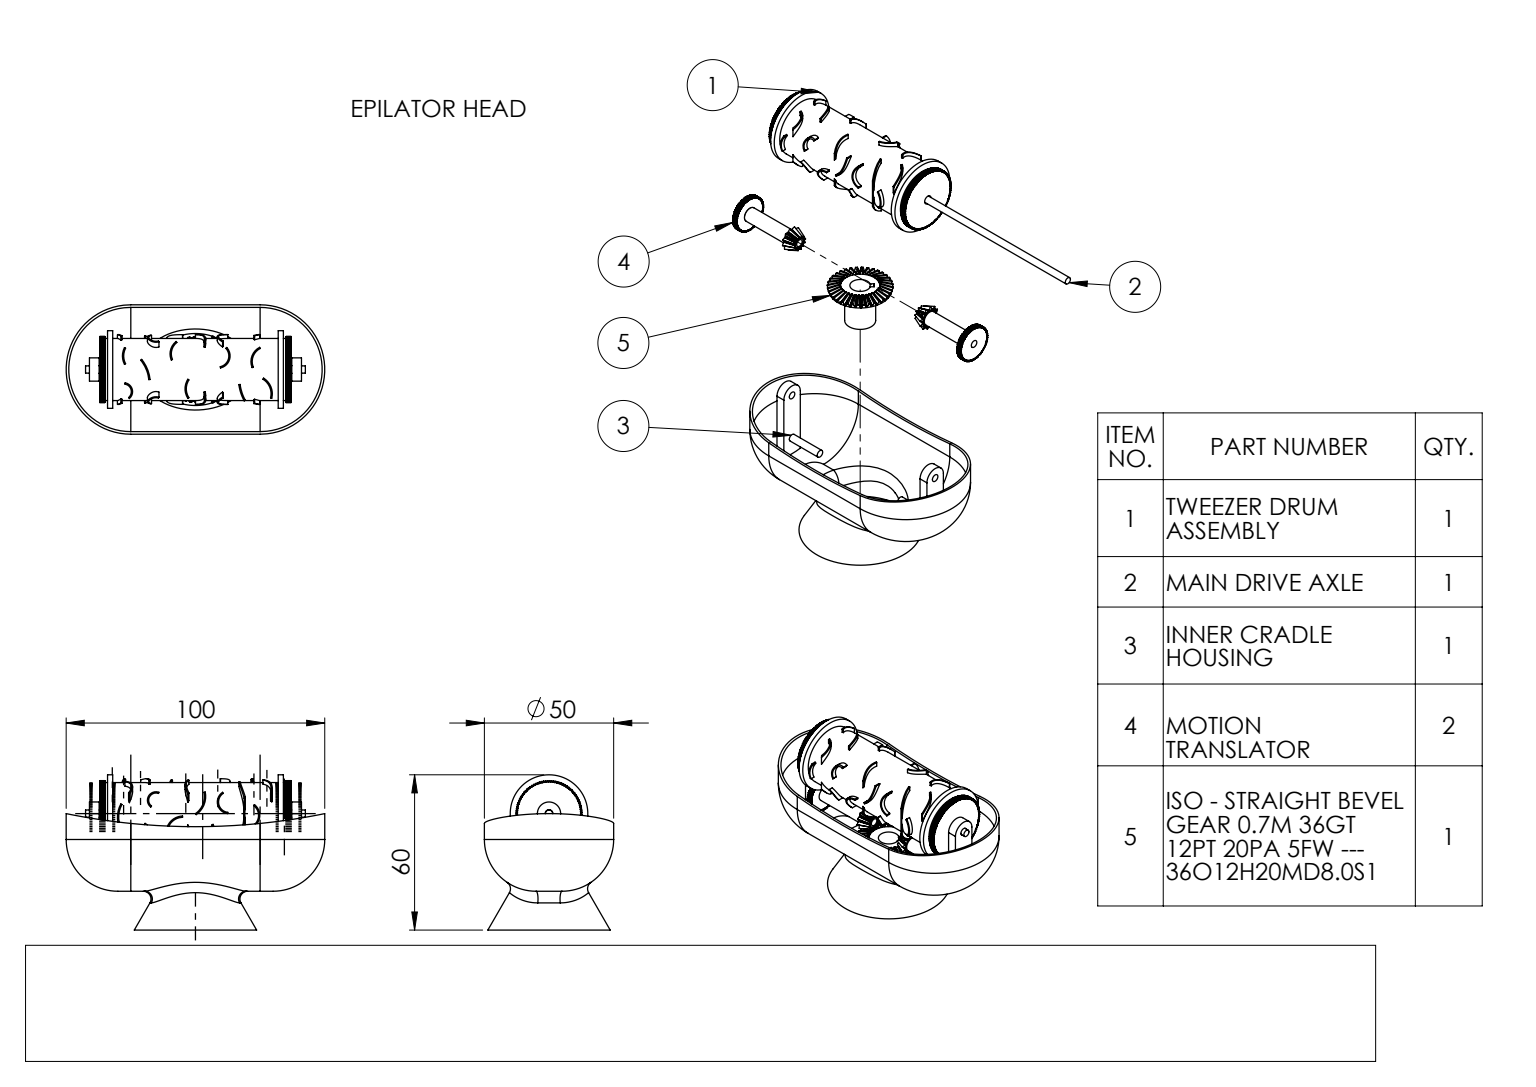
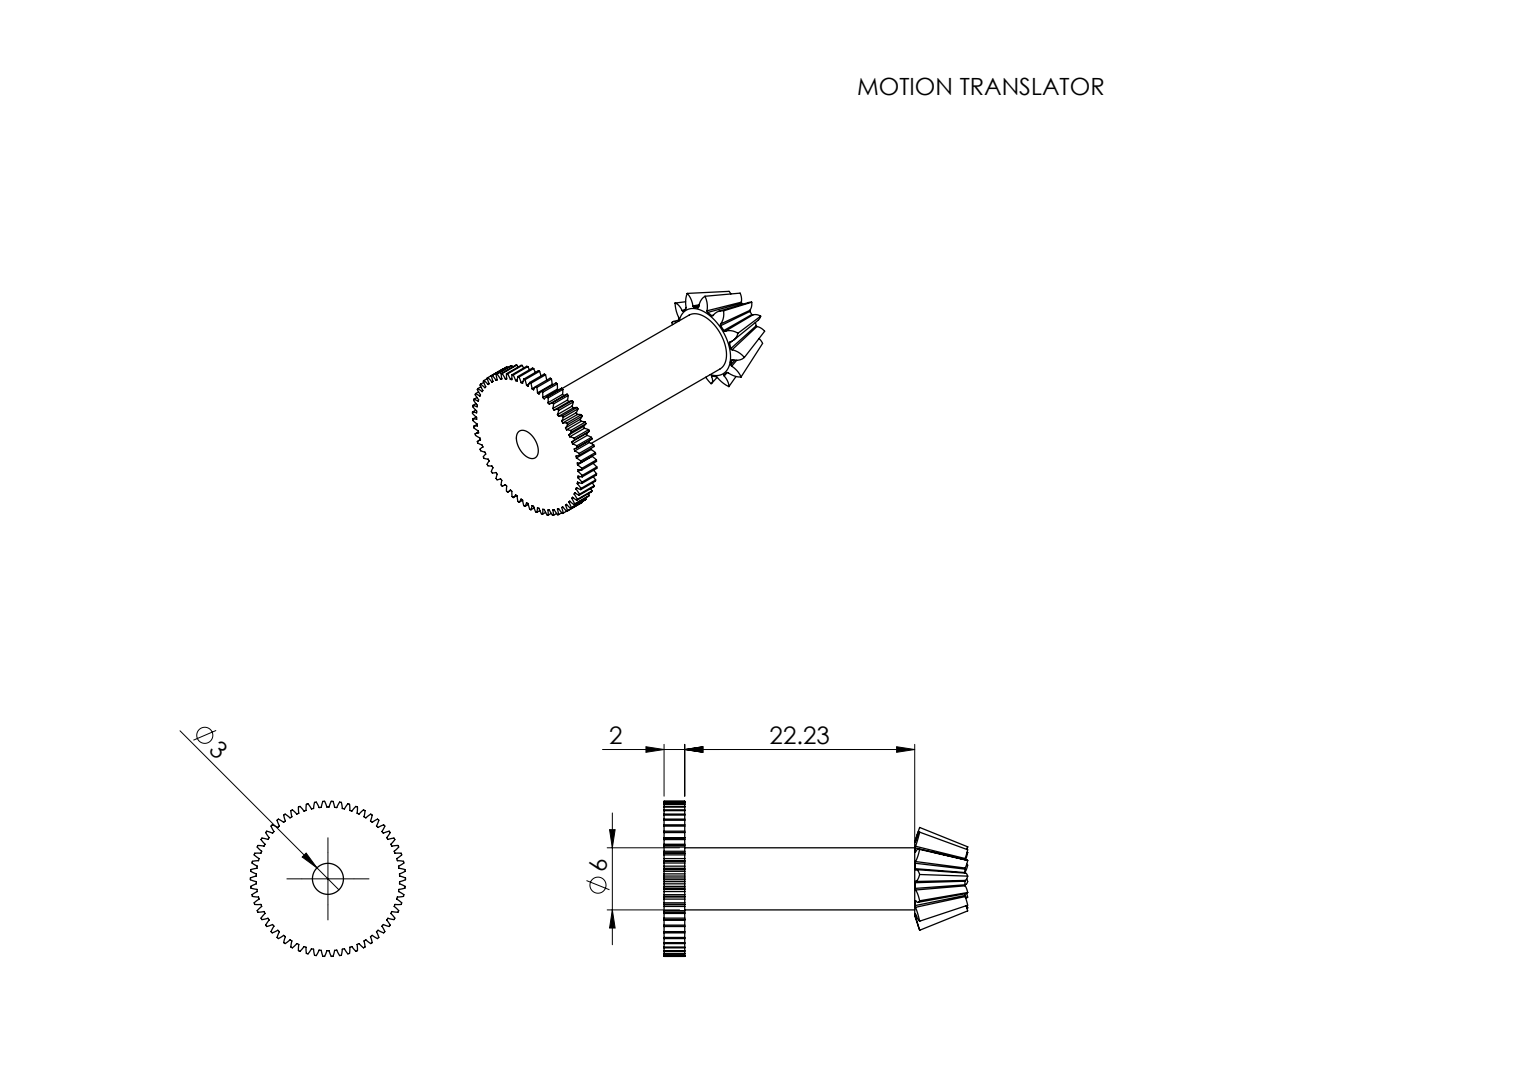
ISO-10303-21;
HEADER;
FILE_DESCRIPTION (('STEP AP214'),
    '1' );
FILE_NAME ('BR-837',
    '2026-10-09T15:17:24',
    ( '' ),
    ( '' ),
    'SwSTEP 2.0',
    'SolidWorks 2026',
    '' );
FILE_SCHEMA (( 'AUTOMOTIVE_DESIGN' ));
ENDSEC;

DATA;
#1 = ORIENTED_EDGE ( 'NONE', *, *, #54093, .F. ) ;
#2 =( BOUNDED_CURVE ( )  B_SPLINE_CURVE ( 3, ( #3306, #62815, #58857, #63152 ),
 .UNSPECIFIED., .F., .T. ) 
 B_SPLINE_CURVE_WITH_KNOTS ( ( 4, 4 ),
 ( 1.289274629942206873, 1.307832622343243267 ),
 .UNSPECIFIED. ) 
 CURVE ( )  GEOMETRIC_REPRESENTATION_ITEM ( )  RATIONAL_B_SPLINE_CURVE ( ( 1.000000000000000000, 0.9999713002824244246, 0.9999713002824244246, 1.000000000000000000 ) ) 
 REPRESENTATION_ITEM ( '' )  );
#3 = DIRECTION ( 'NONE',  ( 1.000000000000000000, 0.000000000000000000, -0.000000000000000000 ) ) ;
#4 = CARTESIAN_POINT ( 'NONE',  ( 34.00000000000000000, 1.267509437117510519E-14, 0.000000000000000000 ) ) ;
#5 = EDGE_CURVE ( 'NONE', #33980, #40116, #8200, .T. ) ;
#6 = ORIENTED_EDGE ( 'NONE', *, *, #26203, .T. ) ;
#7 = CARTESIAN_POINT ( 'NONE',  ( -27.64865282621882869, 11.88308961669896746, -6.412759754742364926 ) ) ;
#8 = CARTESIAN_POINT ( 'NONE',  ( 29.22757921152195948, 7.948027597311009274, 9.002217460645077551 ) ) ;
#9 = DIRECTION ( 'NONE',  ( -1.000000000000000000, 0.000000000000000000, 0.000000000000000000 ) ) ;
#10 = AXIS2_PLACEMENT_3D ( 'NONE', #51106, #21495, #16509 ) ;
#11 = EDGE_LOOP ( 'NONE', ( #13476, #2905, #46275, #26509, #7082, #64281 ) ) ;
#12 = CARTESIAN_POINT ( 'NONE',  ( 2.251152103363648127, -7.636644423939545234, 0.1252683866804877588 ) ) ;
#13 = EDGE_CURVE ( 'NONE', #20288, #62523, #39030, .T. ) ;
#14 = CIRCLE ( 'NONE', #45668, 4.999999999999999112 ) ;
#15 = ORIENTED_EDGE ( 'NONE', *, *, #45352, .F. ) ;
#16 = CARTESIAN_POINT ( 'NONE',  ( -2.532614230583026593, 25.00000000000000000, 10.89930238848911337 ) ) ;
#17 = CARTESIAN_POINT ( 'NONE',  ( -20.31445708845316389, -13.09484702705360704, -3.338600914039887346 ) ) ;
#18 = CARTESIAN_POINT ( 'NONE',  ( -9.857630741398541119, -27.64257788600498245, 14.42778837489968424 ) ) ;
#19 = DIRECTION ( 'NONE',  ( 1.000000000000000000, 0.000000000000000000, 0.000000000000000000 ) ) ;
#20 = CARTESIAN_POINT ( 'NONE',  ( 2.241509619876138171, 7.511759925807403704, 1.363398699156074922 ) ) ;
#21 = EDGE_LOOP ( 'NONE', ( #48561, #59529, #5133, #41435 ) ) ;
#22 = CARTESIAN_POINT ( 'NONE',  ( 37.00000000000000711, -6.303578524887017309, -10.42955799785317872 ) ) ;
#24 = AXIS2_PLACEMENT_3D ( 'NONE', #425, #35953, #14688 ) ;
#23 = CARTESIAN_POINT ( 'NONE',  ( 3.459614771489464946, -11.09853614738469396, 25.00000000000000000 ) ) ;
#25 = CARTESIAN_POINT ( 'NONE',  ( 2.241528039335009215, 3.830846649711605600, -6.603755931420445258 ) ) ;
#26 = CARTESIAN_POINT ( 'NONE',  ( 35.00000000000000000, 4.705694406421931860E-17, -3.469127814946512892E-15 ) ) ;
#27 = CIRCLE ( 'NONE', #62657, 12.18649999999999878 ) ;
#28 = CARTESIAN_POINT ( 'NONE',  ( 0.2671309869109511070, -12.08782215308010066, -1.966882337881812104 ) ) ;
#29 = CARTESIAN_POINT ( 'NONE',  ( 47.00000000000000711, 4.705694406421931860E-17, -3.469127814946512892E-15 ) ) ;
#30 = DIRECTION ( 'NONE',  ( 1.000000000000000000, -0.000000000000000000, 0.000000000000000000 ) ) ;
#31 = CARTESIAN_POINT ( 'NONE',  ( 0.2648978790185610999, -6.008231198269058382, 10.67083876753489946 ) ) ;
#32 = CARTESIAN_POINT ( 'NONE',  ( -36.00000000000000711, -2.527899948230555083, -12.49688848680887077 ) ) ;
#33 = B_SPLINE_CURVE_WITH_KNOTS ( 'NONE', 3,
 ( #58720, #44686, #34706, #18133, #9434, #8152, #55005, #39719, #13453, #43722, #8473, #64002, #3845, #49070, #3519, #23790 ),
 .UNSPECIFIED., .F., .F.,
 ( 4, 3, 3, 3, 3, 4 ),
 ( 0.000000000000000000, 0.0002999043160757348470, 0.0005998071753050991575, 0.0008997092107374514165, 0.001204458948195627314, 0.001510329163476480975 ),
 .UNSPECIFIED. ) ;
#34 = EDGE_CURVE ( 'NONE', #6901, #57938, #39765, .T. ) ;
#35 = CIRCLE ( 'NONE', #8525, 2.899999999999994582 ) ;
#36 = CIRCLE ( 'NONE', #39342, 5.000000000000000000 ) ;
#37 = ORIENTED_EDGE ( 'NONE', *, *, #2591, .T. ) ;
#38 = ORIENTED_EDGE ( 'NONE', *, *, #32481, .T. ) ;
#39 = DIRECTION ( 'NONE',  ( 0.2227494284590502138, 0.000000000000000000, 0.9748757316300199482 ) ) ;
#40 = CARTESIAN_POINT ( 'NONE',  ( -22.27721056931765631, -3.610969226755186057, 0.7178530073137494583 ) ) ;
#41 = DIRECTION ( 'NONE',  ( -1.000000000000000000, 0.000000000000000000, 0.000000000000000000 ) ) ;
#42 = DIRECTION ( 'NONE',  ( -0.000000000000000000, -0.000000000000000000, -1.000000000000000000 ) ) ;
#43 = ORIENTED_EDGE ( 'NONE', *, *, #16886, .F. ) ;
#44 = VERTEX_POINT ( 'NONE', #43427 ) ;
#45 = ORIENTED_EDGE ( 'NONE', *, *, #528, .T. ) ;
#46 = CARTESIAN_POINT ( 'NONE',  ( 2.931247277082686509, 3.034789039497289842, -7.255238984871596131 ) ) ;
#47 = AXIS2_PLACEMENT_3D ( 'NONE', #35700, #25750, #46038 ) ;
#48 = CARTESIAN_POINT ( 'NONE',  ( -20.92008205012189848, -11.37744109147143590, -3.816568647652266222 ) ) ;
#49 = EDGE_CURVE ( 'NONE', #39147, #50867, #8852, .T. ) ;
#50 = ORIENTED_EDGE ( 'NONE', *, *, #19511, .T. ) ;
#51 = CARTESIAN_POINT ( 'NONE',  ( 20.00005080000000035, 0.000000000000000000, 0.000000000000000000 ) ) ;
#52 = CARTESIAN_POINT ( 'NONE',  ( 35.00000000000000000, 3.511814412392283646, 11.66953048682395355 ) ) ;
#53 = CARTESIAN_POINT ( 'NONE',  ( 2.990245332647861964, -8.426135047918856813, 0.9653152459622899029 ) ) ;
#54 = ORIENTED_EDGE ( 'NONE', *, *, #43453, .T. ) ;
#55 = CARTESIAN_POINT ( 'NONE',  ( -22.30078715814471835, 0.2606204736987125514, 3.743307663037636956 ) ) ;
#56 = EDGE_CURVE ( 'NONE', #31963, #46746, #12133, .T. ) ;
#57 = CARTESIAN_POINT ( 'NONE',  ( 1.074417311476297821, -26.55384113566742599, -16.22365110280896161 ) ) ;
#58 = DIRECTION ( 'NONE',  ( -0.000000000000000000, -0.000000000000000000, -1.000000000000000000 ) ) ;
#59 = VERTEX_POINT ( 'NONE', #24459 ) ;
#60 = DIRECTION ( 'NONE',  ( -1.000000000000000000, 0.000000000000000000, 0.000000000000000000 ) ) ;
#61 = EDGE_CURVE ( 'NONE', #21447, #54893, #59089, .T. ) ;
#62 = EDGE_LOOP ( 'NONE', ( #29288, #23107, #41719, #50661 ) ) ;
#63 = CARTESIAN_POINT ( 'NONE',  ( 1.719304012339869514, -10.22720798541492471, 7.581471372739622794 ) ) ;
#64 = VECTOR ( 'NONE', #37546, 1000.000000000000000 ) ;
#65 = ORIENTED_EDGE ( 'NONE', *, *, #16176, .T. ) ;
#66 = CARTESIAN_POINT ( 'NONE',  ( -28.82521652700830117, 2.770713649382011923, -11.70126355471820467 ) ) ;
#67 = DIRECTION ( 'NONE',  ( -1.000000000000000000, 0.000000000000000000, 0.000000000000000000 ) ) ;
#68 = CARTESIAN_POINT ( 'NONE',  ( 37.00000000000000711, -11.24036214326524608, -6.018036132182126963 ) ) ;
#69 = DIRECTION ( 'NONE',  ( 1.000000000000000000, 0.000000000000000000, 0.000000000000000000 ) ) ;
#70 = CARTESIAN_POINT ( 'NONE',  ( -25.62834777364930616, 3.789932915281918113, 0.3208481691297681571 ) ) ;
#71 = LINE ( 'NONE', #60932, #20822 ) ;
#73 = ADVANCED_FACE ( 'NONE', ( #28468 ), #28161, .T. ) ;
#72 = FACE_OUTER_BOUND ( 'NONE', #21763, .T. ) ;
#74 = DIRECTION ( 'NONE',  ( 0.000000000000000000, 0.000000000000000000, -1.000000000000000000 ) ) ;
#75 = CARTESIAN_POINT ( 'NONE',  ( 0.2833330754217384673, -3.999965385632516579, -11.58086621621911583 ) ) ;
#77 = ORIENTED_EDGE ( 'NONE', *, *, #43041, .T. ) ;
#76 = CARTESIAN_POINT ( 'NONE',  ( -37.00000000000000711, 0.7536123767500182424, -11.72195762423409171 ) ) ;
#78 = CARTESIAN_POINT ( 'NONE',  ( -22.30625920655495165, -3.783486345733982237, 0.2529928606556808846 ) ) ;
#79 = AXIS2_PLACEMENT_3D ( 'NONE', #49490, #64734, #28522 ) ;
#80 = ORIENTED_EDGE ( 'NONE', *, *, #29710, .F. ) ;
#81 = CARTESIAN_POINT ( 'NONE',  ( 2.305787727787084407, -3.971363876083918498, -6.545285700970570275 ) ) ;
#82 = VERTEX_POINT ( 'NONE', #8514 ) ;
#83 = EDGE_CURVE ( 'NONE', #13628, #12164, #48775, .T. ) ;
#84 = CARTESIAN_POINT ( 'NONE',  ( 3.047904605210419504, -5.772373816836783078, -5.398304302092596707 ) ) ;
#85 = VECTOR ( 'NONE', #37422, 1000.000000000000000 ) ;
#86 = ORIENTED_EDGE ( 'NONE', *, *, #15250, .T. ) ;
#87 = DIRECTION ( 'NONE',  ( 1.000000000000000000, -0.000000000000000000, -0.000000000000000000 ) ) ;
#88 = LINE ( 'NONE', #34354, #47498 ) ;
#89 = CARTESIAN_POINT ( 'NONE',  ( -27.09229696323321335, -2.225368503508849294, 0.6397626223479151442 ) ) ;
#90 = DIRECTION ( 'NONE',  ( 0.000000000000000000, 0.000000000000000000, -1.000000000000000000 ) ) ;
#91 = DIRECTION ( 'NONE',  ( 1.000000000000000000, 0.000000000000000000, 0.000000000000000000 ) ) ;
#92 = CIRCLE ( 'NONE', #17079, 4.999999999999999112 ) ;
#93 = AXIS2_PLACEMENT_3D ( 'NONE', #46470, #925, #21193 ) ;
#94 = AXIS2_PLACEMENT_3D ( 'NONE', #16809, #31133, #22127 ) ;
#95 = VERTEX_POINT ( 'NONE', #49115 ) ;
#96 = CARTESIAN_POINT ( 'NONE',  ( -37.00000000000000711, 7.474872387601008583, 9.060822531526074641 ) ) ;
#97 = EDGE_CURVE ( 'NONE', #10033, #43796, #33778, .T. ) ;
#98 = AXIS2_PLACEMENT_3D ( 'NONE', #57341, #58008, #7118 ) ;
#99 = ORIENTED_EDGE ( 'NONE', *, *, #2192, .T. ) ;
#100 = CARTESIAN_POINT ( 'NONE',  ( -22.30625920655495165, 0.8854385781085528651, -3.687109008463846926 ) ) ;
#101 = EDGE_CURVE ( 'NONE', #9709, #46803, #31331, .T. ) ;
#102 = FACE_OUTER_BOUND ( 'NONE', #65679, .T. ) ;
#103 = CARTESIAN_POINT ( 'NONE',  ( 0.2652384529303130067, -7.922180393770610785, -9.338494547402472534 ) ) ;
#104 = ORIENTED_EDGE ( 'NONE', *, *, #19181, .T. ) ;
#105 = CARTESIAN_POINT ( 'NONE',  ( -35.00000000000000000, 0.000000000000000000, 0.000000000000000000 ) ) ;
#106 = AXIS2_PLACEMENT_3D ( 'NONE', #32837, #48187, #63433 ) ;
#107 = AXIS2_PLACEMENT_3D ( 'NONE', #48295, #12020, #32299 ) ;
#108 = CIRCLE ( 'NONE', #63839, 12.18649999999999700 ) ;
#109 = AXIS2_PLACEMENT_3D ( 'NONE', #42573, #46294, #734 ) ;
#110 = CARTESIAN_POINT ( 'NONE',  ( 49.33927601438018229, -0.1339636383559821564, -5.724480317196142032 ) ) ;
#111 = B_SPLINE_CURVE_WITH_KNOTS ( 'NONE', 3,
 ( #8141, #22114, #47410, #53377, #22445, #48713, #53707, #37074, #18119, #33412, #57373, #11799, #28412, #13126, #6844, #1847, #63323, #42709, #17792 ),
 .UNSPECIFIED., .F., .F.,
 ( 4, 3, 3, 3, 3, 3, 4 ),
 ( 0.000000000000000000, 2.831840207457774963E-05, 4.217266859783117455E-05, 5.602024318339443094E-05, 6.290810167912943239E-05, 9.120440630890260935E-05, 0.0001153103026480235913 ),
 .UNSPECIFIED. ) ;
#112 = AXIS2_PLACEMENT_3D ( 'NONE', #43314, #33991, #53653 ) ;
#113 = CARTESIAN_POINT ( 'NONE',  ( -10.71713000802667359, -9.043952695441483058, -10.03432938415238951 ) ) ;
#114 = CARTESIAN_POINT ( 'NONE',  ( -38.20713125073509531, -2.115151932665340961, -21.24219930640693832 ) ) ;
#115 = ORIENTED_EDGE ( 'NONE', *, *, #54584, .T. ) ;
#116 = CARTESIAN_POINT ( 'NONE',  ( 19.56743653832046803, -28.99999999999999645, -5.000000000000000888 ) ) ;
#117 = CARTESIAN_POINT ( 'NONE',  ( 2.000000000000001776, -6.441884263200823746, -2.217201541069834914 ) ) ;
#118 = CARTESIAN_POINT ( 'NONE',  ( 2.827825597296804272, -9.007857251166447199, -0.5449445831287991204 ) ) ;
#119 = AXIS2_PLACEMENT_3D ( 'NONE', #1581, #5588, #900 ) ;
#120 = ADVANCED_FACE ( 'NONE', ( #39097 ), #54424, .T. ) ;
#121 = ADVANCED_FACE ( 'NONE', ( #65020 ), #19493, .F. ) ;
#122 = CARTESIAN_POINT ( 'NONE',  ( -37.00000000000000711, 12.02534193257726969, -4.237174932027097718 ) ) ;
#123 = DIRECTION ( 'NONE',  ( 1.000000000000000000, -0.000000000000000000, 0.000000000000000000 ) ) ;
#124 = CIRCLE ( 'NONE', #37284, 5.000000000000000000 ) ;
#125 = VERTEX_POINT ( 'NONE', #10810 ) ;
#126 = CARTESIAN_POINT ( 'NONE',  ( -22.28506771379528573, 3.622079238249921840, 0.8783543640076683090 ) ) ;
#127 = CARTESIAN_POINT ( 'NONE',  ( 2.096166925314653984, 2.110369137379828786, -11.81794094722716260 ) ) ;
#128 = CARTESIAN_POINT ( 'NONE',  ( -22.29570301036918778, 3.588849529203733457, -1.042190670255880525 ) ) ;
#129 = EDGE_LOOP ( 'NONE', ( #26089, #45979, #28221, #53129 ) ) ;
#130 = CARTESIAN_POINT ( 'NONE',  ( -35.00000000000000000, 11.56998259273177787, 3.827046518385122553 ) ) ;
#131 = AXIS2_PLACEMENT_3D ( 'NONE', #9769, #50367, #4141 ) ;
#132 = CARTESIAN_POINT ( 'NONE',  ( 37.00000000000000711, 4.705694406421931860E-17, -3.469127814946512892E-15 ) ) ;
#133 = ORIENTED_EDGE ( 'NONE', *, *, #30675, .T. ) ;
#134 = EDGE_CURVE ( 'NONE', #53943, #37151, #49390, .T. ) ;
#135 = EDGE_LOOP ( 'NONE', ( #15997, #3702, #27078, #2033 ) ) ;
#136 = VERTEX_POINT ( 'NONE', #26116 ) ;
#137 = AXIS2_PLACEMENT_3D ( 'NONE', #15886, #35532, #47176 ) ;
#138 = AXIS2_PLACEMENT_3D ( 'NONE', #35736, #56035, #531 ) ;
#139 = VECTOR ( 'NONE', #13828, 1000.000000000000000 ) ;
#140 = EDGE_CURVE ( 'NONE', #38995, #49368, #10066, .T. ) ;
#141 = ORIENTED_EDGE ( 'NONE', *, *, #6255, .F. ) ;
#142 = FACE_OUTER_BOUND ( 'NONE', #36024, .T. ) ;
#143 = DIRECTION ( 'NONE',  ( 0.000000000000000000, -0.01356324068817999114, 0.9999080150203989437 ) ) ;
#144 = DIRECTION ( 'NONE',  ( 1.000000000000000000, 0.000000000000000000, 0.000000000000000000 ) ) ;
#145 = DIRECTION ( 'NONE',  ( 0.000000000000000000, -0.9796553971857763221, -0.2006870767258792099 ) ) ;
#146 = DIRECTION ( 'NONE',  ( 1.000000000000000000, 0.000000000000000000, 0.000000000000000000 ) ) ;
#147 = CARTESIAN_POINT ( 'NONE',  ( -8.315422948566315142, -32.37591480791618892, 12.77210737139424523 ) ) ;
#148 = CARTESIAN_POINT ( 'NONE',  ( -17.73782175230979874, 11.72754298194778677, 2.564785682591074867 ) ) ;
#150 = ORIENTED_EDGE ( 'NONE', *, *, #41675, .F. ) ;
#149 = CARTESIAN_POINT ( 'NONE',  ( 3.780834652287974773, 8.352030633203074927, 25.00000000000000000 ) ) ;
#151 = DIRECTION ( 'NONE',  ( 0.1024315404614497965, 0.9947400562552481951, 0.000000000000000000 ) ) ;
#152 = EDGE_CURVE ( 'NONE', #21897, #44042, #18588, .T. ) ;
#153 = VERTEX_POINT ( 'NONE', #21105 ) ;
#154 = CARTESIAN_POINT ( 'NONE',  ( 35.00000000000000000, 5.015831474386306610, -10.62137734850269943 ) ) ;
#155 = EDGE_LOOP ( 'NONE', ( #12731, #28986, #56785, #59281 ) ) ;
#156 = ORIENTED_EDGE ( 'NONE', *, *, #22157, .F. ) ;
#157 = CARTESIAN_POINT ( 'NONE',  ( -22.29018399051993882, -0.9010028109495024085, 3.609810019245832002 ) ) ;
#158 = AXIS2_PLACEMENT_3D ( 'NONE', #49089, #24435, #29743 ) ;
#159 = CARTESIAN_POINT ( 'NONE',  ( 14.19127861764911813, -30.11167671974727611, 5.095448428665359408 ) ) ;
#160 = DIRECTION ( 'NONE',  ( 0.9318405276259970060, 0.3628680629012471237, 0.000000000000000000 ) ) ;
#161 = AXIS2_PLACEMENT_3D ( 'NONE', #36598, #16644, #2007 ) ;
#162 = CARTESIAN_POINT ( 'NONE',  ( 3.152665057734087117, 7.886634106564184954, -0.9030954876737516956 ) ) ;
#163 = CARTESIAN_POINT ( 'NONE',  ( 37.00000000000000711, -4.426194442447322075, -11.35427606708804937 ) ) ;
#164 = FACE_OUTER_BOUND ( 'NONE', #34592, .T. ) ;
#166 = ORIENTED_EDGE ( 'NONE', *, *, #2823, .F. ) ;
#165 = AXIS2_PLACEMENT_3D ( 'NONE', #42783, #38794, #59092 ) ;
#167 = VERTEX_POINT ( 'NONE', #45398 ) ;
#168 = CARTESIAN_POINT ( 'NONE',  ( -36.00000000000000711, -10.59380114696474884, 7.094637218249319588 ) ) ;
#169 = EDGE_LOOP ( 'NONE', ( #2246, #11811, #65657, #252 ) ) ;
#170 = EDGE_CURVE ( 'NONE', #3983, #20113, #56362, .T. ) ;
#171 = AXIS2_PLACEMENT_3D ( 'NONE', #20760, #45365, #40362 ) ;
#172 = EDGE_CURVE ( 'NONE', #21730, #4780, #9821, .T. ) ;
#173 = VERTEX_POINT ( 'NONE', #29764 ) ;
#174 = FACE_OUTER_BOUND ( 'NONE', #28123, .T. ) ;
#175 = CARTESIAN_POINT ( 'NONE',  ( -27.08579483061202708, -2.287150433979698416, 0.2015567301747388795 ) ) ;
#176 = DIRECTION ( 'NONE',  ( 0.000000000000000000, -0.4380125133594036657, 0.8989688749565127868 ) ) ;
#177 = CARTESIAN_POINT ( 'NONE',  ( 0.6473888112830216146, -12.12394591856680570, 2.472751636945331732 ) ) ;
#178 = EDGE_CURVE ( 'NONE', #56217, #10069, #62087, .T. ) ;
#179 = FACE_OUTER_BOUND ( 'NONE', #65053, .T. ) ;
#180 = DIRECTION ( 'NONE',  ( -1.000000000000000000, 0.000000000000000000, 0.000000000000000000 ) ) ;
#181 = EDGE_CURVE ( 'NONE', #43273, #6060, #21747, .T. ) ;
#182 = AXIS2_PLACEMENT_3D ( 'NONE', #6884, #41786, #7187 ) ;
#183 = ORIENTED_EDGE ( 'NONE', *, *, #61876, .T. ) ;
#184 = ORIENTED_EDGE ( 'NONE', *, *, #58820, .T. ) ;
#185 = ADVANCED_FACE ( 'NONE', ( #61669 ), #5522, .T. ) ;
#186 = VECTOR ( 'NONE', #14671, 1000.000000000000000 ) ;
#187 = VECTOR ( 'NONE', #61611, 1000.000000000000000 ) ;
#188 = CARTESIAN_POINT ( 'NONE',  ( -19.47984447937493613, -3.750539801530005768, -12.96855624952674724 ) ) ;
#189 = CARTESIAN_POINT ( 'NONE',  ( 36.00000000000000711, 4.983891302653744582, 11.73555825188270596 ) ) ;
#190 = CARTESIAN_POINT ( 'NONE',  ( 6.361445718264521432, -4.355102044641763648, -12.77822703589027320 ) ) ;
#191 = B_SPLINE_CURVE_WITH_KNOTS ( 'NONE', 3,
 ( #18911, #33216, #7968, #28236, #58853, #48528 ),
 .UNSPECIFIED., .F., .F.,
 ( 4, 2, 4 ),
 ( 0.0002637379172017313396, 0.0009975831966478583904, 0.001731428476093985116 ),
 .UNSPECIFIED. ) ;
#192 = AXIS2_PLACEMENT_3D ( 'NONE', #53124, #17228, #57806 ) ;
#193 = VECTOR ( 'NONE', #7034, 1000.000000000000114 ) ;
#194 = CARTESIAN_POINT ( 'NONE',  ( -27.15511094194037867, -2.499833641087594760, 0.1446243978645337658 ) ) ;
#195 = CARTESIAN_POINT ( 'NONE',  ( -35.04709527796842394, 0.01012471662513447779, 0.007095259204982495849 ) ) ;
#196 =( BOUNDED_CURVE ( )  B_SPLINE_CURVE ( 3, ( #42557, #43227, #37603, #11661 ),
 .UNSPECIFIED., .F., .F. ) 
 B_SPLINE_CURVE_WITH_KNOTS ( ( 4, 4 ),
 ( 1.718692970945833176, 1.736025308729231442 ),
 .UNSPECIFIED. ) 
 CURVE ( )  GEOMETRIC_REPRESENTATION_ITEM ( )  RATIONAL_B_SPLINE_CURVE ( ( 1.000000000000000000, 0.9999749659955903258, 0.9999749659955903258, 1.000000000000000000 ) ) 
 REPRESENTATION_ITEM ( '' )  );
#197 = CYLINDRICAL_SURFACE ( 'NONE', #36249, 12.18650000000000055 ) ;
#198 = CARTESIAN_POINT ( 'NONE',  ( 0.4626703367448636306, 2.416235258140044362, -12.07256244737125961 ) ) ;
#199 = CARTESIAN_POINT ( 'NONE',  ( -27.08421860617808363, -2.116856729767840228, -0.8768262158915675064 ) ) ;
#200 = ORIENTED_EDGE ( 'NONE', *, *, #42042, .T. ) ;
#201 = CARTESIAN_POINT ( 'NONE',  ( -27.32343372485683730, 2.534722478175136740, 1.625341394141078144 ) ) ;
#202 = CARTESIAN_POINT ( 'NONE',  ( -35.00000000000000000, 10.14433819232434253, 6.753013023069750709 ) ) ;
#203 = FACE_OUTER_BOUND ( 'NONE', #44719, .T. ) ;
#204 = CIRCLE ( 'NONE', #54373, 12.74999999999999822 ) ;
#205 = AXIS2_PLACEMENT_3D ( 'NONE', #46819, #52490, #27194 ) ;
#206 = EDGE_CURVE ( 'NONE', #57207, #22857, #45089, .T. ) ;
#207 = AXIS2_PLACEMENT_3D ( 'NONE', #6492, #31105, #57702 ) ;
#208 = CARTESIAN_POINT ( 'NONE',  ( 0.2655924914740778187, -12.05257978623652448, -2.169924872618184786 ) ) ;
#209 = EDGE_CURVE ( 'NONE', #63155, #63467, #60591, .T. ) ;
#210 = CARTESIAN_POINT ( 'NONE',  ( 3.092491956585784241, -7.275786042219372085, 3.124176487320387441 ) ) ;
#211 = ORIENTED_EDGE ( 'NONE', *, *, #16595, .T. ) ;
#212 = CARTESIAN_POINT ( 'NONE',  ( -37.00000000000000711, -12.18632975068353019, -0.06441628369849204672 ) ) ;
#213 = CARTESIAN_POINT ( 'NONE',  ( 0.2638984909335720941, -12.02508546958698332, 2.322601104020627805 ) ) ;
#214 = CIRCLE ( 'NONE', #62853, 6.936499999999993449 ) ;
#215 = CARTESIAN_POINT ( 'NONE',  ( 16.21117406328132304, -34.99999999999999289, -4.142385751841744401 ) ) ;
#216 = B_SPLINE_CURVE_WITH_KNOTS ( 'NONE', 3,
 ( #1880, #63683, #38430, #58746, #6877, #27148, #47443, #64026, #15370, #54060, #44980, #50957, #45969, #34971, #50317, #55276, #15032, #5405, #30645 ),
 .UNSPECIFIED., .F., .F.,
 ( 4, 3, 3, 3, 3, 3, 4 ),
 ( 5.818439421673296370E-18, 2.825908398831187513E-05, 4.208813692483793747E-05, 5.591713746943596087E-05, 6.279584083231647704E-05, 9.105792820296370140E-05, 0.0001153131102488875055 ),
 .UNSPECIFIED. ) ;
#217 = VERTEX_POINT ( 'NONE', #15781 ) ;
#218 = CARTESIAN_POINT ( 'NONE',  ( -35.00000000000000000, 8.839356091080043498, 8.389074212634319849 ) ) ;
#219 = DIRECTION ( 'NONE',  ( -1.000000000000000000, 0.000000000000000000, 0.000000000000000000 ) ) ;
#220 = CARTESIAN_POINT ( 'NONE',  ( 0.2655924914740778742, -12.24627751708824341, 0.04405032194299108445 ) ) ;
#221 = AXIS2_PLACEMENT_3D ( 'NONE', #54414, #54070, #45388 ) ;
#222 = EDGE_CURVE ( 'NONE', #29075, #15867, #7943, .T. ) ;
#223 = B_SPLINE_CURVE_WITH_KNOTS ( 'NONE', 3,
 ( #13246, #39149, #18241, #53499, #54134, #28212, #28523, #8905, #39480, #12909, #43480, #33190, #48831, #38166, #17904, #19206 ),
 .UNSPECIFIED., .F., .F.,
 ( 4, 3, 3, 3, 3, 4 ),
 ( 4.848699518061080308E-19, 0.0002176109881720241597, 0.0004352086762394590945, 0.0006528017811446864237, 0.0007615147961451705421, 0.0009453342004947242697 ),
 .UNSPECIFIED. ) ;
#225 = ORIENTED_EDGE ( 'NONE', *, *, #59679, .F. ) ;
#224 = CARTESIAN_POINT ( 'NONE',  ( 2.305787727787083519, 1.164987321564732392, 7.566723232958076473 ) ) ;
#226 = DIRECTION ( 'NONE',  ( -1.000000000000000000, 0.000000000000000000, 0.000000000000000000 ) ) ;
#227 = EDGE_LOOP ( 'NONE', ( #64875, #62526, #21303, #60308, #50623, #6890 ) ) ;
#228 = FACE_OUTER_BOUND ( 'NONE', #46876, .T. ) ;
#229 = CIRCLE ( 'NONE', #27843, 5.000000000000000888 ) ;
#230 = CARTESIAN_POINT ( 'NONE',  ( -9.317410475120057711, 12.33400277018097313, -5.499978468384917996 ) ) ;
#231 = CARTESIAN_POINT ( 'NONE',  ( -18.58686583997218378, 5.413436517372335111, -12.37033473226556701 ) ) ;
#232 = DIRECTION ( 'NONE',  ( 0.000000000000000000, 0.9105187689795939399, -0.4134677391718545314 ) ) ;
#233 = CARTESIAN_POINT ( 'NONE',  ( 2.000000000000001776, -2.562706407243573459, -6.312399813420393357 ) ) ;
#234 = DIRECTION ( 'NONE',  ( 0.000000000000000000, -0.9718671068226485410, 0.2355298848897412756 ) ) ;
#235 = CARTESIAN_POINT ( 'NONE',  ( 0.3610902822527258804, 11.44530431865298681, -4.444884365376487345 ) ) ;
#236 = EDGE_CURVE ( 'NONE', #36605, #55598, #2693, .T. ) ;
#237 = ORIENTED_EDGE ( 'NONE', *, *, #59193, .T. ) ;
#238 = DIRECTION ( 'NONE',  ( 0.000000000000000000, -0.01356324068817999114, 0.9999080150203989437 ) ) ;
#239 = VERTEX_POINT ( 'NONE', #11151 ) ;
#240 = CIRCLE ( 'NONE', #37383, 5.000000000000000000 ) ;
#241 = EDGE_CURVE ( 'NONE', #20405, #8903, #32353, .T. ) ;
#242 = CARTESIAN_POINT ( 'NONE',  ( 35.00000000000000000, 1.771820996347156507, -11.61175578952786935 ) ) ;
#244 = LINE ( 'NONE', #9870, #20494 ) ;
#243 = VECTOR ( 'NONE', #9924, 1000.000000000000000 ) ;
#245 = AXIS2_PLACEMENT_3D ( 'NONE', #20192, #25505, #24868 ) ;
#246 = AXIS2_PLACEMENT_3D ( 'NONE', #24663, #44940, #65220 ) ;
#247 = CARTESIAN_POINT ( 'NONE',  ( 2.000000000000001776, -0.7281529553921466391, -7.464569195442808613 ) ) ;
#248 = ORIENTED_EDGE ( 'NONE', *, *, #64139, .T. ) ;
#249 = CARTESIAN_POINT ( 'NONE',  ( -41.00000000000000711, -1.694065894508600678E-18, 0.000000000000000000 ) ) ;
#250 = CARTESIAN_POINT ( 'NONE',  ( 11.97679899998448683, 9.005363106165312104, -7.938319193498352355 ) ) ;
#251 = CARTESIAN_POINT ( 'NONE',  ( -22.27721056931765631, -1.183805672860815283, 3.486117586310720995 ) ) ;
#252 = ORIENTED_EDGE ( 'NONE', *, *, #20641, .T. ) ;
#253 = ORIENTED_EDGE ( 'NONE', *, *, #48209, .T. ) ;
#254 = FACE_OUTER_BOUND ( 'NONE', #27919, .T. ) ;
#255 = ORIENTED_EDGE ( 'NONE', *, *, #44339, .F. ) ;
#256 = CARTESIAN_POINT ( 'NONE',  ( 25.05309951391468459, -8.823569016628452388, -8.132934882857099979 ) ) ;
#257 = CARTESIAN_POINT ( 'NONE',  ( 5.536195898058073439, 0.008496323383586253108, 0.0002547682446687139432 ) ) ;
#258 = CARTESIAN_POINT ( 'NONE',  ( -27.09483304420799143, 2.317106154747425872, -0.1669215111592681211 ) ) ;
#259 = ADVANCED_FACE ( 'NONE', ( #62326 ), #1174, .T. ) ;
#260 = CARTESIAN_POINT ( 'NONE',  ( -35.00000000000000000, 9.752226076388895493, 6.547236723514054724 ) ) ;
#261 = AXIS2_PLACEMENT_3D ( 'NONE', #65222, #29972, #35280 ) ;
#262 = CARTESIAN_POINT ( 'NONE',  ( -35.04834644901396956, -0.01383120537648091335, 0.0002835132723572086118 ) ) ;
#263 = FACE_OUTER_BOUND ( 'NONE', #15822, .T. ) ;
#264 = EDGE_CURVE ( 'NONE', #36108, #56656, #5132, .T. ) ;
#265 = DIRECTION ( 'NONE',  ( -1.000000000000000000, -0.000000000000000000, 0.000000000000000000 ) ) ;
#266 = VERTEX_POINT ( 'NONE', #11780 ) ;
#267 = AXIS2_PLACEMENT_3D ( 'NONE', #40883, #20912, #26243 ) ;
#268 = CARTESIAN_POINT ( 'NONE',  ( 2.259025283528087069, 7.639069972920474072, -0.1366755880739947138 ) ) ;
#269 = EDGE_CURVE ( 'NONE', #27971, #17610, #57880, .T. ) ;
#270 = DIRECTION ( 'NONE',  ( 1.000000000000000000, 0.000000000000000000, 0.000000000000000000 ) ) ;
#271 = DIRECTION ( 'NONE',  ( 0.000000000000000000, -0.01356324068817999114, 0.9999080150203989437 ) ) ;
#272 = LINE ( 'NONE', #49512, #53068 ) ;
#273 = LINE ( 'NONE', #15537, #61542 ) ;
#274 = FACE_OUTER_BOUND ( 'NONE', #61383, .T. ) ;
#275 = CARTESIAN_POINT ( 'NONE',  ( -37.00000000000000711, 1.591260454995410578, -12.08216339958899077 ) ) ;
#276 = DIRECTION ( 'NONE',  ( 1.000000000000000000, 0.000000000000000000, 0.000000000000000000 ) ) ;
#277 = ORIENTED_EDGE ( 'NONE', *, *, #65294, .F. ) ;
#278 = CARTESIAN_POINT ( 'NONE',  ( 35.00000000000000000, -4.545979934229326780, 11.30684963584393543 ) ) ;
#279 = EDGE_CURVE ( 'NONE', #31543, #49222, #7578, .T. ) ;
#280 = AXIS2_PLACEMENT_3D ( 'NONE', #4610, #53838, #9548 ) ;
#281 = VERTEX_POINT ( 'NONE', #27095 ) ;
#282 = CARTESIAN_POINT ( 'NONE',  ( -3.473816564737393087, -10.12352008167872164, 6.455743956261353667 ) ) ;
#283 = CARTESIAN_POINT ( 'NONE',  ( -37.00000000000000711, 5.246972444134173408, -10.99909370905151995 ) ) ;
#284 = FACE_OUTER_BOUND ( 'NONE', #48979, .T. ) ;
#285 = CYLINDRICAL_SURFACE ( 'NONE', #47961, 1.500000000000000222 ) ;
#286 = CARTESIAN_POINT ( 'NONE',  ( 10.75853767213705225, 7.830989516993144051, 25.00000000000000000 ) ) ;
#287 = ORIENTED_EDGE ( 'NONE', *, *, #23022, .F. ) ;
#288 = AXIS2_PLACEMENT_3D ( 'NONE', #38389, #39045, #58707 ) ;
#289 = FACE_OUTER_BOUND ( 'NONE', #43549, .T. ) ;
#290 = CARTESIAN_POINT ( 'NONE',  ( 2.000000000000001776, 3.155844197800189210, -6.177028383390422484 ) ) ;
#291 = AXIS2_PLACEMENT_3D ( 'NONE', #33597, #54208, #9283 ) ;
#292 = CARTESIAN_POINT ( 'NONE',  ( 1.375507693218757543, -12.51366828189661895, 1.606074886185397510 ) ) ;
#293 = CARTESIAN_POINT ( 'NONE',  ( -27.28573687977896611, -0.4470060700698409994, 2.862048090118440857 ) ) ;
#294 = VECTOR ( 'NONE', #14164, 1000.000000000000000 ) ;
#295 = CARTESIAN_POINT ( 'NONE',  ( 1.937114397841932290, 5.226660192101747704, -11.72279974487458354 ) ) ;
#296 = EDGE_CURVE ( 'NONE', #24592, #42057, #62639, .T. ) ;
#297 = CARTESIAN_POINT ( 'NONE',  ( 2.242418902651940105, 2.704708480794804082, 7.139616612143395713 ) ) ;
#298 = ORIENTED_EDGE ( 'NONE', *, *, #33062, .T. ) ;
#299 = CARTESIAN_POINT ( 'NONE',  ( -27.08702828306202193, -0.5765135930295117728, 2.226264228965860070 ) ) ;
#300 = ORIENTED_EDGE ( 'NONE', *, *, #9759, .F. ) ;
#301 = CYLINDRICAL_SURFACE ( 'NONE', #23785, 4.999999999999999112 ) ;
#302 = CARTESIAN_POINT ( 'NONE',  ( 36.00000000000000711, 1.457575200925544934, -12.66641127287626567 ) ) ;
#303 = B_SPLINE_CURVE_WITH_KNOTS ( 'NONE', 3,
 ( #44114, #19168, #39439, #59738, #4206, #61353, #15793, #39778, #54761, #14486, #10485, #24820, #45746, #4874, #9181, #29458 ),
 .UNSPECIFIED., .F., .F.,
 ( 4, 3, 3, 3, 3, 4 ),
 ( 0.000000000000000000, 0.0002176109881720250270, 0.0004352086762394614256, 0.0006528017811446909773, 0.0007615147961451746621, 0.0009453342004947338107 ),
 .UNSPECIFIED. ) ;
#304 = CIRCLE ( 'NONE', #21567, 6.936499999999989008 ) ;
#305 = CARTESIAN_POINT ( 'NONE',  ( -22.27218376572352554, -3.547715993389675582, 0.9890213205919727857 ) ) ;
#306 = CARTESIAN_POINT ( 'NONE',  ( 0.3675815128205912052, -11.62724744438068569, 3.951233083390429446 ) ) ;
#307 = VECTOR ( 'NONE', #56220, 1000.000000000000000 ) ;
#308 = ORIENTED_EDGE ( 'NONE', *, *, #52732, .F. ) ;
#309 = ORIENTED_EDGE ( 'NONE', *, *, #45374, .F. ) ;
#310 = CARTESIAN_POINT ( 'NONE',  ( -30.12760453383368286, -0.2822123306220293837, 11.99877405949625242 ) ) ;
#311 = VERTEX_POINT ( 'NONE', #11457 ) ;
#312 = CARTESIAN_POINT ( 'NONE',  ( -27.45775109278351067, -10.51123867646838050, -8.471355351200609007 ) ) ;
#313 = DIRECTION ( 'NONE',  ( 0.000000000000000000, 0.000000000000000000, 1.000000000000000000 ) ) ;
#314 = CARTESIAN_POINT ( 'NONE',  ( 2.903928887688428162, -8.044738195288756444, 3.491800274468522591 ) ) ;
#315 = CARTESIAN_POINT ( 'NONE',  ( 0.3675815128205894289, 9.235491948680119023, -8.093875121225982738 ) ) ;
#316 = CARTESIAN_POINT ( 'NONE',  ( -11.40165637463000259, -7.955952249420155553, 10.91980268859785141 ) ) ;
#317 = CARTESIAN_POINT ( 'NONE',  ( -11.37368538729251277, -6.793519583034608011, 9.901714675131643162 ) ) ;
#318 = ORIENTED_EDGE ( 'NONE', *, *, #52044, .T. ) ;
#319 = ADVANCED_FACE ( 'NONE', ( #1518 ), #2557, .F. ) ;
#320 = CARTESIAN_POINT ( 'NONE',  ( 2.000000000000001776, -4.962980376314093611, 4.846014654777763830 ) ) ;
#321 = EDGE_LOOP ( 'NONE', ( #20951, #13092, #29653, #40953 ) ) ;
#322 = CARTESIAN_POINT ( 'NONE',  ( -35.00000000000000000, 1.039216533673073206, -11.70009620280410445 ) ) ;
#323 = EDGE_CURVE ( 'NONE', #38878, #54941, #51144, .T. ) ;
#324 = FACE_OUTER_BOUND ( 'NONE', #21670, .T. ) ;
#325 = VERTEX_POINT ( 'NONE', #18102 ) ;
#326 = FACE_OUTER_BOUND ( 'NONE', #43910, .T. ) ;
#327 = ORIENTED_EDGE ( 'NONE', *, *, #30537, .F. ) ;
#328 = CARTESIAN_POINT ( 'NONE',  ( 0.2648978790185584908, 0.1321385342564118659, -12.24533305150758089 ) ) ;
#329 = CARTESIAN_POINT ( 'NONE',  ( -37.00000000000000711, -10.54834585426215732, -6.102719229070786788 ) ) ;
#330 = CARTESIAN_POINT ( 'NONE',  ( 35.00000000000000000, 1.285879139104720949E-14, 0.000000000000000000 ) ) ;
#331 = CARTESIAN_POINT ( 'NONE',  ( -27.09125059358652976, -2.243253600381622803, -0.5611156659262992452 ) ) ;
#332 = VERTEX_POINT ( 'NONE', #63974 ) ;
#333 = ORIENTED_EDGE ( 'NONE', *, *, #41127, .T. ) ;
#334 = CARTESIAN_POINT ( 'NONE',  ( 0.000000000000000000, 0.000000000000000000, 0.000000000000000000 ) ) ;
#335 = ORIENTED_EDGE ( 'NONE', *, *, #60895, .T. ) ;
#336 = CARTESIAN_POINT ( 'NONE',  ( 1.283627346226758892, -12.00363697230095994, -3.783098238613510578 ) ) ;
#337 = ORIENTED_EDGE ( 'NONE', *, *, #61367, .T. ) ;
#338 = VECTOR ( 'NONE', #37910, 1000.000000000000000 ) ;
#339 = AXIS2_PLACEMENT_3D ( 'NONE', #1310, #57489, #57162 ) ;
#340 = EDGE_LOOP ( 'NONE', ( #633, #26710, #31623, #29348 ) ) ;
#341 = EDGE_LOOP ( 'NONE', ( #2410, #23856, #26253, #58156 ) ) ;
#342 = FACE_OUTER_BOUND ( 'NONE', #65268, .T. ) ;
#343 = EDGE_CURVE ( 'NONE', #56731, #58632, #17524, .T. ) ;
#344 = CARTESIAN_POINT ( 'NONE',  ( 2.241352910868908754, -7.532448145350516988, 1.243507963608069700 ) ) ;
#345 = AXIS2_PLACEMENT_3D ( 'NONE', #43283, #37319, #57631 ) ;
#346 = CARTESIAN_POINT ( 'NONE',  ( 5.514624014163232779, 0.002216125254993209052, -0.003498325728817969996 ) ) ;
#347 = FACE_OUTER_BOUND ( 'NONE', #44647, .T. ) ;
#348 = LINE ( 'NONE', #20626, #43001 ) ;
#349 = EDGE_LOOP ( 'NONE', ( #5413, #53685, #34393, #20305 ) ) ;
#350 = DIRECTION ( 'NONE',  ( 1.000000000000000000, 0.000000000000000000, 0.000000000000000000 ) ) ;
#351 = ORIENTED_EDGE ( 'NONE', *, *, #15803, .T. ) ;
#352 = CARTESIAN_POINT ( 'NONE',  ( -17.29244623348158783, 2.525873743887551814, 13.26159725786978960 ) ) ;
#353 = CARTESIAN_POINT ( 'NONE',  ( -22.27706485742869091, 2.625261754997705310, -2.580541389029900934 ) ) ;
#354 = CARTESIAN_POINT ( 'NONE',  ( -27.59804998575971169, 11.74707290664110637, -6.658303971331236859 ) ) ;
#355 = VECTOR ( 'NONE', #27928, 1000.000000000000000 ) ;
#356 = CARTESIAN_POINT ( 'NONE',  ( 29.03457606387295087, 4.854210015632069997, 10.97436308512422265 ) ) ;
#357 = CARTESIAN_POINT ( 'NONE',  ( 1.375507693220682448, -10.61839108744987925, -6.813306181536405326 ) ) ;
#358 = EDGE_CURVE ( 'NONE', #57018, #62845, #48344, .T. ) ;
#359 = VECTOR ( 'NONE', #61792, 1000.000000000000000 ) ;
#360 = ORIENTED_EDGE ( 'NONE', *, *, #31909, .T. ) ;
#361 = LINE ( 'NONE', #6019, #33319 ) ;
#362 = AXIS2_PLACEMENT_3D ( 'NONE', #13702, #44294, #38671 ) ;
#363 = ORIENTED_EDGE ( 'NONE', *, *, #32286, .F. ) ;
#364 = CARTESIAN_POINT ( 'NONE',  ( 12.47628546223243617, 0.000000000000000000, 13.50000000000000178 ) ) ;
#365 = DIRECTION ( 'NONE',  ( -1.000000000000000000, 0.000000000000000000, 0.000000000000000000 ) ) ;
#366 = AXIS2_PLACEMENT_3D ( 'NONE', #23570, #33544, #18606 ) ;
#367 = CARTESIAN_POINT ( 'NONE',  ( 2.931247277082682068, 6.988361004535491361, -3.607110715259676859 ) ) ;
#368 = CARTESIAN_POINT ( 'NONE',  ( -10.90165637462999904, -7.508992741355383416, -9.360289953322597611 ) ) ;
#369 = CARTESIAN_POINT ( 'NONE',  ( -35.00000000000000000, 0.000000000000000000, 0.000000000000000000 ) ) ;
#370 = ORIENTED_EDGE ( 'NONE', *, *, #43413, .T. ) ;
#371 = DIRECTION ( 'NONE',  ( -1.000000000000000000, 0.000000000000000000, 0.000000000000000000 ) ) ;
#372 = CARTESIAN_POINT ( 'NONE',  ( 36.00000000000000711, 0.3137578094511053184, 12.74613886779084204 ) ) ;
#373 = CARTESIAN_POINT ( 'NONE',  ( 21.64884475953936160, 11.05386968847107454, -4.688304422177896669 ) ) ;
#374 = CARTESIAN_POINT ( 'NONE',  ( 35.00000000000000000, 8.854740511458958352, 7.717887834988148121 ) ) ;
#375 = CIRCLE ( 'NONE', #17362, 2.899999999999995026 ) ;
#376 = EDGE_CURVE ( 'NONE', #58777, #10202, #63172, .T. ) ;
#377 = CARTESIAN_POINT ( 'NONE',  ( -21.04919400413958286, 12.98042452237757516, -3.710884547572586900 ) ) ;
#378 = CARTESIAN_POINT ( 'NONE',  ( 3.152665057734130638, -4.725420687650661478, -6.378477742800524375 ) ) ;
#379 = EDGE_CURVE ( 'NONE', #7202, #39390, #41905, .T. ) ;
#380 = CARTESIAN_POINT ( 'NONE',  ( -37.00000000000000711, 10.80478261802190154, -5.636262487437199376 ) ) ;
#381 = CARTESIAN_POINT ( 'NONE',  ( -37.00000000000000711, -6.280308599560071592, -9.926225166347094842 ) ) ;
#382 = DIRECTION ( 'NONE',  ( 0.000000000000000000, 0.1740410799127543318, 0.9847383929261630531 ) ) ;
#383 = VECTOR ( 'NONE', #63975, 1000.000000000000000 ) ;
#384 = AXIS2_PLACEMENT_3D ( 'NONE', #29738, #61009, #5154 ) ;
#385 = VECTOR ( 'NONE', #46411, 1000.000000000000000 ) ;
#386 = CIRCLE ( 'NONE', #53354, 12.74999999999999822 ) ;
#387 = EDGE_CURVE ( 'NONE', #44901, #11376, #34493, .T. ) ;
#388 = ORIENTED_EDGE ( 'NONE', *, *, #52425, .T. ) ;
#389 = ORIENTED_EDGE ( 'NONE', *, *, #15138, .T. ) ;
#390 = LINE ( 'NONE', #40941, #307 ) ;
#391 = CARTESIAN_POINT ( 'NONE',  ( 36.99853283657033387, -2.301590494557431477, -20.84413141647362266 ) ) ;
#392 = DIRECTION ( 'NONE',  ( 0.000000000000000000, 0.000000000000000000, 1.000000000000000000 ) ) ;
#393 = AXIS2_PLACEMENT_3D ( 'NONE', #15543, #5604, #5260 ) ;
#394 = CARTESIAN_POINT ( 'NONE',  ( 2.241449424704146320, 3.870245369721822648, 6.580749518451812108 ) ) ;
#395 = VERTEX_POINT ( 'NONE', #38712 ) ;
#396 = EDGE_CURVE ( 'NONE', #8331, #58552, #45570, .T. ) ;
#397 = AXIS2_PLACEMENT_3D ( 'NONE', #55947, #25689, #45980 ) ;
#398 = ORIENTED_EDGE ( 'NONE', *, *, #32115, .T. ) ;
#399 = ORIENTED_EDGE ( 'NONE', *, *, #28460, .T. ) ;
#400 = DIRECTION ( 'NONE',  ( 1.000000000000000000, 0.000000000000000000, -0.000000000000000000 ) ) ;
#401 = VECTOR ( 'NONE', #10763, 1000.000000000000114 ) ;
#402 = CARTESIAN_POINT ( 'NONE',  ( 35.00000000000000000, 1.488153103996963100, -11.65150730582935523 ) ) ;
#403 = EDGE_LOOP ( 'NONE', ( #55251, #13058, #53258, #22516 ) ) ;
#404 = CARTESIAN_POINT ( 'NONE',  ( 2.903928887688316252, -0.5297564406061211484, -8.753847148606094919 ) ) ;
#405 = CARTESIAN_POINT ( 'NONE',  ( 35.00000000000000000, -9.076753354953932984, 8.954052073409695112 ) ) ;
#406 = DIRECTION ( 'NONE',  ( 0.000000000000000000, 0.01356324068817998940, -0.9999080150203989437 ) ) ;
#407 = ORIENTED_EDGE ( 'NONE', *, *, #56725, .T. ) ;
#408 = AXIS2_PLACEMENT_3D ( 'NONE', #57980, #3109, #2452 ) ;
#409 = CARTESIAN_POINT ( 'NONE',  ( 2.889800649504073782, 2.030191121417136646, 5.774917447013004690 ) ) ;
#410 =( BOUNDED_SURFACE ( )  B_SPLINE_SURFACE ( 3, 1, ( 
 ( #23398, #43669 ),
 ( #12102, #63958 ),
 ( #38699, #23746 ),
 ( #28707, #49020 ) ),
 .UNSPECIFIED., .F., .F., .F. ) 
 B_SPLINE_SURFACE_WITH_KNOTS ( ( 4, 4 ),
 ( 2, 2 ),
 ( 0.000000000000000000, 1.000000000000000000 ),
 ( 0.000000000000000000, 1.000000000000000000 ),
 .UNSPECIFIED. ) 
 GEOMETRIC_REPRESENTATION_ITEM ( )  RATIONAL_B_SPLINE_SURFACE ( (
 ( 1.000000000000000000, 1.000000000000000000),
 ( 0.9942764183789327692, 0.8450855930916585379),
 ( 0.9942764183789327692, 0.8450855930916585379),
 ( 1.000000000000000000, 1.000000000000000000) ) ) 
 REPRESENTATION_ITEM ( '' )  SURFACE ( )  );
#411 = VECTOR ( 'NONE', #62714, 1000.000000000000000 ) ;
#412 = CARTESIAN_POINT ( 'NONE',  ( -5.808548865028119401, -28.57390223679843544, -12.95295593664668310 ) ) ;
#413 = CARTESIAN_POINT ( 'NONE',  ( 5.515539859299206427, 0.005618668168217187849, 0.002251761459665550975 ) ) ;
#414 = ORIENTED_EDGE ( 'NONE', *, *, #15796, .T. ) ;
#415 = CARTESIAN_POINT ( 'NONE',  ( 35.00000000000000000, 10.80631716521673447, 4.603882218679430594 ) ) ;
#416 = VERTEX_POINT ( 'NONE', #33391 ) ;
#417 = CARTESIAN_POINT ( 'NONE',  ( -29.92777678363736626, -3.750539801530011985, -11.39883551934752681 ) ) ;
#418 = ORIENTED_EDGE ( 'NONE', *, *, #52411, .F. ) ;
#419 = CARTESIAN_POINT ( 'NONE',  ( -22.66110217412718697, 4.192227617777429138, 2.622110956932540038 ) ) ;
#420 = CARTESIAN_POINT ( 'NONE',  ( 2.000000000000001776, 0.000000000000000000, 0.000000000000000000 ) ) ;
#421 = FACE_OUTER_BOUND ( 'NONE', #30596, .T. ) ;
#422 = CARTESIAN_POINT ( 'NONE',  ( 26.08439714455133185, 25.00000000000000000, 3.743551691817327942 ) ) ;
#423 = AXIS2_PLACEMENT_3D ( 'NONE', #17587, #51850, #16598 ) ;
#424 = CARTESIAN_POINT ( 'NONE',  ( 0.2671309869109501633, -12.24572650704445032, 0.1620273132355259660 ) ) ;
#425 = CARTESIAN_POINT ( 'NONE',  ( 37.00000000000000711, 4.705694406421931860E-17, -3.469127814946512892E-15 ) ) ;
#426 = CARTESIAN_POINT ( 'NONE',  ( 25.00000000000000711, -30.00000000000000000, -24.00000000000000000 ) ) ;
#427 = CARTESIAN_POINT ( 'NONE',  ( 35.00000000000000000, -6.475373545682373333, -10.32377448871666026 ) ) ;
#429 = VERTEX_POINT ( 'NONE', #22 ) ;
#428 = CARTESIAN_POINT ( 'NONE',  ( 35.00000000000000000, 3.704519465651471499, 11.60979404548630178 ) ) ;
#430 = DIRECTION ( 'NONE',  ( 1.000000000000000000, 0.000000000000000000, -0.000000000000000000 ) ) ;
#431 = ORIENTED_EDGE ( 'NONE', *, *, #26732, .T. ) ;
#432 = CARTESIAN_POINT ( 'NONE',  ( 12.60173367434126490, -10.92909900068726792, -7.935196926251238736 ) ) ;
#433 = VERTEX_POINT ( 'NONE', #2833 ) ;
#434 = DIRECTION ( 'NONE',  ( 1.000000000000000000, 0.000000000000000000, 0.000000000000000000 ) ) ;
#435 = VECTOR ( 'NONE', #47244, 1000.000000000000000 ) ;
#436 = ORIENTED_EDGE ( 'NONE', *, *, #2172, .F. ) ;
#438 = CIRCLE ( 'NONE', #2582, 12.18650000000000055 ) ;
#437 = DIRECTION ( 'NONE',  ( 0.000000000000000000, 0.3554799084908900619, 0.9346839223284567622 ) ) ;
#439 = CARTESIAN_POINT ( 'NONE',  ( 0.8375941296816026282, 11.81283813871928068, -3.890418817177600186 ) ) ;
#440 = CARTESIAN_POINT ( 'NONE',  ( -27.20102706715913143, -0.8206313329275967128, -2.512061365242614919 ) ) ;
#441 = CIRCLE ( 'NONE', #54549, 6.936499999999987232 ) ;
#442 = EDGE_CURVE ( 'NONE', #3284, #31374, #16898, .T. ) ;
#443 = CARTESIAN_POINT ( 'NONE',  ( -37.00000000000000711, -11.71932350927023414, 3.511386971104904386 ) ) ;
#444 = EDGE_LOOP ( 'NONE', ( #60169, #14313, #42330, #32413 ) ) ;
#445 = CARTESIAN_POINT ( 'NONE',  ( 35.00000000000000000, 10.30098186818249673, -5.644643009979106729 ) ) ;
#446 = VECTOR ( 'NONE', #37071, 1000.000000000000000 ) ;
#447 = ORIENTED_EDGE ( 'NONE', *, *, #54741, .T. ) ;
#448 = FACE_BOUND ( 'NONE', #52190, .T. ) ;
#449 = CARTESIAN_POINT ( 'NONE',  ( 35.00000000000000000, 11.02904044024202967, -4.041347439436060007 ) ) ;
#450 = CARTESIAN_POINT ( 'NONE',  ( -35.00000000000000000, 4.426194442447240363, 11.35427606708807957 ) ) ;
#451 = VERTEX_POINT ( 'NONE', #48384 ) ;
#452 = DIRECTION ( 'NONE',  ( -1.000000000000000000, 0.000000000000000000, 0.000000000000000000 ) ) ;
#453 = AXIS2_PLACEMENT_3D ( 'NONE', #38158, #23546, #33523 ) ;
#454 = ADVANCED_FACE ( 'NONE', ( #53690 ), #60537, .T. ) ;
#455 = EDGE_CURVE ( 'NONE', #51352, #10755, #51524, .T. ) ;
#456 = CARTESIAN_POINT ( 'NONE',  ( -35.04709527796842394, 0.001003525937978352878, -0.01232256164996822778 ) ) ;
#457 = DIRECTION ( 'NONE',  ( 0.000000000000000000, 0.01356324068818000848, -0.9999080150203990547 ) ) ;
#458 = ADVANCED_FACE ( 'NONE', ( #18456 ), #8446, .T. ) ;
#459 = AXIS2_PLACEMENT_3D ( 'NONE', #21770, #46690, #52988 ) ;
#460 = CARTESIAN_POINT ( 'NONE',  ( 36.00000000000000711, -12.21925492305364713, -3.640372113593510761 ) ) ;
#461 = CARTESIAN_POINT ( 'NONE',  ( 0.2956976708475502202, -5.936640677855288040, -10.72256944221093811 ) ) ;
#462 = EDGE_CURVE ( 'NONE', #46347, #21361, #20738, .T. ) ;
#463 = ORIENTED_EDGE ( 'NONE', *, *, #54480, .T. ) ;
#464 = DIRECTION ( 'NONE',  ( 1.000000000000000000, 0.000000000000000000, 0.000000000000000000 ) ) ;
#465 = CARTESIAN_POINT ( 'NONE',  ( 15.59244419633153456, -34.16973227397373591, 7.752328951095602605 ) ) ;
#466 = CARTESIAN_POINT ( 'NONE',  ( 0.9296196016843265575, -3.871279966919617621, -11.85136013469065475 ) ) ;
#467 = CIRCLE ( 'NONE', #37622, 12.73084802173761787 ) ;
#468 = EDGE_CURVE ( 'NONE', #3878, #65629, #14971, .T. ) ;
#469 = CARTESIAN_POINT ( 'NONE',  ( 0.2646305136544072623, 9.465888453932963742, 7.770320294339208900 ) ) ;
#470 = CARTESIAN_POINT ( 'NONE',  ( -14.11589373245165469, 8.250315036047107142, -10.68561190601526256 ) ) ;
#471 = ORIENTED_EDGE ( 'NONE', *, *, #2353, .F. ) ;
#472 = CARTESIAN_POINT ( 'NONE',  ( 0.4626703367442831505, 10.51809671647419542, 6.399577980714641789 ) ) ;
#473 = EDGE_CURVE ( 'NONE', #55881, #65529, #14365, .T. ) ;
#474 = CYLINDRICAL_SURFACE ( 'NONE', #40618, 12.74999999999999822 ) ;
#475 = CARTESIAN_POINT ( 'NONE',  ( -22.28284753389937478, 3.563226652211057388, -0.9912969289936535144 ) ) ;
#476 = VERTEX_POINT ( 'NONE', #20306 ) ;
#477 = CARTESIAN_POINT ( 'NONE',  ( 35.00000000000000000, -11.80185301892977279, 4.824807283154242121 ) ) ;
#478 = CARTESIAN_POINT ( 'NONE',  ( 35.00000000000000000, 11.73808581813437080, -0.4353888892050498116 ) ) ;
#479 = ORIENTED_EDGE ( 'NONE', *, *, #27553, .F. ) ;
#480 = AXIS2_PLACEMENT_3D ( 'NONE', #59042, #13770, #54378 ) ;
#481 = AXIS2_PLACEMENT_3D ( 'NONE', #42373, #6510, #550 ) ;
#482 = ORIENTED_EDGE ( 'NONE', *, *, #61735, .F. ) ;
#483 = ORIENTED_EDGE ( 'NONE', *, *, #25990, .F. ) ;
#484 = EDGE_LOOP ( 'NONE', ( #30253, #3866, #979, #57703 ) ) ;
#485 = EDGE_CURVE ( 'NONE', #64690, #35052, #56203, .T. ) ;
#486 = CARTESIAN_POINT ( 'NONE',  ( 2.655192694324243430, 8.589732161578094605, 4.290256727311597906 ) ) ;
#487 = DIRECTION ( 'NONE',  ( 0.000000000000000000, -0.7381862504171878836, 0.6745969609292743474 ) ) ;
#488 = CARTESIAN_POINT ( 'NONE',  ( -35.00000000000000000, 0.000000000000000000, 0.000000000000000000 ) ) ;
#489 = CARTESIAN_POINT ( 'NONE',  ( 6.812204945636112896, -4.138731716409435712, 11.26369831714195335 ) ) ;
#490 = CARTESIAN_POINT ( 'NONE',  ( -4.989057617119008192, -0.9162120371760335003, 13.46887357958837406 ) ) ;
#491 = CARTESIAN_POINT ( 'NONE',  ( -12.26308380404417164, -33.73908083898199806, 10.29207979367737380 ) ) ;
#492 = CARTESIAN_POINT ( 'NONE',  ( 24.83805482081016791, -1.521295006216393908, -13.41549933947825224 ) ) ;
#494 = ORIENTED_EDGE ( 'NONE', *, *, #26778, .F. ) ;
#493 = CARTESIAN_POINT ( 'NONE',  ( 35.00000000000000000, 10.42955799785319648, -6.303578524886984447 ) ) ;
#495 = PLANE ( 'NONE',  #171 ) ;
#496 = ORIENTED_EDGE ( 'NONE', *, *, #1465, .F. ) ;
#497 = DIRECTION ( 'NONE',  ( -1.000000000000000000, 0.000000000000000000, 0.000000000000000000 ) ) ;
#498 = EDGE_LOOP ( 'NONE', ( #38392, #765, #24138, #47981 ) ) ;
#499 = ORIENTED_EDGE ( 'NONE', *, *, #57601, .F. ) ;
#500 = CARTESIAN_POINT ( 'NONE',  ( -22.29978294495153790, -0.8878583829805396510, 3.642708310327676280 ) ) ;
#501 = CARTESIAN_POINT ( 'NONE',  ( 10.20102756488484275, -27.72270395345634952, 14.27139701651698722 ) ) ;
#502 = AXIS2_PLACEMENT_3D ( 'NONE', #24845, #9864, #15502 ) ;
#503 = DIRECTION ( 'NONE',  ( -1.000000000000000000, -0.000000000000000000, 0.000000000000000000 ) ) ;
#504 = CYLINDRICAL_SURFACE ( 'NONE', #54627, 5.000000000000000888 ) ;
#505 = CYLINDRICAL_SURFACE ( 'NONE', #15469, 5.000000000000000888 ) ;
#506 = CARTESIAN_POINT ( 'NONE',  ( 0.3006302518452033112, -12.03044280705496050, 2.350739146140553792 ) ) ;
#507 = EDGE_LOOP ( 'NONE', ( #54481, #11346, #34608, #56245 ) ) ;
#508 = ORIENTED_EDGE ( 'NONE', *, *, #5192, .T. ) ;
#509 = DIRECTION ( 'NONE',  ( 1.000000000000000000, -0.000000000000000000, -0.000000000000000000 ) ) ;
#510 = ORIENTED_EDGE ( 'NONE', *, *, #14071, .T. ) ;
#511 = ORIENTED_EDGE ( 'NONE', *, *, #46854, .F. ) ;
#512 = CARTESIAN_POINT ( 'NONE',  ( 2.000000000000001776, 0.000000000000000000, 0.000000000000000000 ) ) ;
#513 = CARTESIAN_POINT ( 'NONE',  ( -35.00000000000000000, -10.99909370905153594, -5.246972444134134328 ) ) ;
#514 = CARTESIAN_POINT ( 'NONE',  ( -22.29978294495153790, 0.8878583829805657412, -3.642708310327676280 ) ) ;
#515 = CARTESIAN_POINT ( 'NONE',  ( 17.41455116976016981, 8.220693008476809283, 8.757759849264344254 ) ) ;
#516 = CARTESIAN_POINT ( 'NONE',  ( 2.259830038564999644, 7.639319632525575443, 0.1377140217659458543 ) ) ;
#517 = ADVANCED_FACE ( 'NONE', ( #51579 ), #45917, .T. ) ;
#518 = CARTESIAN_POINT ( 'NONE',  ( -5.884299113211928223, -0.9870258725403491251, -11.95978215124650923 ) ) ;
#519 = AXIS2_PLACEMENT_3D ( 'NONE', #15215, #29220, #49515 ) ;
#520 = CARTESIAN_POINT ( 'NONE',  ( -22.27721698446158172, -0.6951119527727915859, -3.615509722105072044 ) ) ;
#521 = ORIENTED_EDGE ( 'NONE', *, *, #24511, .T. ) ;
#522 = CARTESIAN_POINT ( 'NONE',  ( 2.000000000000001776, -3.979254915827311390, -5.681598592373819478 ) ) ;
#523 = VECTOR ( 'NONE', #9694, 1000.000000000000000 ) ;
#524 = LINE ( 'NONE', #25127, #20210 ) ;
#525 = EDGE_CURVE ( 'NONE', #52168, #55868, #30598, .T. ) ;
#526 = CARTESIAN_POINT ( 'NONE',  ( -3.378459980749651148, -10.08685364769616299, 9.001353960567275436 ) ) ;
#527 = DIRECTION ( 'NONE',  ( -1.000000000000000000, -0.000000000000000000, 0.000000000000000000 ) ) ;
#528 = EDGE_CURVE ( 'NONE', #9921, #51290, #11199, .T. ) ;
#529 = CARTESIAN_POINT ( 'NONE',  ( 35.00000000000000000, 11.42599468261429152, -4.237620530777845396 ) ) ;
#530 = VECTOR ( 'NONE', #52703, 1000.000000000000227 ) ;
#531 = DIRECTION ( 'NONE',  ( 0.000000000000000000, 0.9985334138511239299, -0.05413890858541457046 ) ) ;
#532 = EDGE_CURVE ( 'NONE', #49256, #59168, #43953, .T. ) ;
#533 = CARTESIAN_POINT ( 'NONE',  ( 37.00000000000000711, 2.696588552979229725, 12.46157735505186004 ) ) ;
#534 = CARTESIAN_POINT ( 'NONE',  ( 2.000000000000001776, 6.250523986464036064, -3.007653927006531447 ) ) ;
#535 = EDGE_CURVE ( 'NONE', #13015, #47412, #20651, .T. ) ;
#536 = ORIENTED_EDGE ( 'NONE', *, *, #57948, .T. ) ;
#537 = AXIS2_PLACEMENT_3D ( 'NONE', #40562, #25944, #41206 ) ;
#538 = CARTESIAN_POINT ( 'NONE',  ( 0.2653519890518156732, 10.60552241699067544, 6.123091032184181159 ) ) ;
#539 = DIRECTION ( 'NONE',  ( 0.000000000000000000, -0.6745969609292555846, -0.7381862504172049810 ) ) ;
#540 = LINE ( 'NONE', #61351, #50346 ) ;
#541 = AXIS2_PLACEMENT_3D ( 'NONE', #51689, #37348, #57984 ) ;
#542 = CARTESIAN_POINT ( 'NONE',  ( -15.05999060605171458, -34.74914171045087841, -6.965575872675125346 ) ) ;
#543 = CYLINDRICAL_SURFACE ( 'NONE', #45743, 12.75000000000000178 ) ;
#544 = ORIENTED_EDGE ( 'NONE', *, *, #30185, .F. ) ;
#545 = CARTESIAN_POINT ( 'NONE',  ( -19.17721427606680251, -3.894607805094318032, -12.92689141258588847 ) ) ;
#546 = CARTESIAN_POINT ( 'NONE',  ( 1.937114397841932290, -12.80345148322678561, -0.9020203649533019563 ) ) ;
#547 = ADVANCED_FACE ( 'NONE', ( #26942 ), #6028, .T. ) ;
#548 = CARTESIAN_POINT ( 'NONE',  ( 15.30590914263659386, -28.05839919878968303, -10.93630420992710128 ) ) ;
#549 = ORIENTED_EDGE ( 'NONE', *, *, #20317, .T. ) ;
#550 = DIRECTION ( 'NONE',  ( 0.000000000000000000, -0.01356324068817998940, 0.9999080150203990547 ) ) ;
#551 = DIRECTION ( 'NONE',  ( 0.000000000000000000, 0.000000000000000000, 1.000000000000000000 ) ) ;
#552 = CYLINDRICAL_SURFACE ( 'NONE', #25924, 4.999999999999999112 ) ;
#553 = EDGE_CURVE ( 'NONE', #5802, #65741, #4808, .T. ) ;
#555 = ORIENTED_EDGE ( 'NONE', *, *, #41297, .F. ) ;
#554 = LINE ( 'NONE', #31449, #3124 ) ;
#556 = B_SPLINE_CURVE_WITH_KNOTS ( 'NONE', 3,
 ( #63039, #7858, #51545, #7500, #658, #6873, #56507, #1875, #12169, #47438, #22145, #2879, #2553, #27143, #33103, #23135, #10952, #42744, #32440, #62695, #52750, #63355, #20917, #31239, #5658, #61474, #28134, #48097, #22822, #32755, #17162, #37439, #43078, #12481, #18153, #53412, #27793, #25927, #47754, #17821, #57750, #46216, #33445, #17503, #15916, #37773, #53064, #2203, #7174, #36200, #38426, #41191, #22481, #38086 ),
 .UNSPECIFIED., .F., .F.,
 ( 4, 2, 2, 2, 2, 2, 2, 2, 2, 2, 2, 2, 2, 2, 2, 2, 2, 2, 2, 2, 2, 2, 2, 2, 2, 2, 4 ),
 ( 0.000000000000000000, 0.004712545709777801912, 0.007068818564666702435, 0.009425091419555603825, 0.01413763712933342048, 0.01649390998422233315, 0.01885018283911124234, 0.02356272854888905727, 0.02591900140377796299, 0.02827527425866686525, 0.03063154711355577098, 0.03180968354100022211, 0.03298781996844467324, 0.03770036567822248469, 0.04005663853311138001, 0.04123477496055583114, 0.04241291138800028920, 0.04712545709777810760, 0.04948172995266700985, 0.05183800280755592599, 0.05655054851733373744, 0.06126309422711155583, 0.06361936708200047197, 0.06597563993688937423, 0.07068818564666717874, 0.07304445850155608100, 0.07540073135644498326 ),
 .UNSPECIFIED. ) ;
#557 = CARTESIAN_POINT ( 'NONE',  ( -27.09125059358652265, 2.243253600381615698, 0.5611156659262670487 ) ) ;
#558 = EDGE_CURVE ( 'NONE', #56170, #24551, #58977, .T. ) ;
#559 = CARTESIAN_POINT ( 'NONE',  ( 3.092491956585621260, -7.581757403488263769, -2.283527081234276057 ) ) ;
#560 = ORIENTED_EDGE ( 'NONE', *, *, #56639, .F. ) ;
#561 = EDGE_CURVE ( 'NONE', #2301, #2844, #15412, .T. ) ;
#562 = DIRECTION ( 'NONE',  ( -0.4327406564646559262, 0.9015184547431841500, 0.000000000000000000 ) ) ;
#563 = CARTESIAN_POINT ( 'NONE',  ( -27.08871896697694837, 1.309412067288143078, 1.896680818244922850 ) ) ;
#564 = CARTESIAN_POINT ( 'NONE',  ( 24.06146064158421538, -2.489685948191276310, -11.74338419841854098 ) ) ;
#565 = CARTESIAN_POINT ( 'NONE',  ( 8.449549814414584858, 4.860417429574915182, -12.59635262386618137 ) ) ;
#566 = DIRECTION ( 'NONE',  ( 0.000000000000000000, 0.4935949184179201366, -0.8696919319575217022 ) ) ;
#567 = ADVANCED_FACE ( 'NONE', ( #41231 ), #60880, .T. ) ;
#568 = CARTESIAN_POINT ( 'NONE',  ( 37.00000000000000711, 1.113475361586665491, 12.70128625845191195 ) ) ;
#569 = LINE ( 'NONE', #20831, #8503 ) ;
#570 = MECHANICAL_DESIGN_GEOMETRIC_PRESENTATION_REPRESENTATION (  '', ( #52641 ), #64299 ) ;
#571 = ORIENTED_EDGE ( 'NONE', *, *, #34753, .T. ) ;
#572 = CARTESIAN_POINT ( 'NONE',  ( 2.284126774967664364, -5.036818232552930041, 5.756079777200394432 ) ) ;
#573 = ORIENTED_EDGE ( 'NONE', *, *, #35161, .T. ) ;
#574 = DIRECTION ( 'NONE',  ( -1.149254302834639630E-17, 1.000000000000000000, -2.775557561562903061E-17 ) ) ;
#575 = DIRECTION ( 'NONE',  ( 1.000000000000000000, 0.000000000000000000, -0.000000000000000000 ) ) ;
#576 = CARTESIAN_POINT ( 'NONE',  ( 0.2648321136542706178, 11.45826514585342970, 4.321267941897541043 ) ) ;
#577 = LINE ( 'NONE', #31779, #44701 ) ;
#578 = ORIENTED_EDGE ( 'NONE', *, *, #49298, .F. ) ;
#579 = CARTESIAN_POINT ( 'NONE',  ( -35.00000000000000000, 4.309077947445652867, 10.92721691015457708 ) ) ;
#580 = AXIS2_PLACEMENT_3D ( 'NONE', #12761, #33050, #53357 ) ;
#581 = DIRECTION ( 'NONE',  ( 0.000000000000000000, 0.000000000000000000, 1.000000000000000000 ) ) ;
#582 = DIRECTION ( 'NONE',  ( 0.000000000000000000, 0.7381862504171926576, -0.6745969609292691294 ) ) ;
#583 = ORIENTED_EDGE ( 'NONE', *, *, #15533, .F. ) ;
#584 = ORIENTED_EDGE ( 'NONE', *, *, #3130, .T. ) ;
#585 = CARTESIAN_POINT ( 'NONE',  ( -35.00000000000000000, 0.000000000000000000, 0.000000000000000000 ) ) ;
#586 = EDGE_LOOP ( 'NONE', ( #58558, #49260, #9799, #51354 ) ) ;
#587 = DIRECTION ( 'NONE',  ( 0.000000000000000000, 0.01356324068817998940, -0.9999080150203990547 ) ) ;
#588 = CARTESIAN_POINT ( 'NONE',  ( -27.08485414902839494, 0.5917839443972588986, -2.215517476308472400 ) ) ;
#589 = CARTESIAN_POINT ( 'NONE',  ( -27.08871896697731785, 2.297279805116092977, -0.1856437051692902407 ) ) ;
#590 = AXIS2_PLACEMENT_3D ( 'NONE', #54056, #34078, #29119 ) ;
#591 = CARTESIAN_POINT ( 'NONE',  ( 2.941278708680199916, -2.226055275041829429, 5.721889327162144490 ) ) ;
#592 = EDGE_CURVE ( 'NONE', #6726, #39576, #27098, .T. ) ;
#593 = DIRECTION ( 'NONE',  ( 1.000000000000000000, 0.000000000000000000, -0.000000000000000000 ) ) ;
#594 = CARTESIAN_POINT ( 'NONE',  ( 2.705197763288548884, -7.714317563576063463, 1.076142490489843784 ) ) ;
#595 = DIRECTION ( 'NONE',  ( -0.000000000000000000, -0.000000000000000000, -1.000000000000000000 ) ) ;
#596 = ORIENTED_EDGE ( 'NONE', *, *, #56050, .F. ) ;
#597 =( BOUNDED_SURFACE ( )  B_SPLINE_SURFACE ( 3, 1, ( 
 ( #49658, #4097 ),
 ( #23740, #28066 ),
 ( #48364, #8109 ),
 ( #8428, #29046 ) ),
 .UNSPECIFIED., .F., .F., .F. ) 
 B_SPLINE_SURFACE_WITH_KNOTS ( ( 4, 4 ),
 ( 2, 2 ),
 ( 0.000000000000000000, 1.000000000000000000 ),
 ( 0.000000000000000000, 1.000000000000000000 ),
 .UNSPECIFIED. ) 
 GEOMETRIC_REPRESENTATION_ITEM ( )  RATIONAL_B_SPLINE_SURFACE ( (
 ( 1.000000000000000000, 1.000000000000000000),
 ( 0.6933888150995267674, 0.9895912004443193632),
 ( 0.6933888150995267674, 0.9895912004443193632),
 ( 1.000000000000000000, 1.000000000000000000) ) ) 
 REPRESENTATION_ITEM ( '' )  SURFACE ( )  );
#598 = CARTESIAN_POINT ( 'NONE',  ( 35.00000000000000000, 11.53507381115583108, 2.216820770815121744 ) ) ;
#599 = DIRECTION ( 'NONE',  ( 0.000000000000000000, -0.01356324068817998940, 0.9999080150203990547 ) ) ;
#600 = CARTESIAN_POINT ( 'NONE',  ( 37.00000000000000711, -4.732539170486179891, 11.23004253107769301 ) ) ;
#601 = CARTESIAN_POINT ( 'NONE',  ( 35.00000000000000000, 11.50504120060948487, 4.018060380616274685 ) ) ;
#602 = DIRECTION ( 'NONE',  ( -1.000000000000000000, 0.000000000000000000, -0.000000000000000000 ) ) ;
#603 = CARTESIAN_POINT ( 'NONE',  ( 0.3109076770649076837, -10.73466383006817360, -5.925244271826556108 ) ) ;
#604 = DIRECTION ( 'NONE',  ( -0.3865475372811021937, -0.6938894834606081918, 0.6075346789811139070 ) ) ;
#605 = ADVANCED_FACE ( 'NONE', ( #31279 ), #16314, .T. ) ;
#606 = CARTESIAN_POINT ( 'NONE',  ( 0.3040950598368152291, 4.428852722102732287, 11.43390362554254480 ) ) ;
#607 = AXIS2_PLACEMENT_3D ( 'NONE', #17941, #12282, #63161 ) ;
#608 = ORIENTED_EDGE ( 'NONE', *, *, #47164, .F. ) ;
#609 = CARTESIAN_POINT ( 'NONE',  ( 0.000000000000000000, -1.779948802829851129, 6.576141558201223702 ) ) ;
#610 = ORIENTED_EDGE ( 'NONE', *, *, #32209, .F. ) ;
#611 = CARTESIAN_POINT ( 'NONE',  ( -22.29677679919927868, -3.730758197825073008, 0.2674217835790752007 ) ) ;
#612 = CYLINDRICAL_SURFACE ( 'NONE', #1698, 12.75000000000000178 ) ;
#613 = CARTESIAN_POINT ( 'NONE',  ( 0.2652384770603640751, -12.07140968216695676, 2.061429379240443449 ) ) ;
#614 = CARTESIAN_POINT ( 'NONE',  ( 2.251152103363440293, 2.494172441821923325, -7.218942724308278436 ) ) ;
#615 = EDGE_CURVE ( 'NONE', #42846, #32620, #57927, .T. ) ;
#616 = ORIENTED_EDGE ( 'NONE', *, *, #59826, .T. ) ;
#617 = CARTESIAN_POINT ( 'NONE',  ( -11.08926364416224963, -9.550046432103219018, -9.555892453209455795 ) ) ;
#618 = DIRECTION ( 'NONE',  ( 0.000000000000000000, 0.01356324068817998593, -0.9999080150203990547 ) ) ;
#619 = CARTESIAN_POINT ( 'NONE',  ( 1.014383007554947813, -1.731118468093999496, 12.37541872618881023 ) ) ;
#620 = CARTESIAN_POINT ( 'NONE',  ( -22.71097035706202405, 4.089776368546564456, 2.846599994298306679 ) ) ;
#621 = CARTESIAN_POINT ( 'NONE',  ( 29.03457606387295087, -4.854210015632035358, 10.97436308512422265 ) ) ;
#622 = CARTESIAN_POINT ( 'NONE',  ( 0.000000000000000000, 0.000000000000000000, 0.000000000000000000 ) ) ;
#623 = AXIS2_PLACEMENT_3D ( 'NONE', #44497, #64774, #4635 ) ;
#624 = ORIENTED_EDGE ( 'NONE', *, *, #54431, .T. ) ;
#625 = CARTESIAN_POINT ( 'NONE',  ( -27.09229696323388836, -0.5586335684078734820, 2.247106967996828963 ) ) ;
#626 = ORIENTED_EDGE ( 'NONE', *, *, #10255, .T. ) ;
#627 = CARTESIAN_POINT ( 'NONE',  ( 0.2739690278137269508, -0.1830199730326568797, -12.24770428423990687 ) ) ;
#628 = CARTESIAN_POINT ( 'NONE',  ( 0.3675815128205894289, -2.391755495700522705, -12.04510820461661780 ) ) ;
#629 = CARTESIAN_POINT ( 'NONE',  ( 0.3665391374699472626, -9.237363111276819083, 8.095513416941198415 ) ) ;
#630 = CARTESIAN_POINT ( 'NONE',  ( -10.90165637462998660, -7.182798387602194801, 9.621968923399183637 ) ) ;
#631 = EDGE_CURVE ( 'NONE', #31040, #33343, #47243, .T. ) ;
#632 = CIRCLE ( 'NONE', #37787, 5.000000000000001776 ) ;
#633 = ORIENTED_EDGE ( 'NONE', *, *, #3467, .F. ) ;
#634 = VERTEX_POINT ( 'NONE', #46897 ) ;
#635 = CARTESIAN_POINT ( 'NONE',  ( 36.00000000000000711, 6.564808257521770329, -10.93004082984021252 ) ) ;
#636 = ADVANCED_FACE ( 'NONE', ( #57208 ), #11635, .T. ) ;
#637 = ORIENTED_EDGE ( 'NONE', *, *, #44495, .F. ) ;
#638 = DIRECTION ( 'NONE',  ( 0.000000000000000000, 0.1081190184239353008, 0.9941379571543603744 ) ) ;
#639 = CYLINDRICAL_SURFACE ( 'NONE', #40636, 4.999999999999999112 ) ;
#640 = CARTESIAN_POINT ( 'NONE',  ( -22.27721038036499479, -3.438655654856782373, -1.315315479297514134 ) ) ;
#641 = CARTESIAN_POINT ( 'NONE',  ( 1.549075743843502551, 9.261503792573927640, 8.652116335900316813 ) ) ;
#642 = CARTESIAN_POINT ( 'NONE',  ( 22.68150004936237707, 3.158880575389225065, 11.57756885178368833 ) ) ;
#643 = ADVANCED_FACE ( 'NONE', ( #37224 ), #17294, .T. ) ;
#644 = DIRECTION ( 'NONE',  ( 0.000000000000000000, 0.01356324068818000848, -0.9999080150203990547 ) ) ;
#645 = CARTESIAN_POINT ( 'NONE',  ( 1.198791140422372559, 12.44572864632920606, -1.670544840356793959 ) ) ;
#646 = VERTEX_POINT ( 'NONE', #11962 ) ;
#647 = CARTESIAN_POINT ( 'NONE',  ( 2.835339799623989965, -2.367573116406924694, -7.466040501142053643 ) ) ;
#648 = VERTEX_POINT ( 'NONE', #32243 ) ;
#649 = DIRECTION ( 'NONE',  ( 0.000000000000000000, 0.000000000000000000, 1.000000000000000000 ) ) ;
#650 = CARTESIAN_POINT ( 'NONE',  ( -37.00000000000000711, 7.238157050195776598, -10.49626516989263614 ) ) ;
#651 = CARTESIAN_POINT ( 'NONE',  ( -35.00000000000000000, 9.040300684349693583, 7.499679039484089316 ) ) ;
#652 = ORIENTED_EDGE ( 'NONE', *, *, #58820, .F. ) ;
#653 = CARTESIAN_POINT ( 'NONE',  ( -17.92531974009704498, -29.71422580122558088, 8.391737566679434934 ) ) ;
#654 = ORIENTED_EDGE ( 'NONE', *, *, #45190, .F. ) ;
#655 = CARTESIAN_POINT ( 'NONE',  ( 3.152665057735747567, 7.886634106564638813, 0.9030954876722160352 ) ) ;
#656 = CYLINDRICAL_SURFACE ( 'NONE', #61527, 10.20557198542813815 ) ;
#657 = CARTESIAN_POINT ( 'NONE',  ( 2.524535260912605938, 2.850096701925833642, 7.184101064217893295 ) ) ;
#658 = CARTESIAN_POINT ( 'NONE',  ( -31.19808003874556235, -3.097905286366202215, 23.19915556217947739 ) ) ;
#659 = VERTEX_POINT ( 'NONE', #32553 ) ;
#660 = ORIENTED_EDGE ( 'NONE', *, *, #35188, .F. ) ;
#661 = CARTESIAN_POINT ( 'NONE',  ( 0.000000000000000000, -1.734723475976807094E-15, 13.50000000000000178 ) ) ;
#662 = VERTEX_POINT ( 'NONE', #42878 ) ;
#663 = LINE ( 'NONE', #10958, #26308 ) ;
#664 = EDGE_LOOP ( 'NONE', ( #36440, #17580, #50368, #8037 ) ) ;
#665 = VERTEX_POINT ( 'NONE', #32884 ) ;
#666 = VERTEX_POINT ( 'NONE', #2338 ) ;
#667 = DIRECTION ( 'NONE',  ( 0.000000000000000000, 0.2960891610144510966, 0.9551603052523479631 ) ) ;
#668 = CARTESIAN_POINT ( 'NONE',  ( 0.9296196016816554719, 11.56707937094474126, 4.652334946094312862 ) ) ;
#669 = EDGE_CURVE ( 'NONE', #52645, #21040, #65347, .T. ) ;
#670 = CARTESIAN_POINT ( 'NONE',  ( 2.889800649504073782, 3.118861721612639748, -5.267262008933637496 ) ) ;
#671 = CARTESIAN_POINT ( 'NONE',  ( 0.3665391374699467075, 5.911453292029604789, 10.76665847464314929 ) ) ;
#672 = CARTESIAN_POINT ( 'NONE',  ( -22.31328051695926007, -2.608921479762108753, 2.748895659348124187 ) ) ;
#673 = ORIENTED_EDGE ( 'NONE', *, *, #65732, .F. ) ;
#674 = AXIS2_PLACEMENT_3D ( 'NONE', #36714, #57996, #52358 ) ;
#675 = DIRECTION ( 'NONE',  ( -1.000000000000000000, 0.000000000000000000, 0.000000000000000000 ) ) ;
#676 = ADVANCED_FACE ( 'NONE', ( #21954 ), #1688, .T. ) ;
#677 = CIRCLE ( 'NONE', #34620, 5.000000000000000000 ) ;
#678 = ORIENTED_EDGE ( 'NONE', *, *, #14140, .T. ) ;
#679 = CARTESIAN_POINT ( 'NONE',  ( -29.92777678363736626, -3.750539801530011985, -12.96855624952674724 ) ) ;
#680 = CARTESIAN_POINT ( 'NONE',  ( -27.08776759928964850, 0.6183458186125572187, 2.217308861843124035 ) ) ;
#681 = DIRECTION ( 'NONE',  ( 0.000000000000000000, -0.9246979985058763063, -0.3807014730195120711 ) ) ;
#682 = CARTESIAN_POINT ( 'NONE',  ( -37.00000000000000711, -10.91072401419407001, -5.428340790341820821 ) ) ;
#683 = FACE_OUTER_BOUND ( 'NONE', #43289, .T. ) ;
#684 = CARTESIAN_POINT ( 'NONE',  ( 1.634816307076842001, -10.62369813897163873, -6.964001572439102894 ) ) ;
#685 = EDGE_CURVE ( 'NONE', #60037, #21790, #40763, .T. ) ;
#686 = ORIENTED_EDGE ( 'NONE', *, *, #30624, .T. ) ;
#687 = CARTESIAN_POINT ( 'NONE',  ( 0.000000000000000000, -6.750946897830688798, -1.593658756657146292 ) ) ;
#688 = ORIENTED_EDGE ( 'NONE', *, *, #39482, .T. ) ;
#689 = FACE_OUTER_BOUND ( 'NONE', #23945, .T. ) ;
#690 = CARTESIAN_POINT ( 'NONE',  ( -4.968020780095184108, -25.99038707641916091, -15.26464785194325913 ) ) ;
#691 = CARTESIAN_POINT ( 'NONE',  ( 2.440552418640496768, 6.024135401262435963, -4.797131306497506742 ) ) ;
#692 = DIRECTION ( 'NONE',  ( 0.000000000000000000, -0.01356324068817998940, 0.9999080150203990547 ) ) ;
#693 = CARTESIAN_POINT ( 'NONE',  ( 1.000000000000000888, 7.414200355365252015, 1.131208685655162638 ) ) ;
#694 = EDGE_CURVE ( 'NONE', #57232, #43816, #50467, .T. ) ;
#695 = EDGE_CURVE ( 'NONE', #22968, #32750, #36676, .T. ) ;
#696 = ORIENTED_EDGE ( 'NONE', *, *, #59994, .F. ) ;
#697 = CARTESIAN_POINT ( 'NONE',  ( 36.00000000000000711, 4.400442035670942609, -11.96656215839370851 ) ) ;
#698 = CARTESIAN_POINT ( 'NONE',  ( 47.00000000000000711, 4.705694406421931860E-17, -3.469127814946512892E-15 ) ) ;
#699 = CARTESIAN_POINT ( 'NONE',  ( 23.32362518313050614, 9.357419094640528456, -7.519995448741596533 ) ) ;
#700 = CARTESIAN_POINT ( 'NONE',  ( 23.64431542999218294, -11.46495565953754792, -7.133712268643341403 ) ) ;
#701 = EDGE_CURVE ( 'NONE', #12145, #21025, #36642, .T. ) ;
#702 = CARTESIAN_POINT ( 'NONE',  ( 0.000000000000000000, 6.250523986463984549, 3.007653927006597172 ) ) ;
#703 = CARTESIAN_POINT ( 'NONE',  ( -35.04683013664716640, -0.009445816769442809055, -0.007968230201772305218 ) ) ;
#704 = CARTESIAN_POINT ( 'NONE',  ( -27.08429572838383947, 2.279961732801592422, -0.2296550094122856711 ) ) ;
#705 = CARTESIAN_POINT ( 'NONE',  ( 5.520433897694421610, -0.01120198501134828974, -0.01006947824912434765 ) ) ;
#706 = CARTESIAN_POINT ( 'NONE',  ( 5.520433897694421610, -0.01278034823631958410, -0.007971295965052542856 ) ) ;
#707 = VECTOR ( 'NONE', #33683, 1000.000000000000000 ) ;
#708 = EDGE_CURVE ( 'NONE', #10609, #56404, #22264, .T. ) ;
#709 = CIRCLE ( 'NONE', #32531, 7.499999999999988454 ) ;
#710 = ORIENTED_EDGE ( 'NONE', *, *, #27283, .T. ) ;
#711 = ADVANCED_FACE ( 'NONE', ( #43522 ), #63474, .T. ) ;
#712 = ORIENTED_EDGE ( 'NONE', *, *, #9742, .T. ) ;
#713 = LINE ( 'NONE', #60899, #29959 ) ;
#714 = CYLINDRICAL_SURFACE ( 'NONE', #28997, 4.999999999999997335 ) ;
#715 = CARTESIAN_POINT ( 'NONE',  ( -35.00000000000000000, 0.000000000000000000, 0.000000000000000000 ) ) ;
#716 = DIRECTION ( 'NONE',  ( 0.000000000000000000, -0.01356324068817991828, 0.9999080150203990547 ) ) ;
#717 = ORIENTED_EDGE ( 'NONE', *, *, #21995, .T. ) ;
#718 = ORIENTED_EDGE ( 'NONE', *, *, #61557, .T. ) ;
#719 = EDGE_LOOP ( 'NONE', ( #21137, #14630, #27756, #54283 ) ) ;
#720 = CARTESIAN_POINT ( 'NONE',  ( 37.00000000000000711, -12.74613886779084382, 0.3137578094510532489 ) ) ;
#721 = CARTESIAN_POINT ( 'NONE',  ( -22.27713295444592845, 0.8543895091636684036, 3.580881989303308810 ) ) ;
#722 = ORIENTED_EDGE ( 'NONE', *, *, #37336, .F. ) ;
#723 = CARTESIAN_POINT ( 'NONE',  ( 6.361445718264521432, -4.355102044641763648, 12.77822703589027320 ) ) ;
#724 = CYLINDRICAL_SURFACE ( 'NONE', #42705, 5.000000000000000888 ) ;
#725 = VERTEX_POINT ( 'NONE', #38552 ) ;
#726 = CARTESIAN_POINT ( 'NONE',  ( 2.256373768223944420, 4.807932997207285730, -5.936694589811832401 ) ) ;
#727 = CARTESIAN_POINT ( 'NONE',  ( 18.66975156949926529, -29.88417193384192316, -7.188590896528729068 ) ) ;
#728 = LINE ( 'NONE', #60250, #54703 ) ;
#729 = EDGE_LOOP ( 'NONE', ( #16935, #19715, #52598, #51184 ) ) ;
#730 = LINE ( 'NONE', #49960, #59686 ) ;
#731 = ORIENTED_EDGE ( 'NONE', *, *, #62834, .F. ) ;
#732 = LINE ( 'NONE', #6711, #42192 ) ;
#733 = ORIENTED_EDGE ( 'NONE', *, *, #40830, .F. ) ;
#734 = DIRECTION ( 'NONE',  ( 0.000000000000000000, 0.4134677391718449280, 0.9105187689795983808 ) ) ;
#735 = DIRECTION ( 'NONE',  ( -0.3939253465568944290, 0.1691689424289765653, 0.9034404741085558799 ) ) ;
#736 = CARTESIAN_POINT ( 'NONE',  ( 2.244591118396558560, 3.910457279126710262, 6.558116599718180062 ) ) ;
#737 = DIRECTION ( 'NONE',  ( 1.000000000000000000, 0.000000000000000000, 0.000000000000000000 ) ) ;
#738 = CARTESIAN_POINT ( 'NONE',  ( 3.152665057735260845, 4.377619405893435456, 6.622010822086191517 ) ) ;
#739 = CARTESIAN_POINT ( 'NONE',  ( 2.241352910868908310, -7.503490710578242684, 1.407733736974842165 ) ) ;
#740 = CARTESIAN_POINT ( 'NONE',  ( 1.719304012341582588, 7.017415949614099979, -10.62216384465570762 ) ) ;
#741 = DIRECTION ( 'NONE',  ( 0.9606638835031803270, 0.02862840969242944761, 0.2762341707520462042 ) ) ;
#743 = VERTEX_POINT ( 'NONE', #12287 ) ;
#742 = CARTESIAN_POINT ( 'NONE',  ( 5.187165255848094958, -10.33573060559526446, 8.685987315626189087 ) ) ;
#744 = CARTESIAN_POINT ( 'NONE',  ( 1.948354844647729012, 11.46941405766174604, 3.407825014328282442 ) ) ;
#745 = ADVANCED_FACE ( 'NONE', ( #17946 ), #38208, .T. ) ;
#746 = ORIENTED_EDGE ( 'NONE', *, *, #28329, .F. ) ;
#747 = CARTESIAN_POINT ( 'NONE',  ( 0.2706063244538032264, -4.353289770698299144, 11.44820198696414160 ) ) ;
#748 = CARTESIAN_POINT ( 'NONE',  ( 35.00000000000000000, 11.60979404548634619, -3.704519465651352483 ) ) ;
#749 = ORIENTED_EDGE ( 'NONE', *, *, #60715, .T. ) ;
#750 = CARTESIAN_POINT ( 'NONE',  ( 0.6473888112830223918, -12.36914475328378593, 0.3298838684458400006 ) ) ;
#751 = CARTESIAN_POINT ( 'NONE',  ( 1.375507693220482608, 12.04466556545283140, -3.754650692912763876 ) ) ;
#752 = CARTESIAN_POINT ( 'NONE',  ( -27.09569413923794912, -2.232620870184085060, 0.6513788562879397892 ) ) ;
#753 = AXIS2_PLACEMENT_3D ( 'NONE', #48750, #3202, #43746 ) ;
#754 = CYLINDRICAL_SURFACE ( 'NONE', #41257, 12.75000000000000178 ) ;
#755 = CARTESIAN_POINT ( 'NONE',  ( 2.251152103361941936, 7.218942724306940839, 2.494172441824263231 ) ) ;
#756 = EDGE_CURVE ( 'NONE', #28947, #52648, #34539, .T. ) ;
#757 = ORIENTED_EDGE ( 'NONE', *, *, #3796, .F. ) ;
#758 = VECTOR ( 'NONE', #8324, 1000.000000000000000 ) ;
#759 = CARTESIAN_POINT ( 'NONE',  ( -35.00000000000000000, 0.000000000000000000, 0.000000000000000000 ) ) ;
#760 = EDGE_LOOP ( 'NONE', ( #46114, #4042, #25768, #55762 ) ) ;
#761 = CARTESIAN_POINT ( 'NONE',  ( 2.589278595512600756, 0.2408616556818840848, 7.746633201026948967 ) ) ;
#762 = FACE_OUTER_BOUND ( 'NONE', #45586, .T. ) ;
#763 = CARTESIAN_POINT ( 'NONE',  ( 2.241352910868908310, -2.689314586382304917, -7.145045428366603169 ) ) ;
#764 = ADVANCED_FACE ( 'NONE', ( #2996 ), #41154, .F. ) ;
#765 = ORIENTED_EDGE ( 'NONE', *, *, #30183, .F. ) ;
#766 = CARTESIAN_POINT ( 'NONE',  ( 0.3654063281920738593, -4.446369912832434323, -11.44627072062583828 ) ) ;
#767 =( BOUNDED_CURVE ( )  B_SPLINE_CURVE ( 3, ( #59079, #17840, #43417, #33125 ),
 .UNSPECIFIED., .F., .F. ) 
 B_SPLINE_CURVE_WITH_KNOTS ( ( 4, 4 ),
 ( 0.6374084671583093442, 0.6849672343075862146 ),
 .UNSPECIFIED. ) 
 CURVE ( )  GEOMETRIC_REPRESENTATION_ITEM ( )  RATIONAL_B_SPLINE_CURVE ( ( 1.000000000000000000, 0.9998115225205463918, 0.9998115225205463918, 1.000000000000000000 ) ) 
 REPRESENTATION_ITEM ( '' )  );
#768 = CARTESIAN_POINT ( 'NONE',  ( 26.44191060433393048, 12.90701898410668846, 3.963759825896518763 ) ) ;
#769 = CARTESIAN_POINT ( 'NONE',  ( 49.19530910174992044, -0.1631003452855546987, 6.502801691937079021 ) ) ;
#770 = CARTESIAN_POINT ( 'NONE',  ( 11.99003848479309298, 10.55797189877291054, -8.414293459742244963 ) ) ;
#771 = CARTESIAN_POINT ( 'NONE',  ( 0.3002738374340877536, -5.932527270856326140, -10.72659044316170096 ) ) ;
#772 = CARTESIAN_POINT ( 'NONE',  ( -22.76187086591099984, -0.9059972289356940101, -5.055065309934924755 ) ) ;
#773 = CARTESIAN_POINT ( 'NONE',  ( 3.657075258475105617, -30.77912794045789724, 15.01778408663561493 ) ) ;
#774 = DIRECTION ( 'NONE',  ( -1.000000000000000000, 0.000000000000000000, 0.000000000000000000 ) ) ;
#775 = EDGE_CURVE ( 'NONE', #30093, #56170, #13911, .T. ) ;
#776 = EDGE_LOOP ( 'NONE', ( #11721, #57798, #2709, #5498 ) ) ;
#777 = CARTESIAN_POINT ( 'NONE',  ( -18.06053859689077257, 5.591681739832217168, 12.28972654602461922 ) ) ;
#778 = CARTESIAN_POINT ( 'NONE',  ( 5.514970785353741078, 0.002093325033904021564, 0.004233694591582523939 ) ) ;
#779 = ORIENTED_EDGE ( 'NONE', *, *, #18157, .F. ) ;
#780 = CARTESIAN_POINT ( 'NONE',  ( 2.903928887688147054, -5.221047506681327555, 7.046356840276350120 ) ) ;
#781 = CARTESIAN_POINT ( 'NONE',  ( 37.00000000000000711, 7.499679039484058229, -9.040300684349723781 ) ) ;
#782 = DIRECTION ( 'NONE',  ( 0.3939253465568944290, -0.3234796780324422083, 0.8603393047164927809 ) ) ;
#783 = EDGE_LOOP ( 'NONE', ( #27018, #40138, #64745, #62156 ) ) ;
#784 = CARTESIAN_POINT ( 'NONE',  ( 2.256373768223415510, -6.548448293197158598, 3.934258165100049442 ) ) ;
#785 = CARTESIAN_POINT ( 'NONE',  ( -37.00000000000000711, -11.37311665002361494, -2.936739658819992549 ) ) ;
#786 = VERTEX_POINT ( 'NONE', #60455 ) ;
#787 = ORIENTED_EDGE ( 'NONE', *, *, #22061, .F. ) ;
#788 = ORIENTED_EDGE ( 'NONE', *, *, #27671, .T. ) ;
#789 = EDGE_CURVE ( 'NONE', #16747, #25350, #24974, .T. ) ;
#790 = CARTESIAN_POINT ( 'NONE',  ( -27.20164183316782669, -1.409601201084045297, -2.237540722393188020 ) ) ;
#791 = CIRCLE ( 'NONE', #37956, 12.18650000000000233 ) ;
#792 = ORIENTED_EDGE ( 'NONE', *, *, #53491, .T. ) ;
#793 = CARTESIAN_POINT ( 'NONE',  ( 2.000000000000001776, -6.338823199656649088, -2.816798305433765748 ) ) ;
#794 = CARTESIAN_POINT ( 'NONE',  ( 0.2638984909335720941, -7.718810690099123129, 9.508791614589169328 ) ) ;
#795 = DIRECTION ( 'NONE',  ( -1.000000000000000000, 0.000000000000000000, 0.000000000000000000 ) ) ;
#796 = CARTESIAN_POINT ( 'NONE',  ( 10.75853767213705225, 7.830989516993144051, 9.092612561015865680 ) ) ;
#797 = VERTEX_POINT ( 'NONE', #24897 ) ;
#798 = CARTESIAN_POINT ( 'NONE',  ( 1.719304012341585475, 10.62216384465587993, -7.017415949613843296 ) ) ;
#799 = CARTESIAN_POINT ( 'NONE',  ( 3.702144525957873356, -25.87585389521097312, 15.43847573974272613 ) ) ;
#800 = CARTESIAN_POINT ( 'NONE',  ( 20.00005080000000035, 5.400000000000000355, -1.000000000000000000 ) ) ;
#802 = ORIENTED_EDGE ( 'NONE', *, *, #61825, .F. ) ;
#801 = CARTESIAN_POINT ( 'NONE',  ( 3.152665057734045373, -6.378477742800418682, 4.725420687650736085 ) ) ;
#803 = LINE ( 'NONE', #51023, #53281 ) ;
#804 = ORIENTED_EDGE ( 'NONE', *, *, #45884, .F. ) ;
#805 = CARTESIAN_POINT ( 'NONE',  ( -35.00000000000000000, 5.921969905510501064, -10.14408668126206869 ) ) ;
#806 = ORIENTED_EDGE ( 'NONE', *, *, #17340, .T. ) ;
#807 = VERTEX_POINT ( 'NONE', #45172 ) ;
#808 = LINE ( 'NONE', #11431, #63431 ) ;
#809 = CYLINDRICAL_SURFACE ( 'NONE', #10731, 4.999999999999998224 ) ;
#810 = CARTESIAN_POINT ( 'NONE',  ( 2.249013661412228249, -7.636012530783591323, -0.1200550008339948543 ) ) ;
#811 = ORIENTED_EDGE ( 'NONE', *, *, #53682, .F. ) ;
#812 = FACE_OUTER_BOUND ( 'NONE', #15918, .T. ) ;
#813 = CYLINDRICAL_SURFACE ( 'NONE', #28256, 4.725920239717170901 ) ;
#814 = LINE ( 'NONE', #56699, #25637 ) ;
#815 = VERTEX_POINT ( 'NONE', #59176 ) ;
#816 = EDGE_CURVE ( 'NONE', #36349, #13265, #3325, .T. ) ;
#817 = VERTEX_POINT ( 'NONE', #29533 ) ;
#818 = EDGE_CURVE ( 'NONE', #43621, #13249, #2936, .T. ) ;
#819 = CARTESIAN_POINT ( 'NONE',  ( 0.2911222467163545602, 12.02952766044175625, 2.338869407810904910 ) ) ;
#820 = EDGE_LOOP ( 'NONE', ( #51764, #48932, #27665, #36662 ) ) ;
#821 = EDGE_CURVE ( 'NONE', #21537, #33192, #25015, .T. ) ;
#822 = B_SPLINE_CURVE_WITH_KNOTS ( 'NONE', 3,
 ( #26185, #46458, #55458, #61745, #16205, #36483, #51792, #31492, #30184, #50487, #32778, #57107, #2578, #36811, #1899, #52456 ),
 .UNSPECIFIED., .F., .F.,
 ( 4, 3, 3, 3, 3, 4 ),
 ( 0.000000000000000000, 0.0002176109881720274394, 0.0004352086762394653287, 0.0006528017811446958562, 0.0007615147961451794326, 0.0009453342004942210915 ),
 .UNSPECIFIED. ) ;
#823 = ORIENTED_EDGE ( 'NONE', *, *, #31386, .T. ) ;
#824 = DIRECTION ( 'NONE',  ( -1.000000000000000000, 0.000000000000000000, 0.000000000000000000 ) ) ;
#825 = CARTESIAN_POINT ( 'NONE',  ( 0.000000000000000000, 6.539067737394526958, -2.314222412769764148 ) ) ;
#826 = DIRECTION ( 'NONE',  ( -1.000000000000000000, 0.000000000000000000, 0.000000000000000000 ) ) ;
#827 = B_SPLINE_CURVE_WITH_KNOTS ( 'NONE', 3,
 ( #32126, #1238, #21517, #12180, #16839, #26824, #2566, #37452 ),
 .UNSPECIFIED., .F., .F.,
 ( 4, 2, 2, 4 ),
 ( 0.000000000000000000, 0.0003639104015149979571, 0.0007278208030299959143, 0.001455641606059991829 ),
 .UNSPECIFIED. ) ;
#828 = LINE ( 'NONE', #62628, #34195 ) ;
#829 = LINE ( 'NONE', #56713, #27354 ) ;
#830 = CONICAL_SURFACE ( 'NONE', #22085, 7.938172270156617749, 1.280189991382167047 ) ;
#831 = CARTESIAN_POINT ( 'NONE',  ( -35.00000000000000000, -11.78745411414837818, -3.093009498344053032 ) ) ;
#832 = EDGE_CURVE ( 'NONE', #37322, #43331, #35952, .T. ) ;
#833 = DIRECTION ( 'NONE',  ( 1.000000000000000000, 0.000000000000000000, 0.000000000000000000 ) ) ;
#834 = CIRCLE ( 'NONE', #42232, 12.74999999999999822 ) ;
#835 = ORIENTED_EDGE ( 'NONE', *, *, #4136, .T. ) ;
#836 = FACE_OUTER_BOUND ( 'NONE', #5027, .T. ) ;
#837 = ADVANCED_FACE ( 'NONE', ( #54832 ), #8614, .T. ) ;
#838 = CARTESIAN_POINT ( 'NONE',  ( 2.266490820343223689, 7.500072841116514510, -1.470039317404083778 ) ) ;
#839 = CIRCLE ( 'NONE', #57095, 2.899999999999996358 ) ;
#840 = CARTESIAN_POINT ( 'NONE',  ( 4.036807064762983899, -10.39659893473963947, 5.993789462885469987 ) ) ;
#841 = LINE ( 'NONE', #529, #61898 ) ;
#842 = CIRCLE ( 'NONE', #43306, 5.000000000000000000 ) ;
#843 = ADVANCED_FACE ( 'NONE', ( #40163 ), #38885, .T. ) ;
#844 = CARTESIAN_POINT ( 'NONE',  ( 24.40033961665191953, -0.3581885377669972170, -13.50005958318994814 ) ) ;
#845 = CARTESIAN_POINT ( 'NONE',  ( 1.020182472824350040, 2.608319446515835249, -12.22263240120574146 ) ) ;
#846 = FACE_OUTER_BOUND ( 'NONE', #63936, .T. ) ;
#847 = ORIENTED_EDGE ( 'NONE', *, *, #52308, .T. ) ;
#848 = DIRECTION ( 'NONE',  ( -1.000000000000000000, 0.000000000000000000, -0.000000000000000000 ) ) ;
#849 = CARTESIAN_POINT ( 'NONE',  ( 35.00000000000000000, -10.62137734850271364, -5.015831474386272859 ) ) ;
#850 = CARTESIAN_POINT ( 'NONE',  ( 11.32672149592540833, -33.39346531321398714, 11.05302976539647197 ) ) ;
#851 = CARTESIAN_POINT ( 'NONE',  ( -24.94459482683992135, 9.240370367366107729, 7.658175360001901133 ) ) ;
#852 = CARTESIAN_POINT ( 'NONE',  ( 2.000000000000001776, 6.253963800348318003, -4.139799123620975685 ) ) ;
#853 = VERTEX_POINT ( 'NONE', #39190 ) ;
#854 = CARTESIAN_POINT ( 'NONE',  ( -17.83419946441818027, -9.720786832536937538, -9.367833439828872955 ) ) ;
#855 = DIRECTION ( 'NONE',  ( 0.000000000000000000, 0.01356324068817998940, -0.9999080150203990547 ) ) ;
#856 = CARTESIAN_POINT ( 'NONE',  ( 9.730232070128172595, -26.74067542416307219, -13.98809302346541372 ) ) ;
#857 = ORIENTED_EDGE ( 'NONE', *, *, #24910, .T. ) ;
#858 = DIRECTION ( 'NONE',  ( -1.000000000000000000, 0.000000000000000000, 0.000000000000000000 ) ) ;
#859 = CARTESIAN_POINT ( 'NONE',  ( 0.3040950598368144520, -12.25911170648142523, -0.2511348647276926971 ) ) ;
#860 = CARTESIAN_POINT ( 'NONE',  ( 37.00000000000000711, 4.705694406421931860E-17, -3.469127814946512892E-15 ) ) ;
#862 = ORIENTED_EDGE ( 'NONE', *, *, #20137, .F. ) ;
#861 = CARTESIAN_POINT ( 'NONE',  ( 35.00000000000000000, 4.705694406421931860E-17, -3.469127814946512892E-15 ) ) ;
#863 = CARTESIAN_POINT ( 'NONE',  ( -27.08850691366480490, 2.232573186527712306, 0.5697889027535342210 ) ) ;
#864 = CIRCLE ( 'NONE', #38023, 12.74999999999999822 ) ;
#865 = EDGE_CURVE ( 'NONE', #65236, #8648, #45234, .T. ) ;
#866 = CARTESIAN_POINT ( 'NONE',  ( 2.717984159219664964, -7.415470774237006069, -2.397195612260698994 ) ) ;
#867 = ORIENTED_EDGE ( 'NONE', *, *, #9217, .F. ) ;
#868 = CARTESIAN_POINT ( 'NONE',  ( -22.30625920655495165, 3.150098859949344909, -2.110841417170892242 ) ) ;
#869 = AXIS2_PLACEMENT_3D ( 'NONE', #36595, #26608, #21289 ) ;
#870 = CARTESIAN_POINT ( 'NONE',  ( 23.55206865562520946, -3.422725234784213200, -11.50504497094062550 ) ) ;
#871 = LINE ( 'NONE', #42385, #25569 ) ;
#872 = CARTESIAN_POINT ( 'NONE',  ( -9.790055383657291443, 10.81845249703099299, -5.209507621916693587 ) ) ;
#873 = CARTESIAN_POINT ( 'NONE',  ( -37.00000000000000711, 2.627174906296914525, 11.44858830469741129 ) ) ;
#875 = ORIENTED_EDGE ( 'NONE', *, *, #40087, .T. ) ;
#874 = CARTESIAN_POINT ( 'NONE',  ( 0.8320506296491582132, 0.3827056590416837434, 12.42924193558400958 ) ) ;
#876 = VECTOR ( 'NONE', #40647, 1000.000000000000000 ) ;
#877 = ORIENTED_EDGE ( 'NONE', *, *, #53294, .F. ) ;
#878 = DIRECTION ( 'NONE',  ( 1.000000000000000000, 0.000000000000000000, -0.000000000000000000 ) ) ;
#879 = ORIENTED_EDGE ( 'NONE', *, *, #58206, .T. ) ;
#880 = AXIS2_PLACEMENT_3D ( 'NONE', #6476, #57343, #1160 ) ;
#881 = DIRECTION ( 'NONE',  ( 0.000000000000000000, 0.000000000000000000, 1.000000000000000000 ) ) ;
#882 = CARTESIAN_POINT ( 'NONE',  ( -2.812344914800137818, -12.94091111974181452, 3.845999582511304471 ) ) ;
#883 = CARTESIAN_POINT ( 'NONE',  ( 2.969415267404913017, 1.748187016698500740, 7.680649281077271517 ) ) ;
#884 = EDGE_CURVE ( 'NONE', #59432, #13921, #39910, .T. ) ;
#885 = DIRECTION ( 'NONE',  ( 1.000000000000000000, -0.000000000000000000, -0.000000000000000000 ) ) ;
#886 = VERTEX_POINT ( 'NONE', #24230 ) ;
#887 = CARTESIAN_POINT ( 'NONE',  ( -37.00000000000000711, 12.15823808070322798, 0.8294751490779768144 ) ) ;
#888 = CARTESIAN_POINT ( 'NONE',  ( -37.00000000000000711, 7.608228585767727203, 10.23119532541075394 ) ) ;
#889 = EDGE_CURVE ( 'NONE', #27125, #49767, #43081, .T. ) ;
#890 = FACE_BOUND ( 'NONE', #11009, .T. ) ;
#891 = EDGE_LOOP ( 'NONE', ( #65575, #20229, #17505, #23044 ) ) ;
#892 = ORIENTED_EDGE ( 'NONE', *, *, #1040, .T. ) ;
#893 = CARTESIAN_POINT ( 'NONE',  ( 2.241317068080787234, -7.204761327832114759, -2.524952427345728445 ) ) ;
#894 = EDGE_CURVE ( 'NONE', #54998, #17169, #38397, .T. ) ;
#895 = ORIENTED_EDGE ( 'NONE', *, *, #62262, .F. ) ;
#896 = CARTESIAN_POINT ( 'NONE',  ( 37.00000000000000711, 12.46157735505189201, -2.696588552979104492 ) ) ;
#897 = CARTESIAN_POINT ( 'NONE',  ( 3.152665057733995191, 6.622010822086684456, 4.377619405892240856 ) ) ;
#898 = DIRECTION ( 'NONE',  ( -1.000000000000000000, 0.000000000000000000, 0.000000000000000000 ) ) ;
#899 = CARTESIAN_POINT ( 'NONE',  ( -37.00000000000000711, -9.733281772932221187, 8.235637554476612721 ) ) ;
#900 = DIRECTION ( 'NONE',  ( 0.000000000000000000, 0.9105187689795969375, -0.4134677391718481476 ) ) ;
#901 = CARTESIAN_POINT ( 'NONE',  ( 0.000000000000000000, 0.000000000000000000, 0.000000000000000000 ) ) ;
#902 = AXIS2_PLACEMENT_3D ( 'NONE', #63159, #17287, #26597 ) ;
#903 = ADVANCED_FACE ( 'NONE', ( #35516 ), #11835, .F. ) ;
#904 = CARTESIAN_POINT ( 'NONE',  ( 2.253265082352434501, 7.498995607278136966, 1.452519439326484640 ) ) ;
#905 = ORIENTED_EDGE ( 'NONE', *, *, #34232, .T. ) ;
#906 = CARTESIAN_POINT ( 'NONE',  ( -35.00000000000000000, -11.17622378668009020, 3.614449339633449387 ) ) ;
#907 = AXIS2_PLACEMENT_3D ( 'NONE', #20849, #15201, #35484 ) ;
#908 = EDGE_CURVE ( 'NONE', #45349, #45226, #9101, .T. ) ;
#909 = CYLINDRICAL_SURFACE ( 'NONE', #28937, 4.999999999999999112 ) ;
#910 = DIRECTION ( 'NONE',  ( 1.000000000000000000, 0.000000000000000000, 0.000000000000000000 ) ) ;
#911 = CARTESIAN_POINT ( 'NONE',  ( -8.866453229254560142, 8.638462841324983543, -8.362614154885761764 ) ) ;
#912 = DIRECTION ( 'NONE',  ( 0.000000000000000000, -0.3218879778916041157, 0.9467777615094549182 ) ) ;
#913 = CARTESIAN_POINT ( 'NONE',  ( -18.04458733766117362, 11.34280559204706584, 3.916728392552376370 ) ) ;
#914 = B_SPLINE_CURVE_WITH_KNOTS ( 'NONE', 3,
 ( #2656, #63447, #32211, #32526, #47213, #6961, #22916, #43171, #6312, #52534, #21927, #52836, #26574, #46867, #1970, #1329, #62158, #21605, #7610 ),
 .UNSPECIFIED., .F., .F.,
 ( 4, 3, 3, 3, 3, 3, 4 ),
 ( 1.226634733346699349E-18, 2.831840207458639276E-05, 4.217266859784439504E-05, 5.602024318340332140E-05, 6.290810167913971876E-05, 9.120440630891354624E-05, 0.0001153103026480218702 ),
 .UNSPECIFIED. ) ;
#915 = CARTESIAN_POINT ( 'NONE',  ( 2.000000000000001776, -4.962980376314023445, -4.846014654777856201 ) ) ;
#916 = EDGE_CURVE ( 'NONE', #29332, #12123, #10240, .T. ) ;
#917 = VECTOR ( 'NONE', #57645, 1000.000000000000000 ) ;
#918 = VERTEX_POINT ( 'NONE', #36152 ) ;
#919 = ORIENTED_EDGE ( 'NONE', *, *, #8955, .T. ) ;
#920 = DIRECTION ( 'NONE',  ( 0.000000000000000000, -0.01356324068818697166, 0.9999080150203988326 ) ) ;
#921 = EDGE_CURVE ( 'NONE', #1325, #239, #15234, .T. ) ;
#922 = AXIS2_PLACEMENT_3D ( 'NONE', #48961, #13037, #52946 ) ;
#923 = AXIS2_PLACEMENT_3D ( 'NONE', #20101, #14440, #41031 ) ;
#924 = VERTEX_POINT ( 'NONE', #56460 ) ;
#925 = DIRECTION ( 'NONE',  ( 1.000000000000000000, -0.000000000000000000, 0.000000000000000000 ) ) ;
#926 = CARTESIAN_POINT ( 'NONE',  ( -14.51396536449455610, 7.857708026690540137, -10.97759357154228432 ) ) ;
#927 = EDGE_CURVE ( 'NONE', #35439, #25961, #34586, .T. ) ;
#928 = VECTOR ( 'NONE', #37946, 1000.000000000000000 ) ;
#929 = CARTESIAN_POINT ( 'NONE',  ( 2.276198483117283455, 4.795748742147503130, 5.955030244776311932 ) ) ;
#930 = CARTESIAN_POINT ( 'NONE',  ( 1.937114397841932290, -5.620553190832896284, -11.53912442307261088 ) ) ;
#931 = EDGE_LOOP ( 'NONE', ( #4139, #42751, #11276, #57230 ) ) ;
#932 = CARTESIAN_POINT ( 'NONE',  ( 0.2638984909335720941, 9.508791614589194197, 7.718810690099093819 ) ) ;
#933 = CARTESIAN_POINT ( 'NONE',  ( 2.241526690369557873, -0.01730530154271369553, -7.634439869182785721 ) ) ;
#934 = CARTESIAN_POINT ( 'NONE',  ( 1.372161826076017777, -1.607409531431894134, 12.51237317864369558 ) ) ;
#935 = CIRCLE ( 'NONE', #32749, 5.000000000000000888 ) ;
#936 = CARTESIAN_POINT ( 'NONE',  ( 2.990245332647524901, 4.676740826319936595, -7.075286609974432039 ) ) ;
#937 = CARTESIAN_POINT ( 'NONE',  ( 0.2648321136542694521, 6.245325033825879224, -10.53380804838491791 ) ) ;
#938 = DIRECTION ( 'NONE',  ( -1.000000000000000000, -0.000000000000000000, 0.000000000000000000 ) ) ;
#939 = VERTEX_POINT ( 'NONE', #30517 ) ;
#940 = CARTESIAN_POINT ( 'NONE',  ( 5.516018279890452902, -0.002527316374434336339, 0.006286471671802434068 ) ) ;
#941 = ORIENTED_EDGE ( 'NONE', *, *, #51723, .F. ) ;
#942 = CARTESIAN_POINT ( 'NONE',  ( -22.27384469013076185, 3.564715702084495952, -0.9224151068931343289 ) ) ;
#943 = FACE_OUTER_BOUND ( 'NONE', #16437, .T. ) ;
#944 = CARTESIAN_POINT ( 'NONE',  ( 35.00000000000000000, -0.7214809346829402781, -11.72397916322012179 ) ) ;
#945 = CARTESIAN_POINT ( 'NONE',  ( 28.71051995168708970, -9.891108990099938936, 6.797948428913199947 ) ) ;
#946 = CARTESIAN_POINT ( 'NONE',  ( -5.393986094047766855, -1.427626268664394571, 11.91478156919506404 ) ) ;
#947 = EDGE_CURVE ( 'NONE', #60093, #51437, #11236, .T. ) ;
#948 = ADVANCED_FACE ( 'NONE', ( #65750 ), #31196, .T. ) ;
#949 = ORIENTED_EDGE ( 'NONE', *, *, #54584, .F. ) ;
#950 = EDGE_LOOP ( 'NONE', ( #25283, #63821, #8181, #28315 ) ) ;
#951 = CARTESIAN_POINT ( 'NONE',  ( 5.514624014163232779, -0.001921576324372115032, 0.003668383633201685416 ) ) ;
#952 = ORIENTED_EDGE ( 'NONE', *, *, #24463, .T. ) ;
#953 = CARTESIAN_POINT ( 'NONE',  ( 35.00000000000000000, -9.430788938293991563, 7.718225330433904574 ) ) ;
#954 = CARTESIAN_POINT ( 'NONE',  ( -36.00000000000000711, -12.02534193257724304, 4.237174932027182983 ) ) ;
#955 = CARTESIAN_POINT ( 'NONE',  ( 2.798553295784531159, 25.00000000000000000, 7.462808788758677814 ) ) ;
#956 = CARTESIAN_POINT ( 'NONE',  ( 1.719304012338201737, 9.242227816402087015, 8.755325027793320558 ) ) ;
#958 = CARTESIAN_POINT ( 'NONE',  ( 0.5572780756287532000, -7.697784780878664357, -9.649189244958765954 ) ) ;
#957 = AXIS2_PLACEMENT_3D ( 'NONE', #6472, #26751, #47375 ) ;
#959 = CARTESIAN_POINT ( 'NONE',  ( 1.462291587751621380, 11.25382118863405623, -5.766456054323407798 ) ) ;
#960 = CARTESIAN_POINT ( 'NONE',  ( -8.908813177951650175, -2.340099471291562150, 11.77039042327342067 ) ) ;
#961 = ORIENTED_EDGE ( 'NONE', *, *, #65675, .T. ) ;
#962 = EDGE_CURVE ( 'NONE', #2752, #28450, #1679, .T. ) ;
#963 = CARTESIAN_POINT ( 'NONE',  ( 37.00000000000000711, -9.913596905230170009, -8.017674001891752056 ) ) ;
#964 = ORIENTED_EDGE ( 'NONE', *, *, #16319, .F. ) ;
#965 = CIRCLE ( 'NONE', #16908, 6.936499999999989896 ) ;
#966 = CARTESIAN_POINT ( 'NONE',  ( -37.00000000000000711, 2.772148766916116891, 11.86701198550357361 ) ) ;
#967 = AXIS2_PLACEMENT_3D ( 'NONE', #4976, #11582, #20901 ) ;
#968 = FACE_BOUND ( 'NONE', #43387, .T. ) ;
#969 = ADVANCED_FACE ( 'NONE', ( #40500 ), #46804, .T. ) ;
#970 = ORIENTED_EDGE ( 'NONE', *, *, #59989, .T. ) ;
#971 = CARTESIAN_POINT ( 'NONE',  ( 41.00000000000000711, -25.03188948156373783, 4.499999999999997335 ) ) ;
#972 = CARTESIAN_POINT ( 'NONE',  ( -22.27715526084302056, 3.652257391294508881, -0.4651416883073660746 ) ) ;
#974 = ORIENTED_EDGE ( 'NONE', *, *, #28534, .T. ) ;
#973 = CIRCLE ( 'NONE', #5195, 2.899999999999995914 ) ;
#975 = CARTESIAN_POINT ( 'NONE',  ( 35.00000000000000000, -11.07407352312215387, -3.916263239775311433 ) ) ;
#976 =( BOUNDED_CURVE ( )  B_SPLINE_CURVE ( 3, ( #14907, #9952, #43298, #30235 ),
 .UNSPECIFIED., .F., .F. ) 
 B_SPLINE_CURVE_WITH_KNOTS ( ( 4, 4 ),
 ( 4.466372954730139178, 4.500313351398628647 ),
 .UNSPECIFIED. ) 
 CURVE ( )  GEOMETRIC_REPRESENTATION_ITEM ( )  RATIONAL_B_SPLINE_CURVE ( ( 1.000000000000000000, 0.9999040064266120353, 0.9999040064266120353, 1.000000000000000000 ) ) 
 REPRESENTATION_ITEM ( '' )  );
#977 = LINE ( 'NONE', #51851, #49870 ) ;
#978 = CARTESIAN_POINT ( 'NONE',  ( 47.00000000000000711, 4.705694406421931860E-17, -3.469127814946512892E-15 ) ) ;
#979 = ORIENTED_EDGE ( 'NONE', *, *, #2691, .F. ) ;
#980 = ORIENTED_EDGE ( 'NONE', *, *, #36684, .F. ) ;
#981 = CARTESIAN_POINT ( 'NONE',  ( 5.515188684475870851, -0.002983184900674883035, 0.004442604682416470725 ) ) ;
#982 = ADVANCED_FACE ( 'NONE', ( #30839 ), #5948, .T. ) ;
#983 = VERTEX_POINT ( 'NONE', #45830 ) ;
#984 = CARTESIAN_POINT ( 'NONE',  ( 1.014383007554946481, -11.88680274101309564, -3.853787798429523459 ) ) ;
#985 = ORIENTED_EDGE ( 'NONE', *, *, #43519, .T. ) ;
#986 = EDGE_LOOP ( 'NONE', ( #31605, #32517, #57643, #11627 ) ) ;
#987 = CIRCLE ( 'NONE', #55129, 12.18650000000000055 ) ;
#988 = EDGE_LOOP ( 'NONE', ( #38920, #20606, #12540, #50252 ) ) ;
#989 = CARTESIAN_POINT ( 'NONE',  ( 2.781367136451683653, -5.783466416658768594, 5.255136723410106292 ) ) ;
#990 = CARTESIAN_POINT ( 'NONE',  ( -17.07517663476617997, -28.52001404462332701, 9.261390606240922807 ) ) ;
#991 = CARTESIAN_POINT ( 'NONE',  ( 21.90174657591892071, -11.97747433400148864, -0.7349207973210698519 ) ) ;
#992 = DIRECTION ( 'NONE',  ( 0.000000000000000000, 0.000000000000000000, 1.000000000000000000 ) ) ;
#993 = DIRECTION ( 'NONE',  ( 0.000000000000000000, 0.01356324068817998940, -0.9999080150203989437 ) ) ;
#994 = ORIENTED_EDGE ( 'NONE', *, *, #57357, .F. ) ;
#995 = DIRECTION ( 'NONE',  ( 1.000000000000000000, 0.000000000000000000, -0.000000000000000000 ) ) ;
#996 = ORIENTED_EDGE ( 'NONE', *, *, #3434, .F. ) ;
#997 = CARTESIAN_POINT ( 'NONE',  ( -37.00000000000000711, 4.339012074900111315, -10.91536515067643620 ) ) ;
#998 = EDGE_CURVE ( 'NONE', #52904, #10633, #38823, .T. ) ;
#999 = CARTESIAN_POINT ( 'NONE',  ( -27.09030469827879628, 0.6314616953885330286, 2.221523195520524574 ) ) ;
#1000 = FACE_OUTER_BOUND ( 'NONE', #53126, .T. ) ;
#1001 = ADVANCED_FACE ( 'NONE', ( #289 ), #9308, .F. ) ;
#1002 = DIRECTION ( 'NONE',  ( 0.000000000000000000, 0.000000000000000000, 1.000000000000000000 ) ) ;
#1003 = CARTESIAN_POINT ( 'NONE',  ( 2.034671305878333225, -5.218565780491386086, -10.44529075079083213 ) ) ;
#1004 = FACE_OUTER_BOUND ( 'NONE', #17361, .T. ) ;
#1005 = EDGE_CURVE ( 'NONE', #21005, #53943, #44133, .T. ) ;
#1006 = AXIS2_PLACEMENT_3D ( 'NONE', #6026, #45915, #46251 ) ;
#1007 = ORIENTED_EDGE ( 'NONE', *, *, #42228, .T. ) ;
#1008 = CARTESIAN_POINT ( 'NONE',  ( 2.000000000000001776, 1.058508696394974358, 6.730038252034905355 ) ) ;
#1009 = ADVANCED_FACE ( 'NONE', ( #26854 ), #62740, .T. ) ;
#1010 = AXIS2_PLACEMENT_3D ( 'NONE', #24968, #10626, #19322 ) ;
#1011 = ORIENTED_EDGE ( 'NONE', *, *, #26962, .F. ) ;
#1012 = CARTESIAN_POINT ( 'NONE',  ( 20.00005080000000035, 0.000000000000000000, 4.000000000000000000 ) ) ;
#1013 = CARTESIAN_POINT ( 'NONE',  ( 7.856790134851108220, -26.39165916151114999, -14.61432118582568407 ) ) ;
#1014 = CARTESIAN_POINT ( 'NONE',  ( 37.00000000000000711, 4.705694406421931860E-17, -3.469127814946512892E-15 ) ) ;
#1015 = EDGE_CURVE ( 'NONE', #35544, #27543, #32852, .T. ) ;
#1016 = LINE ( 'NONE', #52861, #2253 ) ;
#1017 = CARTESIAN_POINT ( 'NONE',  ( -22.30625920655495165, -1.076742202099160606, -3.635849356906424745 ) ) ;
#1018 = ORIENTED_EDGE ( 'NONE', *, *, #29438, .F. ) ;
#1019 = DIRECTION ( 'NONE',  ( 0.000000000000000000, -0.01356324068818000848, 0.9999080150203990547 ) ) ;
#1020 = FACE_OUTER_BOUND ( 'NONE', #1382, .T. ) ;
#1021 = FACE_OUTER_BOUND ( 'NONE', #10782, .T. ) ;
#1022 = CARTESIAN_POINT ( 'NONE',  ( 22.12238245485356458, -12.73425672584572332, -4.485642937375443395 ) ) ;
#1023 = B_SPLINE_CURVE_WITH_KNOTS ( 'NONE', 3,
 ( #2979, #13270, #33551, #28551, #65099, #65414, #61104, #15536, #44480, #45156, #24542, #30187 ),
 .UNSPECIFIED., .F., .F.,
 ( 4, 2, 2, 2, 2, 4 ),
 ( 1.734723475976807094E-18, 0.002074334512336499341, 0.003111501768504749445, 0.004148669024672999549, 0.006223003537009496287, 0.008297338049345992159 ),
 .UNSPECIFIED. ) ;
#1024 = VECTOR ( 'NONE', #60903, 1000.000000000000000 ) ;
#1025 = VECTOR ( 'NONE', #16569, 1000.000000000000000 ) ;
#1026 = CARTESIAN_POINT ( 'NONE',  ( 0.2717059086739037066, 12.24704971877459592, -0.1760722388998280097 ) ) ;
#1027 = CARTESIAN_POINT ( 'NONE',  ( 5.516018279890452902, -0.004180585980734566158, 0.005331956019561453694 ) ) ;
#1028 = CARTESIAN_POINT ( 'NONE',  ( -35.00000000000000000, 11.98254675519231682, -2.220215194441768514 ) ) ;
#1029 = CARTESIAN_POINT ( 'NONE',  ( 35.00000000000000000, -8.573591947375261313, 8.029056188533775895 ) ) ;
#1030 = CARTESIAN_POINT ( 'NONE',  ( 2.259830038564998311, 0.1377140217660240973, -7.639319632525571002 ) ) ;
#1031 = ADVANCED_FACE ( 'NONE', ( #43113 ), #42126, .T. ) ;
#1032 = VERTEX_POINT ( 'NONE', #32477 ) ;
#1033 = EDGE_CURVE ( 'NONE', #57362, #60006, #14589, .T. ) ;
#1034 = ORIENTED_EDGE ( 'NONE', *, *, #30537, .T. ) ;
#1035 = CARTESIAN_POINT ( 'NONE',  ( 0.2652384770603646302, 2.061429379240482085, 12.07140968216694610 ) ) ;
#1036 = CARTESIAN_POINT ( 'NONE',  ( 46.86486279825821555, -0.6193039491651846085, 9.927184253397724589 ) ) ;
#1037 = DIRECTION ( 'NONE',  ( -1.000000000000000000, 0.000000000000000000, 0.000000000000000000 ) ) ;
#1038 = DIRECTION ( 'NONE',  ( 0.000000000000000000, 0.01356324068817998940, -0.9999080150203990547 ) ) ;
#1039 = ORIENTED_EDGE ( 'NONE', *, *, #46514, .F. ) ;
#1040 = EDGE_CURVE ( 'NONE', #59522, #20687, #26505, .T. ) ;
#1041 = ORIENTED_EDGE ( 'NONE', *, *, #25305, .F. ) ;
#1043 = ORIENTED_EDGE ( 'NONE', *, *, #24378, .F. ) ;
#1042 = B_SPLINE_CURVE_WITH_KNOTS ( 'NONE', 3,
 ( #23940, #43878, #8628, #58879, #19266, #64468, #18938, #3676, #64162, #13293, #33579, #18636, #38895, #54528, #39203, #59496 ),
 .UNSPECIFIED., .F., .F.,
 ( 4, 3, 3, 3, 3, 4 ),
 ( 1.453652989256292427E-15, 0.0002126834539180066941, 0.0004253519300366991030, 0.0006380165497225274117, 0.0007442707582429557286, 0.0009453531351408830897 ),
 .UNSPECIFIED. ) ;
#1044 = CARTESIAN_POINT ( 'NONE',  ( 2.756135405615951955E-15, -45.00000000000000000, 22.50555349946515804 ) ) ;
#1046 = LINE ( 'NONE', #40617, #52317 ) ;
#1045 = AXIS2_PLACEMENT_3D ( 'NONE', #33482, #4199, #54087 ) ;
#1047 = AXIS2_PLACEMENT_3D ( 'NONE', #27167, #17845, #32464 ) ;
#1048 = ORIENTED_EDGE ( 'NONE', *, *, #11029, .T. ) ;
#1049 = DIRECTION ( 'NONE',  ( -1.000000000000000000, 0.000000000000000000, 0.000000000000000000 ) ) ;
#1050 = DIRECTION ( 'NONE',  ( 1.000000000000000000, 0.000000000000000000, 0.000000000000000000 ) ) ;
#1051 = VERTEX_POINT ( 'NONE', #11553 ) ;
#1052 = CARTESIAN_POINT ( 'NONE',  ( -22.29479313954897890, 0.2707859422896981005, 3.724550806388638780 ) ) ;
#1053 = AXIS2_PLACEMENT_3D ( 'NONE', #55646, #61272, #35333 ) ;
#1054 = CARTESIAN_POINT ( 'NONE',  ( 9.591596427418878079, -32.12122108032075118, -13.09346764506430993 ) ) ;
#1055 = CARTESIAN_POINT ( 'NONE',  ( 37.00000000000000711, 4.705694406421931860E-17, -3.469127814946512892E-15 ) ) ;
#1056 = VERTEX_POINT ( 'NONE', #39108 ) ;
#1057 = CARTESIAN_POINT ( 'NONE',  ( 0.2657645697724713152, 12.08564806881063980, -1.977350809428408906 ) ) ;
#1058 = EDGE_CURVE ( 'NONE', #16108, #50142, #55821, .T. ) ;
#1059 = ORIENTED_EDGE ( 'NONE', *, *, #49853, .T. ) ;
#1060 = CARTESIAN_POINT ( 'NONE',  ( 1.104777566491141227, 7.679758239385275687, -9.895624035729994716 ) ) ;
#1061 = LINE ( 'NONE', #57586, #15991 ) ;
#1062 = EDGE_CURVE ( 'NONE', #33180, #57362, #50334, .T. ) ;
#1063 = AXIS2_PLACEMENT_3D ( 'NONE', #861, #10178, #41085 ) ;
#1064 = CARTESIAN_POINT ( 'NONE',  ( -4.348075857607831551, -31.41176936172747958, 14.02665938297152870 ) ) ;
#1065 = CARTESIAN_POINT ( 'NONE',  ( -24.22918518688384282, 4.353569350872102284, 0.3685645067157813370 ) ) ;
#1066 = DIRECTION ( 'NONE',  ( 1.000000000000000000, 0.000000000000000000, 0.000000000000000000 ) ) ;
#1067 = CARTESIAN_POINT ( 'NONE',  ( -35.00000000000000000, -11.26103545359858060, 3.340853584269496412 ) ) ;
#1068 = CARTESIAN_POINT ( 'NONE',  ( -27.28573687977896611, -2.255103317860393197, -1.818142657385574790 ) ) ;
#1069 = CARTESIAN_POINT ( 'NONE',  ( 0.2653519789438757992, 4.209148152332916837, 11.50012635727056853 ) ) ;
#1071 = ORIENTED_EDGE ( 'NONE', *, *, #40860, .F. ) ;
#1070 = CARTESIAN_POINT ( 'NONE',  ( 7.309108772466194281, -6.069286178474166071, 12.06637494226818497 ) ) ;
#1072 = AXIS2_PLACEMENT_3D ( 'NONE', #24249, #60472, #45192 ) ;
#1073 = CARTESIAN_POINT ( 'NONE',  ( -35.04709527796842394, 0.01117341439754726551, -0.005292201869334239861 ) ) ;
#1074 = VERTEX_POINT ( 'NONE', #18846 ) ;
#1075 = DIRECTION ( 'NONE',  ( -1.000000000000000000, 0.000000000000000000, 0.000000000000000000 ) ) ;
#1076 = DIRECTION ( 'NONE',  ( 1.000000000000000000, 0.000000000000000000, 0.000000000000000000 ) ) ;
#1077 = ORIENTED_EDGE ( 'NONE', *, *, #61845, .T. ) ;
#1078 = FACE_OUTER_BOUND ( 'NONE', #64648, .T. ) ;
#1079 = CARTESIAN_POINT ( 'NONE',  ( 37.00000000000000711, 4.705694406421931860E-17, -3.469127814946512892E-15 ) ) ;
#1080 = AXIS2_PLACEMENT_3D ( 'NONE', #63758, #8253, #58147 ) ;
#1081 = DIRECTION ( 'NONE',  ( 0.000000000000000000, 0.2006870767258889243, -0.9796553971857742127 ) ) ;
#1082 = CARTESIAN_POINT ( 'NONE',  ( -35.04643116707788408, 0.01204777744935082995, -0.001845126042314057524 ) ) ;
#1083 = EDGE_CURVE ( 'NONE', #21740, #52529, #32443, .T. ) ;
#1084 = CARTESIAN_POINT ( 'NONE',  ( 2.000000000000001776, 0.000000000000000000, 0.000000000000000000 ) ) ;
#1085 = ORIENTED_EDGE ( 'NONE', *, *, #1083, .F. ) ;
#1086 = CARTESIAN_POINT ( 'NONE',  ( 37.00000000000000711, 6.415447294506860132, 11.01837265713066039 ) ) ;
#1087 = EDGE_CURVE ( 'NONE', #56385, #30158, #48430, .T. ) ;
#1088 = ORIENTED_EDGE ( 'NONE', *, *, #19961, .F. ) ;
#1089 = CARTESIAN_POINT ( 'NONE',  ( -35.04683013664716640, -0.01065093278703673797, 0.006266879427257444207 ) ) ;
#1090 = DIRECTION ( 'NONE',  ( 0.000000000000000000, 0.5987040770935676548, -0.8009703041134167423 ) ) ;
#1091 = EDGE_CURVE ( 'NONE', #33895, #14308, #19679, .T. ) ;
#1092 = FACE_OUTER_BOUND ( 'NONE', #61960, .T. ) ;
#1093 = ORIENTED_EDGE ( 'NONE', *, *, #44532, .F. ) ;
#1094 = LINE ( 'NONE', #21366, #20226 ) ;
#1095 = CIRCLE ( 'NONE', #9555, 5.000000000000000000 ) ;
#1096 =( GEOMETRIC_REPRESENTATION_CONTEXT ( 3 ) GLOBAL_UNCERTAINTY_ASSIGNED_CONTEXT ( ( #2439 ) ) GLOBAL_UNIT_ASSIGNED_CONTEXT ( ( #30433, #21104, #11150 ) ) REPRESENTATION_CONTEXT ( 'NONE', 'WORKASPACE' ) );
#1097 = DIRECTION ( 'NONE',  ( -1.000000000000000000, 0.000000000000000000, 0.000000000000000000 ) ) ;
#1098 = DIRECTION ( 'NONE',  ( 0.000000000000000000, 0.5472293298355214164, -0.8369827122275381726 ) ) ;
#1099 = CARTESIAN_POINT ( 'NONE',  ( -28.66013792860432119, 1.673433383655442697, 0.7552004871165165500 ) ) ;
#1100 = CARTESIAN_POINT ( 'NONE',  ( -27.45775109278351067, 25.00000000000000000, -8.471355351200609007 ) ) ;
#1101 = CARTESIAN_POINT ( 'NONE',  ( 2.257661810676417691, -5.764872664104550459, 5.013319178751149963 ) ) ;
#1102 = DIRECTION ( 'NONE',  ( -1.000000000000000000, 0.000000000000000000, 0.000000000000000000 ) ) ;
#1103 = VECTOR ( 'NONE', #57071, 1000.000000000000000 ) ;
#1104 = B_SPLINE_CURVE_WITH_KNOTS ( 'NONE', 3,
 ( #36509, #936, #65439, #25213, #45834, #40167, #46481 ),
 .UNSPECIFIED., .F., .F.,
 ( 4, 3, 4 ),
 ( 0.000000000000000000, 0.001700533616330591547, 0.005002426799371403193 ),
 .UNSPECIFIED. ) ;
#1105 = ORIENTED_EDGE ( 'NONE', *, *, #29117, .F. ) ;
#1106 = CARTESIAN_POINT ( 'NONE',  ( -17.13707773434846970, 7.268845792200386846, 11.37713557020030208 ) ) ;
#1107 = CARTESIAN_POINT ( 'NONE',  ( -37.00000000000000711, 10.64792938439755510, 5.927257550915356887 ) ) ;
#1108 = CIRCLE ( 'NONE', #30794, 3.999999999999999112 ) ;
#1109 = EDGE_CURVE ( 'NONE', #46540, #6959, #56926, .T. ) ;
#1110 = ORIENTED_EDGE ( 'NONE', *, *, #38666, .T. ) ;
#1111 = CARTESIAN_POINT ( 'NONE',  ( -22.27720412283625961, 3.493592264983219398, 1.161733799004142309 ) ) ;
#1112 = CARTESIAN_POINT ( 'NONE',  ( -8.382709950485196515, 9.053270168017110819, -10.03930267771108475 ) ) ;
#1113 = VERTEX_POINT ( 'NONE', #19502 ) ;
#1114 = DIRECTION ( 'NONE',  ( -1.000000000000000000, -0.000000000000000000, -0.000000000000000000 ) ) ;
#1115 = DIRECTION ( 'NONE',  ( 0.000000000000000000, -0.3807014730195085739, 0.9246979985058777496 ) ) ;
#1116 = EDGE_LOOP ( 'NONE', ( #42630, #41333, #24812, #1836 ) ) ;
#1117 = AXIS2_PLACEMENT_3D ( 'NONE', #41618, #17000, #31633 ) ;
#1118 = CARTESIAN_POINT ( 'NONE',  ( 3.152665057735843490, -3.546019893114926713, 7.102135024646879735 ) ) ;
#1119 = ORIENTED_EDGE ( 'NONE', *, *, #35766, .T. ) ;
#1120 = ORIENTED_EDGE ( 'NONE', *, *, #9168, .T. ) ;
#1121 = CARTESIAN_POINT ( 'NONE',  ( -27.08417473062937120, -1.729223128152646671, 1.503027223283678548 ) ) ;
#1122 = EDGE_LOOP ( 'NONE', ( #11131, #28574, #253, #22854 ) ) ;
#1123 = DIRECTION ( 'NONE',  ( -1.000000000000000000, -0.000000000000000000, -0.000000000000000000 ) ) ;
#1124 = DIRECTION ( 'NONE',  ( -1.000000000000000000, -0.000000000000000000, -0.000000000000000000 ) ) ;
#1125 = DIRECTION ( 'NONE',  ( 1.000000000000000000, -0.000000000000000000, 0.000000000000000000 ) ) ;
#1126 = CIRCLE ( 'NONE', #7463, 7.499999999999988454 ) ;
#1127 = CARTESIAN_POINT ( 'NONE',  ( 0.6473888112830232799, -0.3298838684457962023, -12.36914475328378060 ) ) ;
#1128 = ORIENTED_EDGE ( 'NONE', *, *, #56050, .T. ) ;
#1129 = DIRECTION ( 'NONE',  ( -1.000000000000000000, 0.000000000000000000, -0.000000000000000000 ) ) ;
#1130 = CARTESIAN_POINT ( 'NONE',  ( 8.754896909465220034, -28.78086681028207749, 9.883947858767236028 ) ) ;
#1131 = CYLINDRICAL_SURFACE ( 'NONE', #46206, 7.499999999999988454 ) ;
#1133 = ORIENTED_EDGE ( 'NONE', *, *, #28308, .T. ) ;
#1132 = DIRECTION ( 'NONE',  ( 1.000000000000000000, -0.000000000000000000, 0.000000000000000000 ) ) ;
#1135 = CIRCLE ( 'NONE', #10652, 12.18649999999999878 ) ;
#1134 = CYLINDRICAL_SURFACE ( 'NONE', #47965, 20.00000000000000000 ) ;
#1136 = EDGE_CURVE ( 'NONE', #35622, #23170, #24469, .T. ) ;
#1137 = ORIENTED_EDGE ( 'NONE', *, *, #46137, .F. ) ;
#1138 = CARTESIAN_POINT ( 'NONE',  ( 35.00000000000000000, 4.041347439436019151, 11.02904044024204211 ) ) ;
#1139 = ORIENTED_EDGE ( 'NONE', *, *, #35866, .T. ) ;
#1140 = CARTESIAN_POINT ( 'NONE',  ( 24.48732188013169520, -8.567156455853016439, -8.406226182303409900 ) ) ;
#1141 = CARTESIAN_POINT ( 'NONE',  ( 35.00000000000000000, -12.31350058095520339, 3.307597835713371737 ) ) ;
#1142 = EDGE_CURVE ( 'NONE', #5306, #8685, #3822, .T. ) ;
#1143 = DIRECTION ( 'NONE',  ( 1.000000000000000000, 0.000000000000000000, -0.000000000000000000 ) ) ;
#1144 = CIRCLE ( 'NONE', #29776, 6.936499999999989008 ) ;
#1145 = ORIENTED_EDGE ( 'NONE', *, *, #50067, .F. ) ;
#1146 = VECTOR ( 'NONE', #37888, 1000.000000000000000 ) ;
#1148 = AXIS2_PLACEMENT_3D ( 'NONE', #55835, #61145, #51522 ) ;
#1147 = DIRECTION ( 'NONE',  ( 0.000000000000000000, 0.01356324068817998940, -0.9999080150203990547 ) ) ;
#1149 = CARTESIAN_POINT ( 'NONE',  ( -19.63078887151198515, 11.93475341793434730, -1.289600524599101572 ) ) ;
#1150 = CYLINDRICAL_SURFACE ( 'NONE', #57509, 7.499999999999988454 ) ;
#1151 = ORIENTED_EDGE ( 'NONE', *, *, #37057, .T. ) ;
#1152 = ORIENTED_EDGE ( 'NONE', *, *, #45461, .T. ) ;
#1153 = CARTESIAN_POINT ( 'NONE',  ( 35.00000000000000000, 2.772148766916280316, 11.86701198550353098 ) ) ;
#1154 = ORIENTED_EDGE ( 'NONE', *, *, #32074, .F. ) ;
#1155 = ORIENTED_EDGE ( 'NONE', *, *, #41410, .F. ) ;
#1156 = CARTESIAN_POINT ( 'NONE',  ( 35.00000000000000000, -11.68758509253247091, 1.171570255487570655 ) ) ;
#1157 = CARTESIAN_POINT ( 'NONE',  ( 0.7400311444011731243, -10.56075429936772103, 6.506979270898144208 ) ) ;
#1158 = CARTESIAN_POINT ( 'NONE',  ( 2.241537034860906275, -7.172440248506141813, -2.615577641485596239 ) ) ;
#1159 = CARTESIAN_POINT ( 'NONE',  ( 25.00000000000000355, -28.99999999999999645, -4.999999999999999112 ) ) ;
#1161 = AXIS2_PLACEMENT_3D ( 'NONE', #49958, #33676, #43990 ) ;
#1160 = DIRECTION ( 'NONE',  ( 0.000000000000000000, 0.7790879021242529401, -0.6269146997507959451 ) ) ;
#1162 = EDGE_CURVE ( 'NONE', #12842, #47761, #3890, .T. ) ;
#1163 = CIRCLE ( 'NONE', #38299, 4.999999999999999112 ) ;
#1164 = DIRECTION ( 'NONE',  ( 0.000000000000000000, -0.000000000000000000, 1.000000000000000000 ) ) ;
#1165 = CYLINDRICAL_SURFACE ( 'NONE', #49359, 12.74999999999999822 ) ;
#1166 = CIRCLE ( 'NONE', #20287, 4.999999999999999112 ) ;
#1167 =( BOUNDED_SURFACE ( )  B_SPLINE_SURFACE ( 3, 1, ( 
 ( #31988, #5779 ),
 ( #45999, #51654 ),
 ( #36332, #46982 ),
 ( #456, #57625 ) ),
 .UNSPECIFIED., .F., .F., .F. ) 
 B_SPLINE_SURFACE_WITH_KNOTS ( ( 4, 4 ),
 ( 2, 2 ),
 ( 0.000000000000000000, 1.000000000000000000 ),
 ( 0.000000000000000000, 1.000000000000000000 ),
 .UNSPECIFIED. ) 
 GEOMETRIC_REPRESENTATION_ITEM ( )  RATIONAL_B_SPLINE_SURFACE ( (
 ( 1.000000000000000000, 1.000000000000000000),
 ( 0.8716676215708681896, 0.8964445200148167814),
 ( 0.8716676215708681896, 0.8964445200148167814),
 ( 1.000000000000000000, 1.000000000000000000) ) ) 
 REPRESENTATION_ITEM ( '' )  SURFACE ( )  );
#1168 = ORIENTED_EDGE ( 'NONE', *, *, #27101, .T. ) ;
#1169 = AXIS2_PLACEMENT_3D ( 'NONE', #39836, #34520, #50801 ) ;
#1170 = B_SPLINE_CURVE_WITH_KNOTS ( 'NONE', 3,
 ( #43101, #1589, #42425, #52771, #17191, #57774, #63376, #17844, #47780, #2231, #42772, #63066, #37796, #58090, #12505, #32780 ),
 .UNSPECIFIED., .F., .F.,
 ( 4, 2, 2, 2, 2, 2, 2, 4 ),
 ( 0.000000000000000000, 0.001069476264344462095, 0.002138952528688924191, 0.003208428793033386069, 0.004277905057377848382, 0.005347381321722308525, 0.006416857586066768669, 0.008555810114755681151 ),
 .UNSPECIFIED. ) ;
#1171 = CARTESIAN_POINT ( 'NONE',  ( 5.515188684475870851, 0.001283816547384723609, -0.005194992164431485628 ) ) ;
#1172 = CIRCLE ( 'NONE', #59553, 1.500000000000000222 ) ;
#1173 = EDGE_CURVE ( 'NONE', #14200, #27538, #25441, .T. ) ;
#1174 = CYLINDRICAL_SURFACE ( 'NONE', #20700, 12.18650000000000055 ) ;
#1175 = DIRECTION ( 'NONE',  ( -0.5551681190699946367, -0.8317381556525372810, 0.000000000000000000 ) ) ;
#1176 = CIRCLE ( 'NONE', #2225, 2.899999999999994582 ) ;
#1177 = CARTESIAN_POINT ( 'NONE',  ( 23.98848397398876386, -2.635302845098066005, -13.24129003998613818 ) ) ;
#1178 = CARTESIAN_POINT ( 'NONE',  ( 1.719304012341412724, 2.961219984259706450, -12.38166659046466300 ) ) ;
#1179 = CARTESIAN_POINT ( 'NONE',  ( 0.000000000000000000, 2.315790869867065283, 7.133520354428103616 ) ) ;
#1180 = ORIENTED_EDGE ( 'NONE', *, *, #57328, .T. ) ;
#1181 = CYLINDRICAL_SURFACE ( 'NONE', #21717, 6.936499999999988120 ) ;
#1182 = CARTESIAN_POINT ( 'NONE',  ( 3.152665057736233845, -4.725420687649230622, 6.378477742801980988 ) ) ;
#1183 = CARTESIAN_POINT ( 'NONE',  ( 2.589278595513890391, 1.107986312493318248, -7.670769623692590855 ) ) ;
#1184 = DIRECTION ( 'NONE',  ( 0.000000000000000000, 0.01356324068817998940, -0.9999080150203990547 ) ) ;
#1185 = VECTOR ( 'NONE', #16056, 1000.000000000000000 ) ;
#1186 = AXIS2_PLACEMENT_3D ( 'NONE', #32629, #36666, #57626 ) ;
#1187 = AXIS2_PLACEMENT_3D ( 'NONE', #38821, #13847, #54458 ) ;
#1188 = CYLINDRICAL_SURFACE ( 'NONE', #10759, 12.18649999999999878 ) ;
#1189 = ADVANCED_FACE ( 'NONE', ( #24151 ), #60062, .T. ) ;
#1190 = ORIENTED_EDGE ( 'NONE', *, *, #47667, .T. ) ;
#1191 = VECTOR ( 'NONE', #8769, 1000.000000000000000 ) ;
#1192 = DIRECTION ( 'NONE',  ( 0.000000000000000000, -0.01356324068817991828, 0.9999080150203990547 ) ) ;
#1193 = CARTESIAN_POINT ( 'NONE',  ( 35.00000000000000000, 4.705694406421931860E-17, -3.469127814946512892E-15 ) ) ;
#1194 = CARTESIAN_POINT ( 'NONE',  ( -37.00000000000000711, 9.557269938331666381, -7.561043153947866635 ) ) ;
#1195 = ORIENTED_EDGE ( 'NONE', *, *, #16801, .F. ) ;
#1196 = ADVANCED_FACE ( 'NONE', ( #49754 ), #20478, .T. ) ;
#1197 = CARTESIAN_POINT ( 'NONE',  ( 1.719304012338199295, 12.64775761152512423, 1.452142814150486183 ) ) ;
#1198 = DIRECTION ( 'NONE',  ( 1.000000000000000000, -0.000000000000000000, 0.000000000000000000 ) ) ;
#1199 = DIRECTION ( 'NONE',  ( 0.000000000000000000, 0.01356324068817998940, -0.9999080150203990547 ) ) ;
#1201 = VERTEX_POINT ( 'NONE', #15147 ) ;
#1200 = DIRECTION ( 'NONE',  ( -0.3162277663656185012, 0.1673616205762862574, 0.9338040949457712125 ) ) ;
#1202 = CARTESIAN_POINT ( 'NONE',  ( -27.08935880048752409, 2.235999130317591010, 0.5666837974575442693 ) ) ;
#1203 = CIRCLE ( 'NONE', #58554, 2.899999999999995470 ) ;
#1204 = CIRCLE ( 'NONE', #54337, 12.74999999999999822 ) ;
#1205 = EDGE_CURVE ( 'NONE', #54991, #48474, #10944, .T. ) ;
#1206 = CARTESIAN_POINT ( 'NONE',  ( 5.514970785353741078, -0.001326349372336327673, 0.004532877335078707229 ) ) ;
#1207 = VERTEX_POINT ( 'NONE', #1182 ) ;
#1208 = AXIS2_PLACEMENT_3D ( 'NONE', #4040, #59247, #13668 ) ;
#1209 = CARTESIAN_POINT ( 'NONE',  ( 0.3675815128205894289, -9.574637318042015011, 7.689697408877242957 ) ) ;
#1210 = FACE_OUTER_BOUND ( 'NONE', #31559, .T. ) ;
#1211 = FACE_OUTER_BOUND ( 'NONE', #48333, .T. ) ;
#1212 = CARTESIAN_POINT ( 'NONE',  ( -3.937012649977812195, -11.99793950917781871, 6.201358434801304220 ) ) ;
#1213 = CARTESIAN_POINT ( 'NONE',  ( 0.2648978790185584908, -11.46165506714225479, -4.312320170909353045 ) ) ;
#1214 = AXIS2_PLACEMENT_3D ( 'NONE', #38750, #59356, #48734 ) ;
#1215 = DIRECTION ( 'NONE',  ( -1.000000000000000000, 0.000000000000000000, 0.000000000000000000 ) ) ;
#1217 = EDGE_LOOP ( 'NONE', ( #62554, #41264, #18470, #150 ) ) ;
#1216 = DIRECTION ( 'NONE',  ( 1.000000000000000000, 0.000000000000000000, -0.000000000000000000 ) ) ;
#1218 = EDGE_CURVE ( 'NONE', #50940, #29095, #58539, .T. ) ;
#1219 = ORIENTED_EDGE ( 'NONE', *, *, #23759, .T. ) ;
#1220 = CARTESIAN_POINT ( 'NONE',  ( 36.00000000000000711, -7.379373053628790480, 10.39746860227898395 ) ) ;
#1221 = AXIS2_PLACEMENT_3D ( 'NONE', #48517, #2969, #43494 ) ;
#1222 = ORIENTED_EDGE ( 'NONE', *, *, #6307, .F. ) ;
#1223 = CARTESIAN_POINT ( 'NONE',  ( 0.000000000000000000, 0.000000000000000000, 0.000000000000000000 ) ) ;
#1224 = DIRECTION ( 'NONE',  ( -0.000000000000000000, -0.000000000000000000, -1.000000000000000000 ) ) ;
#1225 = CARTESIAN_POINT ( 'NONE',  ( -18.08686583997241115, 5.151216734910855521, 10.83812558286605920 ) ) ;
#1226 = DIRECTION ( 'NONE',  ( -1.000000000000000000, -0.000000000000000000, 0.000000000000000000 ) ) ;
#1227 = ORIENTED_EDGE ( 'NONE', *, *, #18704, .T. ) ;
#1228 = DIRECTION ( 'NONE',  ( 0.000000000000000000, 0.8989688749565143411, 0.4380125133594006681 ) ) ;
#1229 = CARTESIAN_POINT ( 'NONE',  ( -32.00000000000000711, -12.00000000000000000, 0.000000000000000000 ) ) ;
#1230 = CARTESIAN_POINT ( 'NONE',  ( -22.27718150314433387, -1.117371044661075841, 3.507884203786634458 ) ) ;
#1231 = ORIENTED_EDGE ( 'NONE', *, *, #38538, .T. ) ;
#1232 = EDGE_LOOP ( 'NONE', ( #11511, #7631, #29856, #47653 ) ) ;
#1233 = CARTESIAN_POINT ( 'NONE',  ( 27.63711073776143223, -12.51469113205075168, 5.065401719838317440 ) ) ;
#1234 = VECTOR ( 'NONE', #2454, 1000.000000000000000 ) ;
#1235 = AXIS2_PLACEMENT_3D ( 'NONE', #2780, #48642, #58287 ) ;
#1236 = ORIENTED_EDGE ( 'NONE', *, *, #57082, .T. ) ;
#1237 = CARTESIAN_POINT ( 'NONE',  ( 21.94266139820581429, -11.68884937910924293, -2.741396137623683948 ) ) ;
#1238 = CARTESIAN_POINT ( 'NONE',  ( -22.35190811654612375, 3.252894036332518723, -2.161847148103698935 ) ) ;
#1239 = DIRECTION ( 'NONE',  ( 1.000000000000000000, 0.000000000000000000, 0.000000000000000000 ) ) ;
#1240 = CARTESIAN_POINT ( 'NONE',  ( -27.08579483061179261, 0.9690219683526832828, -2.081508743190604083 ) ) ;
#1241 = VECTOR ( 'NONE', #6426, 1000.000000000000000 ) ;
#1242 = AXIS2_PLACEMENT_3D ( 'NONE', #60511, #15295, #41533 ) ;
#1243 = LINE ( 'NONE', #20853, #12880 ) ;
#1244 = CARTESIAN_POINT ( 'NONE',  ( 35.00000000000000000, -4.986700593229777212, -10.63508530065520219 ) ) ;
#1245 = VECTOR ( 'NONE', #6917, 1000.000000000000000 ) ;
#1246 = CARTESIAN_POINT ( 'NONE',  ( 2.251139882113959878, 7.499076289418103336, 1.448366094935441550 ) ) ;
#1247 = EDGE_LOOP ( 'NONE', ( #2779, #5008, #62184, #20386 ) ) ;
#1248 = CARTESIAN_POINT ( 'NONE',  ( -35.00000000000000000, 0.000000000000000000, 0.000000000000000000 ) ) ;
#1249 = VERTEX_POINT ( 'NONE', #5189 ) ;
#1250 = DIRECTION ( 'NONE',  ( 0.000000000000000000, 0.07632122047556488820, -0.9970832820307038435 ) ) ;
#1251 = LINE ( 'NONE', #62721, #48697 ) ;
#1252 = CARTESIAN_POINT ( 'NONE',  ( 26.08439714455133185, -12.97057518889163674, 3.743551691817328386 ) ) ;
#1253 = CARTESIAN_POINT ( 'NONE',  ( 35.00000000000000000, -5.921969905510278132, 10.14408668126219304 ) ) ;
#1255 = B_SPLINE_CURVE_WITH_KNOTS ( 'NONE', 3,
 ( #54171, #8611, #43196, #19252, #7638, #53852, #59483, #34200, #27923, #33230, #43864, #64455, #39518 ),
 .UNSPECIFIED., .F., .F.,
 ( 4, 3, 3, 3, 4 ),
 ( 2.453269466693398698E-18, 6.607593386745386026E-05, 0.0001321518677373480157, 0.0001982171734706193690, 0.0002642860854759500723 ),
 .UNSPECIFIED. ) ;
#1254 = DIRECTION ( 'NONE',  ( 1.000000000000000000, 0.000000000000000000, 0.000000000000000000 ) ) ;
#1256 = FACE_BOUND ( 'NONE', #34167, .T. ) ;
#1257 = AXIS2_PLACEMENT_3D ( 'NONE', #41429, #62068, #5570 ) ;
#1258 = ORIENTED_EDGE ( 'NONE', *, *, #38065, .T. ) ;
#1259 = EDGE_CURVE ( 'NONE', #40664, #61618, #26125, .T. ) ;
#1260 = CIRCLE ( 'NONE', #23566, 6.936499999999989008 ) ;
#1261 = EDGE_LOOP ( 'NONE', ( #2127, #37907, #43374, #41136 ) ) ;
#1262 = CARTESIAN_POINT ( 'NONE',  ( 1.452237505248555660, -10.65201107290472393, 6.833827325205280800 ) ) ;
#1263 = AXIS2_PLACEMENT_3D ( 'NONE', #9918, #44836, #55139 ) ;
#1264 = ORIENTED_EDGE ( 'NONE', *, *, #30145, .F. ) ;
#1265 = CARTESIAN_POINT ( 'NONE',  ( -22.29479313954897890, -3.724550806388635227, 0.2707859422896675139 ) ) ;
#1266 = DIRECTION ( 'NONE',  ( 0.000000000000000000, 0.000000000000000000, 1.000000000000000000 ) ) ;
#1267 = AXIS2_PLACEMENT_3D ( 'NONE', #42009, #42317, #47666 ) ;
#1268 = CARTESIAN_POINT ( 'NONE',  ( 2.253265082352446935, 4.810902415501113971, 5.932955906470541052 ) ) ;
#1269 = CARTESIAN_POINT ( 'NONE',  ( 2.258463476536644698, 1.460294809171041708, -7.499249607179725885 ) ) ;
#1270 = ORIENTED_EDGE ( 'NONE', *, *, #14859, .T. ) ;
#1271 = DIRECTION ( 'NONE',  ( 0.000000000000000000, 0.000000000000000000, 1.000000000000000000 ) ) ;
#1273 = VECTOR ( 'NONE', #55372, 1000.000000000000000 ) ;
#1272 = DIRECTION ( 'NONE',  ( 0.000000000000000000, 0.01356324068817991828, -0.9999080150203990547 ) ) ;
#1274 = CARTESIAN_POINT ( 'NONE',  ( 1.104777566491146112, -1.703053712365408368, 12.40974092093471448 ) ) ;
#1275 = DIRECTION ( 'NONE',  ( 0.000000000000000000, 0.000000000000000000, 1.000000000000000000 ) ) ;
#1276 = EDGE_CURVE ( 'NONE', #40046, #47952, #60886, .T. ) ;
#1277 = CARTESIAN_POINT ( 'NONE',  ( 35.00000000000000000, 6.891188680298960811, 9.512294188640820991 ) ) ;
#1278 = CIRCLE ( 'NONE', #10844, 7.938172270156617749 ) ;
#1279 = CARTESIAN_POINT ( 'NONE',  ( -28.66013792860432119, 0.4872053345172169814, -1.770123732198267463 ) ) ;
#1280 = VERTEX_POINT ( 'NONE', #10480 ) ;
#1281 = EDGE_CURVE ( 'NONE', #41836, #46784, #10112, .T. ) ;
#1282 = DIRECTION ( 'NONE',  ( 0.000000000000000000, 0.000000000000000000, 1.000000000000000000 ) ) ;
#1283 = ORIENTED_EDGE ( 'NONE', *, *, #51389, .T. ) ;
#1284 = EDGE_CURVE ( 'NONE', #44262, #34193, #56371, .T. ) ;
#1285 = CARTESIAN_POINT ( 'NONE',  ( 0.000000000000000000, 0.000000000000000000, 0.000000000000000000 ) ) ;
#1286 = CARTESIAN_POINT ( 'NONE',  ( 37.00000000000000711, 12.18359334611896294, 0.2661492558803733588 ) ) ;
#1287 = CARTESIAN_POINT ( 'NONE',  ( 3.152665057734040488, 0.000000000000000000, 0.000000000000000000 ) ) ;
#1288 = CARTESIAN_POINT ( 'NONE',  ( 0.2646305136544065406, -9.296005949277276414, 7.972778379581520802 ) ) ;
#1289 = CYLINDRICAL_SURFACE ( 'NONE', #23548, 6.936499999999988120 ) ;
#1290 = CIRCLE ( 'NONE', #40516, 5.000000000000000888 ) ;
#1291 = CIRCLE ( 'NONE', #35191, 12.75000000000000178 ) ;
#1292 = ORIENTED_EDGE ( 'NONE', *, *, #30703, .T. ) ;
#1294 = VERTEX_POINT ( 'NONE', #16138 ) ;
#1293 = ADVANCED_FACE ( 'NONE', ( #5868 ), #46400, .T. ) ;
#1295 = LINE ( 'NONE', #635, #38213 ) ;
#1296 = ORIENTED_EDGE ( 'NONE', *, *, #64814, .F. ) ;
#1297 = CARTESIAN_POINT ( 'NONE',  ( -35.00000000000000000, -3.916263239775430005, 11.07407352312211302 ) ) ;
#1298 = CARTESIAN_POINT ( 'NONE',  ( 2.311395794103597190, 2.385532211604124431, -13.30448733390617200 ) ) ;
#1299 = DIRECTION ( 'NONE',  ( 0.000000000000000000, 0.9651210252299786685, 0.2618041379715667083 ) ) ;
#1300 = CARTESIAN_POINT ( 'NONE',  ( 1.020182472820979624, 9.280950437305079959, 8.370187102468841900 ) ) ;
#1301 = CARTESIAN_POINT ( 'NONE',  ( 2.907497136248777370, 7.848280798452265117, -0.3592423305246287835 ) ) ;
#1302 = EDGE_CURVE ( 'NONE', #3684, #16346, #11158, .T. ) ;
#1303 = CARTESIAN_POINT ( 'NONE',  ( -34.00000000000000000, 1.836970198721035357E-16, 0.000000000000000000 ) ) ;
#1304 = DIRECTION ( 'NONE',  ( 0.000000000000000000, 0.9985334138511240409, -0.05413890858541454271 ) ) ;
#1305 = ORIENTED_EDGE ( 'NONE', *, *, #43787, .F. ) ;
#1306 = CARTESIAN_POINT ( 'NONE',  ( 0.7400311444011726802, -5.892391870929093223, 10.91558650018040844 ) ) ;
#1307 = ORIENTED_EDGE ( 'NONE', *, *, #42679, .F. ) ;
#1308 = CARTESIAN_POINT ( 'NONE',  ( 35.00000000000000000, 11.30684963584395675, 4.545979934229284147 ) ) ;
#1309 = AXIS2_PLACEMENT_3D ( 'NONE', #24829, #20155, #14812 ) ;
#1310 = CARTESIAN_POINT ( 'NONE',  ( 37.00000000000000711, -11.68758509253247091, 1.171570255487570655 ) ) ;
#1312 = EDGE_CURVE ( 'NONE', #11089, #62148, #17781, .T. ) ;
#1311 = CIRCLE ( 'NONE', #12966, 7.938172270156617749 ) ;
#1313 = CARTESIAN_POINT ( 'NONE',  ( 37.00000000000000711, -11.23004253107767880, -4.732539170486222524 ) ) ;
#1314 = ORIENTED_EDGE ( 'NONE', *, *, #9225, .T. ) ;
#1315 = CARTESIAN_POINT ( 'NONE',  ( 37.00000000000000711, -12.18632975068352664, -0.06441628369832411161 ) ) ;
#1316 = CARTESIAN_POINT ( 'NONE',  ( -19.56743653832047158, -33.00000000000000000, 5.000000000000000888 ) ) ;
#1317 = DIRECTION ( 'NONE',  ( -1.000000000000000000, -0.000000000000000000, -0.000000000000000000 ) ) ;
#1318 = ORIENTED_EDGE ( 'NONE', *, *, #37285, .F. ) ;
#1319 = AXIS2_PLACEMENT_3D ( 'NONE', #334, #15284, #14603 ) ;
#1321 = ADVANCED_FACE ( 'NONE', ( #63314 ), #37395, .T. ) ;
#1320 = EDGE_LOOP ( 'NONE', ( #39520, #12299, #58562, #58515 ) ) ;
#1322 = CARTESIAN_POINT ( 'NONE',  ( 1.557635548354367794, 1.399767314629970505, 13.43135513698036299 ) ) ;
#1323 = EDGE_LOOP ( 'NONE', ( #39107, #2329, #36527, #17256 ) ) ;
#1324 = CARTESIAN_POINT ( 'NONE',  ( 0.5547464869798220954, -11.69908463509554331, -3.933612953276354851 ) ) ;
#1325 = VERTEX_POINT ( 'NONE', #7813 ) ;
#1326 = VERTEX_POINT ( 'NONE', #28096 ) ;
#1327 = ORIENTED_EDGE ( 'NONE', *, *, #32180, .F. ) ;
#1328 = CARTESIAN_POINT ( 'NONE',  ( 2.241537034860905386, -7.175668896091115023, 2.606707005150518341 ) ) ;
#1329 = CARTESIAN_POINT ( 'NONE',  ( 2.284126774967179863, 5.036818232552660923, -5.756079777200417524 ) ) ;
#1330 = CARTESIAN_POINT ( 'NONE',  ( -20.34666746044321073, -11.74305062490097029, -2.487411478320596725 ) ) ;
#1331 = CARTESIAN_POINT ( 'NONE',  ( -25.86628395826706850, 8.041618865309581921, 10.84354029019568522 ) ) ;
#1332 = FACE_OUTER_BOUND ( 'NONE', #7494, .T. ) ;
#1333 = ORIENTED_EDGE ( 'NONE', *, *, #46244, .T. ) ;
#1334 = CARTESIAN_POINT ( 'NONE',  ( -22.59983133926798615, -3.996991822164155383, -2.378226455340851420 ) ) ;
#1335 = AXIS2_PLACEMENT_3D ( 'NONE', #32137, #48122, #7196 ) ;
#1336 = VERTEX_POINT ( 'NONE', #43038 ) ;
#1337 = DIRECTION ( 'NONE',  ( -1.000000000000000000, 0.000000000000000000, 0.000000000000000000 ) ) ;
#1338 = CARTESIAN_POINT ( 'NONE',  ( -22.27711351828769892, 2.657880562424700610, -2.547249869018249235 ) ) ;
#1339 = DIRECTION ( 'NONE',  ( 0.000000000000000000, -0.01356324068817999114, 0.9999080150203989437 ) ) ;
#1340 = CARTESIAN_POINT ( 'NONE',  ( 0.3675815128205912052, 9.574637318042068301, -7.689697408877177232 ) ) ;
#1341 = CARTESIAN_POINT ( 'NONE',  ( 0.5572780756290729443, -10.53376864352709674, -6.434474476008335664 ) ) ;
#1342 = CIRCLE ( 'NONE', #7733, 5.000000000000000000 ) ;
#1343 = CIRCLE ( 'NONE', #26811, 4.999999999999999112 ) ;
#1344 = ADVANCED_FACE ( 'NONE', ( #48392 ), #32400, .T. ) ;
#1345 = AXIS2_PLACEMENT_3D ( 'NONE', #49197, #64138, #59165 ) ;
#1346 = ORIENTED_EDGE ( 'NONE', *, *, #6034, .T. ) ;
#1347 = DIRECTION ( 'NONE',  ( 1.000000000000000000, 0.000000000000000000, 0.000000000000000000 ) ) ;
#1348 = VERTEX_POINT ( 'NONE', #6497 ) ;
#1349 = FACE_OUTER_BOUND ( 'NONE', #63831, .T. ) ;
#1350 = CARTESIAN_POINT ( 'NONE',  ( 9.722110222095126986, -26.73349363795548328, -14.00621188957225272 ) ) ;
#1351 = CARTESIAN_POINT ( 'NONE',  ( 2.931247277082681180, 6.255823895767027132, -4.765826751677371576 ) ) ;
#1352 = CARTESIAN_POINT ( 'NONE',  ( 2.177405672431261152, 6.668684901899884387, -8.997150696569983452 ) ) ;
#1353 = CARTESIAN_POINT ( 'NONE',  ( -37.00000000000000711, 12.31350058095527977, -3.307597835713114609 ) ) ;
#1354 = ORIENTED_EDGE ( 'NONE', *, *, #49116, .T. ) ;
#1355 = EDGE_CURVE ( 'NONE', #63364, #34567, #51610, .T. ) ;
#1356 = CARTESIAN_POINT ( 'NONE',  ( 36.00000000000000711, -12.02534193257717732, 4.237174932027350849 ) ) ;
#1357 = CARTESIAN_POINT ( 'NONE',  ( -19.56743653832047514, -30.00000000000000000, 5.000000000000000888 ) ) ;
#1358 = CARTESIAN_POINT ( 'NONE',  ( -37.00000000000000711, 0.000000000000000000, 0.000000000000000000 ) ) ;
#1359 = CARTESIAN_POINT ( 'NONE',  ( 3.152665057734095555, 3.546019893116337141, 7.102135024645864547 ) ) ;
#1360 = AXIS2_PLACEMENT_3D ( 'NONE', #14903, #24921, #60155 ) ;
#1361 = EDGE_CURVE ( 'NONE', #21752, #26538, #18835, .T. ) ;
#1362 = CARTESIAN_POINT ( 'NONE',  ( -37.00000000000000711, 9.063649021439076137, -8.146229107149299153 ) ) ;
#1363 = CIRCLE ( 'NONE', #62902, 4.999999999999999112 ) ;
#1364 = CARTESIAN_POINT ( 'NONE',  ( -35.00000000000000000, 3.645068577060182946, -11.16627499335651130 ) ) ;
#1365 = EDGE_CURVE ( 'NONE', #54583, #6133, #31419, .T. ) ;
#1366 = CARTESIAN_POINT ( 'NONE',  ( 0.7446945582524626683, -5.891988114924091136, -10.91757157182818538 ) ) ;
#1367 = DIRECTION ( 'NONE',  ( 1.000000000000000000, -0.000000000000000000, 0.000000000000000000 ) ) ;
#1368 = DIRECTION ( 'NONE',  ( 0.000000000000000000, 0.2149704402110177992, 0.9766205557100881007 ) ) ;
#1369 = VERTEX_POINT ( 'NONE', #17121 ) ;
#1370 = AXIS2_PLACEMENT_3D ( 'NONE', #58301, #28044, #48656 ) ;
#1371 = ORIENTED_EDGE ( 'NONE', *, *, #30278, .F. ) ;
#1373 = CARTESIAN_POINT ( 'NONE',  ( 2.000000000000001776, 1.836970198721030181E-16, -1.500000000000000222 ) ) ;
#1372 =( BOUNDED_CURVE ( )  B_SPLINE_CURVE ( 3, ( #42728, #17809, #52740, #7164 ),
 .UNSPECIFIED., .F., .F. ) 
 B_SPLINE_CURVE_WITH_KNOTS ( ( 4, 4 ),
 ( 4.409534938676864968, 4.430491180286858288 ),
 .UNSPECIFIED. ) 
 CURVE ( )  GEOMETRIC_REPRESENTATION_ITEM ( )  RATIONAL_B_SPLINE_CURVE ( ( 1.000000000000000000, 0.9999634033296326274, 0.9999634033296326274, 1.000000000000000000 ) ) 
 REPRESENTATION_ITEM ( '' )  );
#1374 = CARTESIAN_POINT ( 'NONE',  ( 2.000000000000001776, 6.586971819220387658, -3.586335490831350725 ) ) ;
#1375 = CARTESIAN_POINT ( 'NONE',  ( 0.7400311444011752338, -7.698344902199155904, 9.726551103566787759 ) ) ;
#1376 = ADVANCED_FACE ( 'NONE', ( #27415 ), #62998, .T. ) ;
#1377 = CARTESIAN_POINT ( 'NONE',  ( 0.2671309869109468327, -1.966882337881771248, 12.08782215308011843 ) ) ;
#1378 = ORIENTED_EDGE ( 'NONE', *, *, #20910, .F. ) ;
#1379 = EDGE_CURVE ( 'NONE', #26248, #26251, #21803, .T. ) ;
#1380 = CIRCLE ( 'NONE', #59751, 2.899999999999994582 ) ;
#1381 = ORIENTED_EDGE ( 'NONE', *, *, #64814, .T. ) ;
#1382 = EDGE_LOOP ( 'NONE', ( #26703, #19641, #8896, #19929 ) ) ;
#1383 = DIRECTION ( 'NONE',  ( -1.000000000000000000, -0.000000000000000000, 0.000000000000000000 ) ) ;
#1384 = EDGE_CURVE ( 'NONE', #9803, #36432, #16619, .T. ) ;
#1385 = AXIS2_PLACEMENT_3D ( 'NONE', #65031, #20479, #15478 ) ;
#1387 = AXIS2_PLACEMENT_3D ( 'NONE', #21736, #33335, #27348 ) ;
#1386 = CARTESIAN_POINT ( 'NONE',  ( -35.00000000000000000, 11.68758509253248334, -1.171570255487489609 ) ) ;
#1388 = EDGE_LOOP ( 'NONE', ( #16752, #1462, #26249, #1120 ) ) ;
#1389 = EDGE_CURVE ( 'NONE', #56717, #10498, #42052, .T. ) ;
#1390 = LINE ( 'NONE', #6701, #43213 ) ;
#1391 = ADVANCED_FACE ( 'NONE', ( #57364 ), #22783, .T. ) ;
#1392 = DIRECTION ( 'NONE',  ( -1.000000000000000000, 0.000000000000000000, 0.000000000000000000 ) ) ;
#1393 = VERTEX_POINT ( 'NONE', #52389 ) ;
#1394 = DIRECTION ( 'NONE',  ( -1.000000000000000000, 0.000000000000000000, 0.000000000000000000 ) ) ;
#1395 = CARTESIAN_POINT ( 'NONE',  ( 19.43600551875691451, -29.99999999999999645, -5.447264023289523749 ) ) ;
#1396 = CARTESIAN_POINT ( 'NONE',  ( 22.88594695219327235, -4.822122601967141264, 10.98850006195556261 ) ) ;
#1397 = ORIENTED_EDGE ( 'NONE', *, *, #11958, .F. ) ;
#1398 = EDGE_CURVE ( 'NONE', #41624, #60517, #38382, .T. ) ;
#1399 = CARTESIAN_POINT ( 'NONE',  ( 0.2648978790185593790, 12.08224454301451445, -1.996248716311504801 ) ) ;
#1400 = ORIENTED_EDGE ( 'NONE', *, *, #54116, .T. ) ;
#1401 = CARTESIAN_POINT ( 'NONE',  ( 1.633930747253263371, 7.601388527387222815, -10.17701904908809141 ) ) ;
#1402 = CIRCLE ( 'NONE', #65067, 12.18650000000000055 ) ;
#1403 = CARTESIAN_POINT ( 'NONE',  ( -17.99580626142726913, -9.062273765671413628, 10.02044534816332444 ) ) ;
#1404 = FACE_OUTER_BOUND ( 'NONE', #7670, .T. ) ;
#1405 = AXIS2_PLACEMENT_3D ( 'NONE', #57150, #41841, #26543 ) ;
#1406 = CARTESIAN_POINT ( 'NONE',  ( 2.000000000000001776, -6.767909380267593811, 0.7805499053120233954 ) ) ;
#1407 = DIRECTION ( 'NONE',  ( 1.000000000000000000, 0.000000000000000000, 0.000000000000000000 ) ) ;
#1408 = CARTESIAN_POINT ( 'NONE',  ( 9.378405691591813920, 1.708243947577828603, 11.87965240138111334 ) ) ;
#1409 = CARTESIAN_POINT ( 'NONE',  ( 1.109979610372474168, 6.674783385105688360, -10.60154531817214085 ) ) ;
#1410 = CARTESIAN_POINT ( 'NONE',  ( -37.00000000000000711, 4.074242145636005397, 12.08151691381191917 ) ) ;
#1411 = EDGE_LOOP ( 'NONE', ( #9726, #61869, #50151, #56073 ) ) ;
#1412 = LINE ( 'NONE', #16368, #43875 ) ;
#1413 = ORIENTED_EDGE ( 'NONE', *, *, #32374, .T. ) ;
#1414 = DIRECTION ( 'NONE',  ( -1.000000000000000000, 0.000000000000000000, 0.000000000000000000 ) ) ;
#1415 = AXIS2_PLACEMENT_3D ( 'NONE', #34083, #430, #18818 ) ;
#1416 = CARTESIAN_POINT ( 'NONE',  ( 3.152665057733930798, -5.761241965769118067, -5.461013642405381674 ) ) ;
#1417 = ORIENTED_EDGE ( 'NONE', *, *, #45658, .F. ) ;
#1418 = CARTESIAN_POINT ( 'NONE',  ( 2.368238019615325651, 7.273245349264801263, 2.455958560214660746 ) ) ;
#1419 = CARTESIAN_POINT ( 'NONE',  ( 1.452237505248555660, 10.06489946308202299, 7.672309600508729233 ) ) ;
#1420 = DIRECTION ( 'NONE',  ( -0.000000000000000000, -0.000000000000000000, -1.000000000000000000 ) ) ;
#1421 = DIRECTION ( 'NONE',  ( 0.000000000000000000, -0.2355298848897586506, -0.9718671068226442111 ) ) ;
#1422 = VERTEX_POINT ( 'NONE', #54684 ) ;
#1423 = CARTESIAN_POINT ( 'NONE',  ( 2.653899356900081941, -4.109946795501341121, -6.596318473603846044 ) ) ;
#1424 = EDGE_CURVE ( 'NONE', #59191, #52452, #53699, .T. ) ;
#1425 = VECTOR ( 'NONE', #15661, 1000.000000000000000 ) ;
#1426 = ORIENTED_EDGE ( 'NONE', *, *, #42084, .F. ) ;
#1427 = CARTESIAN_POINT ( 'NONE',  ( -17.22487315615078529, -6.630673841149409498, -10.00324445667050632 ) ) ;
#1428 = ORIENTED_EDGE ( 'NONE', *, *, #17508, .T. ) ;
#1429 = CARTESIAN_POINT ( 'NONE',  ( 1.000000000000000888, -7.414200355365233364, -1.131208685655244350 ) ) ;
#1430 = DIRECTION ( 'NONE',  ( 0.000000000000000000, 0.01356324068817991828, -0.9999080150203990547 ) ) ;
#1431 = DIRECTION ( 'NONE',  ( -1.000000000000000000, 0.000000000000000000, 0.000000000000000000 ) ) ;
#1432 = ORIENTED_EDGE ( 'NONE', *, *, #31378, .F. ) ;
#1433 = AXIS2_PLACEMENT_3D ( 'NONE', #57152, #60822, #5639 ) ;
#1434 = EDGE_CURVE ( 'NONE', #33641, #15285, #25060, .T. ) ;
#1435 = AXIS2_PLACEMENT_3D ( 'NONE', #4838, #49720, #160 ) ;
#1436 = CARTESIAN_POINT ( 'NONE',  ( 0.3109076770649051857, -4.414555973477746420, -11.43910935267336804 ) ) ;
#1437 = AXIS2_PLACEMENT_3D ( 'NONE', #13118, #38721, #7136 ) ;
#1438 = AXIS2_PLACEMENT_3D ( 'NONE', #54853, #24588, #58891 ) ;
#1439 = CARTESIAN_POINT ( 'NONE',  ( 25.05309951391468459, -8.823569016628452388, -8.132934882857099979 ) ) ;
#1440 = FACE_OUTER_BOUND ( 'NONE', #7234, .T. ) ;
#1441 = CIRCLE ( 'NONE', #47057, 12.74999999999999822 ) ;
#1442 = CARTESIAN_POINT ( 'NONE',  ( -47.00000000000000711, 0.000000000000000000, 0.000000000000000000 ) ) ;
#1443 = DIRECTION ( 'NONE',  ( 0.000000000000000000, 0.01356324068817998593, -0.9999080150203990547 ) ) ;
#1444 = ADVANCED_FACE ( 'NONE', ( #44036 ), #64307, .T. ) ;
#1445 = CARTESIAN_POINT ( 'NONE',  ( -35.00000000000000000, 8.029056188533687077, 8.573591947375351907 ) ) ;
#1446 = CARTESIAN_POINT ( 'NONE',  ( 3.459614771489464946, -11.09853614738469396, -4.563167253695070258 ) ) ;
#1447 = CARTESIAN_POINT ( 'NONE',  ( 0.000000000000000000, 0.000000000000000000, 0.000000000000000000 ) ) ;
#1448 = AXIS2_PLACEMENT_3D ( 'NONE', #48467, #3236, #53776 ) ;
#1449 = EDGE_CURVE ( 'NONE', #61567, #28743, #13368, .T. ) ;
#1450 = AXIS2_PLACEMENT_3D ( 'NONE', #48727, #3181, #23447 ) ;
#1451 = ORIENTED_EDGE ( 'NONE', *, *, #30996, .F. ) ;
#1452 = CARTESIAN_POINT ( 'NONE',  ( -17.69390680376402258, 6.600471761193754894, 11.77845348364601996 ) ) ;
#1453 = DIRECTION ( 'NONE',  ( -1.000000000000000000, 0.000000000000000000, -0.000000000000000000 ) ) ;
#1454 = ORIENTED_EDGE ( 'NONE', *, *, #58874, .T. ) ;
#1455 = CARTESIAN_POINT ( 'NONE',  ( 1.549075743843518982, 10.62322497417013878, 6.912427991522386961 ) ) ;
#1456 = CARTESIAN_POINT ( 'NONE',  ( 0.5572780756290133253, -9.256402261579143698, -8.165890079445691896 ) ) ;
#1457 = CIRCLE ( 'NONE', #52440, 12.73084802173761787 ) ;
#1458 = ORIENTED_EDGE ( 'NONE', *, *, #55303, .T. ) ;
#1459 = CARTESIAN_POINT ( 'NONE',  ( -35.00000000000000000, 12.00000000000000000, 1.469576158976823947E-15 ) ) ;
#1460 = VERTEX_POINT ( 'NONE', #19429 ) ;
#1461 = CARTESIAN_POINT ( 'NONE',  ( -35.00000000000000000, -12.63095688309030251, 1.738225594539951180 ) ) ;
#1462 = ORIENTED_EDGE ( 'NONE', *, *, #37652, .F. ) ;
#1463 = ORIENTED_EDGE ( 'NONE', *, *, #41590, .T. ) ;
#1464 = ADVANCED_FACE ( 'NONE', ( #54013 ), #21162, .F. ) ;
#1465 = EDGE_CURVE ( 'NONE', #23780, #54185, #42038, .T. ) ;
#1466 = CARTESIAN_POINT ( 'NONE',  ( 2.297017764050093724, -7.133399178907334104, 2.771707546665567623 ) ) ;
#1467 = AXIS2_PLACEMENT_3D ( 'NONE', #21914, #47200, #23554 ) ;
#1468 = ORIENTED_EDGE ( 'NONE', *, *, #58715, .T. ) ;
#1469 = EDGE_CURVE ( 'NONE', #55989, #47412, #52698, .T. ) ;
#1470 = CARTESIAN_POINT ( 'NONE',  ( -24.82451523953541894, -8.749778939910779485, 8.214417963206811280 ) ) ;
#1471 = CARTESIAN_POINT ( 'NONE',  ( -22.28169757117798966, -3.561623073126547911, 0.9841724999439861454 ) ) ;
#1472 = CYLINDRICAL_SURFACE ( 'NONE', #36511, 12.18650000000000055 ) ;
#1473 = DIRECTION ( 'NONE',  ( -0.000000000000000000, -1.000000000000000000, -0.000000000000000000 ) ) ;
#1474 = VERTEX_POINT ( 'NONE', #29386 ) ;
#1475 = CARTESIAN_POINT ( 'NONE',  ( 0.2650492433740077591, -6.027445608088923379, 10.66007796911767080 ) ) ;
#1476 = CARTESIAN_POINT ( 'NONE',  ( 3.024435290549866817, -27.93754772256033192, 12.30283293119135202 ) ) ;
#1477 = CARTESIAN_POINT ( 'NONE',  ( 2.000000000000001776, 7.203928197742132333, -2.086484728383096510 ) ) ;
#1479 = VERTEX_POINT ( 'NONE', #9411 ) ;
#1478 = CARTESIAN_POINT ( 'NONE',  ( -24.30326519513172912, 8.383402268046477701, 8.588829520052238209 ) ) ;
#1480 = EDGE_CURVE ( 'NONE', #50535, #50607, #4897, .T. ) ;
#1481 = FACE_OUTER_BOUND ( 'NONE', #57483, .T. ) ;
#1482 = VERTEX_POINT ( 'NONE', #63983 ) ;
#1483 = AXIS2_PLACEMENT_3D ( 'NONE', #18572, #34782, #53801 ) ;
#1484 = DIRECTION ( 'NONE',  ( 1.000000000000000000, 0.000000000000000000, 0.000000000000000000 ) ) ;
#1485 = AXIS2_PLACEMENT_3D ( 'NONE', #4253, #44462, #34500 ) ;
#1486 = B_SPLINE_CURVE_WITH_KNOTS ( 'NONE', 3,
 ( #50746, #210, #56740, #61051, #4875, #35747, #46729, #20148, #11164, #10486, #61686, #6183, #65677, #51738, #56043, #40418 ),
 .UNSPECIFIED., .F., .F.,
 ( 4, 3, 3, 3, 3, 4 ),
 ( 2.556437191840625382E-15, 0.0002126834539179719454, 0.0004253519300366298225, 0.0006380165497224222441, 0.0007442707582428313706, 0.0009453531351417650882 ),
 .UNSPECIFIED. ) ;
#1487 = EDGE_LOOP ( 'NONE', ( #40463, #44615, #58905, #31420 ) ) ;
#1488 = CARTESIAN_POINT ( 'NONE',  ( 23.33049619018955312, -9.351986643931601506, -7.526857238819390616 ) ) ;
#1489 = DIRECTION ( 'NONE',  ( 0.000000000000000000, 0.000000000000000000, 1.000000000000000000 ) ) ;
#1490 = CARTESIAN_POINT ( 'NONE',  ( 2.298277635560269871, -7.651596582281746883, -0.1650558796844905085 ) ) ;
#1491 = ORIENTED_EDGE ( 'NONE', *, *, #26515, .F. ) ;
#1492 = DIRECTION ( 'NONE',  ( 0.000000000000000000, 0.01356324068817998940, -0.9999080150203990547 ) ) ;
#1493 = EDGE_CURVE ( 'NONE', #46522, #8559, #53740, .T. ) ;
#1494 = DIRECTION ( 'NONE',  ( 0.000000000000000000, -0.01356324068817998940, 0.9999080150203990547 ) ) ;
#1495 = CARTESIAN_POINT ( 'NONE',  ( 0.3654063281920717499, -12.04448018134537612, 2.391195511198612067 ) ) ;
#1496 = ORIENTED_EDGE ( 'NONE', *, *, #9929, .F. ) ;
#1497 = AXIS2_PLACEMENT_3D ( 'NONE', #59919, #25635, #9334 ) ;
#1498 = EDGE_LOOP ( 'NONE', ( #10895, #64421, #21344, #12911 ) ) ;
#1499 = CARTESIAN_POINT ( 'NONE',  ( 2.507146904658096531, 7.565123178000315640, 1.553587269793084369 ) ) ;
#1500 = ORIENTED_EDGE ( 'NONE', *, *, #63507, .F. ) ;
#1501 = AXIS2_PLACEMENT_3D ( 'NONE', #3959, #28890, #49202 ) ;
#1502 = VERTEX_POINT ( 'NONE', #59660 ) ;
#1503 = AXIS2_PLACEMENT_3D ( 'NONE', #7546, #12863, #16874 ) ;
#1504 = DIRECTION ( 'NONE',  ( 1.000000000000000000, 0.000000000000000000, 0.000000000000000000 ) ) ;
#1505 = DIRECTION ( 'NONE',  ( -1.000000000000000000, 0.000000000000000000, 0.000000000000000000 ) ) ;
#1506 = CARTESIAN_POINT ( 'NONE',  ( 2.665405856346786173, -7.981834391067681445, -5.274989403260977205 ) ) ;
#1507 = DIRECTION ( 'NONE',  ( 1.000000000000000000, 0.000000000000000000, 0.000000000000000000 ) ) ;
#1508 = LINE ( 'NONE', #21785, #38033 ) ;
#1509 = CIRCLE ( 'NONE', #9928, 5.000000000000000888 ) ;
#1510 = CARTESIAN_POINT ( 'NONE',  ( -9.424604252909290381, -2.780242171103320725, -11.67835095153480651 ) ) ;
#1511 = CARTESIAN_POINT ( 'NONE',  ( 2.000000000000001776, 6.201547234537079234, -2.820401998297854096 ) ) ;
#1512 = EDGE_CURVE ( 'NONE', #38977, #43321, #21885, .T. ) ;
#1513 = ORIENTED_EDGE ( 'NONE', *, *, #62573, .T. ) ;
#1514 = VECTOR ( 'NONE', #11526, 1000.000000000000000 ) ;
#1515 = DIRECTION ( 'NONE',  ( 0.000000000000000000, 0.01356324068817992175, -0.9999080150203990547 ) ) ;
#1516 = CARTESIAN_POINT ( 'NONE',  ( -3.700366998126892071, -10.78403306819907037, 5.280571526603965005 ) ) ;
#1517 = EDGE_CURVE ( 'NONE', #63755, #61730, #59022, .T. ) ;
#1518 = FACE_OUTER_BOUND ( 'NONE', #51247, .T. ) ;
#1519 = AXIS2_PLACEMENT_3D ( 'NONE', #11060, #47303, #56621 ) ;
#1520 = CARTESIAN_POINT ( 'NONE',  ( 35.00000000000000000, -11.60979404548631777, 3.704519465651427534 ) ) ;
#1521 = DIRECTION ( 'NONE',  ( -1.000000000000000000, -0.000000000000000000, 0.000000000000000000 ) ) ;
#1522 = CARTESIAN_POINT ( 'NONE',  ( 8.459345231580508440, 3.955827861842277748, -11.33263784498325322 ) ) ;
#1523 = EDGE_CURVE ( 'NONE', #39184, #59129, #3827, .T. ) ;
#1525 = EDGE_CURVE ( 'NONE', #15504, #38810, #44342, .T. ) ;
#1524 = VERTEX_POINT ( 'NONE', #24080 ) ;
#1526 = DIRECTION ( 'NONE',  ( -1.000000000000000000, 0.000000000000000000, 0.000000000000000000 ) ) ;
#1527 = AXIS2_PLACEMENT_3D ( 'NONE', #57874, #11963, #21638 ) ;
#1528 = DIRECTION ( 'NONE',  ( -1.000000000000000000, 0.000000000000000000, 0.000000000000000000 ) ) ;
#1529 = CARTESIAN_POINT ( 'NONE',  ( 2.524535260913002954, 1.123794384998896723, -7.646662375930566746 ) ) ;
#1530 = CARTESIAN_POINT ( 'NONE',  ( 2.653899356900512707, -1.606012885791721301, -7.604196386057654244 ) ) ;
#1531 = EDGE_CURVE ( 'NONE', #662, #48402, #34379, .T. ) ;
#1532 = CARTESIAN_POINT ( 'NONE',  ( 12.03570575446059365, 0.5714357744993003863, -13.48808386659669090 ) ) ;
#1533 = DIRECTION ( 'NONE',  ( 0.000000000000000000, 0.9987865678893278476, -0.04924826701374234589 ) ) ;
#1534 = CLOSED_SHELL ( 'NONE', ( #61097, #60293, #55039, #63809, #65692, #36548, #31545, #4048, #46722, #5916, #49794, #18381, #24153, #54881, #39764, #57160, #48204, #14423, #31819, #52918, #23674, #36072, #52484, #33996, #2388, #27711, #30410, #65420, #34631, #9670, #41058, #5324, #39090, #32330, #20790, #31553, #49718, #12763, #5443, #3476, #17652, #11291, #42458, #3290, #53534, #8291, #18824, #18027, #37065, #13983, #7474, #5343, #2011, #60008, #5837, #32345, #41997, #50663, #16888, #6344, #11148, #16828, #63038, #3194, #5981, #42443, #26756, #6094, #41656, #1001, #51727, #37752, #57889, #51260, #27088, #26537, #33506, #14084, #49706, #47692, #9016, #29626, #8784, #27764, #35173, #14851, #19005, #63559, #30435, #55708, #8623, #63017, #48062, #63044, #22083, #26074, #14451, #31023, #42961, #33246, #20326, #40141, #56157, #53157, #9000, #57877, #8318, #24540, #22751, #43204, #24087, #33581, #15983, #12791, #43599, #13639, #2157, #17263, #40787, #25448, #43334, #33495, #16627, #59249, #23082, #63319, #28888, #19325, #51959, #1464, #28257, #4273, #18577, #30908, #63121, #52092, #58110, #34611, #63148, #62236, #20008, #2469, #36392, #23464, #6164, #62123, #37365, #45048, #39120, #29510, #9505, #13049, #46742, #47214, #60429, #12676, #2515, #26231, #6264, #63857, #7817, #10864, #62386, #22559, #14257, #25422, #46622, #60118, #58678, #46459, #56758, #13518, #33462, #18825, #58588, #36167, #49217, #9341, #63347, #52697, #34562, #24565, #12292, #40397, #20582, #5259, #11251, #11162, #27328, #45183, #57079, #48542, #50182, #36994, #52097, #42520, #27918, #34127, #56808, #52127, #33866, #56491, #62991, #12737, #764, #54809, #34581, #1963, #19146, #55464, #21738, #34803, #48240, #25556, #62162, #42914, #50897, #19201, #2666, #51451, #11461, #45211, #36616, #33709, #23761, #29010, #16423, #46858, #60665, #26591, #6379 ) ) ;
#1535 = ORIENTED_EDGE ( 'NONE', *, *, #11385, .T. ) ;
#1536 = CARTESIAN_POINT ( 'NONE',  ( 1.719304012341585253, 9.242227816401774376, -8.755325027795295867 ) ) ;
#1537 = DIRECTION ( 'NONE',  ( -1.000000000000000000, 0.000000000000000000, 0.000000000000000000 ) ) ;
#1538 = CARTESIAN_POINT ( 'NONE',  ( -22.30625920655495165, 3.783486345733975131, -0.2529928606556600679 ) ) ;
#1539 = VERTEX_POINT ( 'NONE', #34687 ) ;
#1540 = CARTESIAN_POINT ( 'NONE',  ( -8.891032880924175430, -12.93614229090407974, -3.860857758255645589 ) ) ;
#1541 = CYLINDRICAL_SURFACE ( 'NONE', #57609, 7.499999999999988454 ) ;
#1542 = B_SPLINE_CURVE_WITH_KNOTS ( 'NONE', 3,
 ( #51876, #51564, #50572, #60863, #26268, #61497, #680, #20290, #6013, #999, #20936, #40568, #50886, #25607, #46542, #21267, #41542, #36573, #45900 ),
 .UNSPECIFIED., .F., .F.,
 ( 4, 3, 3, 3, 3, 3, 4 ),
 ( 0.000000000000000000, 2.832085443540684365E-05, 4.217789847394754410E-05, 5.603488375046140088E-05, 6.989180858579403647E-05, 9.821094829919064780E-05, 0.0001178165571465091021 ),
 .UNSPECIFIED. ) ;
#1543 = CIRCLE ( 'NONE', #56749, 4.999999999999999112 ) ;
#1545 = ORIENTED_EDGE ( 'NONE', *, *, #49357, .T. ) ;
#1544 = CARTESIAN_POINT ( 'NONE',  ( 0.2651627682582918810, -12.24583720278847210, 0.08809604936501859440 ) ) ;
#1546 = CARTESIAN_POINT ( 'NONE',  ( -37.00000000000000711, 0.000000000000000000, 0.000000000000000000 ) ) ;
#1547 = EDGE_CURVE ( 'NONE', #54224, #31440, #12444, .T. ) ;
#1548 = DIRECTION ( 'NONE',  ( 0.000000000000000000, 0.1740410799127544150, 0.9847383929261631641 ) ) ;
#1549 = EDGE_LOOP ( 'NONE', ( #57812, #3118, #14716, #20448, #33194, #50371 ) ) ;
#1550 = EDGE_CURVE ( 'NONE', #14567, #26639, #62212, .T. ) ;
#1551 = LINE ( 'NONE', #37087, #27003 ) ;
#1552 = DIRECTION ( 'NONE',  ( 0.000000000000000000, -0.8515178078024812081, 0.5243256840888652626 ) ) ;
#1553 = CARTESIAN_POINT ( 'NONE',  ( 0.2653141334712548205, -7.837911425448844227, 9.409392642815717522 ) ) ;
#1554 = FACE_OUTER_BOUND ( 'NONE', #54024, .T. ) ;
#1555 = CARTESIAN_POINT ( 'NONE',  ( -22.27722019117890540, 0.6494988092404053726, 3.623917154020592335 ) ) ;
#1556 = AXIS2_PLACEMENT_3D ( 'NONE', #41594, #52585, #31301 ) ;
#1557 = CARTESIAN_POINT ( 'NONE',  ( 0.2676618633000453218, 5.983781707237607606, 10.68562420805844582 ) ) ;
#1559 = ORIENTED_EDGE ( 'NONE', *, *, #44651, .T. ) ;
#1558 = CARTESIAN_POINT ( 'NONE',  ( 0.2648978790185619880, 11.46165506714233828, -4.312320170909121231 ) ) ;
#1560 = VERTEX_POINT ( 'NONE', #36338 ) ;
#1561 = CARTESIAN_POINT ( 'NONE',  ( -37.00000000000000711, 11.26103545359856106, -3.340853584269573684 ) ) ;
#1562 = ORIENTED_EDGE ( 'NONE', *, *, #47404, .F. ) ;
#1563 = APPLICATION_PROTOCOL_DEFINITION ( 'draft international standard', 'automotive_design', 1998, #13670 ) ;
#1564 = CARTESIAN_POINT ( 'NONE',  ( 0.000000000000000000, 6.470132594555819239, 2.133363481234098469 ) ) ;
#1565 = CARTESIAN_POINT ( 'NONE',  ( 2.665405856346785285, 1.089747929268691351, 9.505137710817288976 ) ) ;
#1566 = AXIS2_PLACEMENT_3D ( 'NONE', #49824, #8597, #40146 ) ;
#1567 = CARTESIAN_POINT ( 'NONE',  ( 35.00000000000000000, -10.70999494708488520, 5.814360711498399503 ) ) ;
#1568 = ORIENTED_EDGE ( 'NONE', *, *, #10098, .T. ) ;
#1569 =( BOUNDED_SURFACE ( )  B_SPLINE_SURFACE ( 3, 1, ( 
 ( #43414, #12496 ),
 ( #32770, #33121 ),
 ( #28148, #53752 ),
 ( #47453, #27812 ) ),
 .UNSPECIFIED., .F., .F., .F. ) 
 B_SPLINE_SURFACE_WITH_KNOTS ( ( 4, 4 ),
 ( 2, 2 ),
 ( 0.000000000000000000, 1.000000000000000000 ),
 ( 0.000000000000000000, 1.000000000000000000 ),
 .UNSPECIFIED. ) 
 GEOMETRIC_REPRESENTATION_ITEM ( )  RATIONAL_B_SPLINE_SURFACE ( (
 ( 1.000000000000000000, 1.000000000000000000),
 ( 0.6933888150995267674, 0.9895912004443193632),
 ( 0.6933888150995267674, 0.9895912004443193632),
 ( 1.000000000000000000, 1.000000000000000000) ) ) 
 REPRESENTATION_ITEM ( '' )  SURFACE ( )  );
#1570 = CARTESIAN_POINT ( 'NONE',  ( 2.000000000000001776, 0.000000000000000000, 0.000000000000000000 ) ) ;
#1571 = CARTESIAN_POINT ( 'NONE',  ( -37.00000000000000711, 0.000000000000000000, 0.000000000000000000 ) ) ;
#1572 = ORIENTED_EDGE ( 'NONE', *, *, #64314, .T. ) ;
#1573 = ORIENTED_EDGE ( 'NONE', *, *, #28751, .T. ) ;
#1574 = CARTESIAN_POINT ( 'NONE',  ( 2.430348790457260488, 7.544199152379035489, -1.528169972228324625 ) ) ;
#1575 = AXIS2_PLACEMENT_3D ( 'NONE', #57977, #37341, #41999 ) ;
#1576 = ORIENTED_EDGE ( 'NONE', *, *, #65162, .F. ) ;
#1577 = CARTESIAN_POINT ( 'NONE',  ( 2.241528039335008327, 1.341200777944249634, -7.515727438419993689 ) ) ;
#1578 = CARTESIAN_POINT ( 'NONE',  ( 5.515188684475870851, -0.005140903460551598213, -0.001485678338381495175 ) ) ;
#1579 = DIRECTION ( 'NONE',  ( 0.000000000000000000, 0.5243256840888563808, 0.8515178078024868702 ) ) ;
#1580 = CARTESIAN_POINT ( 'NONE',  ( 1.283627346226319244, 12.47820286973601966, 1.641214790178025629 ) ) ;
#1581 = CARTESIAN_POINT ( 'NONE',  ( -35.00000000000000000, 8.854740511458851770, 7.717887834988275131 ) ) ;
#1582 = CARTESIAN_POINT ( 'NONE',  ( 37.00000000000000711, -0.3025107581130382917, 11.74226168163341022 ) ) ;
#1583 = CARTESIAN_POINT ( 'NONE',  ( 2.245754705088396808, 7.499730934370272273, 1.435454129948234625 ) ) ;
#1584 = ADVANCED_FACE ( 'NONE', ( #50355 ), #16049, .T. ) ;
#1585 = VERTEX_POINT ( 'NONE', #30683 ) ;
#1586 = CARTESIAN_POINT ( 'NONE',  ( 0.8320506296491603226, 12.42924193558400070, -0.3827056590417270421 ) ) ;
#1587 = VERTEX_POINT ( 'NONE', #41315 ) ;
#1588 = CARTESIAN_POINT ( 'NONE',  ( 145.1370849898475797, 3.309064568108273190E-14, 0.000000000000000000 ) ) ;
#1589 = CARTESIAN_POINT ( 'NONE',  ( -9.027317351555117497, -12.84017734719011727, -4.182396712693398300 ) ) ;
#1590 = AXIS2_PLACEMENT_3D ( 'NONE', #52840, #62468, #52200 ) ;
#1591 = CARTESIAN_POINT ( 'NONE',  ( -7.181456785175555524, 5.890186129966279438, -10.45493698471458188 ) ) ;
#1592 = CARTESIAN_POINT ( 'NONE',  ( 2.255723233588951437, -3.933511348457480405, 6.548644987607549872 ) ) ;
#1593 = CARTESIAN_POINT ( 'NONE',  ( 0.2739690278137277835, -10.69833303470760377, -5.965352196073705926 ) ) ;
#1594 = CARTESIAN_POINT ( 'NONE',  ( 0.2648978790185584908, -11.46165506714225479, -4.312320170909353045 ) ) ;
#1595 = VECTOR ( 'NONE', #34066, 1000.000000000000000 ) ;
#1596 = ORIENTED_EDGE ( 'NONE', *, *, #24861, .F. ) ;
#1597 = VERTEX_POINT ( 'NONE', #55314 ) ;
#1598 = ADVANCED_FACE ( 'NONE', ( #60629 ), #60302, .T. ) ;
#1599 = CARTESIAN_POINT ( 'NONE',  ( 5.514624014163232779, -0.003498325728817977369, -0.002216125254993196909 ) ) ;
#1600 = ORIENTED_EDGE ( 'NONE', *, *, #54426, .F. ) ;
#1601 = CYLINDRICAL_SURFACE ( 'NONE', #4382, 4.999999999999999112 ) ;
#1602 = CARTESIAN_POINT ( 'NONE',  ( -15.22041587299536580, 7.970357817492780939, -10.89607067939092921 ) ) ;
#1603 = CARTESIAN_POINT ( 'NONE',  ( 35.00000000000000000, -8.295159312811920316, -8.927548052240867449 ) ) ;
#1604 = CARTESIAN_POINT ( 'NONE',  ( 0.2651627682582914924, -0.08809604936497586469, -12.24583720278847565 ) ) ;
#1605 = EDGE_CURVE ( 'NONE', #5918, #64188, #25380, .T. ) ;
#1606 = ORIENTED_EDGE ( 'NONE', *, *, #38771, .T. ) ;
#1607 = CARTESIAN_POINT ( 'NONE',  ( 3.100650473569745547, 2.280184661131199775, 7.585586315875747943 ) ) ;
#1608 = CYLINDRICAL_SURFACE ( 'NONE', #8785, 4.999999999999999112 ) ;
#1609 = CARTESIAN_POINT ( 'NONE',  ( 1.194176325881340039, -1.672143286119645245, 12.44396189284383958 ) ) ;
#1610 = CARTESIAN_POINT ( 'NONE',  ( -49.33927601438018939, -0.1339636383559742183, 5.724480317196145585 ) ) ;
#1611 = CIRCLE ( 'NONE', #16463, 12.74999999999999822 ) ;
#1612 = CARTESIAN_POINT ( 'NONE',  ( -19.69476066079020171, -4.201994156881551312, 12.82938989607585789 ) ) ;
#1613 = DIRECTION ( 'NONE',  ( 0.000000000000000000, 0.4935949184179201366, -0.8696919319575218132 ) ) ;
#1614 = VERTEX_POINT ( 'NONE', #41003 ) ;
#1615 = DIRECTION ( 'NONE',  ( 0.000000000000000000, 0.01356324068817998940, -0.9999080150203990547 ) ) ;
#1616 = EDGE_LOOP ( 'NONE', ( #3027, #44782, #54567, #22064 ) ) ;
#1617 = LINE ( 'NONE', #46492, #47192 ) ;
#1618 = DIRECTION ( 'NONE',  ( -1.000000000000000000, -0.000000000000000000, 0.000000000000000000 ) ) ;
#1619 = CARTESIAN_POINT ( 'NONE',  ( 2.903928887688454363, -8.528865300112075332, 2.041797854847293703 ) ) ;
#1620 = CARTESIAN_POINT ( 'NONE',  ( -35.04643116707788408, 0.01156612771643569793, 0.003844232202706091006 ) ) ;
#1621 = CARTESIAN_POINT ( 'NONE',  ( -10.41597200609069596, -5.095536857955488941, 10.87159232434287048 ) ) ;
#1622 = ORIENTED_EDGE ( 'NONE', *, *, #18904, .T. ) ;
#1623 = VERTEX_POINT ( 'NONE', #20397 ) ;
#1624 = CARTESIAN_POINT ( 'NONE',  ( 1.937114397841935398, -12.80345148322679982, 0.9020203649531247647 ) ) ;
#1625 = VERTEX_POINT ( 'NONE', #11083 ) ;
#1626 = FACE_OUTER_BOUND ( 'NONE', #59385, .T. ) ;
#1628 = AXIS2_PLACEMENT_3D ( 'NONE', #62830, #62492, #53855 ) ;
#1627 = CARTESIAN_POINT ( 'NONE',  ( 3.221585903514446514, 4.631497350863631901, -12.68724791558186737 ) ) ;
#1629 = CARTESIAN_POINT ( 'NONE',  ( 35.00000000000000000, 0.4871980014161481631, -12.74068829017554272 ) ) ;
#1630 = DIRECTION ( 'NONE',  ( 0.000000000000000000, 0.000000000000000000, -1.000000000000000000 ) ) ;
#1631 = CARTESIAN_POINT ( 'NONE',  ( 0.7446945582524635565, -7.698291984229281404, -9.728576129010285456 ) ) ;
#1632 = FACE_OUTER_BOUND ( 'NONE', #13235, .T. ) ;
#1633 = CARTESIAN_POINT ( 'NONE',  ( 0.4626703367451678317, 12.17089897506954799, -1.858541096400990078 ) ) ;
#1634 = ORIENTED_EDGE ( 'NONE', *, *, #57808, .T. ) ;
#1635 = EDGE_CURVE ( 'NONE', #18994, #21897, #55971, .T. ) ;
#1636 = CARTESIAN_POINT ( 'NONE',  ( -27.35552965826137140, 1.320216934008397569, 2.810569013793730697 ) ) ;
#1637 = EDGE_LOOP ( 'NONE', ( #29744, #46586, #63482, #8654 ) ) ;
#1638 = B_SPLINE_CURVE_WITH_KNOTS ( 'NONE', 3,
 ( #48811, #3262, #32499, #43138, #63417, #43461, #17887, #7925, #63741, #23535, #43809, #64089, #13532, #33812, #54111, #49149, #24840, #19532, #4896, #8888, #39459, #35111 ),
 .UNSPECIFIED., .F., .F.,
 ( 4, 3, 3, 3, 3, 3, 3, 4 ),
 ( 5.421010862427522170E-20, 4.449119708437005534E-05, 6.626296329540603137E-05, 8.803456484962761982E-05, 0.0001098060367612829541, 0.0001315774408628521560, 0.0001760698110411172115, 0.0001829697163287832666 ),
 .UNSPECIFIED. ) ;
#1639 = CARTESIAN_POINT ( 'NONE',  ( 35.00000000000000000, 4.705694406421931860E-17, -3.469127814946512892E-15 ) ) ;
#1641 = CYLINDRICAL_SURFACE ( 'NONE', #30194, 12.18649999999999878 ) ;
#1640 = AXIS2_PLACEMENT_3D ( 'NONE', #55925, #40284, #5392 ) ;
#1642 = EDGE_CURVE ( 'NONE', #14018, #19254, #4803, .T. ) ;
#1643 = CARTESIAN_POINT ( 'NONE',  ( 5.516018279890452902, 0.005752102158674347356, 0.003580555109620895717 ) ) ;
#1644 = DIRECTION ( 'NONE',  ( 0.000000000000000000, 0.3193015301359806712, -0.9476531711828022342 ) ) ;
#1645 = ORIENTED_EDGE ( 'NONE', *, *, #22512, .F. ) ;
#1646 = CARTESIAN_POINT ( 'NONE',  ( 35.00000000000000000, -12.16632754454236043, 0.7008968033240018380 ) ) ;
#1647 = CARTESIAN_POINT ( 'NONE',  ( -35.00000000000000000, -3.473736367725171359, -12.26766708251995475 ) ) ;
#1648 = CARTESIAN_POINT ( 'NONE',  ( 35.00000000000000000, 6.946017217730082294, 10.01317267707878500 ) ) ;
#1649 = ORIENTED_EDGE ( 'NONE', *, *, #26145, .F. ) ;
#1650 = VERTEX_POINT ( 'NONE', #65597 ) ;
#1651 = CARTESIAN_POINT ( 'NONE',  ( 2.676981048097610394, 3.126245636041473652, 13.13819726198281401 ) ) ;
#1652 = ORIENTED_EDGE ( 'NONE', *, *, #36627, .F. ) ;
#1653 = ORIENTED_EDGE ( 'NONE', *, *, #51338, .T. ) ;
#1654 = ORIENTED_EDGE ( 'NONE', *, *, #24018, .F. ) ;
#1655 = B_SPLINE_CURVE_WITH_KNOTS ( 'NONE', 3,
 ( #51192, #41178, #5645, #4979, #20251, #35546, #10270, #41505, #647, #10592, #60484, #61460, #20904, #36186, #65464, #40532 ),
 .UNSPECIFIED., .F., .F.,
 ( 4, 3, 3, 3, 3, 4 ),
 ( 0.000000000000000000, 0.0002176109881720252981, 0.0004352086762394648950, 0.0006528017811446961815, 0.0007615147961451798663, 0.0009453342004946652891 ),
 .UNSPECIFIED. ) ;
#1656 = ORIENTED_EDGE ( 'NONE', *, *, #24245, .F. ) ;
#1657 = FACE_OUTER_BOUND ( 'NONE', #27220, .T. ) ;
#1658 = DIRECTION ( 'NONE',  ( 0.000000000000000000, -0.2149704402110115264, -0.9766205557100894330 ) ) ;
#1659 = CIRCLE ( 'NONE', #59005, 12.74999999999999822 ) ;
#1660 = ADVANCED_FACE ( 'NONE', ( #46334 ), #20072, .T. ) ;
#1661 = DIRECTION ( 'NONE',  ( 0.000000000000000000, -0.01356324068817991828, 0.9999080150203990547 ) ) ;
#1662 = CARTESIAN_POINT ( 'NONE',  ( -27.28563798457900091, 1.483130241384917891, -2.487904455214884347 ) ) ;
#1663 = DIRECTION ( 'NONE',  ( 1.000000000000000000, 0.000000000000000000, 0.000000000000000000 ) ) ;
#1664 = EDGE_LOOP ( 'NONE', ( #38738, #24437, #29499, #200 ) ) ;
#1665 = CARTESIAN_POINT ( 'NONE',  ( -22.71097035706202405, -4.089776368546547580, -2.846599994298351977 ) ) ;
#1666 = EDGE_CURVE ( 'NONE', #31754, #32570, #1716, .T. ) ;
#1667 = ORIENTED_EDGE ( 'NONE', *, *, #21231, .F. ) ;
#1668 = LINE ( 'NONE', #56531, #27445 ) ;
#1669 = B_SPLINE_CURVE_WITH_KNOTS ( 'NONE', 3,
 ( #31136, #6861, #61708, #872, #27441, #2186, #26800, #51446, #5894, #37091, #10848, #26155, #51760, #12155, #22465, #46752, #21144, #16814 ),
 .UNSPECIFIED., .F., .F.,
 ( 4, 2, 2, 2, 2, 2, 2, 2, 4 ),
 ( 3.127317220692751144E-18, 0.001286103680247937435, 0.002572207360495871835, 0.003858311040743806018, 0.004501362880867774627, 0.005144414720991742802, 0.006430518401239680021, 0.007716622081487616372, 0.01028882944198348734 ),
 .UNSPECIFIED. ) ;
#1670 = DIRECTION ( 'NONE',  ( 0.000000000000000000, 0.01356324068817998940, -0.9999080150203990547 ) ) ;
#1671 = EDGE_CURVE ( 'NONE', #3168, #52651, #38877, .T. ) ;
#1672 = DIRECTION ( 'NONE',  ( 1.000000000000000000, -0.000000000000000000, -0.000000000000000000 ) ) ;
#1673 = CARTESIAN_POINT ( 'NONE',  ( 0.2915757698887273541, -8.040595355212891704, -9.248369946372616113 ) ) ;
#1674 = DIRECTION ( 'NONE',  ( 1.000000000000000000, -0.000000000000000000, 0.000000000000000000 ) ) ;
#1675 = DIRECTION ( 'NONE',  ( -1.000000000000000000, -1.836970198721029688E-16, -0.000000000000000000 ) ) ;
#1676 = ORIENTED_EDGE ( 'NONE', *, *, #56782, .T. ) ;
#1677 = ADVANCED_FACE ( 'NONE', ( #17384 ), #47633, .T. ) ;
#1678 = DIRECTION ( 'NONE',  ( -1.000000000000000000, 0.000000000000000000, 0.000000000000000000 ) ) ;
#1679 = CIRCLE ( 'NONE', #36735, 2.899999999999994582 ) ;
#1680 = ORIENTED_EDGE ( 'NONE', *, *, #29933, .T. ) ;
#1681 = EDGE_CURVE ( 'NONE', #29318, #36377, #56899, .T. ) ;
#1682 = DIRECTION ( 'NONE',  ( -1.000000000000000000, 0.000000000000000000, 0.000000000000000000 ) ) ;
#1683 = CARTESIAN_POINT ( 'NONE',  ( -0.4967434119545894866, -25.72578597719286364, -15.66300405139958407 ) ) ;
#1684 = CARTESIAN_POINT ( 'NONE',  ( 2.990245332647883725, 8.130497889782956733, -2.413832934171042055 ) ) ;
#1685 = CARTESIAN_POINT ( 'NONE',  ( -27.08702828306175903, -0.6138566972905382668, -2.216258174335471232 ) ) ;
#1686 = CARTESIAN_POINT ( 'NONE',  ( 2.251139882113957658, -6.675617500148627315, 3.710800524304805226 ) ) ;
#1687 = EDGE_LOOP ( 'NONE', ( #43716, #4623, #55256, #11570 ) ) ;
#1688 = CYLINDRICAL_SURFACE ( 'NONE', #32395, 12.18650000000000055 ) ;
#1689 = CARTESIAN_POINT ( 'NONE',  ( -22.71097035706202760, 2.846599994298365743, -4.089776368546553798 ) ) ;
#1690 = DIRECTION ( 'NONE',  ( -1.000000000000000000, 0.000000000000000000, -0.000000000000000000 ) ) ;
#1691 = CARTESIAN_POINT ( 'NONE',  ( 0.2648978790185610999, -2.256510822326061483, -12.03635331166814382 ) ) ;
#1692 = AXIS2_PLACEMENT_3D ( 'NONE', #2032, #7331, #31944 ) ;
#1693 = ADVANCED_FACE ( 'NONE', ( #32327 ), #21378, .T. ) ;
#1694 = CARTESIAN_POINT ( 'NONE',  ( 0.2647959493198550618, 12.24513905663510549, -0.1469673141001992533 ) ) ;
#1695 = ORIENTED_EDGE ( 'NONE', *, *, #38371, .T. ) ;
#1696 = CARTESIAN_POINT ( 'NONE',  ( 2.368238019615076961, -0.1797502808084734671, -7.674602282635998307 ) ) ;
#1697 = DIRECTION ( 'NONE',  ( 0.000000000000000000, 0.01356324068817992522, -0.9999080150203990547 ) ) ;
#1698 = AXIS2_PLACEMENT_3D ( 'NONE', #20873, #11872, #61116 ) ;
#1699 = ORIENTED_EDGE ( 'NONE', *, *, #52657, .F. ) ;
#1700 = ORIENTED_EDGE ( 'NONE', *, *, #12834, .F. ) ;
#1701 = CARTESIAN_POINT ( 'NONE',  ( 0.2638984909335716500, -2.322601104020747265, 12.02508546958696201 ) ) ;
#1702 = CARTESIAN_POINT ( 'NONE',  ( 48.61333473403966821, -0.2789806315675412152, 4.308813575818149388 ) ) ;
#1703 = DIRECTION ( 'NONE',  ( 0.000000000000000000, 0.01356324068817998940, -0.9999080150203990547 ) ) ;
#1704 = CARTESIAN_POINT ( 'NONE',  ( 0.3654063281920745809, -1.872466061177166408, 12.13594617907221540 ) ) ;
#1705 = ORIENTED_EDGE ( 'NONE', *, *, #15911, .F. ) ;
#1706 = ORIENTED_EDGE ( 'NONE', *, *, #28656, .F. ) ;
#1707 = ORIENTED_EDGE ( 'NONE', *, *, #343, .F. ) ;
#1708 = FACE_OUTER_BOUND ( 'NONE', #2461, .T. ) ;
#1709 = ADVANCED_FACE ( 'NONE', ( #31357 ), #52315, .T. ) ;
#1710 = FACE_OUTER_BOUND ( 'NONE', #53273, .T. ) ;
#1711 = ORIENTED_EDGE ( 'NONE', *, *, #56369, .F. ) ;
#1712 = AXIS2_PLACEMENT_3D ( 'NONE', #44240, #23311, #59541 ) ;
#1713 = DIRECTION ( 'NONE',  ( -0.000000000000000000, -1.000000000000000000, -0.000000000000000000 ) ) ;
#1714 = FACE_OUTER_BOUND ( 'NONE', #2932, .T. ) ;
#1715 = ORIENTED_EDGE ( 'NONE', *, *, #65265, .F. ) ;
#1716 = CIRCLE ( 'NONE', #7019, 12.73084802173761787 ) ;
#1717 = CARTESIAN_POINT ( 'NONE',  ( 0.2648978790185619880, 11.46165506714233828, -4.312320170909121231 ) ) ;
#1718 = CARTESIAN_POINT ( 'NONE',  ( 9.992127424267872371, -32.24574823824523406, -12.88148438038769150 ) ) ;
#1719 = CARTESIAN_POINT ( 'NONE',  ( 2.276198483118644145, 7.130755363255238066, 2.759333101208258476 ) ) ;
#1720 = ORIENTED_EDGE ( 'NONE', *, *, #27553, .T. ) ;
#1721 = CARTESIAN_POINT ( 'NONE',  ( 0.2676618633000472092, 12.08777609394272368, -1.968216791520369657 ) ) ;
#1722 = ORIENTED_EDGE ( 'NONE', *, *, #16385, .T. ) ;
#1723 = CARTESIAN_POINT ( 'NONE',  ( 12.19644689801851811, 0.02881586504203031279, -13.50000000000000000 ) ) ;
#1724 = CARTESIAN_POINT ( 'NONE',  ( -18.06844711592810526, -5.734463224907465850, 12.22455983143679781 ) ) ;
#1725 = CARTESIAN_POINT ( 'NONE',  ( 16.21117406328131594, -35.00000000000000000, -4.142385751841773711 ) ) ;
#1726 = CARTESIAN_POINT ( 'NONE',  ( 36.00000000000000711, 11.01837265713073144, -6.415447294506746445 ) ) ;
#1727 = DIRECTION ( 'NONE',  ( -1.000000000000000000, -1.836970198721029688E-16, 0.000000000000000000 ) ) ;
#1728 = EDGE_CURVE ( 'NONE', #28136, #25112, #677, .T. ) ;
#1729 = DIRECTION ( 'NONE',  ( -1.000000000000000000, -0.000000000000000000, -0.000000000000000000 ) ) ;
#1730 = FACE_OUTER_BOUND ( 'NONE', #16630, .T. ) ;
#1731 = CARTESIAN_POINT ( 'NONE',  ( 0.2650492433740070375, 4.291726136518546397, 11.46945725111968706 ) ) ;
#1732 = ORIENTED_EDGE ( 'NONE', *, *, #54686, .T. ) ;
#1733 = CARTESIAN_POINT ( 'NONE',  ( 0.000000000000000000, -5.217815162096861137, 5.387430271863535403 ) ) ;
#1734 = ORIENTED_EDGE ( 'NONE', *, *, #29161, .F. ) ;
#1735 = CARTESIAN_POINT ( 'NONE',  ( -47.00000000000000711, 0.000000000000000000, 0.000000000000000000 ) ) ;
#1736 = EDGE_CURVE ( 'NONE', #3747, #26969, #6009, .T. ) ;
#1737 = DIRECTION ( 'NONE',  ( 0.000000000000000000, -0.01356324068817998940, 0.9999080150203990547 ) ) ;
#1738 = EDGE_CURVE ( 'NONE', #35815, #16693, #51652, .T. ) ;
#1739 = ORIENTED_EDGE ( 'NONE', *, *, #46333, .F. ) ;
#1740 = DIRECTION ( 'NONE',  ( 0.000000000000000000, -0.01356324068818000848, 0.9999080150203990547 ) ) ;
#1741 = CARTESIAN_POINT ( 'NONE',  ( 0.2647959493198567271, 6.249846955854266639, 10.53111783886892994 ) ) ;
#1742 = DIRECTION ( 'NONE',  ( -1.000000000000000000, 0.000000000000000000, 0.000000000000000000 ) ) ;
#1743 = EDGE_LOOP ( 'NONE', ( #40308, #678, #33809, #1774 ) ) ;
#1744 = ORIENTED_EDGE ( 'NONE', *, *, #5, .T. ) ;
#1745 = EDGE_CURVE ( 'NONE', #21179, #58982, #25187, .T. ) ;
#1746 = FACE_OUTER_BOUND ( 'NONE', #56468, .T. ) ;
#1747 = ORIENTED_EDGE ( 'NONE', *, *, #45104, .F. ) ;
#1748 = EDGE_CURVE ( 'NONE', #34943, #52755, #41980, .T. ) ;
#1749 = DIRECTION ( 'NONE',  ( -1.000000000000000000, -1.836970198721029688E-16, 0.000000000000000000 ) ) ;
#1750 = DIRECTION ( 'NONE',  ( 0.000000000000000000, 0.000000000000000000, -1.000000000000000000 ) ) ;
#1751 = B_SPLINE_CURVE_WITH_KNOTS ( 'NONE', 3,
 ( #23981, #53906, #2734, #8675, #52911, #43248, #23312, #44241, #3382, #58579, #3721, #23652, #33288, #43575, #58921, #33618 ),
 .UNSPECIFIED., .F., .F.,
 ( 4, 3, 3, 3, 3, 4 ),
 ( 9.757819552369539906E-19, 0.0003017745587525238376, 0.0006035491769808721142, 0.0009053241094668146218, 0.001207275924541910319, 0.001510325902536801233 ),
 .UNSPECIFIED. ) ;
#1752 = CARTESIAN_POINT ( 'NONE',  ( -3.167879205347148286, -12.42824319244124531, 5.282660448253479579 ) ) ;
#1753 = CYLINDRICAL_SURFACE ( 'NONE', #48787, 5.000000000000000888 ) ;
#1754 = CARTESIAN_POINT ( 'NONE',  ( 0.000000000000000000, 0.000000000000000000, 0.000000000000000000 ) ) ;
#1755 = EDGE_CURVE ( 'NONE', #35942, #13458, #26717, .T. ) ;
#1756 = EDGE_LOOP ( 'NONE', ( #52914, #46976, #29109, #49555 ) ) ;
#1757 = B_SPLINE_CURVE_WITH_KNOTS ( 'NONE', 3,
 ( #44467, #64747, #17915, #23229, #28868, #48842, #59148, #63769, #64429, #13259, #13560, #53512, #14220, #7956, #33843, #28223, #3289, #38177, #58489 ),
 .UNSPECIFIED., .F., .F.,
 ( 4, 3, 3, 3, 3, 3, 4 ),
 ( 0.000000000000000000, 2.832085443685227149E-05, 4.217789847592207954E-05, 5.603488375296408508E-05, 6.989180858882511338E-05, 9.821094830335176152E-05, 0.0001178165571463577204 ),
 .UNSPECIFIED. ) ;
#1758 = CARTESIAN_POINT ( 'NONE',  ( 0.2706063244538056134, -12.03021891034989466, -2.299194104693211393 ) ) ;
#1759 = EDGE_CURVE ( 'NONE', #13124, #60470, #2769, .T. ) ;
#1760 = B_SPLINE_CURVE_WITH_KNOTS ( 'NONE', 3,
 ( #23699, #59589, #48325, #23035, #48636, #3091, #19025, #19359, #43968, #58959, #63909, #49314, #43290, #24326, #39624, #53633, #32983, #13370, #18042, #49617, #53947, #8388 ),
 .UNSPECIFIED., .F., .F.,
 ( 4, 3, 3, 3, 3, 3, 3, 4 ),
 ( 2.201357640472097428E-18, 4.449119708436821897E-05, 6.626296329540375455E-05, 8.803456484962473314E-05, 0.0001098060367612801081, 0.0001315774408628522915, 0.0001760698110411177265, 0.0001829697163287813150 ),
 .UNSPECIFIED. ) ;
#1761 = EDGE_CURVE ( 'NONE', #38782, #40551, #43282, .T. ) ;
#1762 = CARTESIAN_POINT ( 'NONE',  ( -22.70624764888619751, -1.907540768355087124, -4.891815784104558418 ) ) ;
#1763 =( BOUNDED_CURVE ( )  B_SPLINE_CURVE ( 3, ( #62574, #31355, #37317, #22346 ),
 .UNSPECIFIED., .F., .F. ) 
 B_SPLINE_CURVE_WITH_KNOTS ( ( 4, 4 ),
 ( 1.881236687097070925, 1.898360998982701053 ),
 .UNSPECIFIED. ) 
 CURVE ( )  GEOMETRIC_REPRESENTATION_ITEM ( )  RATIONAL_B_SPLINE_CURVE ( ( 1.000000000000000000, 0.9999755633111596653, 0.9999755633111596653, 1.000000000000000000 ) ) 
 REPRESENTATION_ITEM ( '' )  );
#1764 = DIRECTION ( 'NONE',  ( 0.000000000000000000, -0.8989688749565204473, -0.4380125133593880671 ) ) ;
#1765 = ADVANCED_FACE ( 'NONE', ( #32972 ), #59258, .T. ) ;
#1766 = CARTESIAN_POINT ( 'NONE',  ( 2.000000000000001776, 5.457833520448658327, 4.281014542496528463 ) ) ;
#1767 = CARTESIAN_POINT ( 'NONE',  ( 0.3160775863651090756, -5.922381034681523104, -10.73821170199162545 ) ) ;
#1768 = CARTESIAN_POINT ( 'NONE',  ( 5.514624014163232779, -0.0005510299962886537617, -0.004104370840204212174 ) ) ;
#1769 = DIRECTION ( 'NONE',  ( 0.000000000000000000, -0.01356324068817998940, 0.9999080150203990547 ) ) ;
#1770 = DIRECTION ( 'NONE',  ( 1.000000000000000000, -0.000000000000000000, -0.000000000000000000 ) ) ;
#1771 = ORIENTED_EDGE ( 'NONE', *, *, #21808, .T. ) ;
#1772 = CARTESIAN_POINT ( 'NONE',  ( 2.889800649504073782, -2.030191121417098898, -5.774917447013018901 ) ) ;
#1773 = DIRECTION ( 'NONE',  ( 0.000000000000000000, 0.5155538571770230671, -0.8568571761675883858 ) ) ;
#1774 = ORIENTED_EDGE ( 'NONE', *, *, #61825, .T. ) ;
#1775 = DIRECTION ( 'NONE',  ( 1.000000000000000000, 0.000000000000000000, 0.000000000000000000 ) ) ;
#1776 = CARTESIAN_POINT ( 'NONE',  ( 3.152665057736204535, -4.377619405894248139, -6.622010822085805160 ) ) ;
#1777 = ORIENTED_EDGE ( 'NONE', *, *, #54236, .F. ) ;
#1778 = CARTESIAN_POINT ( 'NONE',  ( -35.04834644901396956, -0.01046409687784406219, -0.009049049589502401736 ) ) ;
#1779 = ORIENTED_EDGE ( 'NONE', *, *, #28548, .F. ) ;
#1780 = CARTESIAN_POINT ( 'NONE',  ( 0.3474126878361822324, -5.911350916722116544, 10.75620725594714422 ) ) ;
#1781 = ORIENTED_EDGE ( 'NONE', *, *, #64674, .F. ) ;
#1782 = ORIENTED_EDGE ( 'NONE', *, *, #35275, .F. ) ;
#1784 = ADVANCED_FACE ( 'NONE', ( #7730 ), #18376, .T. ) ;
#1783 = DIRECTION ( 'NONE',  ( 0.000000000000000000, -0.6269146997508042718, -0.7790879021242460567 ) ) ;
#1785 = ORIENTED_EDGE ( 'NONE', *, *, #13728, .F. ) ;
#1786 = DIRECTION ( 'NONE',  ( 0.000000000000000000, 0.01356324068817992522, -0.9999080150203990547 ) ) ;
#1787 = CARTESIAN_POINT ( 'NONE',  ( 1.634816307077031849, -11.67158647524064108, -5.013416918609148176 ) ) ;
#1788 = DIRECTION ( 'NONE',  ( -0.9688695217174486674, 0.000000000000000000, -0.2475719085175094036 ) ) ;
#1789 = DIRECTION ( 'NONE',  ( -1.000000000000000000, 0.000000000000000000, 0.000000000000000000 ) ) ;
#1790 = EDGE_LOOP ( 'NONE', ( #47577, #39844, #6297, #333 ) ) ;
#1791 = CARTESIAN_POINT ( 'NONE',  ( 0.3610902822527190525, -7.689482111308914014, 9.572034936626860002 ) ) ;
#1792 = CARTESIAN_POINT ( 'NONE',  ( 5.926183177043330197, -31.73296902231061978, 13.63811545878544607 ) ) ;
#1793 = CARTESIAN_POINT ( 'NONE',  ( 5.530133899448235191, -0.01437126147332077469, -0.006998616117864021532 ) ) ;
#1795 = VERTEX_POINT ( 'NONE', #64870 ) ;
#1794 = CARTESIAN_POINT ( 'NONE',  ( -25.77840011361687189, 10.55150440484683294, 5.716830058840185025 ) ) ;
#1796 = CARTESIAN_POINT ( 'NONE',  ( -27.86543437857248762, 9.320859823866943117, -7.583027560034842018 ) ) ;
#1797 = ORIENTED_EDGE ( 'NONE', *, *, #8646, .F. ) ;
#1798 = DIRECTION ( 'NONE',  ( 0.000000000000000000, -0.8009703041134103030, -0.5987040770935764256 ) ) ;
#1799 = EDGE_CURVE ( 'NONE', #65150, #23145, #39949, .T. ) ;
#1800 = VERTEX_POINT ( 'NONE', #38642 ) ;
#1801 = CIRCLE ( 'NONE', #44264, 12.75000000000000178 ) ;
#1802 = DIRECTION ( 'NONE',  ( 0.000000000000000000, 0.000000000000000000, 1.000000000000000000 ) ) ;
#1803 = CARTESIAN_POINT ( 'NONE',  ( 0.000000000000000000, 5.107597897712347290, 4.693343793638412365 ) ) ;
#1804 = CARTESIAN_POINT ( 'NONE',  ( 1.719304012338831678, -5.066286238785654206, 11.67935079956403044 ) ) ;
#1805 = ORIENTED_EDGE ( 'NONE', *, *, #54412, .T. ) ;
#1806 = FACE_BOUND ( 'NONE', #38250, .T. ) ;
#1807 = EDGE_CURVE ( 'NONE', #32874, #52513, #58953, .T. ) ;
#1808 = VECTOR ( 'NONE', #48269, 1000.000000000000000 ) ;
#1809 = DIRECTION ( 'NONE',  ( 0.000000000000000000, 0.01356324068817992175, -0.9999080150203990547 ) ) ;
#1810 = DIRECTION ( 'NONE',  ( 0.000000000000000000, 1.000000000000000000, 0.000000000000000000 ) ) ;
#1811 = ORIENTED_EDGE ( 'NONE', *, *, #58271, .F. ) ;
#1812 = ORIENTED_EDGE ( 'NONE', *, *, #41245, .T. ) ;
#1813 = DIRECTION ( 'NONE',  ( 0.000000000000000000, 0.000000000000000000, -1.000000000000000000 ) ) ;
#1814 = VERTEX_POINT ( 'NONE', #13683 ) ;
#1815 = EDGE_CURVE ( 'NONE', #7231, #19321, #55904, .T. ) ;
#1816 = VERTEX_POINT ( 'NONE', #54275 ) ;
#1817 = LINE ( 'NONE', #12101, #62500 ) ;
#1818 = DIRECTION ( 'NONE',  ( 0.000000000000000000, -0.9551603052523447435, 0.2960891610144610886 ) ) ;
#1819 = FACE_OUTER_BOUND ( 'NONE', #27952, .T. ) ;
#1820 = DIRECTION ( 'NONE',  ( -1.000000000000000000, 0.000000000000000000, 0.000000000000000000 ) ) ;
#1821 = DIRECTION ( 'NONE',  ( -1.000000000000000000, 0.000000000000000000, 0.000000000000000000 ) ) ;
#1822 = LINE ( 'NONE', #48030, #35229 ) ;
#1823 = CARTESIAN_POINT ( 'NONE',  ( -22.27706485742869091, -0.9221835209182183135, -3.563814065926679042 ) ) ;
#1824 = ORIENTED_EDGE ( 'NONE', *, *, #38666, .F. ) ;
#1825 = DIRECTION ( 'NONE',  ( -1.000000000000000000, 0.000000000000000000, 0.000000000000000000 ) ) ;
#1826 = CARTESIAN_POINT ( 'NONE',  ( -37.00000000000000711, -11.39945968423475264, 5.710938531231672499 ) ) ;
#1827 = EDGE_CURVE ( 'NONE', #7333, #31040, #33603, .T. ) ;
#1828 = DIRECTION ( 'NONE',  ( 0.000000000000000000, 0.01356324068817998940, -0.9999080150203990547 ) ) ;
#1829 = CARTESIAN_POINT ( 'NONE',  ( -36.00000000000000711, 12.26766708251996363, -3.473736367725129615 ) ) ;
#1830 = CARTESIAN_POINT ( 'NONE',  ( 2.000000000000001776, 4.376687952327412034, -5.220963330856592144 ) ) ;
#1831 = EDGE_CURVE ( 'NONE', #15972, #44370, #64383, .T. ) ;
#1832 = VECTOR ( 'NONE', #59971, 1000.000000000000000 ) ;
#1833 = CYLINDRICAL_SURFACE ( 'NONE', #33063, 5.000000000000002665 ) ;
#1834 = ADVANCED_FACE ( 'NONE', ( #44583 ), #4050, .T. ) ;
#1835 = CARTESIAN_POINT ( 'NONE',  ( 11.92129028673735647, 0.08362343793122377356, -11.99997311782909115 ) ) ;
#1836 = ORIENTED_EDGE ( 'NONE', *, *, #35408, .T. ) ;
#1837 = CARTESIAN_POINT ( 'NONE',  ( -27.08419642509983305, 0.4837273216075048676, 2.239682169453929284 ) ) ;
#1838 = CARTESIAN_POINT ( 'NONE',  ( -35.00000000000000000, 0.000000000000000000, 0.000000000000000000 ) ) ;
#1839 = CARTESIAN_POINT ( 'NONE',  ( 2.368238019615420242, 1.155661230551846330, -7.589221137922761429 ) ) ;
#1840 = CARTESIAN_POINT ( 'NONE',  ( 2.000000000000001776, 1.145812388885126820, 6.715725538143592743 ) ) ;
#1841 = AXIS2_PLACEMENT_3D ( 'NONE', #48515, #54145, #34174 ) ;
#1842 = CARTESIAN_POINT ( 'NONE',  ( -24.81237754203414170, 8.088796810898713829, 8.871815844506174997 ) ) ;
#1843 = DIRECTION ( 'NONE',  ( 0.000000000000000000, -0.01356324068817991828, 0.9999080150203990547 ) ) ;
#1844 = ORIENTED_EDGE ( 'NONE', *, *, #16176, .F. ) ;
#1845 = CARTESIAN_POINT ( 'NONE',  ( 18.54132159498832166, -6.065857072570194575, 10.36437726158596639 ) ) ;
#1846 = CARTESIAN_POINT ( 'NONE',  ( 37.00000000000000711, 10.68873102412842258, -6.950793414699834472 ) ) ;
#1847 = CARTESIAN_POINT ( 'NONE',  ( 2.284126774967170093, -4.793997684221434241, -5.959830409747408630 ) ) ;
#1848 = CARTESIAN_POINT ( 'NONE',  ( 42.50000000000000000, -2.710505431213761085E-17, 1.201363017033314212E-18 ) ) ;
#1849 = ORIENTED_EDGE ( 'NONE', *, *, #57670, .T. ) ;
#1850 = CARTESIAN_POINT ( 'NONE',  ( 0.2739690278137246748, 2.307031017960451624, 12.02985305092651735 ) ) ;
#1851 = CARTESIAN_POINT ( 'NONE',  ( -25.54417658651491863, 7.498517398407837931, 11.22596262356930197 ) ) ;
#1853 = VERTEX_POINT ( 'NONE', #19017 ) ;
#1852 = DIRECTION ( 'NONE',  ( 0.000000000000000000, 0.01356324068817998940, -0.9999080150203989437 ) ) ;
#1854 = DIRECTION ( 'NONE',  ( 1.000000000000000000, -0.000000000000000000, -0.000000000000000000 ) ) ;
#1855 = EDGE_CURVE ( 'NONE', #51673, #20923, #59103, .T. ) ;
#1856 = DIRECTION ( 'NONE',  ( 0.000000000000000000, 0.000000000000000000, 1.000000000000000000 ) ) ;
#1857 = ORIENTED_EDGE ( 'NONE', *, *, #50684, .F. ) ;
#1858 = DIRECTION ( 'NONE',  ( 0.000000000000000000, 0.000000000000000000, -1.000000000000000000 ) ) ;
#1859 = EDGE_CURVE ( 'NONE', #22430, #41989, #61215, .T. ) ;
#1860 = CARTESIAN_POINT ( 'NONE',  ( 16.78263030916553689, 12.17295508002146320, 5.836879698929895888 ) ) ;
#1861 = CARTESIAN_POINT ( 'NONE',  ( 23.76574300270097595, 1.690451441203562055, -11.88488507406290218 ) ) ;
#1862 = CARTESIAN_POINT ( 'NONE',  ( 37.00000000000000711, -11.81949347079744506, 2.968224442958526943 ) ) ;
#1863 = CARTESIAN_POINT ( 'NONE',  ( 1.000000000000000888, 7.414200355365271555, -1.131208685655096691 ) ) ;
#1864 = CARTESIAN_POINT ( 'NONE',  ( 0.2956976708475462234, 5.936640677855365311, 10.72256944221088837 ) ) ;
#1866 = ORIENTED_EDGE ( 'NONE', *, *, #24512, .T. ) ;
#1865 = DIRECTION ( 'NONE',  ( 0.000000000000000000, 0.000000000000000000, 1.000000000000000000 ) ) ;
#1867 = CARTESIAN_POINT ( 'NONE',  ( -22.27722019094931483, 2.374181302999014420, 2.813874087059979878 ) ) ;
#1868 = ORIENTED_EDGE ( 'NONE', *, *, #60167, .F. ) ;
#1869 = CARTESIAN_POINT ( 'NONE',  ( 24.83517902727939841, -1.538878142198703225, -11.90257845377566248 ) ) ;
#1870 = ORIENTED_EDGE ( 'NONE', *, *, #60748, .F. ) ;
#1871 = EDGE_CURVE ( 'NONE', #25468, #16649, #27987, .T. ) ;
#1872 = DIRECTION ( 'NONE',  ( -1.000000000000000000, 0.000000000000000000, 0.000000000000000000 ) ) ;
#1873 = AXIS2_PLACEMENT_3D ( 'NONE', #18740, #13079, #53659 ) ;
#1874 = CARTESIAN_POINT ( 'NONE',  ( 0.3665391374699467075, -9.576575648339071378, 7.691255657244262522 ) ) ;
#1875 = CARTESIAN_POINT ( 'NONE',  ( -35.62380706382417372, -2.504225566391070856, 21.57767586339570443 ) ) ;
#1876 = CARTESIAN_POINT ( 'NONE',  ( 22.68139259647346861, 3.158742727684422213, 13.12595410559641529 ) ) ;
#1877 = ORIENTED_EDGE ( 'NONE', *, *, #58799, .T. ) ;
#1878 = AXIS2_PLACEMENT_3D ( 'NONE', #1248, #41449, #20858 ) ;
#1879 = CARTESIAN_POINT ( 'NONE',  ( 5.514624014163232779, -0.004104370840204217379, 0.0005510299962886126704 ) ) ;
#1880 = CARTESIAN_POINT ( 'NONE',  ( 2.305787727787083519, 5.756228004061526349, -5.047606869482997638 ) ) ;
#1881 = ORIENTED_EDGE ( 'NONE', *, *, #7064, .T. ) ;
#1882 = ORIENTED_EDGE ( 'NONE', *, *, #60352, .F. ) ;
#1883 = CARTESIAN_POINT ( 'NONE',  ( 2.247112776671467138, -7.214825360831402357, -2.501955819907554890 ) ) ;
#1884 = EDGE_CURVE ( 'NONE', #16592, #38075, #50271, .T. ) ;
#1885 = EDGE_LOOP ( 'NONE', ( #14299, #23165, #55326, #62263 ) ) ;
#1886 = CIRCLE ( 'NONE', #64523, 7.499999999999988454 ) ;
#1887 = CARTESIAN_POINT ( 'NONE',  ( 12.93723047338301058, 4.476360154859203355, 25.00000000000000000 ) ) ;
#1888 = DIRECTION ( 'NONE',  ( -1.000000000000000000, -0.000000000000000000, -0.000000000000000000 ) ) ;
#1889 = ADVANCED_FACE ( 'NONE', ( #10654 ), #14645, .T. ) ;
#1890 = CARTESIAN_POINT ( 'NONE',  ( 1.633930747250412319, 12.61425129500095643, 1.494486044210056708 ) ) ;
#1891 = LINE ( 'NONE', #13483, #39409 ) ;
#1892 = DIRECTION ( 'NONE',  ( 0.000000000000000000, 0.000000000000000000, 1.000000000000000000 ) ) ;
#1893 = AXIS2_PLACEMENT_3D ( 'NONE', #48503, #64107, #53151 ) ;
#1894 = B_SPLINE_CURVE_WITH_KNOTS ( 'NONE', 3,
 ( #256, #56088, #21170, #25179, #10527, #41440, #9884, #61399, #61731, #20531, #45453, #51124, #11206, #31483, #51780, #1237, #25851, #46142, #21516, #65719 ),
 .UNSPECIFIED., .F., .F.,
 ( 4, 2, 2, 2, 2, 2, 2, 2, 2, 4 ),
 ( 8.498374721940737388E-18, 0.001129263999270209906, 0.002258527998540411572, 0.003387791997810613454, 0.004517055997080814470, 0.005646319996351015919, 0.006210951995986116643, 0.006775583995621218235, 0.007904847994891418816, 0.009034111994161618531 ),
 .UNSPECIFIED. ) ;
#1895 = DIRECTION ( 'NONE',  ( -1.000000000000000000, 0.000000000000000000, 0.000000000000000000 ) ) ;
#1896 = VERTEX_POINT ( 'NONE', #31 ) ;
#1897 = FACE_OUTER_BOUND ( 'NONE', #12593, .T. ) ;
#1898 = ORIENTED_EDGE ( 'NONE', *, *, #59724, .T. ) ;
#1899 = CARTESIAN_POINT ( 'NONE',  ( 3.100650473569758869, 4.345221797103608452, -6.622643684997338909 ) ) ;
#1900 = DIRECTION ( 'NONE',  ( -0.000000000000000000, -0.000000000000000000, -1.000000000000000000 ) ) ;
#1901 = B_SPLINE_CURVE_WITH_KNOTS ( 'NONE', 3,
 ( #15994, #36282, #35629, #11028, #35937, #45955, #4754, #50619, #16350, #31309, #51611, #40624, #26315, #15010, #1052, #36621, #55, #56927, #11347, #60574, #30326, #35296 ),
 .UNSPECIFIED., .F., .F.,
 ( 4, 3, 3, 3, 3, 3, 3, 4 ),
 ( 0.000000000000000000, 4.447697177976342209E-05, 6.624143997791237092E-05, 8.800576886944197236E-05, 0.0001097699864780881258, 0.0001315341395364363788, 0.0001760120188223247427, 0.0001867971373174718945 ),
 .UNSPECIFIED. ) ;
#1902 = CARTESIAN_POINT ( 'NONE',  ( 2.969415267404317493, -3.055358878717488569, -7.260393470501798951 ) ) ;
#1903 = CARTESIAN_POINT ( 'NONE',  ( 0.2652384770603659625, -11.48486213386623511, -4.250454630553679891 ) ) ;
#1904 = EDGE_CURVE ( 'NONE', #63443, #65388, #61219, .T. ) ;
#1905 = ORIENTED_EDGE ( 'NONE', *, *, #19527, .F. ) ;
#1906 = ORIENTED_EDGE ( 'NONE', *, *, #49929, .T. ) ;
#1907 = CARTESIAN_POINT ( 'NONE',  ( -27.09048036756592026, 0.1785511875143080684, 2.303144499688032809 ) ) ;
#1908 = ADVANCED_FACE ( 'NONE', ( #30945 ), #45928, .T. ) ;
#1909 = ORIENTED_EDGE ( 'NONE', *, *, #42296, .F. ) ;
#1910 = CARTESIAN_POINT ( 'NONE',  ( 35.00000000000000000, 4.705694406421931860E-17, -3.469127814946512892E-15 ) ) ;
#1911 = CARTESIAN_POINT ( 'NONE',  ( 37.00000000000000711, 4.705694406421931860E-17, -3.469127814946512892E-15 ) ) ;
#1912 = ORIENTED_EDGE ( 'NONE', *, *, #9583, .T. ) ;
#1913 = CARTESIAN_POINT ( 'NONE',  ( 2.507146904658095199, 2.437115546363220808, 7.328382489803280997 ) ) ;
#1914 = DIRECTION ( 'NONE',  ( -1.000000000000000000, 0.000000000000000000, 0.000000000000000000 ) ) ;
#1915 = CARTESIAN_POINT ( 'NONE',  ( -29.25399988568289444, 1.550971944432816718, -13.41706731610524450 ) ) ;
#1916 = CYLINDRICAL_SURFACE ( 'NONE', #55027, 5.000000000000000888 ) ;
#1917 = AXIS2_PLACEMENT_3D ( 'NONE', #3547, #23819, #64352 ) ;
#1918 = B_SPLINE_CURVE_WITH_KNOTS ( 'NONE', 3,
 ( #19464, #51029, #9791, #25101, #30408, #46047, #45370, #60670, #15107, #35386, #55693, #10130, #50705, #5151, #5491, #12086, #2117, #26400, #26090 ),
 .UNSPECIFIED., .F., .F.,
 ( 4, 3, 3, 3, 3, 3, 4 ),
 ( 8.883182750045175563E-18, 4.457896483013979952E-05, 6.639290541541090999E-05, 8.820687556477923707E-05, 0.0001100173248778835882, 0.0001545671401658055700, 0.0001830328308068600405 ),
 .UNSPECIFIED. ) ;
#1919 = CARTESIAN_POINT ( 'NONE',  ( 37.00000000000000711, 12.60630747491662973, -1.908798535168425792 ) ) ;
#1920 = CARTESIAN_POINT ( 'NONE',  ( -47.00000000000000711, 0.000000000000000000, 0.000000000000000000 ) ) ;
#1921 = VECTOR ( 'NONE', #32346, 1000.000000000000000 ) ;
#1922 = ORIENTED_EDGE ( 'NONE', *, *, #61949, .F. ) ;
#1923 = CARTESIAN_POINT ( 'NONE',  ( -12.81094353615575088, -29.07674955874293943, -3.635823793966369788 ) ) ;
#1924 = ORIENTED_EDGE ( 'NONE', *, *, #23729, .F. ) ;
#1925 = CIRCLE ( 'NONE', #13586, 4.999999999999999112 ) ;
#1926 = CARTESIAN_POINT ( 'NONE',  ( -35.04683013664716640, -0.01075274317999010479, -0.006090538653967201080 ) ) ;
#1927 = FACE_OUTER_BOUND ( 'NONE', #51480, .T. ) ;
#1928 = CARTESIAN_POINT ( 'NONE',  ( -35.00000000000000000, 9.896810808925495806, -7.110831038798170134 ) ) ;
#1929 = VECTOR ( 'NONE', #21014, 1000.000000000000000 ) ;
#1930 = CARTESIAN_POINT ( 'NONE',  ( 37.00000000000000711, 4.705694406421931860E-17, -3.469127814946512892E-15 ) ) ;
#1931 = DIRECTION ( 'NONE',  ( 0.000000000000000000, 0.000000000000000000, -1.000000000000000000 ) ) ;
#1932 = ORIENTED_EDGE ( 'NONE', *, *, #16739, .T. ) ;
#1933 = ORIENTED_EDGE ( 'NONE', *, *, #24025, .T. ) ;
#1934 = CARTESIAN_POINT ( 'NONE',  ( 0.2833330754217391889, 1.928200609300473101, 12.09951353627561588 ) ) ;
#1935 = ORIENTED_EDGE ( 'NONE', *, *, #12328, .T. ) ;
#1936 = EDGE_CURVE ( 'NONE', #29286, #11296, #27408, .T. ) ;
#1937 = LINE ( 'NONE', #63105, #47894 ) ;
#1939 = CARTESIAN_POINT ( 'NONE',  ( -35.04643116707788408, -0.01204777744936991191, 0.001845126042312322800 ) ) ;
#1938 =( BOUNDED_SURFACE ( )  B_SPLINE_SURFACE ( 3, 1, ( 
 ( #40206, #60495 ),
 ( #14927, #20915 ),
 ( #41189, #31237 ),
 ( #51543, #44882 ) ),
 .UNSPECIFIED., .F., .F., .F. ) 
 B_SPLINE_SURFACE_WITH_KNOTS ( ( 4, 4 ),
 ( 2, 2 ),
 ( 0.000000000000000000, 1.000000000000000000 ),
 ( 0.000000000000000000, 1.000000000000000000 ),
 .UNSPECIFIED. ) 
 GEOMETRIC_REPRESENTATION_ITEM ( )  RATIONAL_B_SPLINE_SURFACE ( (
 ( 1.000000000000000000, 1.000000000000000000),
 ( 0.6933888150995267674, 0.9895912004443193632),
 ( 0.6933888150995267674, 0.9895912004443193632),
 ( 1.000000000000000000, 1.000000000000000000) ) ) 
 REPRESENTATION_ITEM ( '' )  SURFACE ( )  );
#1940 = CARTESIAN_POINT ( 'NONE',  ( 0.000000000000000000, 5.769711778877324448, 4.791703871138532023 ) ) ;
#1941 = CARTESIAN_POINT ( 'NONE',  ( 1.633930747253263149, 3.662223193115260234, -12.16309769563678067 ) ) ;
#1942 = CARTESIAN_POINT ( 'NONE',  ( 1.549075743846073827, -7.618376504786843029, -10.12891450359553147 ) ) ;
#1943 = CARTESIAN_POINT ( 'NONE',  ( 2.305787727787084407, 7.566723232958072032, 1.164987321564758371 ) ) ;
#1944 = LINE ( 'NONE', #33818, #55213 ) ;
#1945 = EDGE_LOOP ( 'NONE', ( #24408, #51110, #63276, #20739 ) ) ;
#1946 = VERTEX_POINT ( 'NONE', #15642 ) ;
#1947 = B_SPLINE_CURVE_WITH_KNOTS ( 'NONE', 3,
 ( #30120, #4868, #25454, #199, #45403, #20141, #40407, #60711, #40755, #61043, #56037, #35738, #14158, #34450, #11155, #57361 ),
 .UNSPECIFIED., .F., .F.,
 ( 4, 3, 3, 3, 3, 4 ),
 ( 1.371419323662639293E-18, 6.991367980366453884E-05, 0.0001398269368981367756, 0.0002097400188389093086, 0.0002811534801551364318, 0.0003526297678872523478 ),
 .UNSPECIFIED. ) ;
#1948 = CARTESIAN_POINT ( 'NONE',  ( 1.372161826076364610, -5.789954543171384138, 11.20801830616777472 ) ) ;
#1949 = ORIENTED_EDGE ( 'NONE', *, *, #12500, .T. ) ;
#1950 = CARTESIAN_POINT ( 'NONE',  ( -9.351388602708162523, 11.42638970207765681, -3.665735721005252135 ) ) ;
#1951 = DIRECTION ( 'NONE',  ( 1.000000000000000000, 0.000000000000000000, -0.000000000000000000 ) ) ;
#1952 = EDGE_CURVE ( 'NONE', #1056, #33980, #27239, .T. ) ;
#1953 = CARTESIAN_POINT ( 'NONE',  ( -27.09569413923886572, 1.680421072128821303, 1.607816962455205889 ) ) ;
#1954 = ORIENTED_EDGE ( 'NONE', *, *, #62247, .F. ) ;
#1955 = CARTESIAN_POINT ( 'NONE',  ( 0.9232058338315058954, -0.3773051331667114372, -12.46548196349786508 ) ) ;
#1956 = CARTESIAN_POINT ( 'NONE',  ( -22.38932658256920405, 1.810630688302315550, -3.587092141214307528 ) ) ;
#1957 = AXIS2_PLACEMENT_3D ( 'NONE', #7343, #42932, #58578 ) ;
#1958 = CARTESIAN_POINT ( 'NONE',  ( 3.152665057734126197, -1.848755561852092333, 7.719888720907804647 ) ) ;
#1959 = VERTEX_POINT ( 'NONE', #4388 ) ;
#1960 = ORIENTED_EDGE ( 'NONE', *, *, #22683, .F. ) ;
#1961 = FACE_OUTER_BOUND ( 'NONE', #62063, .T. ) ;
#1962 = ORIENTED_EDGE ( 'NONE', *, *, #44115, .T. ) ;
#1963 = ADVANCED_FACE ( 'NONE', ( #30300 ), #64464, .F. ) ;
#1964 = ORIENTED_EDGE ( 'NONE', *, *, #3810, .F. ) ;
#1965 = DIRECTION ( 'NONE',  ( -1.000000000000000000, 0.000000000000000000, 0.000000000000000000 ) ) ;
#1966 = ORIENTED_EDGE ( 'NONE', *, *, #19244, .F. ) ;
#1967 = ORIENTED_EDGE ( 'NONE', *, *, #3399, .F. ) ;
#1968 = CARTESIAN_POINT ( 'NONE',  ( 2.241506898688420346, -7.160521809579514674, 2.648071636522706829 ) ) ;
#1969 = EDGE_CURVE ( 'NONE', #23644, #35611, #24068, .T. ) ;
#1971 = CIRCLE ( 'NONE', #5193, 4.999999999999999112 ) ;
#1970 = CARTESIAN_POINT ( 'NONE',  ( 2.276198483116805615, 5.031786924855208731, -5.756970692722325644 ) ) ;
#1972 = FACE_OUTER_BOUND ( 'NONE', #43844, .T. ) ;
#1973 = CARTESIAN_POINT ( 'NONE',  ( 5.516018279890452902, -0.006771744149385743039, -0.0002248006052446425063 ) ) ;
#1974 = CARTESIAN_POINT ( 'NONE',  ( -37.00000000000000711, -9.821084925794515641, -7.215058775251366185 ) ) ;
#1975 = CARTESIAN_POINT ( 'NONE',  ( -35.00000000000000000, -8.389074212634351824, 8.839356091080015076 ) ) ;
#1976 = VECTOR ( 'NONE', #45259, 1000.000000000000000 ) ;
#1977 = VECTOR ( 'NONE', #16746, 1000.000000000000000 ) ;
#1978 = ORIENTED_EDGE ( 'NONE', *, *, #49712, .T. ) ;
#1979 = FACE_OUTER_BOUND ( 'NONE', #46224, .T. ) ;
#1980 = DIRECTION ( 'NONE',  ( 0.000000000000000000, 0.8369827122275325104, 0.5472293298355301872 ) ) ;
#1981 = CIRCLE ( 'NONE', #20001, 12.74999999999999822 ) ;
#1982 = DIRECTION ( 'NONE',  ( 0.000000000000000000, -0.5243256840888623760, -0.8515178078024829844 ) ) ;
#1983 = CARTESIAN_POINT ( 'NONE',  ( 0.000000000000000000, 1.145812388885215194, -6.715725538143608730 ) ) ;
#1984 = CARTESIAN_POINT ( 'NONE',  ( -35.00000000000000000, 0.000000000000000000, 0.000000000000000000 ) ) ;
#1985 = DIRECTION ( 'NONE',  ( -1.000000000000000000, 0.000000000000000000, 0.000000000000000000 ) ) ;
#1986 = AXIS2_PLACEMENT_3D ( 'NONE', #50488, #910, #46153 ) ;
#1987 = EDGE_CURVE ( 'NONE', #13432, #21858, #51426, .T. ) ;
#1988 = ORIENTED_EDGE ( 'NONE', *, *, #28623, .F. ) ;
#1989 = CARTESIAN_POINT ( 'NONE',  ( -37.00000000000000711, -1.488153103997047033, 11.65150730582934102 ) ) ;
#1990 = ORIENTED_EDGE ( 'NONE', *, *, #27825, .F. ) ;
#1991 = CARTESIAN_POINT ( 'NONE',  ( 2.000000000000001776, 5.107597897712416568, -4.693343793638371508 ) ) ;
#1992 = CARTESIAN_POINT ( 'NONE',  ( 2.249013661412227805, 5.926694833810679519, -4.816366775941289369 ) ) ;
#1993 = CARTESIAN_POINT ( 'NONE',  ( 2.034671305879536263, 11.19279775165900226, -3.325478336154866099 ) ) ;
#1994 = DIRECTION ( 'NONE',  ( 0.000000000000000000, 0.000000000000000000, 1.000000000000000000 ) ) ;
#1995 = CARTESIAN_POINT ( 'NONE',  ( 2.835339799623984636, -4.778327228934542426, -6.206025468804415191 ) ) ;
#1996 = ORIENTED_EDGE ( 'NONE', *, *, #57073, .F. ) ;
#1997 = DIRECTION ( 'NONE',  ( 0.000000000000000000, -0.01356324068818000848, 0.9999080150203990547 ) ) ;
#1998 = DIRECTION ( 'NONE',  ( 1.000000000000000000, 0.000000000000000000, 0.000000000000000000 ) ) ;
#1999 = LINE ( 'NONE', #38210, #3599 ) ;
#2000 = CYLINDRICAL_SURFACE ( 'NONE', #44416, 12.18650000000000055 ) ;
#2001 = EDGE_CURVE ( 'NONE', #40032, #38215, #40767, .T. ) ;
#2002 = CARTESIAN_POINT ( 'NONE',  ( -37.00000000000000711, -4.018060380616481631, 11.50504120060941915 ) ) ;
#2003 = ORIENTED_EDGE ( 'NONE', *, *, #41792, .T. ) ;
#2004 = AXIS2_PLACEMENT_3D ( 'NONE', #64591, #39333, #49661 ) ;
#2005 = PRODUCT_DEFINITION_CONTEXT ( 'detailed design', #20477, 'design' ) ;
#2006 = CARTESIAN_POINT ( 'NONE',  ( 0.2655924914740778187, -9.409507842006076928, 7.838010948425017332 ) ) ;
#2007 = DIRECTION ( 'NONE',  ( 0.000000000000000000, -0.01356324068817992001, 0.9999080150203990547 ) ) ;
#2008 = CIRCLE ( 'NONE', #26402, 4.999999999999999112 ) ;
#2009 = EDGE_LOOP ( 'NONE', ( #41662, #43468, #25227, #43967 ) ) ;
#2010 = VECTOR ( 'NONE', #19988, 1000.000000000000000 ) ;
#2012 = ORIENTED_EDGE ( 'NONE', *, *, #5105, .T. ) ;
#2011 = ADVANCED_FACE ( 'NONE', ( #40934 ), #48387, .F. ) ;
#2013 = CARTESIAN_POINT ( 'NONE',  ( 0.3040950598368144520, -2.376091969481297195, 12.02925914197704493 ) ) ;
#2014 = CARTESIAN_POINT ( 'NONE',  ( 31.24126863879125438, -3.096129103239020797, 23.22707964006411530 ) ) ;
#2015 = CARTESIAN_POINT ( 'NONE',  ( -34.00000000000000000, 1.836970198721036590E-16, 0.000000000000000000 ) ) ;
#2016 = VECTOR ( 'NONE', #25948, 1000.000000000000000 ) ;
#2017 = CARTESIAN_POINT ( 'NONE',  ( 0.3341166715381319596, -1.881279064087924224, 12.12403120948088642 ) ) ;
#2018 = EDGE_CURVE ( 'NONE', #8029, #9770, #16324, .T. ) ;
#2019 = VERTEX_POINT ( 'NONE', #56903 ) ;
#2020 = ORIENTED_EDGE ( 'NONE', *, *, #24564, .T. ) ;
#2021 = CIRCLE ( 'NONE', #27500, 12.18649999999999878 ) ;
#2022 = VERTEX_POINT ( 'NONE', #36601 ) ;
#2023 = CARTESIAN_POINT ( 'NONE',  ( 3.100650473568240084, 7.907988569971625026, 0.4517506188700623482 ) ) ;
#2024 = DIRECTION ( 'NONE',  ( 0.000000000000000000, 0.01356324068817998940, -0.9999080150203989437 ) ) ;
#2025 = EDGE_CURVE ( 'NONE', #49629, #4304, #26614, .T. ) ;
#2026 = VERTEX_POINT ( 'NONE', #21647 ) ;
#2027 = CARTESIAN_POINT ( 'NONE',  ( 35.00000000000000000, 6.018036132182163378, -11.24036214326522654 ) ) ;
#2028 = CARTESIAN_POINT ( 'NONE',  ( 2.245754705088394587, -7.538396044169879850, 1.216173395688216807 ) ) ;
#2029 = VERTEX_POINT ( 'NONE', #48150 ) ;
#2030 = DIRECTION ( 'NONE',  ( 1.000000000000000000, -0.000000000000000000, 0.000000000000000000 ) ) ;
#2031 = CARTESIAN_POINT ( 'NONE',  ( 8.782331025771476618, -31.88110954670732866, -13.48440172003491178 ) ) ;
#2032 = CARTESIAN_POINT ( 'NONE',  ( 35.00000000000000000, 11.72397916322012179, -0.7214809346829029746 ) ) ;
#2033 = ORIENTED_EDGE ( 'NONE', *, *, #20320, .F. ) ;
#2034 = ORIENTED_EDGE ( 'NONE', *, *, #18654, .F. ) ;
#2035 = DIRECTION ( 'NONE',  ( -1.000000000000000000, -0.000000000000000000, -0.000000000000000000 ) ) ;
#2036 = ORIENTED_EDGE ( 'NONE', *, *, #6051, .T. ) ;
#2037 = DIRECTION ( 'NONE',  ( 0.000000000000000000, 0.000000000000000000, 1.000000000000000000 ) ) ;
#2038 = DIRECTION ( 'NONE',  ( 1.000000000000000000, 0.000000000000000000, -0.000000000000000000 ) ) ;
#2039 = CARTESIAN_POINT ( 'NONE',  ( -19.47984447937493613, -3.750539801530005768, 11.39883551934753925 ) ) ;
#2040 = CARTESIAN_POINT ( 'NONE',  ( 35.00000000000000000, 5.143145423404279271, -11.66664283989681827 ) ) ;
#2042 = CARTESIAN_POINT ( 'NONE',  ( 0.2646305136544065406, 9.296005949277333258, -7.972778379581457742 ) ) ;
#2041 = AXIS2_PLACEMENT_3D ( 'NONE', #13469, #8488, #3540 ) ;
#2043 = DIRECTION ( 'NONE',  ( -1.000000000000000000, -0.000000000000000000, -0.000000000000000000 ) ) ;
#2044 = CARTESIAN_POINT ( 'NONE',  ( 0.6511581176972717211, 6.471755598256907049, -10.54760823437315764 ) ) ;
#2045 = DIRECTION ( 'NONE',  ( 0.000000000000000000, 0.01356324068817991828, -0.9999080150203990547 ) ) ;
#2046 = EDGE_LOOP ( 'NONE', ( #35707, #36113, #6467, #52889 ) ) ;
#2047 = ADVANCED_FACE ( 'NONE', ( #61865 ), #13980, .F. ) ;
#2048 = CARTESIAN_POINT ( 'NONE',  ( 2.000000000000001776, -5.997115278587647147, 3.485633455389469226 ) ) ;
#2049 = ORIENTED_EDGE ( 'NONE', *, *, #24914, .F. ) ;
#2050 = AXIS2_PLACEMENT_3D ( 'NONE', #58930, #64215, #44560 ) ;
#2051 = DIRECTION ( 'NONE',  ( 1.000000000000000000, 0.000000000000000000, 0.000000000000000000 ) ) ;
#2052 = CARTESIAN_POINT ( 'NONE',  ( 2.269879328255101303, 6.692746930934405647, 3.692763753157670692 ) ) ;
#2053 = ORIENTED_EDGE ( 'NONE', *, *, #21061, .T. ) ;
#2054 = CARTESIAN_POINT ( 'NONE',  ( 1.547277799338579118, -12.65564732076265209, 0.6737945300323602282 ) ) ;
#2055 = CARTESIAN_POINT ( 'NONE',  ( 0.2834382757448004053, 12.02923522794685240, -2.326926314863185130 ) ) ;
#2056 = DIRECTION ( 'NONE',  ( 0.000000000000000000, -0.5472293298355331848, 0.8369827122275305120 ) ) ;
#2057 = AXIS2_PLACEMENT_3D ( 'NONE', #13838, #8880, #29172 ) ;
#2058 = VERTEX_POINT ( 'NONE', #31287 ) ;
#2059 = ORIENTED_EDGE ( 'NONE', *, *, #5404, .T. ) ;
#2060 = DIRECTION ( 'NONE',  ( -1.000000000000000000, -0.000000000000000000, -0.000000000000000000 ) ) ;
#2061 = CIRCLE ( 'NONE', #26445, 7.499999999999988454 ) ;
#2062 = ORIENTED_EDGE ( 'NONE', *, *, #6020, .T. ) ;
#2063 = CARTESIAN_POINT ( 'NONE',  ( -35.00000000000000000, -6.657191900728257394, -9.677500615117970995 ) ) ;
#2064 = CARTESIAN_POINT ( 'NONE',  ( -27.08429572838383947, 2.089332284968718145, 0.9410937941433747955 ) ) ;
#2065 = FACE_OUTER_BOUND ( 'NONE', #44955, .T. ) ;
#2066 = DIRECTION ( 'NONE',  ( -1.000000000000000000, -0.000000000000000000, 0.000000000000000000 ) ) ;
#2067 = EDGE_LOOP ( 'NONE', ( #8310, #48829, #48406, #37613 ) ) ;
#2068 = B_SPLINE_CURVE_WITH_KNOTS ( 'NONE', 3,
 ( #49290, #3745, #24000, #39269, #34286, #24644, #10318, #51245, #15950, #56550, #14967, #30288, #19977, #56199, #25622, #50901 ),
 .UNSPECIFIED., .F., .F.,
 ( 4, 3, 3, 3, 3, 4 ),
 ( 3.074549376240319640E-15, 0.0002126834539179954726, 0.0004253519300366764974, 0.0006380165497224911993, 0.0007442707582429119268, 0.0009453531351411830885 ),
 .UNSPECIFIED. ) ;
#2069 = AXIS2_PLACEMENT_3D ( 'NONE', #61587, #41642, #16388 ) ;
#2070 = DIRECTION ( 'NONE',  ( 0.000000000000000000, 0.000000000000000000, 1.000000000000000000 ) ) ;
#2071 = EDGE_CURVE ( 'NONE', #47315, #28963, #61561, .T. ) ;
#2072 = CARTESIAN_POINT ( 'NONE',  ( 19.24109636373441390, -29.98159021036885363, -5.977446804020350335 ) ) ;
#2073 = DIRECTION ( 'NONE',  ( -1.000000000000000000, 0.000000000000000000, 0.000000000000000000 ) ) ;
#2074 = CARTESIAN_POINT ( 'NONE',  ( 6.361445718264521432, -4.355102044641763648, 25.00000000000000000 ) ) ;
#2075 = CARTESIAN_POINT ( 'NONE',  ( 2.000000000000001776, 1.058508696395052517, -6.730038252034905355 ) ) ;
#2076 = FACE_OUTER_BOUND ( 'NONE', #5382, .T. ) ;
#2077 = CARTESIAN_POINT ( 'NONE',  ( 2.247112776671465806, -5.774169979601956548, 4.997244136394455083 ) ) ;
#2078 = CARTESIAN_POINT ( 'NONE',  ( 2.373367633546872302, 5.072743978105314966, -5.764146204907413917 ) ) ;
#2079 = AXIS2_PLACEMENT_3D ( 'NONE', #1911, #22182, #57787 ) ;
#2080 = EDGE_CURVE ( 'NONE', #32174, #47999, #22752, .T. ) ;
#2081 = ORIENTED_EDGE ( 'NONE', *, *, #2651, .F. ) ;
#2082 = DIRECTION ( 'NONE',  ( 1.000000000000000000, 0.000000000000000000, 0.000000000000000000 ) ) ;
#2083 = CARTESIAN_POINT ( 'NONE',  ( 37.00000000000000711, 10.43555801961475282, -5.391785509271000087 ) ) ;
#2084 = ORIENTED_EDGE ( 'NONE', *, *, #42682, .T. ) ;
#2085 = VECTOR ( 'NONE', #49994, 1000.000000000000000 ) ;
#2086 = EDGE_CURVE ( 'NONE', #28230, #52659, #42461, .T. ) ;
#2087 = CARTESIAN_POINT ( 'NONE',  ( 36.00000000000000711, -2.250029553613672295, 12.54989509947652770 ) ) ;
#2088 = CARTESIAN_POINT ( 'NONE',  ( -35.00000000000000000, -11.56998259273174945, -3.827046518385204266 ) ) ;
#2089 = ORIENTED_EDGE ( 'NONE', *, *, #34398, .T. ) ;
#2090 = DIRECTION ( 'NONE',  ( -1.000000000000000000, 0.000000000000000000, 0.000000000000000000 ) ) ;
#2091 = EDGE_CURVE ( 'NONE', #2794, #25335, #38473, .T. ) ;
#2092 = ORIENTED_EDGE ( 'NONE', *, *, #36645, .T. ) ;
#2093 = DIRECTION ( 'NONE',  ( -1.000000000000000000, 0.000000000000000000, 0.000000000000000000 ) ) ;
#2094 = EDGE_LOOP ( 'NONE', ( #25010, #16187, #63956, #48859 ) ) ;
#2095 = VERTEX_POINT ( 'NONE', #63401 ) ;
#2096 = AXIS2_PLACEMENT_3D ( 'NONE', #30955, #20971, #1038 ) ;
#2097 = CARTESIAN_POINT ( 'NONE',  ( -27.08426571771018487, -1.845988025802333787, 1.357728109767515345 ) ) ;
#2098 = EDGE_CURVE ( 'NONE', #21166, #60814, #11002, .T. ) ;
#2099 = ORIENTED_EDGE ( 'NONE', *, *, #13165, .T. ) ;
#2100 = DIRECTION ( 'NONE',  ( 0.000000000000000000, 0.000000000000000000, 1.000000000000000000 ) ) ;
#2101 = CARTESIAN_POINT ( 'NONE',  ( 3.709656308118471912, 4.519821899412372446, 12.72824511710198792 ) ) ;
#2102 = AXIS2_PLACEMENT_3D ( 'NONE', #59192, #59504, #34226 ) ;
#2103 = CARTESIAN_POINT ( 'NONE',  ( -36.00000000000000711, -4.824807283154036064, -11.80185301892985983 ) ) ;
#2104 = CARTESIAN_POINT ( 'NONE',  ( 1.719304012341317467, -0.7661785589597189805, -12.70777170743969009 ) ) ;
#2105 = ORIENTED_EDGE ( 'NONE', *, *, #26511, .T. ) ;
#2106 = CYLINDRICAL_SURFACE ( 'NONE', #45841, 12.18649999999999878 ) ;
#2107 = ADVANCED_FACE ( 'NONE', ( #28182 ), #48472, .T. ) ;
#2108 = CARTESIAN_POINT ( 'NONE',  ( 13.74768401152558894, -27.65692779101644305, 12.04119239038937117 ) ) ;
#2109 = CARTESIAN_POINT ( 'NONE',  ( 2.589278595513877512, -7.746633201027364635, 0.2408616556822583132 ) ) ;
#2111 = VERTEX_POINT ( 'NONE', #2920 ) ;
#2110 = CARTESIAN_POINT ( 'NONE',  ( 0.2651627682582904932, -12.07509313786331973, -2.039709641845705690 ) ) ;
#2112 = CARTESIAN_POINT ( 'NONE',  ( 35.00000000000000000, -5.927257550915237871, 10.64792938439761549 ) ) ;
#2113 = VERTEX_POINT ( 'NONE', #45105 ) ;
#2114 = CARTESIAN_POINT ( 'NONE',  ( -37.00000000000000711, 0.000000000000000000, 0.000000000000000000 ) ) ;
#2115 = AXIS2_PLACEMENT_3D ( 'NONE', #55523, #34569, #4003 ) ;
#2116 = ORIENTED_EDGE ( 'NONE', *, *, #16294, .T. ) ;
#2117 = CARTESIAN_POINT ( 'NONE',  ( 0.2657645697724712597, 9.477802844074149746, -7.755260067564052839 ) ) ;
#2118 = DIRECTION ( 'NONE',  ( 0.000000000000000000, -0.01356324068817998940, 0.9999080150203990547 ) ) ;
#2119 = CARTESIAN_POINT ( 'NONE',  ( 35.00000000000000000, 6.917234959366825642, -9.493370459201726064 ) ) ;
#2120 = ORIENTED_EDGE ( 'NONE', *, *, #57931, .F. ) ;
#2121 = CARTESIAN_POINT ( 'NONE',  ( 0.7400311444011720141, 8.241979373543657061, 9.270387619166349680 ) ) ;
#2122 = DIRECTION ( 'NONE',  ( -1.000000000000000000, -0.000000000000000000, -0.000000000000000000 ) ) ;
#2123 = CARTESIAN_POINT ( 'NONE',  ( -22.29018399051993526, -3.609810019245839108, -0.9010028109495191728 ) ) ;
#2125 = ORIENTED_EDGE ( 'NONE', *, *, #13653, .F. ) ;
#2124 = EDGE_CURVE ( 'NONE', #33360, #15413, #64127, .T. ) ;
#2126 =( BOUNDED_SURFACE ( )  B_SPLINE_SURFACE ( 3, 1, ( 
 ( #44053, #14106 ),
 ( #55002, #3517 ),
 ( #18790, #14429 ),
 ( #39053, #59343 ) ),
 .UNSPECIFIED., .F., .F., .F. ) 
 B_SPLINE_SURFACE_WITH_KNOTS ( ( 4, 4 ),
 ( 2, 2 ),
 ( 0.000000000000000000, 1.000000000000000000 ),
 ( 0.000000000000000000, 1.000000000000000000 ),
 .UNSPECIFIED. ) 
 GEOMETRIC_REPRESENTATION_ITEM ( )  RATIONAL_B_SPLINE_SURFACE ( (
 ( 1.000000000000000000, 1.000000000000000000),
 ( 0.8716676215708681896, 0.8964445200148167814),
 ( 0.8716676215708681896, 0.8964445200148167814),
 ( 1.000000000000000000, 1.000000000000000000) ) ) 
 REPRESENTATION_ITEM ( '' )  SURFACE ( )  );
#2127 = ORIENTED_EDGE ( 'NONE', *, *, #26732, .F. ) ;
#2128 = CARTESIAN_POINT ( 'NONE',  ( 3.100650473569637189, 7.709402782713580038, 1.818095316078564005 ) ) ;
#2129 = ORIENTED_EDGE ( 'NONE', *, *, #32713, .F. ) ;
#2130 = EDGE_CURVE ( 'NONE', #20972, #23800, #14807, .T. ) ;
#2131 = ORIENTED_EDGE ( 'NONE', *, *, #7041, .F. ) ;
#2132 = LINE ( 'NONE', #16763, #49799 ) ;
#2133 = CARTESIAN_POINT ( 'NONE',  ( 145.1370849898475797, 3.309064568108273190E-14, 0.000000000000000000 ) ) ;
#2134 = DIRECTION ( 'NONE',  ( 0.000000000000000000, -0.2006870767258747135, 0.9796553971857772103 ) ) ;
#2135 = DIRECTION ( 'NONE',  ( 0.000000000000000000, 0.000000000000000000, 1.000000000000000000 ) ) ;
#2136 = CARTESIAN_POINT ( 'NONE',  ( 5.516018279890452902, -0.003191189039764480428, 0.005976902763918706153 ) ) ;
#2137 = DIRECTION ( 'NONE',  ( 0.000000000000000000, 0.000000000000000000, -1.000000000000000000 ) ) ;
#2138 = AXIS2_PLACEMENT_3D ( 'NONE', #59492, #54521, #3333 ) ;
#2139 = AXIS2_PLACEMENT_3D ( 'NONE', #1984, #38191, #22252 ) ;
#2140 = DIRECTION ( 'NONE',  ( 0.000000000000000000, -1.000000000000000000, 0.000000000000000000 ) ) ;
#2141 =( BOUNDED_SURFACE ( )  B_SPLINE_SURFACE ( 3, 1, ( 
 ( #10981, #61837 ),
 ( #15307, #35583 ),
 ( #55877, #20636 ),
 ( #45902, #10309 ) ),
 .UNSPECIFIED., .F., .F., .F. ) 
 B_SPLINE_SURFACE_WITH_KNOTS ( ( 4, 4 ),
 ( 2, 2 ),
 ( 0.000000000000000000, 1.000000000000000000 ),
 ( 0.000000000000000000, 1.000000000000000000 ),
 .UNSPECIFIED. ) 
 GEOMETRIC_REPRESENTATION_ITEM ( )  RATIONAL_B_SPLINE_SURFACE ( (
 ( 1.000000000000000000, 1.000000000000000000),
 ( 0.6933888150995267674, 0.9895912004443193632),
 ( 0.6933888150995267674, 0.9895912004443193632),
 ( 1.000000000000000000, 1.000000000000000000) ) ) 
 REPRESENTATION_ITEM ( '' )  SURFACE ( )  );
#2142 = VERTEX_POINT ( 'NONE', #4209 ) ;
#2143 = CARTESIAN_POINT ( 'NONE',  ( -35.00000000000000000, -12.01765980939843281, 2.021542716731355771 ) ) ;
#2144 = DIRECTION ( 'NONE',  ( 0.000000000000000000, -0.9551603052523509607, 0.2960891610144411601 ) ) ;
#2145 = AXIS2_PLACEMENT_3D ( 'NONE', #15184, #25163, #54118 ) ;
#2146 = EDGE_CURVE ( 'NONE', #58714, #32257, #64385, .T. ) ;
#2147 = CARTESIAN_POINT ( 'NONE',  ( 0.3278977287071224711, 4.427879319183047890, -11.44003061923226916 ) ) ;
#2148 = CARTESIAN_POINT ( 'NONE',  ( 35.00000000000000000, 4.705694406421931860E-17, -3.469127814946512892E-15 ) ) ;
#2149 = CARTESIAN_POINT ( 'NONE',  ( -35.00000000000000000, 0.000000000000000000, 0.000000000000000000 ) ) ;
#2150 = CONICAL_SURFACE ( 'NONE', #3216, 7.938172270156617749, 1.280189991382167047 ) ;
#2151 = CARTESIAN_POINT ( 'NONE',  ( 35.00000000000000000, 11.05394794832829497, -5.130401251914769922 ) ) ;
#2152 = CARTESIAN_POINT ( 'NONE',  ( 9.625472734749340731, 2.219514715007567141, -11.79494074077256904 ) ) ;
#2153 = ORIENTED_EDGE ( 'NONE', *, *, #52516, .T. ) ;
#2154 = DIRECTION ( 'NONE',  ( 0.000000000000000000, -0.6943713148249691658, 0.7196168960969744344 ) ) ;
#2155 = DIRECTION ( 'NONE',  ( 0.000000000000000000, -0.01356324068817999114, 0.9999080150203989437 ) ) ;
#2156 = CARTESIAN_POINT ( 'NONE',  ( 5.536195898058073439, -0.008071068258923201275, 0.002666509901869582554 ) ) ;
#2157 = ADVANCED_FACE ( 'NONE', ( #19171 ), #20787, .F. ) ;
#2158 = LINE ( 'NONE', #52714, #51393 ) ;
#2159 = ADVANCED_FACE ( 'NONE', ( #59408 ), #9498, .T. ) ;
#2160 = CARTESIAN_POINT ( 'NONE',  ( 12.93723047338301058, 4.476360154859203355, 25.00000000000000000 ) ) ;
#2161 = DIRECTION ( 'NONE',  ( -1.000000000000000000, 0.000000000000000000, -0.000000000000000000 ) ) ;
#2162 = VECTOR ( 'NONE', #8756, 1000.000000000000000 ) ;
#2163 = ORIENTED_EDGE ( 'NONE', *, *, #21823, .T. ) ;
#2164 = DIRECTION ( 'NONE',  ( -0.000000000000000000, -1.000000000000000000, -0.000000000000000000 ) ) ;
#2165 = CARTESIAN_POINT ( 'NONE',  ( 1.452237505248552996, -1.611965288198645929, -12.55261342181977113 ) ) ;
#2166 = CARTESIAN_POINT ( 'NONE',  ( 0.2648978790185593790, 9.295532325666449935, 7.972372351883061370 ) ) ;
#2167 = CARTESIAN_POINT ( 'NONE',  ( -22.70624764888619751, -0.08990180771016251238, 5.249808673991983810 ) ) ;
#2168 = ORIENTED_EDGE ( 'NONE', *, *, #39019, .F. ) ;
#2169 = DIRECTION ( 'NONE',  ( 0.000000000000000000, -0.01356324068817998940, 0.9999080150203990547 ) ) ;
#2170 = AXIS2_PLACEMENT_3D ( 'NONE', #48812, #60085, #56399 ) ;
#2171 = LINE ( 'NONE', #61362, #7840 ) ;
#2172 = EDGE_CURVE ( 'NONE', #43940, #7543, #5285, .T. ) ;
#2173 = ORIENTED_EDGE ( 'NONE', *, *, #50269, .F. ) ;
#2174 = ORIENTED_EDGE ( 'NONE', *, *, #31651, .F. ) ;
#2175 = FACE_OUTER_BOUND ( 'NONE', #40364, .T. ) ;
#2176 = VECTOR ( 'NONE', #45492, 999.9999999999998863 ) ;
#2177 = AXIS2_PLACEMENT_3D ( 'NONE', #50583, #33950, #34604 ) ;
#2178 = VECTOR ( 'NONE', #11059, 1000.000000000000000 ) ;
#2179 = CIRCLE ( 'NONE', #46744, 7.499999999999988454 ) ;
#2180 = CARTESIAN_POINT ( 'NONE',  ( -37.00000000000000711, 0.000000000000000000, 0.000000000000000000 ) ) ;
#2181 = VERTEX_POINT ( 'NONE', #24823 ) ;
#2182 = CARTESIAN_POINT ( 'NONE',  ( 0.2676618633000428238, -9.484212776852388060, 7.748413788583189188 ) ) ;
#2183 = DIRECTION ( 'NONE',  ( 0.000000000000000000, 0.1118654143051617117, 0.9937233664769761221 ) ) ;
#2184 = CARTESIAN_POINT ( 'NONE',  ( 2.241526690369555652, 7.515450538999852270, -1.342748965918806769 ) ) ;
#2185 = CARTESIAN_POINT ( 'NONE',  ( -35.00000000000000000, 11.29812557209476864, 3.213188559034282132 ) ) ;
#2186 = CARTESIAN_POINT ( 'NONE',  ( -9.838546225284394708, 10.19292628221959518, -6.347466807329325000 ) ) ;
#2187 = ADVANCED_FACE ( 'NONE', ( #54097 ), #54782, .F. ) ;
#2188 = CARTESIAN_POINT ( 'NONE',  ( -10.79842706929647278, -9.842369975612381694, 9.240427863961670596 ) ) ;
#2190 = VERTEX_POINT ( 'NONE', #49764 ) ;
#2189 = CARTESIAN_POINT ( 'NONE',  ( -35.00000000000000000, 10.62137734850268345, 5.015831474386344802 ) ) ;
#2191 = DIRECTION ( 'NONE',  ( -1.000000000000000000, 0.000000000000000000, 0.000000000000000000 ) ) ;
#2192 = EDGE_CURVE ( 'NONE', #46377, #63634, #59915, .T. ) ;
#2193 = ORIENTED_EDGE ( 'NONE', *, *, #20768, .T. ) ;
#2194 = DIRECTION ( 'NONE',  ( -1.000000000000000000, 0.000000000000000000, 0.000000000000000000 ) ) ;
#2195 = ORIENTED_EDGE ( 'NONE', *, *, #39656, .F. ) ;
#2196 = ORIENTED_EDGE ( 'NONE', *, *, #14629, .T. ) ;
#2197 = APPLICATION_PROTOCOL_DEFINITION ( 'draft international standard', 'automotive_design', 1998, #57885 ) ;
#2198 = CARTESIAN_POINT ( 'NONE',  ( 0.4613984246114896104, -11.46927345719239710, 4.475519447653946159 ) ) ;
#2199 = EDGE_CURVE ( 'NONE', #16200, #36996, #52042, .T. ) ;
#2200 = CIRCLE ( 'NONE', #15984, 12.74999999999999822 ) ;
#2201 = CARTESIAN_POINT ( 'NONE',  ( -15.83540182711247191, -34.24586518154816872, 7.348477566591424370 ) ) ;
#2202 = LINE ( 'NONE', #32439, #39618 ) ;
#2203 = CARTESIAN_POINT ( 'NONE',  ( -32.73308617475133531, -2.903166307960748593, -22.77405829473930865 ) ) ;
#2204 = EDGE_CURVE ( 'NONE', #16590, #54151, #60955, .T. ) ;
#2205 = DIRECTION ( 'NONE',  ( 1.000000000000000000, 0.000000000000000000, 0.000000000000000000 ) ) ;
#2207 = ORIENTED_EDGE ( 'NONE', *, *, #64392, .F. ) ;
#2206 = VECTOR ( 'NONE', #46791, 1000.000000000000000 ) ;
#2208 = AXIS2_PLACEMENT_3D ( 'NONE', #47807, #57803, #36840 ) ;
#2209 = CARTESIAN_POINT ( 'NONE',  ( 0.2646305136544072623, 11.55263159009964191, -4.064188116014436858 ) ) ;
#2210 = CARTESIAN_POINT ( 'NONE',  ( 0.8320506296491601006, -3.891425424503382580, 11.81055997318802397 ) ) ;
#2211 = ORIENTED_EDGE ( 'NONE', *, *, #33043, .F. ) ;
#2212 = ORIENTED_EDGE ( 'NONE', *, *, #49357, .F. ) ;
#2213 = VECTOR ( 'NONE', #3653, 1000.000000000000000 ) ;
#2214 = EDGE_CURVE ( 'NONE', #62530, #44220, #34597, .T. ) ;
#2215 = FACE_OUTER_BOUND ( 'NONE', #44117, .T. ) ;
#2216 = ORIENTED_EDGE ( 'NONE', *, *, #20034, .F. ) ;
#2217 = AXIS2_PLACEMENT_3D ( 'NONE', #18678, #9303, #9630 ) ;
#2218 = CYLINDRICAL_SURFACE ( 'NONE', #31691, 12.75000000000000178 ) ;
#2219 = DIRECTION ( 'NONE',  ( 1.000000000000000000, 0.000000000000000000, -0.000000000000000000 ) ) ;
#2220 = CARTESIAN_POINT ( 'NONE',  ( -37.00000000000000711, -11.74614673114904129, -0.01609748574457297438 ) ) ;
#2221 = CARTESIAN_POINT ( 'NONE',  ( -22.27706485742869091, 0.9221835209182547288, 3.563814065926663499 ) ) ;
#2222 = DIRECTION ( 'NONE',  ( 1.000000000000000000, 0.000000000000000000, 0.000000000000000000 ) ) ;
#2223 = CARTESIAN_POINT ( 'NONE',  ( -27.08429572838383947, -1.859677275556421927, 1.338867938658193424 ) ) ;
#2224 = CARTESIAN_POINT ( 'NONE',  ( 2.253265082352434057, 3.929729351083079969, -6.549959928643395379 ) ) ;
#2225 = AXIS2_PLACEMENT_3D ( 'NONE', #29351, #65559, #9712 ) ;
#2226 = ORIENTED_EDGE ( 'NONE', *, *, #55583, .F. ) ;
#2227 = DIRECTION ( 'NONE',  ( 1.000000000000000000, -0.000000000000000000, -0.000000000000000000 ) ) ;
#2228 = ORIENTED_EDGE ( 'NONE', *, *, #7230, .F. ) ;
#2229 = AXIS2_PLACEMENT_3D ( 'NONE', #23782, #33074, #27763 ) ;
#2230 = CARTESIAN_POINT ( 'NONE',  ( 0.2652384770603659070, -6.180206054297680218, 10.57229757085620570 ) ) ;
#2231 = CARTESIAN_POINT ( 'NONE',  ( -9.010009660721790326, -10.91952191215454526, -7.945783354247663688 ) ) ;
#2232 = DIRECTION ( 'NONE',  ( 0.000000000000000000, 0.000000000000000000, 1.000000000000000000 ) ) ;
#2233 = DIRECTION ( 'NONE',  ( -1.000000000000000000, -0.000000000000000000, 0.000000000000000000 ) ) ;
#2234 = VERTEX_POINT ( 'NONE', #25144 ) ;
#2235 = CIRCLE ( 'NONE', #41508, 4.999999999999999112 ) ;
#2236 = EDGE_CURVE ( 'NONE', #28622, #44459, #25071, .T. ) ;
#2237 = CIRCLE ( 'NONE', #35086, 2.899999999999995026 ) ;
#2238 = ORIENTED_EDGE ( 'NONE', *, *, #18675, .T. ) ;
#2239 = VECTOR ( 'NONE', #46424, 1000.000000000000000 ) ;
#2240 = CYLINDRICAL_SURFACE ( 'NONE', #64129, 4.999999999999997335 ) ;
#2241 = VERTEX_POINT ( 'NONE', #212 ) ;
#2242 = DIRECTION ( 'NONE',  ( 1.000000000000000000, 0.000000000000000000, 0.000000000000000000 ) ) ;
#2243 = CARTESIAN_POINT ( 'NONE',  ( 8.437200413559441614, 4.868584981346780971, 10.97613720874745269 ) ) ;
#2244 = CARTESIAN_POINT ( 'NONE',  ( 1.194176325881340039, -9.940715479868391213, -7.670099510969166978 ) ) ;
#2245 = DIRECTION ( 'NONE',  ( 0.000000000000000000, -0.9903235168508566222, -0.1387779952735712363 ) ) ;
#2246 = ORIENTED_EDGE ( 'NONE', *, *, #64741, .T. ) ;
#2247 = CARTESIAN_POINT ( 'NONE',  ( 0.3610902822527219946, 12.13436647668549639, 1.873269382026034657 ) ) ;
#2248 = CARTESIAN_POINT ( 'NONE',  ( -23.41523303002442091, -0.3963225057404748397, 4.681453266967022131 ) ) ;
#2249 = EDGE_CURVE ( 'NONE', #23975, #51925, #11474, .T. ) ;
#2250 = CARTESIAN_POINT ( 'NONE',  ( -22.71097035706202405, 0.4203397252017515573, -4.965150228107761521 ) ) ;
#2251 = CARTESIAN_POINT ( 'NONE',  ( -35.00000000000000000, 9.321877890560440250, 7.146664589317944127 ) ) ;
#2252 = CIRCLE ( 'NONE', #10729, 1.500000000000000222 ) ;
#2253 = VECTOR ( 'NONE', #26938, 1000.000000000000000 ) ;
#2254 = CARTESIAN_POINT ( 'NONE',  ( -37.00000000000000711, 12.71517666308949579, -0.9416912585473031783 ) ) ;
#2255 = VECTOR ( 'NONE', #41696, 1000.000000000000000 ) ;
#2256 = CARTESIAN_POINT ( 'NONE',  ( 2.000000000000001776, -1.865193240757054394, -6.552473556515217012 ) ) ;
#2257 = EDGE_LOOP ( 'NONE', ( #19542, #2542, #30218, #9068 ) ) ;
#2258 = CIRCLE ( 'NONE', #62750, 4.999999999999999112 ) ;
#2259 = CARTESIAN_POINT ( 'NONE',  ( -12.58725039716645000, -33.86007533429943095, -10.00564543523592320 ) ) ;
#2260 = ORIENTED_EDGE ( 'NONE', *, *, #47857, .T. ) ;
#2261 = CARTESIAN_POINT ( 'NONE',  ( 35.00000000000000000, 4.705694406421931860E-17, -3.469127814946512892E-15 ) ) ;
#2262 = DIRECTION ( 'NONE',  ( -1.000000000000000000, -0.000000000000000000, -0.000000000000000000 ) ) ;
#2263 = DIRECTION ( 'NONE',  ( 0.000000000000000000, 0.01356324068817991481, -0.9999080150203990547 ) ) ;
#2264 = EDGE_CURVE ( 'NONE', #48793, #61407, #52467, .T. ) ;
#2265 = AXIS2_PLACEMENT_3D ( 'NONE', #52763, #53431, #48444 ) ;
#2266 = DIRECTION ( 'NONE',  ( 0.9364047569793457759, -0.3509218304786018705, 0.000000000000000000 ) ) ;
#2267 = EDGE_CURVE ( 'NONE', #47648, #28210, #63924, .T. ) ;
#2268 = CARTESIAN_POINT ( 'NONE',  ( 0.2739690278137258961, -11.44648082006009560, 4.360944092821414486 ) ) ;
#2269 = VERTEX_POINT ( 'NONE', #41398 ) ;
#2270 = ORIENTED_EDGE ( 'NONE', *, *, #57217, .F. ) ;
#2271 = CARTESIAN_POINT ( 'NONE',  ( 5.516018279890452902, 0.003580555109620797271, 0.005752102158673854694 ) ) ;
#2272 = ORIENTED_EDGE ( 'NONE', *, *, #56146, .T. ) ;
#2273 = AXIS2_PLACEMENT_3D ( 'NONE', #3939, #24202, #8262 ) ;
#2274 = CARTESIAN_POINT ( 'NONE',  ( 2.872766899732817958, 3.568102790788560963, 11.46450991852135637 ) ) ;
#2275 = CARTESIAN_POINT ( 'NONE',  ( 2.507146904658100084, 7.328382489803307642, -2.437115546363147534 ) ) ;
#2276 = CARTESIAN_POINT ( 'NONE',  ( 3.152665057736161902, 7.719888720907650992, -1.848755561854025231 ) ) ;
#2277 = CARTESIAN_POINT ( 'NONE',  ( 1.283627346226916766, 3.783098238613507913, -12.00363697230100968 ) ) ;
#2278 = CARTESIAN_POINT ( 'NONE',  ( 0.000000000000000000, -5.457833520448623688, -4.281014542496604847 ) ) ;
#2279 = CARTESIAN_POINT ( 'NONE',  ( 2.305787727787084407, -1.164987321564783684, 7.566723232958066703 ) ) ;
#2280 = DIRECTION ( 'NONE',  ( 0.000000000000000000, 0.01356324068817998940, -0.9999080150203990547 ) ) ;
#2281 = ORIENTED_EDGE ( 'NONE', *, *, #44975, .F. ) ;
#2282 = AXIS2_PLACEMENT_3D ( 'NONE', #17570, #57151, #6936 ) ;
#2283 = ORIENTED_EDGE ( 'NONE', *, *, #18854, .F. ) ;
#2284 = DIRECTION ( 'NONE',  ( 0.000000000000000000, -0.01356324068817999114, 0.9999080150203989437 ) ) ;
#2285 = ORIENTED_EDGE ( 'NONE', *, *, #6769, .F. ) ;
#2286 =( NAMED_UNIT ( * ) SI_UNIT ( $, .STERADIAN. ) SOLID_ANGLE_UNIT ( ) );
#2287 = EDGE_CURVE ( 'NONE', #58825, #45959, #61688, .T. ) ;
#2288 = DIRECTION ( 'NONE',  ( 1.000000000000000000, 0.000000000000000000, 0.000000000000000000 ) ) ;
#2290 = DIRECTION ( 'NONE',  ( -1.000000000000000000, -0.000000000000000000, 0.000000000000000000 ) ) ;
#2289 = VECTOR ( 'NONE', #8965, 1000.000000000000114 ) ;
#2291 = ADVANCED_FACE ( 'NONE', ( #11166 ), #31441, .T. ) ;
#2292 = CARTESIAN_POINT ( 'NONE',  ( -22.31213670151049300, -1.669817926839913147, 3.398324501467281156 ) ) ;
#2293 = VERTEX_POINT ( 'NONE', #33068 ) ;
#2294 = DIRECTION ( 'NONE',  ( 1.000000000000000000, 0.000000000000000000, -0.000000000000000000 ) ) ;
#2295 = CARTESIAN_POINT ( 'NONE',  ( -14.80332308495361815, -33.90539544391017301, -8.876538241604327695 ) ) ;
#2296 = CARTESIAN_POINT ( 'NONE',  ( -37.00000000000000711, 0.000000000000000000, 0.000000000000000000 ) ) ;
#2297 = VERTEX_POINT ( 'NONE', #53375 ) ;
#2298 = VERTEX_POINT ( 'NONE', #62659 ) ;
#2299 = EDGE_CURVE ( 'NONE', #49715, #11584, #43045, .T. ) ;
#2300 = CARTESIAN_POINT ( 'NONE',  ( 1.719304012338199517, 0.000000000000000000, 0.000000000000000000 ) ) ;
#2301 = VERTEX_POINT ( 'NONE', #32079 ) ;
#2302 = ORIENTED_EDGE ( 'NONE', *, *, #37993, .T. ) ;
#2303 = DIRECTION ( 'NONE',  ( 0.000000000000000000, 0.6478160128811893959, -0.7617968321374923857 ) ) ;
#2304 = VERTEX_POINT ( 'NONE', #62341 ) ;
#2305 = ORIENTED_EDGE ( 'NONE', *, *, #52599, .T. ) ;
#2306 = CIRCLE ( 'NONE', #40486, 4.999999999999999112 ) ;
#2307 = CARTESIAN_POINT ( 'NONE',  ( -22.27720412283625961, -2.752887114864230877, 2.444672752438195928 ) ) ;
#2308 = CARTESIAN_POINT ( 'NONE',  ( 37.00000000000000711, 4.705694406421931860E-17, -3.469127814946512892E-15 ) ) ;
#2309 = CIRCLE ( 'NONE', #50049, 12.74999999999999822 ) ;
#2310 = FACE_BOUND ( 'NONE', #52616, .T. ) ;
#2311 = DIRECTION ( 'NONE',  ( 0.000000000000000000, 0.9937233664769765662, -0.1118654143051580896 ) ) ;
#2312 = DIRECTION ( 'NONE',  ( -1.000000000000000000, 0.000000000000000000, 0.000000000000000000 ) ) ;
#2313 = ADVANCED_FACE ( 'NONE', ( #7821 ), #12135, .T. ) ;
#2314 = CIRCLE ( 'NONE', #22459, 6.000000000000000888 ) ;
#2315 = DIRECTION ( 'NONE',  ( -1.000000000000000000, -0.000000000000000000, 0.000000000000000000 ) ) ;
#2316 = EDGE_LOOP ( 'NONE', ( #32470, #31681, #2371, #436 ) ) ;
#2317 = CARTESIAN_POINT ( 'NONE',  ( 2.941278708680199916, 1.198640839021388960, -6.021511413163950444 ) ) ;
#2318 = CARTESIAN_POINT ( 'NONE',  ( -35.00000000000000000, 0.000000000000000000, 0.000000000000000000 ) ) ;
#2319 = CIRCLE ( 'NONE', #62810, 4.999999999999998224 ) ;
#2320 = CARTESIAN_POINT ( 'NONE',  ( 5.514970785353741078, 0.002619824551223220045, -0.003929719953530077733 ) ) ;
#2321 = CARTESIAN_POINT ( 'NONE',  ( 29.56688794281942023, 5.030830317295369447, 10.90585321954392128 ) ) ;
#2322 = DIRECTION ( 'NONE',  ( -1.000000000000000000, 0.000000000000000000, -0.000000000000000000 ) ) ;
#2323 = CARTESIAN_POINT ( 'NONE',  ( 0.3474126878361875614, -11.61929161290143675, -3.953748424960759067 ) ) ;
#2324 = DIRECTION ( 'NONE',  ( 0.000000000000000000, 0.07632122047556495759, -0.9970832820307038435 ) ) ;
#2325 = ORIENTED_EDGE ( 'NONE', *, *, #25207, .T. ) ;
#2326 = CARTESIAN_POINT ( 'NONE',  ( 2.963017218115622242, -7.259628195185911181, -3.051711603120605520 ) ) ;
#2327 = CIRCLE ( 'NONE', #63862, 12.18650000000000055 ) ;
#2328 = EDGE_CURVE ( 'NONE', #51491, #51616, #5770, .T. ) ;
#2329 = ORIENTED_EDGE ( 'NONE', *, *, #24038, .F. ) ;
#2330 = CARTESIAN_POINT ( 'NONE',  ( 0.3654063281920728601, 10.76363796011285068, 5.910280591919091719 ) ) ;
#2331 = CARTESIAN_POINT ( 'NONE',  ( 2.268878695253351729, 5.949442550447466616, -4.798796461777989464 ) ) ;
#2332 = CARTESIAN_POINT ( 'NONE',  ( 12.25434804473628247, -13.17050011957374878, -2.969510513515200678 ) ) ;
#2333 = AXIS2_PLACEMENT_3D ( 'NONE', #2318, #52845, #48524 ) ;
#2335 = AXIS2_PLACEMENT_3D ( 'NONE', #7078, #53299, #42629 ) ;
#2334 = CARTESIAN_POINT ( 'NONE',  ( 0.000000000000000000, 0.000000000000000000, 0.000000000000000000 ) ) ;
#2336 = DIRECTION ( 'NONE',  ( 0.000000000000000000, -0.6051742151937558045, -0.7960930657056509707 ) ) ;
#2337 = ORIENTED_EDGE ( 'NONE', *, *, #54609, .F. ) ;
#2338 = CARTESIAN_POINT ( 'NONE',  ( -22.27722019117889474, -0.6494988092404023750, -3.623917154020615428 ) ) ;
#2339 = DIRECTION ( 'NONE',  ( 0.000000000000000000, 0.000000000000000000, 1.000000000000000000 ) ) ;
#2340 = B_SPLINE_CURVE_WITH_KNOTS ( 'NONE', 3,
 ( #23938, #38893, #9258, #64784, #33887, #8624 ),
 .UNSPECIFIED., .F., .F.,
 ( 4, 2, 4 ),
 ( 0.004238702544367933985, 0.006292126001073344854, 0.008345549457778756591 ),
 .UNSPECIFIED. ) ;
#2341 = CYLINDRICAL_SURFACE ( 'NONE', #29013, 12.75000000000000178 ) ;
#2342 = CARTESIAN_POINT ( 'NONE',  ( -4.007992427301752869, 10.70267137441327776, 8.237965989174103498 ) ) ;
#2343 = AXIS2_PLACEMENT_3D ( 'NONE', #42066, #43375, #6515 ) ;
#2344 = AXIS2_PLACEMENT_3D ( 'NONE', #27897, #6645, #37868 ) ;
#2345 = CYLINDRICAL_SURFACE ( 'NONE', #59473, 2.899999999999994582 ) ;
#2346 =( BOUNDED_SURFACE ( )  B_SPLINE_SURFACE ( 3, 1, ( 
 ( #940, #40508 ),
 ( #10571, #10248 ),
 ( #35180, #41828 ),
 ( #60805, #15243 ) ),
 .UNSPECIFIED., .F., .F., .F. ) 
 B_SPLINE_SURFACE_WITH_KNOTS ( ( 4, 4 ),
 ( 2, 2 ),
 ( 0.000000000000000000, 1.000000000000000000 ),
 ( 0.000000000000000000, 1.000000000000000000 ),
 .UNSPECIFIED. ) 
 GEOMETRIC_REPRESENTATION_ITEM ( )  RATIONAL_B_SPLINE_SURFACE ( (
 ( 1.000000000000000000, 1.000000000000000000),
 ( 0.6933888150995267674, 0.9895912004443193632),
 ( 0.6933888150995267674, 0.9895912004443193632),
 ( 1.000000000000000000, 1.000000000000000000) ) ) 
 REPRESENTATION_ITEM ( '' )  SURFACE ( )  );
#2347 = ORIENTED_EDGE ( 'NONE', *, *, #1361, .T. ) ;
#2348 = FACE_OUTER_BOUND ( 'NONE', #36031, .T. ) ;
#2350 = EDGE_CURVE ( 'NONE', #55613, #65690, #32260, .T. ) ;
#2349 = CARTESIAN_POINT ( 'NONE',  ( -8.868684597663976987, -31.89901926473304883, 13.46243262195112678 ) ) ;
#2351 = B_SPLINE_CURVE_WITH_KNOTS ( 'NONE', 3,
 ( #16438, #52674, #32031, #11745, #52351, #6790, #27065, #47357, #22063, #42319, #17073, #37352, #23382 ),
 .UNSPECIFIED., .F., .F.,
 ( 4, 3, 3, 3, 4 ),
 ( 2.453269466693398313E-18, 6.607593386745693668E-05, 0.0001321518677373556864, 0.0001982171734706220795, 0.0002642860854759481208 ),
 .UNSPECIFIED. ) ;
#2352 = AXIS2_PLACEMENT_3D ( 'NONE', #46510, #35850, #16256 ) ;
#2353 = EDGE_CURVE ( 'NONE', #8559, #36681, #30130, .T. ) ;
#2354 = AXIS2_PLACEMENT_3D ( 'NONE', #53205, #2698, #23941 ) ;
#2355 = EDGE_LOOP ( 'NONE', ( #59616, #36920, #42552, #1572 ) ) ;
#2357 = CARTESIAN_POINT ( 'NONE',  ( -7.181456785175555524, 5.890186129966279438, -10.45493698471458188 ) ) ;
#2356 = VECTOR ( 'NONE', #36667, 1000.000000000000000 ) ;
#2358 = ORIENTED_EDGE ( 'NONE', *, *, #39553, .T. ) ;
#2359 = FACE_OUTER_BOUND ( 'NONE', #61775, .T. ) ;
#2360 = CARTESIAN_POINT ( 'NONE',  ( 2.000000000000001776, -1.956810415765224187, 6.654767106875530303 ) ) ;
#2361 = CARTESIAN_POINT ( 'NONE',  ( 25.79281180259795292, -3.718204414137759262, 24.00000000000000355 ) ) ;
#2362 = CARTESIAN_POINT ( 'NONE',  ( -29.52025388906147541, -3.281486406648443044, 13.10044398286176559 ) ) ;
#2363 = CIRCLE ( 'NONE', #39501, 5.000000000000000000 ) ;
#2364 = CARTESIAN_POINT ( 'NONE',  ( -22.31213670151048944, -2.108126385153791471, -3.145266995071696936 ) ) ;
#2365 = ORIENTED_EDGE ( 'NONE', *, *, #45022, .T. ) ;
#2366 = AXIS2_PLACEMENT_3D ( 'NONE', #52693, #43023, #28390 ) ;
#2367 = ORIENTED_EDGE ( 'NONE', *, *, #58785, .F. ) ;
#2368 = ORIENTED_EDGE ( 'NONE', *, *, #20567, .F. ) ;
#2369 = CARTESIAN_POINT ( 'NONE',  ( 2.249013661412228693, 7.216565855998295476, -2.498855301843012633 ) ) ;
#2370 = EDGE_CURVE ( 'NONE', #48435, #47727, #23795, .T. ) ;
#2371 = ORIENTED_EDGE ( 'NONE', *, *, #33515, .F. ) ;
#2372 = CARTESIAN_POINT ( 'NONE',  ( 36.00000000000000711, -11.66664283989683604, -5.143145423404237526 ) ) ;
#2373 = AXIS2_PLACEMENT_3D ( 'NONE', #61023, #56020, #35404 ) ;
#2374 = CARTESIAN_POINT ( 'NONE',  ( 35.00000000000000000, 0.4993900848169179896, 12.17626345777662600 ) ) ;
#2375 = ORIENTED_EDGE ( 'NONE', *, *, #23711, .F. ) ;
#2376 = CARTESIAN_POINT ( 'NONE',  ( -22.27706485742869091, 0.9832726768967819941, -3.547445275915930285 ) ) ;
#2377 = CARTESIAN_POINT ( 'NONE',  ( 2.260457164927187623, -2.742969430850472179, -7.131443009846826442 ) ) ;
#2378 = CARTESIAN_POINT ( 'NONE',  ( 2.298277635560813881, 7.133696409974520591, 2.772101951899156536 ) ) ;
#2379 = EDGE_LOOP ( 'NONE', ( #45485, #48910, #61777, #48884 ) ) ;
#2380 = ORIENTED_EDGE ( 'NONE', *, *, #59871, .T. ) ;
#2381 = LINE ( 'NONE', #57244, #29962 ) ;
#2382 = ORIENTED_EDGE ( 'NONE', *, *, #28629, .F. ) ;
#2383 = CARTESIAN_POINT ( 'NONE',  ( 8.437200413559445167, 4.214301595845684645, -12.82835998935028776 ) ) ;
#2384 = ORIENTED_EDGE ( 'NONE', *, *, #27450, .F. ) ;
#2385 = AXIS2_PLACEMENT_3D ( 'NONE', #34946, #59937, #23119 ) ;
#2386 = CARTESIAN_POINT ( 'NONE',  ( 2.298277635560277421, 3.682855706290137032, 6.709004959608384944 ) ) ;
#2387 = DIRECTION ( 'NONE',  ( -1.000000000000000000, 0.000000000000000000, 0.000000000000000000 ) ) ;
#2388 = ADVANCED_FACE ( 'NONE', ( #16794 ), #54608, .T. ) ;
#2389 = DIRECTION ( 'NONE',  ( 0.000000000000000000, -0.7196168960969868689, -0.6943713148249562872 ) ) ;
#2390 = DIRECTION ( 'NONE',  ( 0.000000000000000000, -0.01356324068817998940, 0.9999080150203990547 ) ) ;
#2391 = DIRECTION ( 'NONE',  ( -0.3939253465568943735, -0.6978179301705798032, 0.5982248387291173586 ) ) ;
#2392 = CARTESIAN_POINT ( 'NONE',  ( 0.2638984909335716500, -6.295352574289060144, 10.50550771760518209 ) ) ;
#2393 = CARTESIAN_POINT ( 'NONE',  ( 3.347841273039249721, -10.61118957148187825, -5.603807266321158664 ) ) ;
#2394 = ORIENTED_EDGE ( 'NONE', *, *, #41950, .T. ) ;
#2395 = CARTESIAN_POINT ( 'NONE',  ( 3.152665057734040488, 0.000000000000000000, 0.000000000000000000 ) ) ;
#2396 = EDGE_LOOP ( 'NONE', ( #28433, #35547, #30639, #32533 ) ) ;
#2397 = CARTESIAN_POINT ( 'NONE',  ( -28.67667724226168602, 1.695959153103731465, 0.8389685652161870122 ) ) ;
#2398 = CYLINDRICAL_SURFACE ( 'NONE', #45760, 12.18650000000000055 ) ;
#2399 = EDGE_LOOP ( 'NONE', ( #12021, #54011, #25735, #54477 ) ) ;
#2400 = CARTESIAN_POINT ( 'NONE',  ( 2.524535260912720958, 7.335347545455701557, 2.434550409953099681 ) ) ;
#2401 = CARTESIAN_POINT ( 'NONE',  ( 0.2801149460245138112, 12.02936836014266220, -2.320387321174041784 ) ) ;
#2402 = CARTESIAN_POINT ( 'NONE',  ( -35.04683013664716640, -0.0001018103929411406472, -0.01235741808123163275 ) ) ;
#2403 = CIRCLE ( 'NONE', #33181, 6.936499999999989008 ) ;
#2404 = VERTEX_POINT ( 'NONE', #52719 ) ;
#2405 = VECTOR ( 'NONE', #14019, 1000.000000000000000 ) ;
#2406 = EDGE_LOOP ( 'NONE', ( #28324, #28630, #43642, #24421 ) ) ;
#2407 = CARTESIAN_POINT ( 'NONE',  ( -37.00000000000000711, -5.921969905510425569, 10.14408668126211488 ) ) ;
#2408 = EDGE_CURVE ( 'NONE', #63443, #41839, #57713, .T. ) ;
#2409 = VECTOR ( 'NONE', #52013, 1000.000000000000000 ) ;
#2410 = ORIENTED_EDGE ( 'NONE', *, *, #19134, .F. ) ;
#2411 = DIRECTION ( 'NONE',  ( 0.000000000000000000, -0.01356324068817998940, 0.9999080150203990547 ) ) ;
#2412 = CIRCLE ( 'NONE', #56560, 12.18649999999999878 ) ;
#2413 = CARTESIAN_POINT ( 'NONE',  ( -27.08418322526030408, 2.134267017050455184, 0.8335872080609374457 ) ) ;
#2414 = EDGE_CURVE ( 'NONE', #8430, #7261, #43305, .T. ) ;
#2415 = CARTESIAN_POINT ( 'NONE',  ( 2.350038591457886294, 10.55267716396152444, -1.210550722321003692 ) ) ;
#2416 = CARTESIAN_POINT ( 'NONE',  ( 2.000000000000001776, 3.786546189469266466, -5.663561025469129540 ) ) ;
#2417 = VERTEX_POINT ( 'NONE', #11797 ) ;
#2418 = CARTESIAN_POINT ( 'NONE',  ( -35.00000000000000000, 9.926225166347114381, -6.280308599560036065 ) ) ;
#2419 = EDGE_CURVE ( 'NONE', #45412, #12619, #55215, .T. ) ;
#2420 = CIRCLE ( 'NONE', #19356, 4.999999999999999112 ) ;
#2421 = CARTESIAN_POINT ( 'NONE',  ( 9.836964722002395689, -27.64452029744604644, -14.41904541651817873 ) ) ;
#2422 = CARTESIAN_POINT ( 'NONE',  ( 22.21243700998469350, 12.61357499758618772, -4.824052666793012811 ) ) ;
#2423 = CARTESIAN_POINT ( 'NONE',  ( 37.00000000000000711, -9.060822531525994705, 7.474872387601095625 ) ) ;
#2424 = CARTESIAN_POINT ( 'NONE',  ( 22.88594695219327235, -4.822122601967141264, 12.60940655271284427 ) ) ;
#2425 = ADVANCED_FACE ( 'NONE', ( #35755 ), #19838, .T. ) ;
#2426 = DIRECTION ( 'NONE',  ( -1.000000000000000000, 0.000000000000000000, -0.000000000000000000 ) ) ;
#2427 = CARTESIAN_POINT ( 'NONE',  ( -22.29382655386184453, -2.689927793811001333, -2.586160974799840417 ) ) ;
#2428 = CIRCLE ( 'NONE', #53399, 12.75000000000000178 ) ;
#2429 = CIRCLE ( 'NONE', #26809, 4.999999999999999112 ) ;
#2430 = AXIS2_PLACEMENT_3D ( 'NONE', #53108, #39109, #3235 ) ;
#2431 = CIRCLE ( 'NONE', #34264, 7.499999999999988454 ) ;
#2432 = ORIENTED_EDGE ( 'NONE', *, *, #10252, .T. ) ;
#2433 = CARTESIAN_POINT ( 'NONE',  ( -2.952869152607106251, 25.00000000000000000, 3.755417052241485365 ) ) ;
#2434 = CARTESIAN_POINT ( 'NONE',  ( 0.3002738374340838678, -12.25576345519757915, -0.2255758963752761692 ) ) ;
#2435 = ORIENTED_EDGE ( 'NONE', *, *, #47857, .F. ) ;
#2436 = LINE ( 'NONE', #28027, #11062 ) ;
#2437 = CARTESIAN_POINT ( 'NONE',  ( -22.46509356695200310, 3.157489876851330646, 2.840174833751751393 ) ) ;
#2438 = ORIENTED_EDGE ( 'NONE', *, *, #28088, .F. ) ;
#2439 = UNCERTAINTY_MEASURE_WITH_UNIT (LENGTH_MEASURE( 1.000000000000000082E-05 ), #30433, 'distance_accuracy_value', 'NONE');
#2440 = CARTESIAN_POINT ( 'NONE',  ( -35.00000000000000000, 4.603882218679707705, -10.80631716521661900 ) ) ;
#2441 = ORIENTED_EDGE ( 'NONE', *, *, #38364, .T. ) ;
#2442 = AXIS2_PLACEMENT_3D ( 'NONE', #13497, #39763, #55052 ) ;
#2443 = CARTESIAN_POINT ( 'NONE',  ( 37.00000000000000711, 4.074242145636174151, 12.08151691381185167 ) ) ;
#2444 = VERTEX_POINT ( 'NONE', #45112 ) ;
#2445 = VERTEX_POINT ( 'NONE', #25811 ) ;
#2446 = AXIS2_PLACEMENT_3D ( 'NONE', #8640, #54538, #58545 ) ;
#2447 = CARTESIAN_POINT ( 'NONE',  ( -22.49803948133827802, 0.1132714802761836531, 4.343047530463623573 ) ) ;
#2448 = VERTEX_POINT ( 'NONE', #55747 ) ;
#2449 = CARTESIAN_POINT ( 'NONE',  ( -35.00000000000000000, -9.926225166347071749, 6.280308599560108007 ) ) ;
#2450 = CARTESIAN_POINT ( 'NONE',  ( 3.598314112554458877, 4.116749633316167944, 12.86379551159408230 ) ) ;
#2451 = CARTESIAN_POINT ( 'NONE',  ( 22.57855258442564761, -4.427776684447072952, 25.00000000000000000 ) ) ;
#2452 = DIRECTION ( 'NONE',  ( 0.000000000000000000, 0.000000000000000000, 1.000000000000000000 ) ) ;
#2453 = ORIENTED_EDGE ( 'NONE', *, *, #32816, .F. ) ;
#2454 = DIRECTION ( 'NONE',  ( 6.123233995736778362E-17, -0.8660254037844380415, 0.5000000000000009992 ) ) ;
#2455 = AXIS2_PLACEMENT_3D ( 'NONE', #53253, #11362, #7700 ) ;
#2456 = CARTESIAN_POINT ( 'NONE',  ( 2.000000000000001776, 0.000000000000000000, 0.000000000000000000 ) ) ;
#2457 = CARTESIAN_POINT ( 'NONE',  ( 2.491965175174684521, -7.715025372671061810, 0.2120508241299217667 ) ) ;
#2459 = ORIENTED_EDGE ( 'NONE', *, *, #57575, .F. ) ;
#2458 = CARTESIAN_POINT ( 'NONE',  ( 12.51043607184429796, 0.3316456940255356201, -13.49694458083817672 ) ) ;
#2460 = DIRECTION ( 'NONE',  ( -1.000000000000000000, 0.000000000000000000, 0.000000000000000000 ) ) ;
#2461 = EDGE_LOOP ( 'NONE', ( #41703, #13045, #49058, #56258 ) ) ;
#2463 = EDGE_CURVE ( 'NONE', #11727, #14210, #30140, .T. ) ;
#2462 = CARTESIAN_POINT ( 'NONE',  ( 37.00000000000000711, 11.39945968423471534, -5.710938531231753323 ) ) ;
#2464 = ORIENTED_EDGE ( 'NONE', *, *, #55323, .T. ) ;
#2465 = CARTESIAN_POINT ( 'NONE',  ( 2.034671305879986125, 3.325478336154549019, 11.19279775165752788 ) ) ;
#2466 = FACE_OUTER_BOUND ( 'NONE', #17509, .T. ) ;
#2467 = DIRECTION ( 'NONE',  ( 0.000000000000000000, 0.000000000000000000, 1.000000000000000000 ) ) ;
#2468 = CARTESIAN_POINT ( 'NONE',  ( 0.2767916011545403787, -4.010899340181499184, 11.57477803659171478 ) ) ;
#2469 = ADVANCED_FACE ( 'NONE', ( #65045 ), #16121, .F. ) ;
#2470 = AXIS2_PLACEMENT_3D ( 'NONE', #20680, #41265, #25661 ) ;
#2471 = DIRECTION ( 'NONE',  ( 0.000000000000000000, 0.01356324068817998940, -0.9999080150203990547 ) ) ;
#2472 = DIRECTION ( 'NONE',  ( -1.000000000000000000, 0.000000000000000000, -0.000000000000000000 ) ) ;
#2473 = CARTESIAN_POINT ( 'NONE',  ( 13.41517466982755558, 12.56449639282538833, -4.957758779083538236 ) ) ;
#2474 = ORIENTED_EDGE ( 'NONE', *, *, #20938, .T. ) ;
#2475 = ORIENTED_EDGE ( 'NONE', *, *, #36230, .F. ) ;
#2476 = CARTESIAN_POINT ( 'NONE',  ( 0.2759803524722195811, 12.02930579076649664, 2.313459762622579685 ) ) ;
#2477 = ORIENTED_EDGE ( 'NONE', *, *, #26149, .F. ) ;
#2478 = AXIS2_PLACEMENT_3D ( 'NONE', #14581, #34555, #38906 ) ;
#2479 = VERTEX_POINT ( 'NONE', #50440 ) ;
#2481 = CIRCLE ( 'NONE', #60848, 12.18650000000000233 ) ;
#2480 = CARTESIAN_POINT ( 'NONE',  ( 19.13486214123186357, -6.258902428715801491, 11.96274114462062421 ) ) ;
#2482 = CARTESIAN_POINT ( 'NONE',  ( -22.28350523959501217, 3.346230442873243227, 1.580062893038950200 ) ) ;
#2483 = DIRECTION ( 'NONE',  ( 1.000000000000000000, 0.000000000000000000, -0.000000000000000000 ) ) ;
#2484 = B_SPLINE_CURVE_WITH_KNOTS ( 'NONE', 3,
 ( #64919, #60270, #53981, #8425, #24054, #19058 ),
 .UNSPECIFIED., .F., .F.,
 ( 4, 2, 4 ),
 ( 0.0001654224980408428632, 0.0006219428995476552254, 0.001078463301054467588 ),
 .UNSPECIFIED. ) ;
#2485 = CARTESIAN_POINT ( 'NONE',  ( -22.27878402819508352, 0.9624056734348347408, 3.558531829368139388 ) ) ;
#2486 = DIRECTION ( 'NONE',  ( -1.000000000000000000, 0.000000000000000000, 0.000000000000000000 ) ) ;
#2487 = CARTESIAN_POINT ( 'NONE',  ( -37.00000000000000711, -0.4353888892047496628, -11.73808581813438501 ) ) ;
#2488 = AXIS2_PLACEMENT_3D ( 'NONE', #35844, #4974, #31221 ) ;
#2489 = EDGE_CURVE ( 'NONE', #52527, #15712, #57782, .T. ) ;
#2490 = LINE ( 'NONE', #54339, #47208 ) ;
#2491 = ADVANCED_FACE ( 'NONE', ( #35448 ), #552, .T. ) ;
#2492 = EDGE_CURVE ( 'NONE', #7978, #11644, #55076, .T. ) ;
#2493 = EDGE_LOOP ( 'NONE', ( #46842, #4376, #48635, #47775 ) ) ;
#2494 = CIRCLE ( 'NONE', #9917, 5.000000000000000000 ) ;
#2495 = DIRECTION ( 'NONE',  ( -1.000000000000000000, 0.000000000000000000, 0.000000000000000000 ) ) ;
#2496 = ADVANCED_FACE ( 'NONE', ( #41084 ), #4216, .T. ) ;
#2497 = CARTESIAN_POINT ( 'NONE',  ( -35.00000000000000000, 0.000000000000000000, 0.000000000000000000 ) ) ;
#2498 = VECTOR ( 'NONE', #5951, 1000.000000000000000 ) ;
#2499 = CIRCLE ( 'NONE', #34317, 6.936499999999989896 ) ;
#2500 = CARTESIAN_POINT ( 'NONE',  ( 2.273267844204871047, -4.797225296800578853, 5.952585402747290644 ) ) ;
#2501 = FACE_OUTER_BOUND ( 'NONE', #39729, .T. ) ;
#2502 = DIRECTION ( 'NONE',  ( 0.000000000000000000, -0.4198891015602527754, -0.9075754196709624466 ) ) ;
#2503 = EDGE_CURVE ( 'NONE', #4743, #56025, #48873, .T. ) ;
#2504 = CIRCLE ( 'NONE', #57753, 5.000000000000000000 ) ;
#2505 = DIRECTION ( 'NONE',  ( -1.000000000000000000, 0.000000000000000000, 0.000000000000000000 ) ) ;
#2506 = EDGE_CURVE ( 'NONE', #21166, #40181, #46097, .T. ) ;
#2507 = VECTOR ( 'NONE', #995, 1000.000000000000000 ) ;
#2508 = CARTESIAN_POINT ( 'NONE',  ( 0.2648978790185593790, -0.1321385342563263510, 12.24533305150758089 ) ) ;
#2509 = VERTEX_POINT ( 'NONE', #36762 ) ;
#2510 = DIRECTION ( 'NONE',  ( 1.000000000000000000, 0.000000000000000000, 0.000000000000000000 ) ) ;
#2511 = DIRECTION ( 'NONE',  ( 0.000000000000000000, 0.01356324068817998940, -0.9999080150203990547 ) ) ;
#2512 = CARTESIAN_POINT ( 'NONE',  ( 32.00000000000000000, 1.230770033143089974E-14, 0.000000000000000000 ) ) ;
#2513 = CARTESIAN_POINT ( 'NONE',  ( 2.907497136251165237, -1.716624290781506135, -7.666666002096779842 ) ) ;
#2514 = CIRCLE ( 'NONE', #39659, 5.000000000000000000 ) ;
#2515 = ADVANCED_FACE ( 'NONE', ( #41405 ), #23720, .F. ) ;
#2516 = DIRECTION ( 'NONE',  ( -1.000000000000000000, 0.000000000000000000, -0.000000000000000000 ) ) ;
#2517 = CARTESIAN_POINT ( 'NONE',  ( 2.000000000000001776, 6.201547234537035713, 2.820401998297911383 ) ) ;
#2518 = EDGE_LOOP ( 'NONE', ( #38015, #52775, #11245, #28931 ) ) ;
#2519 = CARTESIAN_POINT ( 'NONE',  ( 17.54630545878690739, -9.526853237520755968, 7.355185947339629493 ) ) ;
#2520 = CARTESIAN_POINT ( 'NONE',  ( -35.00000000000000000, 0.000000000000000000, 0.000000000000000000 ) ) ;
#2521 = DIRECTION ( 'NONE',  ( -1.000000000000000000, 0.000000000000000000, 0.000000000000000000 ) ) ;
#2522 = CARTESIAN_POINT ( 'NONE',  ( 2.305787727787083519, 1.164987321564732392, 7.566723232958076473 ) ) ;
#2523 = ORIENTED_EDGE ( 'NONE', *, *, #45730, .F. ) ;
#2524 = DIRECTION ( 'NONE',  ( 0.000000000000000000, -1.000000000000000000, 0.000000000000000000 ) ) ;
#2525 = DIRECTION ( 'NONE',  ( 0.000000000000000000, 0.1387779952735747058, -0.9903235168508560671 ) ) ;
#2526 = ORIENTED_EDGE ( 'NONE', *, *, #49622, .T. ) ;
#2527 = AXIS2_PLACEMENT_3D ( 'NONE', #64911, #15366, #45966 ) ;
#2528 = VERTEX_POINT ( 'NONE', #51433 ) ;
#2529 = DIRECTION ( 'NONE',  ( -1.000000000000000000, 0.000000000000000000, 0.000000000000000000 ) ) ;
#2530 = CIRCLE ( 'NONE', #56693, 5.000000000000000000 ) ;
#2531 = CARTESIAN_POINT ( 'NONE',  ( -35.00000000000000000, 3.093009498344089447, -11.78745411414836930 ) ) ;
#2532 = VERTEX_POINT ( 'NONE', #15806 ) ;
#2533 = DIRECTION ( 'NONE',  ( 0.000000000000000000, -0.01356324068817999114, 0.9999080150203989437 ) ) ;
#2534 = DIRECTION ( 'NONE',  ( 0.000000000000000000, -0.01356324068817991828, 0.9999080150203990547 ) ) ;
#2536 = CARTESIAN_POINT ( 'NONE',  ( 0.000000000000000000, 6.997684042076905087, 2.698595569414227402 ) ) ;
#2535 =( BOUNDED_CURVE ( )  B_SPLINE_CURVE ( 3, ( #49702, #64636, #34062, #34402 ),
 .UNSPECIFIED., .F., .F. ) 
 B_SPLINE_CURVE_WITH_KNOTS ( ( 4, 4 ),
 ( 0.4559373747858286308, 0.4950834085599552514 ),
 .UNSPECIFIED. ) 
 CURVE ( )  GEOMETRIC_REPRESENTATION_ITEM ( )  RATIONAL_B_SPLINE_CURVE ( ( 1.000000000000000000, 0.9998723030801468514, 0.9998723030801468514, 1.000000000000000000 ) ) 
 REPRESENTATION_ITEM ( '' )  );
#2537 = CARTESIAN_POINT ( 'NONE',  ( 2.244591118396556340, -7.537402265771627086, -1.219892024449326762 ) ) ;
#2538 = CARTESIAN_POINT ( 'NONE',  ( -27.65886887683002726, 11.28192300254632663, -4.098983338605609816 ) ) ;
#2539 = VECTOR ( 'NONE', #28558, 1000.000000000000000 ) ;
#2540 = CARTESIAN_POINT ( 'NONE',  ( -37.00000000000000711, 0.000000000000000000, 0.000000000000000000 ) ) ;
#2542 = ORIENTED_EDGE ( 'NONE', *, *, #25059, .F. ) ;
#2541 = DIRECTION ( 'NONE',  ( 0.000000000000000000, 0.01356324068817992522, -0.9999080150203990547 ) ) ;
#2543 = CARTESIAN_POINT ( 'NONE',  ( 9.269227953188480029, 6.105058365070425097, 12.04509100434534652 ) ) ;
#2544 = ORIENTED_EDGE ( 'NONE', *, *, #14124, .F. ) ;
#2545 = CARTESIAN_POINT ( 'NONE',  ( 37.00000000000000711, 7.817492529713852889, -9.348667969174437431 ) ) ;
#2546 = VECTOR ( 'NONE', #7137, 1000.000000000000000 ) ;
#2547 = VERTEX_POINT ( 'NONE', #17137 ) ;
#2548 = EDGE_LOOP ( 'NONE', ( #555, #42906, #60473, #53029 ) ) ;
#2549 = CARTESIAN_POINT ( 'NONE',  ( -16.05148112979938091, 8.371939882860468529, 10.59070107784759962 ) ) ;
#2550 = CARTESIAN_POINT ( 'NONE',  ( -22.27722019094931483, 3.623977093944217298, -0.6491642780571648119 ) ) ;
#2551 = CARTESIAN_POINT ( 'NONE',  ( -27.19357181888462094, 12.48377454417557253, 5.138615876886901468 ) ) ;
#2552 = EDGE_CURVE ( 'NONE', #42135, #11634, #2171, .T. ) ;
#2553 = CARTESIAN_POINT ( 'NONE',  ( -41.38732981120779186, -1.602042930228848583, 17.55180477253565030 ) ) ;
#2554 = DIRECTION ( 'NONE',  ( 1.000000000000000000, -0.000000000000000000, 0.000000000000000000 ) ) ;
#2555 = ORIENTED_EDGE ( 'NONE', *, *, #39920, .F. ) ;
#2556 = CARTESIAN_POINT ( 'NONE',  ( 37.00000000000000711, 6.711949091238143872, -10.84030624090609152 ) ) ;
#2557 =( BOUNDED_SURFACE ( )  B_SPLINE_SURFACE ( 3, 1, ( 
 ( #37386, #12116 ),
 ( #32391, #27737 ),
 ( #27406, #47702 ),
 ( #22420, #42686 ) ),
 .UNSPECIFIED., .F., .F., .F. ) 
 B_SPLINE_SURFACE_WITH_KNOTS ( ( 4, 4 ),
 ( 2, 2 ),
 ( 0.000000000000000000, 1.000000000000000000 ),
 ( 0.000000000000000000, 1.000000000000000000 ),
 .UNSPECIFIED. ) 
 GEOMETRIC_REPRESENTATION_ITEM ( )  RATIONAL_B_SPLINE_SURFACE ( (
 ( 1.000000000000000000, 1.000000000000000000),
 ( 0.9257577194822556033, 0.9980522942447415113),
 ( 0.9257577194822556033, 0.9980522942447415113),
 ( 1.000000000000000000, 1.000000000000000000) ) ) 
 REPRESENTATION_ITEM ( '' )  SURFACE ( )  );
#2558 = DIRECTION ( 'NONE',  ( 1.000000000000000000, 0.000000000000000000, -0.000000000000000000 ) ) ;
#2560 = ORIENTED_EDGE ( 'NONE', *, *, #60361, .F. ) ;
#2559 = CARTESIAN_POINT ( 'NONE',  ( 2.000000000000001776, 3.805198749487436416, 5.799611601383225512 ) ) ;
#2561 = AXIS2_PLACEMENT_3D ( 'NONE', #19143, #40066, #50410 ) ;
#2562 = ORIENTED_EDGE ( 'NONE', *, *, #48987, .T. ) ;
#2563 = DIRECTION ( 'NONE',  ( -1.000000000000000000, 0.000000000000000000, 0.000000000000000000 ) ) ;
#2564 = VERTEX_POINT ( 'NONE', #26788 ) ;
#2565 = DIRECTION ( 'NONE',  ( -1.000000000000000000, 0.000000000000000000, 0.000000000000000000 ) ) ;
#2566 = CARTESIAN_POINT ( 'NONE',  ( -22.65996813707687707, 4.292955455498910666, -2.220979297960689713 ) ) ;
#2567 = CARTESIAN_POINT ( 'NONE',  ( 2.000000000000001776, 5.107597897712347290, 4.693343793638412365 ) ) ;
#2568 = CARTESIAN_POINT ( 'NONE',  ( -27.28573687977897677, -2.702109387930236473, 1.043905432732878946 ) ) ;
#2569 = CARTESIAN_POINT ( 'NONE',  ( 37.00000000000000711, -6.280308599560208371, -9.926225166347007800 ) ) ;
#2570 = CARTESIAN_POINT ( 'NONE',  ( -28.41827485489077532, 3.509237424706436403, 13.03592162821792222 ) ) ;
#2571 = AXIS2_PLACEMENT_3D ( 'NONE', #975, #61164, #56161 ) ;
#2572 = ADVANCED_FACE ( 'NONE', ( #62043 ), #10836, .T. ) ;
#2573 = LINE ( 'NONE', #50725, #18514 ) ;
#2574 = ORIENTED_EDGE ( 'NONE', *, *, #14124, .T. ) ;
#2575 = DIRECTION ( 'NONE',  ( -1.000000000000000000, -0.000000000000000000, -0.000000000000000000 ) ) ;
#2576 = ADVANCED_FACE ( 'NONE', ( #42063 ), #52725, .T. ) ;
#2577 = EDGE_LOOP ( 'NONE', ( #65321, #31343, #61697, #48279 ) ) ;
#2578 = CARTESIAN_POINT ( 'NONE',  ( 2.994568964204218808, 4.283796412555572530, -6.620406464816346315 ) ) ;
#2579 = EDGE_CURVE ( 'NONE', #14758, #35654, #35134, .T. ) ;
#2580 = DIRECTION ( 'NONE',  ( 0.000000000000000000, 0.01356324068818000848, -0.9999080150203990547 ) ) ;
#2581 = CARTESIAN_POINT ( 'NONE',  ( 2.524535260912187162, -2.850096701925626252, -7.184101064217829347 ) ) ;
#2582 = AXIS2_PLACEMENT_3D ( 'NONE', #22580, #42842, #37862 ) ;
#2583 = DIRECTION ( 'NONE',  ( -1.000000000000000000, 0.000000000000000000, 0.000000000000000000 ) ) ;
#2584 = VERTEX_POINT ( 'NONE', #1851 ) ;
#2585 = AXIS2_PLACEMENT_3D ( 'NONE', #57639, #36678, #56977 ) ;
#2586 = ORIENTED_EDGE ( 'NONE', *, *, #36253, .F. ) ;
#2587 = DIRECTION ( 'NONE',  ( -1.000000000000000000, 0.000000000000000000, -0.000000000000000000 ) ) ;
#2588 = AXIS2_PLACEMENT_3D ( 'NONE', #1029, #15966, #21296 ) ;
#2589 = EDGE_LOOP ( 'NONE', ( #35933, #7040, #52957, #50640 ) ) ;
#2590 = CARTESIAN_POINT ( 'NONE',  ( -35.00000000000000000, -9.621072037177055947, 8.366449238204328509 ) ) ;
#2591 = EDGE_CURVE ( 'NONE', #8602, #8461, #30871, .T. ) ;
#2592 = DIRECTION ( 'NONE',  ( -1.000000000000000000, -0.000000000000000000, 0.000000000000000000 ) ) ;
#2593 = CARTESIAN_POINT ( 'NONE',  ( 2.305787727787084407, 5.047606869483056258, 5.756228004061473946 ) ) ;
#2594 = CARTESIAN_POINT ( 'NONE',  ( 35.00000000000000000, 4.705694406421931860E-17, -3.469127814946512892E-15 ) ) ;
#2595 = EDGE_CURVE ( 'NONE', #35057, #40781, #8626, .T. ) ;
#2596 = ORIENTED_EDGE ( 'NONE', *, *, #4064, .F. ) ;
#2597 = CIRCLE ( 'NONE', #19571, 12.74999999999999822 ) ;
#2598 = CARTESIAN_POINT ( 'NONE',  ( 0.2653519789438758547, -6.142177718873863768, -10.59450269107740183 ) ) ;
#2599 = CARTESIAN_POINT ( 'NONE',  ( -22.27706089016750113, -2.622757446538683368, 2.583072118615359347 ) ) ;
#2600 = CARTESIAN_POINT ( 'NONE',  ( 0.2648978790185593790, -10.53870023327859151, -6.237101853238657512 ) ) ;
#2601 = CARTESIAN_POINT ( 'NONE',  ( -35.00000000000000000, 11.26103545359856106, -3.340853584269573684 ) ) ;
#2602 = EDGE_CURVE ( 'NONE', #51996, #19892, #7527, .T. ) ;
#2603 = CIRCLE ( 'NONE', #52479, 12.74999999999999822 ) ;
#2604 = EDGE_CURVE ( 'NONE', #3374, #31862, #32415, .T. ) ;
#2605 = CARTESIAN_POINT ( 'NONE',  ( 2.781367136452101541, -3.637318098960572677, 6.916275212954527518 ) ) ;
#2606 = DIRECTION ( 'NONE',  ( -0.3939253465568944290, 0.5982248387291196901, 0.6978179301705778048 ) ) ;
#2607 = ORIENTED_EDGE ( 'NONE', *, *, #908, .T. ) ;
#2608 = CARTESIAN_POINT ( 'NONE',  ( -27.08417568107324058, 1.774279301226123984, -1.449568724721373325 ) ) ;
#2610 = VECTOR ( 'NONE', #61883, 1000.000000000000000 ) ;
#2609 = CARTESIAN_POINT ( 'NONE',  ( 29.29356854117942177, 11.61667008512750598, 6.891473480132332519 ) ) ;
#2612 = EDGE_CURVE ( 'NONE', #39541, #30999, #6493, .T. ) ;
#2611 = CARTESIAN_POINT ( 'NONE',  ( -13.20530710592869283, -34.09051099065911217, -9.405657446765959051 ) ) ;
#2613 = ORIENTED_EDGE ( 'NONE', *, *, #45161, .T. ) ;
#2614 = CARTESIAN_POINT ( 'NONE',  ( -11.40165637462999548, -7.140361382672671731, -11.46568811481329320 ) ) ;
#2615 = CARTESIAN_POINT ( 'NONE',  ( 1.634816307076110586, -8.702988562439410103, 9.253014110594328656 ) ) ;
#2616 = DIRECTION ( 'NONE',  ( 1.000000000000000000, 0.000000000000000000, 0.000000000000000000 ) ) ;
#2617 = CARTESIAN_POINT ( 'NONE',  ( 0.2833330754217406322, -11.58086621621910517, 3.999965385632548553 ) ) ;
#2618 = CIRCLE ( 'NONE', #1519, 7.938172270156617749 ) ;
#2619 = ORIENTED_EDGE ( 'NONE', *, *, #60397, .T. ) ;
#2620 = ORIENTED_EDGE ( 'NONE', *, *, #53045, .F. ) ;
#2621 = CARTESIAN_POINT ( 'NONE',  ( 0.3053067050349203004, 1.901204202464671589, 12.11120005789971188 ) ) ;
#2622 = ORIENTED_EDGE ( 'NONE', *, *, #56044, .F. ) ;
#2623 = CARTESIAN_POINT ( 'NONE',  ( 34.00000000000000000, 1.267509437117510519E-14, 0.000000000000000000 ) ) ;
#2624 = CARTESIAN_POINT ( 'NONE',  ( 2.573738926104376379, 7.355212866432331076, -2.426778239006382343 ) ) ;
#2625 = CARTESIAN_POINT ( 'NONE',  ( 2.406456491624914484, 10.14681500356570432, -2.427896847127299029 ) ) ;
#2626 = CARTESIAN_POINT ( 'NONE',  ( -19.47984447937493613, -1.416020129149132334, 25.00000000000000000 ) ) ;
#2627 = CARTESIAN_POINT ( 'NONE',  ( 2.241537034860907163, -3.821322318518419969, 6.609284473755325351 ) ) ;
#2628 = CARTESIAN_POINT ( 'NONE',  ( 2.280717697723836590, 7.556934756535390818, 1.173604464351628573 ) ) ;
#2629 = DIRECTION ( 'NONE',  ( 1.000000000000000000, 0.000000000000000000, -0.000000000000000000 ) ) ;
#2630 = EDGE_LOOP ( 'NONE', ( #53656, #57220, #39139, #9933 ) ) ;
#2631 = CIRCLE ( 'NONE', #4763, 12.75000000000000178 ) ;
#2632 = VERTEX_POINT ( 'NONE', #52403 ) ;
#2633 = CIRCLE ( 'NONE', #48298, 6.936499999999989896 ) ;
#2634 = CARTESIAN_POINT ( 'NONE',  ( 5.514624014163232779, 0.003060352188290547774, -0.002789935220458479061 ) ) ;
#2635 = ORIENTED_EDGE ( 'NONE', *, *, #54269, .T. ) ;
#2636 = B_SPLINE_CURVE_WITH_KNOTS ( 'NONE', 3,
 ( #47547, #58180, #32879, #58864, #7636, #1992, #22608, #27575, #17288, #52859, #63469, #57867, #2679, #2331, #58517, #42523, #37218, #12281, #12946 ),
 .UNSPECIFIED., .F., .F.,
 ( 4, 3, 3, 3, 3, 3, 4 ),
 ( 0.000000000000000000, 2.831840207499475751E-05, 4.217266859840493434E-05, 5.602024318395896146E-05, 6.290810167969121175E-05, 9.120440630944927764E-05, 0.0001153103026479774721 ),
 .UNSPECIFIED. ) ;
#2637 = SURFACE_STYLE_FILL_AREA ( #47829 ) ;
#2638 = CARTESIAN_POINT ( 'NONE',  ( -22.28546858134833641, 2.587024666338670897, -2.654201075783116259 ) ) ;
#2639 = DIRECTION ( 'NONE',  ( 0.000000000000000000, 0.000000000000000000, -1.000000000000000000 ) ) ;
#2640 = EDGE_CURVE ( 'NONE', #57837, #60506, #33011, .T. ) ;
#2641 = DIRECTION ( 'NONE',  ( 0.000000000000000000, 0.7621620551276377942, -0.6473862847818260269 ) ) ;
#2642 = ORIENTED_EDGE ( 'NONE', *, *, #31297, .F. ) ;
#2643 = DIRECTION ( 'NONE',  ( 1.000000000000000000, 0.000000000000000000, -0.000000000000000000 ) ) ;
#2644 = CARTESIAN_POINT ( 'NONE',  ( -29.43980975494970309, -3.641506875706030488, 12.99959336572439561 ) ) ;
#2645 = CARTESIAN_POINT ( 'NONE',  ( 2.835339799623987300, -1.682641786445494336, 7.649567297875986327 ) ) ;
#2646 = ORIENTED_EDGE ( 'NONE', *, *, #13071, .F. ) ;
#2647 = ORIENTED_EDGE ( 'NONE', *, *, #17683, .T. ) ;
#2648 = CARTESIAN_POINT ( 'NONE',  ( 0.000000000000000000, 1.018311147294167274, 6.861346417234447159 ) ) ;
#2649 = ORIENTED_EDGE ( 'NONE', *, *, #13071, .T. ) ;
#2650 = DIRECTION ( 'NONE',  ( 0.000000000000000000, -1.000000000000000000, 0.000000000000000000 ) ) ;
#2651 = EDGE_CURVE ( 'NONE', #28214, #62051, #55328, .T. ) ;
#2652 = ORIENTED_EDGE ( 'NONE', *, *, #2214, .F. ) ;
#2653 = ORIENTED_EDGE ( 'NONE', *, *, #12034, .T. ) ;
#2654 = CARTESIAN_POINT ( 'NONE',  ( -22.27721038036499834, -2.858424446490929416, 2.320305412324230154 ) ) ;
#2655 = AXIS2_PLACEMENT_3D ( 'NONE', #36098, #10849, #41096 ) ;
#2656 = CARTESIAN_POINT ( 'NONE',  ( 2.241352910868908310, 4.970878533273838329, -5.794346703933798359 ) ) ;
#2657 = DIRECTION ( 'NONE',  ( -1.000000000000000000, 0.000000000000000000, 0.000000000000000000 ) ) ;
#2658 = CARTESIAN_POINT ( 'NONE',  ( 0.3106921474978480702, 8.060345844326409548, -9.239619355094065511 ) ) ;
#2659 = CARTESIAN_POINT ( 'NONE',  ( 35.00000000000000000, 9.060822531526046220, -7.474872387601039669 ) ) ;
#2660 = EDGE_CURVE ( 'NONE', #41862, #6306, #7153, .T. ) ;
#2661 = CARTESIAN_POINT ( 'NONE',  ( 0.3006302518452008132, 11.59403866275566131, 3.979421585299158348 ) ) ;
#2662 = ORIENTED_EDGE ( 'NONE', *, *, #40756, .F. ) ;
#2663 = DIRECTION ( 'NONE',  ( -1.000000000000000000, -0.000000000000000000, -0.000000000000000000 ) ) ;
#2664 = CARTESIAN_POINT ( 'NONE',  ( -22.27718112499583469, 2.901898111564464422, -2.265557025479496556 ) ) ;
#2665 = DIRECTION ( 'NONE',  ( -1.000000000000000000, 0.000000000000000000, 0.000000000000000000 ) ) ;
#2666 = ADVANCED_FACE ( 'NONE', ( #61694 ), #37287, .F. ) ;
#2667 = CARTESIAN_POINT ( 'NONE',  ( -22.27384469013076185, -3.358914544760244869, -1.508555848190776150 ) ) ;
#2668 = DIRECTION ( 'NONE',  ( -0.3939253465568943735, 0.8008152550167566552, 0.4511294145502791619 ) ) ;
#2669 = CARTESIAN_POINT ( 'NONE',  ( 35.00000000000000000, -0.7008968033239626472, -12.16632754454236576 ) ) ;
#2670 = FACE_OUTER_BOUND ( 'NONE', #15590, .T. ) ;
#2671 = DIRECTION ( 'NONE',  ( 1.000000000000000000, 0.000000000000000000, -0.000000000000000000 ) ) ;
#2672 = CARTESIAN_POINT ( 'NONE',  ( -27.31123137524929589, -10.57279367158372452, -8.394978051634900851 ) ) ;
#2673 = VECTOR ( 'NONE', #38869, 1000.000000000000000 ) ;
#2674 = EDGE_LOOP ( 'NONE', ( #5927, #12896, #37205, #6932 ) ) ;
#2675 = B_SPLINE_CURVE_WITH_KNOTS ( 'NONE', 3,
 ( #45573, #51251, #6031, #46900, #56896, #10013, #15326, #15637, #30294, #11320, #35264, #35907, #50591, #25628, #60541, #1359 ),
 .UNSPECIFIED., .F., .F.,
 ( 4, 3, 3, 3, 3, 4 ),
 ( 0.000000000000000000, 0.0002176109881720219913, 0.0004352086762394580103, 0.0006528017811446826290, 0.0007615147961451645790, 0.0009453342004946926110 ),
 .UNSPECIFIED. ) ;
#2676 = DIRECTION ( 'NONE',  ( 0.000000000000000000, 0.9847383929261624980, -0.1740410799127578012 ) ) ;
#2677 = ORIENTED_EDGE ( 'NONE', *, *, #40477, .F. ) ;
#2678 = CARTESIAN_POINT ( 'NONE',  ( -11.40165637463000436, -7.977372332587114201, 8.984547431638254977 ) ) ;
#2679 = CARTESIAN_POINT ( 'NONE',  ( 2.262775599886255762, 5.943524836196993455, -4.802882839669003978 ) ) ;
#2680 = DIRECTION ( 'NONE',  ( -1.000000000000000000, 0.000000000000000000, 0.000000000000000000 ) ) ;
#2681 = CARTESIAN_POINT ( 'NONE',  ( -22.27706485742869091, -2.985151051101489372, 2.154081322712201096 ) ) ;
#2682 = CARTESIAN_POINT ( 'NONE',  ( 3.152665057734130638, -4.725420687650661478, -6.378477742800524375 ) ) ;
#2683 = ORIENTED_EDGE ( 'NONE', *, *, #3424, .T. ) ;
#2684 =( GEOMETRIC_REPRESENTATION_CONTEXT ( 3 ) GLOBAL_UNCERTAINTY_ASSIGNED_CONTEXT ( ( #8334 ) ) GLOBAL_UNIT_ASSIGNED_CONTEXT ( ( #22219, #27215, #7937 ) ) REPRESENTATION_CONTEXT ( 'NONE', 'WORKASPACE' ) );
#2685 = CARTESIAN_POINT ( 'NONE',  ( 1.459561108994217093, 10.62073135189165285, -6.861308540878105156 ) ) ;
#2686 = CARTESIAN_POINT ( 'NONE',  ( -35.00000000000000000, 0.000000000000000000, 0.000000000000000000 ) ) ;
#2687 = LINE ( 'NONE', #43870, #355 ) ;
#2688 = CARTESIAN_POINT ( 'NONE',  ( 0.2653519789438763543, -2.148225749114911487, -12.05632450344285012 ) ) ;
#2689 = EDGE_CURVE ( 'NONE', #20437, #55446, #54310, .T. ) ;
#2690 = B_SPLINE_CURVE_WITH_KNOTS ( 'NONE', 3,
 ( #28970, #54248, #8687, #43938, #50247, #49278, #29599, #45240, #49589, #3393, #19966, #39916, #9643, #60200, #44561, #23663, #4706, #39594, #65497 ),
 .UNSPECIFIED., .F., .F.,
 ( 4, 3, 3, 3, 3, 3, 4 ),
 ( 1.164142361166801473E-17, 4.457896483014695525E-05, 6.639290541541897374E-05, 8.820687556478713819E-05, 0.0001100173248778907168, 0.0001545671401658091479, 0.0001830328308068564897 ),
 .UNSPECIFIED. ) ;
#2691 = EDGE_CURVE ( 'NONE', #29107, #17242, #13445, .T. ) ;
#2692 = DIRECTION ( 'NONE',  ( 0.000000000000000000, -0.01356324068817998940, 0.9999080150203990547 ) ) ;
#2693 = CIRCLE ( 'NONE', #21753, 6.936499999999989008 ) ;
#2694 = ORIENTED_EDGE ( 'NONE', *, *, #462, .T. ) ;
#2696 = ADVANCED_FACE ( 'NONE', ( #43051 ), #18125, .T. ) ;
#2695 = CARTESIAN_POINT ( 'NONE',  ( 3.092491956585210477, -0.4473002062004609036, -7.905533744258606887 ) ) ;
#2697 = DIRECTION ( 'NONE',  ( -1.000000000000000000, 0.000000000000000000, 0.000000000000000000 ) ) ;
#2698 = DIRECTION ( 'NONE',  ( 1.000000000000000000, 0.000000000000000000, 0.000000000000000000 ) ) ;
#2699 = AXIS2_PLACEMENT_3D ( 'NONE', #64569, #33007, #39647 ) ;
#2700 = ORIENTED_EDGE ( 'NONE', *, *, #12386, .F. ) ;
#2701 = DIRECTION ( 'NONE',  ( 0.000000000000000000, -0.9467777615094604693, -0.3218879778915876289 ) ) ;
#2702 = ORIENTED_EDGE ( 'NONE', *, *, #47798, .T. ) ;
#2703 = CARTESIAN_POINT ( 'NONE',  ( -18.01337138201670030, 3.271325267346269161, 11.54736685641333160 ) ) ;
#2704 = DIRECTION ( 'NONE',  ( -1.000000000000000000, 0.000000000000000000, 0.000000000000000000 ) ) ;
#2705 = CARTESIAN_POINT ( 'NONE',  ( 36.00000000000000711, 7.882940143791775434, -10.02106554660711701 ) ) ;
#2706 = DIRECTION ( 'NONE',  ( 0.000000000000000000, 0.000000000000000000, 1.000000000000000000 ) ) ;
#2707 = CARTESIAN_POINT ( 'NONE',  ( -22.28482751661422512, -2.105139449411421282, -3.048214341614495559 ) ) ;
#2708 = ORIENTED_EDGE ( 'NONE', *, *, #49696, .T. ) ;
#2709 = ORIENTED_EDGE ( 'NONE', *, *, #4391, .T. ) ;
#2710 = ORIENTED_EDGE ( 'NONE', *, *, #39070, .T. ) ;
#2711 = CARTESIAN_POINT ( 'NONE',  ( -42.50000000000000000, 1.443454975684918283E-16, -1.399999999999999911 ) ) ;
#2712 = AXIS2_PLACEMENT_3D ( 'NONE', #43683, #48380, #14076 ) ;
#2713 = CYLINDRICAL_SURFACE ( 'NONE', #41655, 12.74999999999999822 ) ;
#2714 = EDGE_CURVE ( 'NONE', #45191, #35989, #40850, .T. ) ;
#2715 = ORIENTED_EDGE ( 'NONE', *, *, #55077, .F. ) ;
#2716 = CARTESIAN_POINT ( 'NONE',  ( 35.00000000000000000, 4.705694406421931860E-17, -3.469127814946512892E-15 ) ) ;
#2717 = CARTESIAN_POINT ( 'NONE',  ( -22.31099767395441091, -0.2534174342804020874, -3.774495463598473766 ) ) ;
#2718 = EDGE_CURVE ( 'NONE', #29384, #11130, #33416, .T. ) ;
#2719 = EDGE_LOOP ( 'NONE', ( #32378, #45023, #65484, #60596 ) ) ;
#2720 = FACE_OUTER_BOUND ( 'NONE', #7014, .T. ) ;
#2721 = CARTESIAN_POINT ( 'NONE',  ( 0.000000000000000000, 0.000000000000000000, 0.000000000000000000 ) ) ;
#2722 = DIRECTION ( 'NONE',  ( 1.000000000000000000, 0.000000000000000000, -0.000000000000000000 ) ) ;
#2723 = ORIENTED_EDGE ( 'NONE', *, *, #63965, .F. ) ;
#2724 = ORIENTED_EDGE ( 'NONE', *, *, #48916, .T. ) ;
#2725 = CARTESIAN_POINT ( 'NONE',  ( 35.00000000000000000, 11.07407352312218052, 3.916263239775223504 ) ) ;
#2726 = ORIENTED_EDGE ( 'NONE', *, *, #3503, .T. ) ;
#2727 = EDGE_LOOP ( 'NONE', ( #27679, #35001, #15455, #28749 ) ) ;
#2728 = CARTESIAN_POINT ( 'NONE',  ( 9.222597103870787905, 1.921402420396019828, -13.36471210326569725 ) ) ;
#2729 = EDGE_LOOP ( 'NONE', ( #58236, #27164, #39804, #57675 ) ) ;
#2730 = EDGE_CURVE ( 'NONE', #9320, #16904, #18178, .T. ) ;
#2731 = CARTESIAN_POINT ( 'NONE',  ( 2.305787727787083519, 3.682701754025512919, 6.711944854845837583 ) ) ;
#2732 = CARTESIAN_POINT ( 'NONE',  ( 35.00000000000000000, 4.705694406421931860E-17, -3.469127814946512892E-15 ) ) ;
#2733 = FACE_OUTER_BOUND ( 'NONE', #18156, .T. ) ;
#2734 = CARTESIAN_POINT ( 'NONE',  ( 0.5547464869798248710, 11.49049644196208853, -4.506704303875337381 ) ) ;
#2735 = CARTESIAN_POINT ( 'NONE',  ( 0.7446945582518830209, -0.3561743995936043627, 12.40088838629986157 ) ) ;
#2736 = CARTESIAN_POINT ( 'NONE',  ( -27.28559572956275758, -11.69480911083762642, -2.740757448209772740 ) ) ;
#2737 = ORIENTED_EDGE ( 'NONE', *, *, #63333, .T. ) ;
#2738 = CARTESIAN_POINT ( 'NONE',  ( 0.5547464869798232057, 10.83828453080465160, 5.905377260991259369 ) ) ;
#2739 = VECTOR ( 'NONE', #36907, 1000.000000000000000 ) ;
#2740 = ORIENTED_EDGE ( 'NONE', *, *, #51926, .T. ) ;
#2741 = CARTESIAN_POINT ( 'NONE',  ( 2.249013661412229137, -2.724484898587339110, 7.134443398813868242 ) ) ;
#2742 = CARTESIAN_POINT ( 'NONE',  ( 2.266490820341523715, 6.690312181903024680, 3.694838443753504453 ) ) ;
#2743 = ADVANCED_FACE ( 'NONE', ( #53712 ), #34054, .T. ) ;
#2744 = ADVANCED_FACE ( 'NONE', ( #8145 ), #49397, .T. ) ;
#2745 = ORIENTED_EDGE ( 'NONE', *, *, #1284, .T. ) ;
#2746 = CYLINDRICAL_SURFACE ( 'NONE', #2050, 12.74999999999999822 ) ;
#2747 = CARTESIAN_POINT ( 'NONE',  ( 0.3223008802179221921, 6.343104382804310326, 10.49760329338521458 ) ) ;
#2748 = CARTESIAN_POINT ( 'NONE',  ( -22.28506771379528573, 2.697635452840769332, 2.571716811880536024 ) ) ;
#2749 = ADVANCED_FACE ( 'NONE', ( #44048 ), #13130, .T. ) ;
#2750 = CIRCLE ( 'NONE', #50521, 12.75000000000000178 ) ;
#2751 = ORIENTED_EDGE ( 'NONE', *, *, #20214, .T. ) ;
#2752 = VERTEX_POINT ( 'NONE', #33729 ) ;
#2753 = CYLINDRICAL_SURFACE ( 'NONE', #31137, 6.936499999999988120 ) ;
#2754 =( BOUNDED_SURFACE ( )  B_SPLINE_SURFACE ( 3, 1, ( 
 ( #53795, #1624 ),
 ( #6930, #63103 ),
 ( #27515, #27862 ),
 ( #2271, #53128 ) ),
 .UNSPECIFIED., .F., .F., .F. ) 
 B_SPLINE_SURFACE_WITH_KNOTS ( ( 4, 4 ),
 ( 2, 2 ),
 ( 0.000000000000000000, 1.000000000000000000 ),
 ( 0.000000000000000000, 1.000000000000000000 ),
 .UNSPECIFIED. ) 
 GEOMETRIC_REPRESENTATION_ITEM ( )  RATIONAL_B_SPLINE_SURFACE ( (
 ( 1.000000000000000000, 1.000000000000000000),
 ( 0.6933888150995267674, 0.9895912004443193632),
 ( 0.6933888150995267674, 0.9895912004443193632),
 ( 1.000000000000000000, 1.000000000000000000) ) ) 
 REPRESENTATION_ITEM ( '' )  SURFACE ( )  );
#2755 = VERTEX_POINT ( 'NONE', #38057 ) ;
#2756 = CARTESIAN_POINT ( 'NONE',  ( 1.719304012341432264, 5.066286238787408358, -11.67935079956426847 ) ) ;
#2757 = CARTESIAN_POINT ( 'NONE',  ( -3.191454007415039040, -11.27527210208590347, 4.125543110481471487 ) ) ;
#2758 = CARTESIAN_POINT ( 'NONE',  ( -27.08417473062937120, 2.166271322019585277, 0.7460375461499114680 ) ) ;
#2759 = CARTESIAN_POINT ( 'NONE',  ( -35.00000000000000000, -8.352657516904613999, -8.258652103341526995 ) ) ;
#2760 = CARTESIAN_POINT ( 'NONE',  ( -18.01369897008283161, -9.089080147352223804, 7.856079936729432056 ) ) ;
#2761 = ORIENTED_EDGE ( 'NONE', *, *, #12161, .F. ) ;
#2762 = CARTESIAN_POINT ( 'NONE',  ( -47.00000000000000711, 0.000000000000000000, 0.000000000000000000 ) ) ;
#2763 = EDGE_CURVE ( 'NONE', #4753, #63287, #55915, .T. ) ;
#2764 = AXIS2_PLACEMENT_3D ( 'NONE', #12947, #33874, #28247 ) ;
#2765 = EDGE_CURVE ( 'NONE', #49572, #57602, #26663, .T. ) ;
#2766 = CARTESIAN_POINT ( 'NONE',  ( 2.022082860508893187, -26.59007814299271999, -16.17076096363556914 ) ) ;
#2767 = CARTESIAN_POINT ( 'NONE',  ( 22.36482863261543486, 13.46837713145128923, -0.9234811557364158707 ) ) ;
#2768 = CARTESIAN_POINT ( 'NONE',  ( 5.536195898058073439, 0.007485416011288106679, 0.004027525919832979431 ) ) ;
#2769 = LINE ( 'NONE', #64542, #10188 ) ;
#2770 = CARTESIAN_POINT ( 'NONE',  ( 0.4626703367447424498, -3.943760108616721549, -11.66326339726751016 ) ) ;
#2771 = CIRCLE ( 'NONE', #17659, 1.399999999999999911 ) ;
#2772 = ORIENTED_EDGE ( 'NONE', *, *, #17105, .F. ) ;
#2773 = CARTESIAN_POINT ( 'NONE',  ( -25.42680463514451716, 1.651747791411784627, 3.516354806212989459 ) ) ;
#2774 = AXIS2_PLACEMENT_3D ( 'NONE', #11467, #1528, #12126 ) ;
#2775 = ORIENTED_EDGE ( 'NONE', *, *, #59116, .T. ) ;
#2776 = LINE ( 'NONE', #64550, #2405 ) ;
#2777 = CARTESIAN_POINT ( 'NONE',  ( -27.10719052120871098, -1.310802520592025955, -1.962717903527680718 ) ) ;
#2778 = CARTESIAN_POINT ( 'NONE',  ( 1.719304012340734378, -7.017415949613340587, -10.62216384465587282 ) ) ;
#2779 = ORIENTED_EDGE ( 'NONE', *, *, #24683, .T. ) ;
#2780 = CARTESIAN_POINT ( 'NONE',  ( -35.00000000000000000, -11.16627499335652374, -3.645068577060142978 ) ) ;
#2781 = ORIENTED_EDGE ( 'NONE', *, *, #56167, .F. ) ;
#2782 = CARTESIAN_POINT ( 'NONE',  ( 2.000000000000001776, -6.164400007374764456, -2.900694413976575792 ) ) ;
#2783 = ORIENTED_EDGE ( 'NONE', *, *, #473, .F. ) ;
#2784 = ORIENTED_EDGE ( 'NONE', *, *, #15216, .T. ) ;
#2785 = CARTESIAN_POINT ( 'NONE',  ( 29.52102924165219378, -11.15227936632555483, 7.620086186309502629 ) ) ;
#2786 = VECTOR ( 'NONE', #40970, 1000.000000000000000 ) ;
#2787 = CARTESIAN_POINT ( 'NONE',  ( 2.247112776671468026, -7.135103076758469776, 2.720990995225279985 ) ) ;
#2788 = VERTEX_POINT ( 'NONE', #13764 ) ;
#2789 = CARTESIAN_POINT ( 'NONE',  ( 2.373367633546871414, 5.764146204907464544, 5.072743978105256346 ) ) ;
#2790 = CARTESIAN_POINT ( 'NONE',  ( -27.45775109278351067, 8.499184579339635448, -8.471355351200609007 ) ) ;
#2791 = CYLINDRICAL_SURFACE ( 'NONE', #9983, 6.936499999999988120 ) ;
#2792 = CARTESIAN_POINT ( 'NONE',  ( 37.00000000000000711, -5.636262487437393887, -10.80478261802180207 ) ) ;
#2793 = EDGE_CURVE ( 'NONE', #56080, #29748, #47889, .T. ) ;
#2794 = VERTEX_POINT ( 'NONE', #12455 ) ;
#2795 = DIRECTION ( 'NONE',  ( -1.000000000000000000, -0.000000000000000000, 0.000000000000000000 ) ) ;
#2796 = DIRECTION ( 'NONE',  ( 1.000000000000000000, 0.000000000000000000, -0.000000000000000000 ) ) ;
#2797 = CARTESIAN_POINT ( 'NONE',  ( 2.000000000000001776, 4.472310526050767621, 6.020667617347370104 ) ) ;
#2799 = ORIENTED_EDGE ( 'NONE', *, *, #59038, .T. ) ;
#2798 = CARTESIAN_POINT ( 'NONE',  ( -25.29775422704755172, 10.32001691524481402, 6.125646727044483875 ) ) ;
#2800 = DIRECTION ( 'NONE',  ( -0.000000000000000000, -1.000000000000000000, -0.000000000000000000 ) ) ;
#2801 = VERTEX_POINT ( 'NONE', #35364 ) ;
#2802 = DIRECTION ( 'NONE',  ( 1.000000000000000000, 0.000000000000000000, 0.000000000000000000 ) ) ;
#2803 = VERTEX_POINT ( 'NONE', #19770 ) ;
#2804 = CARTESIAN_POINT ( 'NONE',  ( 37.00000000000000711, 11.10408318471059452, -6.265926637539536159 ) ) ;
#2805 = CARTESIAN_POINT ( 'NONE',  ( 0.2834382757448014045, 3.999440312567370537, -11.58108645293227035 ) ) ;
#2806 = DIRECTION ( 'NONE',  ( -1.000000000000000000, 0.000000000000000000, 0.000000000000000000 ) ) ;
#2807 = CARTESIAN_POINT ( 'NONE',  ( 35.00000000000000000, -1.171570255487531131, -11.68758509253248157 ) ) ;
#2808 = EDGE_CURVE ( 'NONE', #39817, #40383, #60643, .T. ) ;
#2809 = CARTESIAN_POINT ( 'NONE',  ( 0.3057689695767511484, 9.538231270095108627, 7.702054583838497059 ) ) ;
#2810 = DIRECTION ( 'NONE',  ( 0.9486832985018465170, 0.000000000000000000, -0.3162277646628396943 ) ) ;
#2811 = CARTESIAN_POINT ( 'NONE',  ( 2.241526690369555652, -5.837196604699884439, 4.920579984890946612 ) ) ;
#2812 = ORIENTED_EDGE ( 'NONE', *, *, #59950, .F. ) ;
#2813 = FACE_OUTER_BOUND ( 'NONE', #29033, .T. ) ;
#2814 = ORIENTED_EDGE ( 'NONE', *, *, #43181, .T. ) ;
#2815 = EDGE_CURVE ( 'NONE', #14551, #6535, #14968, .T. ) ;
#2816 = EDGE_LOOP ( 'NONE', ( #50574, #6694, #16683, #18126 ) ) ;
#2817 = CARTESIAN_POINT ( 'NONE',  ( 35.00000000000000000, 11.74226168163341377, 0.3025107581129941048 ) ) ;
#2818 = B_SPLINE_CURVE_WITH_KNOTS ( 'NONE', 3,
 ( #64753, #4927, #35147, #39830, #24876, #20200, #29212, #5248, #45807, #14227, #268, #44813, #19226, #10220, #65093, #35493, #60436, #19567, #55790 ),
 .UNSPECIFIED., .F., .F.,
 ( 4, 3, 3, 3, 3, 3, 4 ),
 ( 6.759600587344757484E-18, 2.825908398831393172E-05, 4.208813692484047856E-05, 5.591713746943926768E-05, 6.279584083231935017E-05, 9.105792820296614086E-05, 0.0001153131102488857165 ),
 .UNSPECIFIED. ) ;
#2819 = CARTESIAN_POINT ( 'NONE',  ( -18.25240752046768833, -11.98742856354572339, 0.6375846530299378312 ) ) ;
#2820 = CARTESIAN_POINT ( 'NONE',  ( -27.10719052120871098, 2.261993590776037788, -0.6736837626858775963 ) ) ;
#2821 = CARTESIAN_POINT ( 'NONE',  ( 0.3675815128205894289, -10.50067073900656212, 6.367184624550128014 ) ) ;
#2822 = FACE_OUTER_BOUND ( 'NONE', #45449, .T. ) ;
#2823 = EDGE_CURVE ( 'NONE', #15607, #17370, #64856, .T. ) ;
#2824 = CARTESIAN_POINT ( 'NONE',  ( 2.241536586108912932, -7.519576125149797896, -1.319514354261274391 ) ) ;
#2825 = AXIS2_PLACEMENT_3D ( 'NONE', #6144, #26405, #1147 ) ;
#2826 = LINE ( 'NONE', #39017, #65216 ) ;
#2827 = AXIS2_PLACEMENT_3D ( 'NONE', #48964, #53285, #3085 ) ;
#2828 = ORIENTED_EDGE ( 'NONE', *, *, #34295, .T. ) ;
#2829 = CARTESIAN_POINT ( 'NONE',  ( 0.2638984909335716500, 2.322601104020825868, -12.02508546958694602 ) ) ;
#2830 = DIRECTION ( 'NONE',  ( 0.000000000000000000, 0.000000000000000000, 1.000000000000000000 ) ) ;
#2831 = FACE_OUTER_BOUND ( 'NONE', #40202, .T. ) ;
#2832 = EDGE_CURVE ( 'NONE', #2026, #5091, #45792, .T. ) ;
#2833 = CARTESIAN_POINT ( 'NONE',  ( -37.00000000000000711, 1.908798535168378274, 12.60630747491664039 ) ) ;
#2834 = DIRECTION ( 'NONE',  ( -1.000000000000000000, 0.000000000000000000, 0.000000000000000000 ) ) ;
#2835 = LINE ( 'NONE', #2151, #4428 ) ;
#2836 = CARTESIAN_POINT ( 'NONE',  ( -10.90165637462999548, -7.338442233538555293, 11.33311006114865016 ) ) ;
#2837 = ORIENTED_EDGE ( 'NONE', *, *, #58030, .F. ) ;
#2838 = CARTESIAN_POINT ( 'NONE',  ( 5.516018279890452902, 0.006629829924290974764, 0.001397286410094337149 ) ) ;
#2839 = CARTESIAN_POINT ( 'NONE',  ( 16.93394556191337230, -34.50000000000000000, 4.811904876957209254 ) ) ;
#2840 = CARTESIAN_POINT ( 'NONE',  ( 3.152665057733881504, -7.719888720907738922, -1.848755561851823881 ) ) ;
#2841 = EDGE_CURVE ( 'NONE', #10202, #44435, #31966, .T. ) ;
#2842 = DIRECTION ( 'NONE',  ( 1.000000000000000000, 0.000000000000000000, 0.000000000000000000 ) ) ;
#2843 = CARTESIAN_POINT ( 'NONE',  ( -24.79843077534458118, -10.56684401205973067, 8.408718480432709086 ) ) ;
#2844 = VERTEX_POINT ( 'NONE', #30054 ) ;
#2845 = CYLINDRICAL_SURFACE ( 'NONE', #288, 2.809571291727933851 ) ;
#2846 = CARTESIAN_POINT ( 'NONE',  ( 2.000000000000001776, 0.000000000000000000, 0.000000000000000000 ) ) ;
#2847 = CARTESIAN_POINT ( 'NONE',  ( 0.000000000000000000, 0.000000000000000000, -6.000000000000000888 ) ) ;
#2848 = EDGE_LOOP ( 'NONE', ( #49569, #20665, #41019, #53208 ) ) ;
#2849 = CARTESIAN_POINT ( 'NONE',  ( -37.00000000000000711, 0.000000000000000000, 0.000000000000000000 ) ) ;
#2850 = CARTESIAN_POINT ( 'NONE',  ( -37.00000000000000711, 10.91536515067641844, 4.339012074900148619 ) ) ;
#2851 = ORIENTED_EDGE ( 'NONE', *, *, #5754, .T. ) ;
#2852 = ORIENTED_EDGE ( 'NONE', *, *, #39819, .F. ) ;
#2853 = VECTOR ( 'NONE', #40637, 1000.000000000000000 ) ;
#2854 = CARTESIAN_POINT ( 'NONE',  ( -10.48620311856347875, -9.720786832536937538, 25.00000000000000000 ) ) ;
#2855 = AXIS2_PLACEMENT_3D ( 'NONE', #34707, #49703, #39720 ) ;
#2856 = ORIENTED_EDGE ( 'NONE', *, *, #10380, .F. ) ;
#2857 = CARTESIAN_POINT ( 'NONE',  ( 35.00000000000000000, 8.352657516904789858, 8.258652103341336925 ) ) ;
#2858 = DIRECTION ( 'NONE',  ( 0.000000000000000000, -0.01356324068817998940, 0.9999080150203990547 ) ) ;
#2859 = CARTESIAN_POINT ( 'NONE',  ( -35.00000000000000000, -7.474872387600942858, -9.060822531526127932 ) ) ;
#2860 = CARTESIAN_POINT ( 'NONE',  ( 2.242418902651938772, -7.535443599794972691, -1.227462051872218129 ) ) ;
#2861 = EDGE_CURVE ( 'NONE', #51096, #54376, #29715, .T. ) ;
#2862 = DIRECTION ( 'NONE',  ( 0.000000000000000000, 0.6745969609292664648, 0.7381862504171951000 ) ) ;
#2863 = EDGE_CURVE ( 'NONE', #13659, #64505, #45675, .T. ) ;
#2864 = CARTESIAN_POINT ( 'NONE',  ( 0.3002738374340840899, 5.932527270856402524, 10.72659044316165300 ) ) ;
#2866 = VERTEX_POINT ( 'NONE', #29398 ) ;
#2865 = DIRECTION ( 'NONE',  ( 0.000000000000000000, 0.000000000000000000, 1.000000000000000000 ) ) ;
#2867 = EDGE_CURVE ( 'NONE', #17595, #52959, #27700, .T. ) ;
#2868 = CARTESIAN_POINT ( 'NONE',  ( 9.582000644489843566, 6.678480302218151365, 11.73685885562068698 ) ) ;
#2869 = VERTEX_POINT ( 'NONE', #30695 ) ;
#2870 = CARTESIAN_POINT ( 'NONE',  ( 0.2851083653049504285, -0.4107471485392698018, -11.99296822225284131 ) ) ;
#2871 = VERTEX_POINT ( 'NONE', #25080 ) ;
#2872 = ORIENTED_EDGE ( 'NONE', *, *, #6828, .T. ) ;
#2873 = ITEM_DEFINED_TRANSFORMATION ( 'NONE', 'NONE', #9047,  #24966 ) ;
#2874 = CARTESIAN_POINT ( 'NONE',  ( -24.92192216651048042, 9.674054327626246064, 9.421735467875462788 ) ) ;
#2875 = CARTESIAN_POINT ( 'NONE',  ( -7.049735699850023352, -28.78059498260736504, 12.46475915493964415 ) ) ;
#2876 = FACE_OUTER_BOUND ( 'NONE', #28107, .T. ) ;
#2877 = ADVANCED_FACE ( 'NONE', ( #49695 ), #14738, .T. ) ;
#2878 = DIRECTION ( 'NONE',  ( -1.000000000000000000, -0.000000000000000000, -0.000000000000000000 ) ) ;
#2879 = CARTESIAN_POINT ( 'NONE',  ( -40.80553070818748296, -1.699139512677864561, 18.07784515657014168 ) ) ;
#2880 = CARTESIAN_POINT ( 'NONE',  ( -18.08686583997218733, 5.151216734910788908, 12.47858029384653733 ) ) ;
#2881 = EDGE_LOOP ( 'NONE', ( #38268, #60198, #62102, #14492 ) ) ;
#2882 = CARTESIAN_POINT ( 'NONE',  ( 37.00000000000000711, -0.06441628369827803735, 12.18632975068352309 ) ) ;
#2883 = CARTESIAN_POINT ( 'NONE',  ( -36.00000000000000711, -3.640372113593638659, 12.21925492305361161 ) ) ;
#2884 = DIRECTION ( 'NONE',  ( -1.000000000000000000, 0.000000000000000000, -0.000000000000000000 ) ) ;
#2885 = ORIENTED_EDGE ( 'NONE', *, *, #57234, .T. ) ;
#2886 = CARTESIAN_POINT ( 'NONE',  ( 0.000000000000000000, 7.493043167941616289, 0.3229614270519615693 ) ) ;
#2887 = ORIENTED_EDGE ( 'NONE', *, *, #65660, .F. ) ;
#2888 = CARTESIAN_POINT ( 'NONE',  ( 37.00000000000000711, 4.705694406421931860E-17, -3.469127814946512892E-15 ) ) ;
#2889 = CARTESIAN_POINT ( 'NONE',  ( 0.2648978790185593790, -10.53870023327859151, -6.237101853238657512 ) ) ;
#2890 = CARTESIAN_POINT ( 'NONE',  ( 0.3675815128205894289, 8.093875121226078662, 9.235491948680033758 ) ) ;
#2891 = DIRECTION ( 'NONE',  ( -1.000000000000000000, -0.000000000000000000, 0.000000000000000000 ) ) ;
#2892 = CARTESIAN_POINT ( 'NONE',  ( -35.00000000000000000, -6.917234959366895808, 9.493370459201672773 ) ) ;
#2893 = CARTESIAN_POINT ( 'NONE',  ( 22.88594695219327235, 3.421158645304719137, 25.00000000000000000 ) ) ;
#2894 = EDGE_CURVE ( 'NONE', #58474, #4846, #34698, .T. ) ;
#2895 = EDGE_LOOP ( 'NONE', ( #56832, #21515, #23366, #1932 ) ) ;
#2896 = CARTESIAN_POINT ( 'NONE',  ( -36.00000000000000711, -2.865935305911713638, 12.42372387097881514 ) ) ;
#2897 = CIRCLE ( 'NONE', #40021, 5.000000000000000888 ) ;
#2898 = ORIENTED_EDGE ( 'NONE', *, *, #18521, .F. ) ;
#2899 = CARTESIAN_POINT ( 'NONE',  ( 1.634816307075117159, 3.661851000131278511, 12.16351623921463343 ) ) ;
#2900 = CARTESIAN_POINT ( 'NONE',  ( -35.00000000000000000, 8.766823244862097297, -7.817610399097422835 ) ) ;
#2901 = CIRCLE ( 'NONE', #1841, 4.999999999999999112 ) ;
#2902 = CARTESIAN_POINT ( 'NONE',  ( 36.00000000000000711, -6.564808257521689505, 10.93004082984025160 ) ) ;
#2903 = CARTESIAN_POINT ( 'NONE',  ( -35.00000000000000000, -11.71932350927023414, 3.511386971104906163 ) ) ;
#2904 = LINE ( 'NONE', #42778, #6808 ) ;
#2905 = ORIENTED_EDGE ( 'NONE', *, *, #10978, .T. ) ;
#2906 = CARTESIAN_POINT ( 'NONE',  ( 0.2739690278137238422, 7.732471127692722490, -9.499928778897034576 ) ) ;
#2907 = CARTESIAN_POINT ( 'NONE',  ( -28.85619398320021745, 3.750539801530000439, -11.39883551934754280 ) ) ;
#2908 = CARTESIAN_POINT ( 'NONE',  ( 2.260457164927185847, 1.462935478981605586, 7.499412009325151729 ) ) ;
#2909 = FACE_OUTER_BOUND ( 'NONE', #53583, .T. ) ;
#2910 = ORIENTED_EDGE ( 'NONE', *, *, #37555, .T. ) ;
#2911 = CARTESIAN_POINT ( 'NONE',  ( 2.994568964204198824, 2.317954327151229954, 7.537093683963799862 ) ) ;
#2912 = CARTESIAN_POINT ( 'NONE',  ( -22.27706485742869091, -2.625261754997692876, 2.580541389029905819 ) ) ;
#2913 = CARTESIAN_POINT ( 'NONE',  ( 2.717984159220057538, -1.073093837952399321, 7.719081760284438154 ) ) ;
#2914 = CARTESIAN_POINT ( 'NONE',  ( -49.59714883329487378, -0.08190040965286676800, -4.488761805454715592 ) ) ;
#2915 = EDGE_CURVE ( 'NONE', #23899, #52056, #51122, .T. ) ;
#2916 = DIRECTION ( 'NONE',  ( -1.000000000000000000, 0.000000000000000000, 0.000000000000000000 ) ) ;
#2917 = DIRECTION ( 'NONE',  ( 0.000000000000000000, -0.9868265225415245867, -0.1617819965527747539 ) ) ;
#2918 =( BOUNDED_CURVE ( )  B_SPLINE_CURVE ( 3, ( #43238, #17986, #38247, #53582 ),
 .UNSPECIFIED., .F., .F. ) 
 B_SPLINE_CURVE_WITH_KNOTS ( ( 4, 4 ),
 ( 4.678153363932756825, 4.712388980384688786 ),
 .UNSPECIFIED. ) 
 CURVE ( )  GEOMETRIC_REPRESENTATION_ITEM ( )  RATIONAL_B_SPLINE_CURVE ( ( 1.000000000000000000, 0.9999023292654991568, 0.9999023292654991568, 1.000000000000000000 ) ) 
 REPRESENTATION_ITEM ( '' )  );
#2919 = EDGE_LOOP ( 'NONE', ( #1043, #44630, #41176, #13059 ) ) ;
#2920 = CARTESIAN_POINT ( 'NONE',  ( 37.00000000000000711, -10.93004082984022851, -6.564808257521734802 ) ) ;
#2921 = CARTESIAN_POINT ( 'NONE',  ( 35.00000000000000000, 4.705694406421931860E-17, -3.469127814946512892E-15 ) ) ;
#2922 = CARTESIAN_POINT ( 'NONE',  ( 5.516018279890452902, 0.003191189039764837348, 0.005976902763919047894 ) ) ;
#2923 = ORIENTED_EDGE ( 'NONE', *, *, #38317, .T. ) ;
#2924 = DIRECTION ( 'NONE',  ( 1.000000000000000000, -0.000000000000000000, -0.000000000000000000 ) ) ;
#2925 = CARTESIAN_POINT ( 'NONE',  ( 37.00000000000000711, -10.91072401419414462, -5.428340790341669830 ) ) ;
#2926 = CARTESIAN_POINT ( 'NONE',  ( 35.00000000000000000, 11.23004253107771078, 4.732539170486136371 ) ) ;
#2927 = CARTESIAN_POINT ( 'NONE',  ( 37.00000000000000711, 4.705694406421931860E-17, -3.469127814946512892E-15 ) ) ;
#2928 = CARTESIAN_POINT ( 'NONE',  ( 0.3223008802179222476, -11.43958962819736058, 4.423848692584651410 ) ) ;
#2929 = EDGE_CURVE ( 'NONE', #19851, #45626, #57484, .T. ) ;
#2930 = ORIENTED_EDGE ( 'NONE', *, *, #30564, .F. ) ;
#2931 = CARTESIAN_POINT ( 'NONE',  ( -35.00000000000000000, 9.557269938331666381, -7.561043153947866635 ) ) ;
#2932 = EDGE_LOOP ( 'NONE', ( #26415, #12554, #11118, #10219 ) ) ;
#2933 = DIRECTION ( 'NONE',  ( -1.000000000000000000, -1.836970198721029688E-16, -0.000000000000000000 ) ) ;
#2934 = CARTESIAN_POINT ( 'NONE',  ( 2.899286259009687061, 7.494390643303807664, -2.348384892629290732 ) ) ;
#2935 = CARTESIAN_POINT ( 'NONE',  ( 2.781367136452742805, -4.783057651000458321, 6.179587792204651819 ) ) ;
#2936 =( BOUNDED_CURVE ( )  B_SPLINE_CURVE ( 3, ( #23598, #43868, #14253, #49837 ),
 .UNSPECIFIED., .F., .F. ) 
 B_SPLINE_CURVE_WITH_KNOTS ( ( 4, 4 ),
 ( 0.7870380171267665759, 0.8138757160357118492 ),
 .UNSPECIFIED. ) 
 CURVE ( )  GEOMETRIC_REPRESENTATION_ITEM ( )  RATIONAL_B_SPLINE_CURVE ( ( 1.000000000000000000, 0.9999399790604226457, 0.9999399790604226457, 1.000000000000000000 ) ) 
 REPRESENTATION_ITEM ( '' )  );
#2937 = DIRECTION ( 'NONE',  ( 1.000000000000000000, -0.000000000000000000, 0.000000000000000000 ) ) ;
#2938 = CARTESIAN_POINT ( 'NONE',  ( -36.00000000000000711, -11.10408318471063893, 6.265926637539455335 ) ) ;
#2939 = EDGE_CURVE ( 'NONE', #44680, #17260, #17042, .T. ) ;
#2940 = CARTESIAN_POINT ( 'NONE',  ( 2.266490820343221912, -1.183790889241783439, 7.550546162186916987 ) ) ;
#2941 = CARTESIAN_POINT ( 'NONE',  ( 0.2638984909335716500, 7.718810690099061844, 9.508791614589220842 ) ) ;
#2942 = EDGE_LOOP ( 'NONE', ( #47407, #41244, #12232, #15298 ) ) ;
#2943 = ADVANCED_FACE ( 'NONE', ( #40346 ), #60644, .T. ) ;
#2944 = VERTEX_POINT ( 'NONE', #64966 ) ;
#2945 = SURFACE_STYLE_USAGE ( .BOTH. , #28849 ) ;
#2946 = ORIENTED_EDGE ( 'NONE', *, *, #22340, .T. ) ;
#2947 = VECTOR ( 'NONE', #29132, 1000.000000000000000 ) ;
#2948 = CARTESIAN_POINT ( 'NONE',  ( -22.27878402819508707, 2.600576127690929162, -2.612733676624897416 ) ) ;
#2949 = CARTESIAN_POINT ( 'NONE',  ( -27.10719052120871098, -0.1538293304135310291, -2.355164825213519109 ) ) ;
#2950 = AXIS2_PLACEMENT_3D ( 'NONE', #52012, #10777, #1802 ) ;
#2951 = ADVANCED_FACE ( 'NONE', ( #14425 ), #64629, .T. ) ;
#2952 = DIRECTION ( 'NONE',  ( 0.000000000000000000, -0.6051742151937555825, -0.7960930657056509707 ) ) ;
#2953 = ORIENTED_EDGE ( 'NONE', *, *, #22959, .F. ) ;
#2954 = DIRECTION ( 'NONE',  ( 0.000000000000000000, 0.01356324068818000848, -0.9999080150203990547 ) ) ;
#2955 = LINE ( 'NONE', #34164, #34793 ) ;
#2957 = ADVANCED_FACE ( 'NONE', ( #26375 ), #57302, .T. ) ;
#2956 = DIRECTION ( 'NONE',  ( 0.000000000000000000, 0.000000000000000000, 1.000000000000000000 ) ) ;
#2958 = ORIENTED_EDGE ( 'NONE', *, *, #53017, .F. ) ;
#2959 = ORIENTED_EDGE ( 'NONE', *, *, #35908, .T. ) ;
#2960 = DIRECTION ( 'NONE',  ( -1.000000000000000000, -0.000000000000000000, -0.000000000000000000 ) ) ;
#2961 = ORIENTED_EDGE ( 'NONE', *, *, #7551, .T. ) ;
#2962 = DIRECTION ( 'NONE',  ( -0.000000000000000000, -0.000000000000000000, -1.000000000000000000 ) ) ;
#2963 = ORIENTED_EDGE ( 'NONE', *, *, #9225, .F. ) ;
#2965 = EDGE_CURVE ( 'NONE', #42155, #13349, #34150, .T. ) ;
#2964 = ORIENTED_EDGE ( 'NONE', *, *, #20451, .T. ) ;
#2966 = CARTESIAN_POINT ( 'NONE',  ( 0.2646305136544072623, -6.008537389229345216, -10.67138229758235823 ) ) ;
#2967 = CARTESIAN_POINT ( 'NONE',  ( -35.00000000000000000, 0.000000000000000000, 0.000000000000000000 ) ) ;
#2968 = CARTESIAN_POINT ( 'NONE',  ( -27.08954555554413801, -2.300063521504145836, 0.1819824474943266546 ) ) ;
#2969 = DIRECTION ( 'NONE',  ( -1.000000000000000000, 0.000000000000000000, -0.000000000000000000 ) ) ;
#2970 = FACE_OUTER_BOUND ( 'NONE', #29494, .T. ) ;
#2971 = ADVANCED_FACE ( 'NONE', ( #27040 ), #47002, .T. ) ;
#2972 = DIRECTION ( 'NONE',  ( 0.000000000000000000, -0.01356324068817991828, 0.9999080150203990547 ) ) ;
#2973 = ORIENTED_EDGE ( 'NONE', *, *, #32600, .F. ) ;
#2974 = LINE ( 'NONE', #8269, #30672 ) ;
#2975 = CARTESIAN_POINT ( 'NONE',  ( -22.27722019094931483, 2.813874087060014517, -2.374181302998998877 ) ) ;
#2976 = EDGE_CURVE ( 'NONE', #6394, #47785, #29876, .T. ) ;
#2977 = CARTESIAN_POINT ( 'NONE',  ( 2.266490820343733947, 3.694838443752039403, -6.690312181904674915 ) ) ;
#2978 = DIRECTION ( 'NONE',  ( -1.000000000000000000, 0.000000000000000000, 0.000000000000000000 ) ) ;
#2979 = CARTESIAN_POINT ( 'NONE',  ( -18.04458733766117362, 12.91933584589294703, 3.916728392552376370 ) ) ;
#2980 = DIRECTION ( 'NONE',  ( 1.000000000000000000, 0.000000000000000000, 0.000000000000000000 ) ) ;
#2981 = CARTESIAN_POINT ( 'NONE',  ( -27.08418322526031119, 1.431535851194455145, 1.789041206975748199 ) ) ;
#2982 = CARTESIAN_POINT ( 'NONE',  ( 0.3610902822527282119, -11.62472836966321132, -3.951920836718837649 ) ) ;
#2983 = CARTESIAN_POINT ( 'NONE',  ( 0.6511581176955585359, 5.898618881004847658, 10.87850887236043818 ) ) ;
#2984 = AXIS2_PLACEMENT_3D ( 'NONE', #13475, #8495, #59372 ) ;
#2985 = ORIENTED_EDGE ( 'NONE', *, *, #22245, .F. ) ;
#2986 = CARTESIAN_POINT ( 'NONE',  ( 2.835339799623981527, -7.241165502254423458, -2.985412098050572283 ) ) ;
#2987 = B_SPLINE_CURVE_WITH_KNOTS ( 'NONE', 3,
 ( #25501, #64739, #49495, #40810, #61087, #15520, #19211, #39485, #59783, #14211, #34498, #32123, #6222, #57410, #1883, #5577, #47446, #893, #62704 ),
 .UNSPECIFIED., .F., .F.,
 ( 4, 3, 3, 3, 3, 3, 4 ),
 ( 5.587587132013241302E-18, 2.825908398831385041E-05, 4.208813692484114264E-05, 5.591713746944058905E-05, 6.279584083231968899E-05, 9.105792820296830926E-05, 0.0001153131102488871938 ),
 .UNSPECIFIED. ) ;
#2988 = ORIENTED_EDGE ( 'NONE', *, *, #46326, .F. ) ;
#2989 = CARTESIAN_POINT ( 'NONE',  ( -35.00000000000000000, 0.000000000000000000, 0.000000000000000000 ) ) ;
#2990 = CARTESIAN_POINT ( 'NONE',  ( 0.3002738374340847005, -0.2255758963752309276, 12.25576345519757204 ) ) ;
#2991 = CARTESIAN_POINT ( 'NONE',  ( 12.73187067999545263, -12.88776733229570759, -4.024014788385745334 ) ) ;
#2992 = CIRCLE ( 'NONE', #10402, 12.75000000000000178 ) ;
#2993 = DIRECTION ( 'NONE',  ( -1.000000000000000000, 0.000000000000000000, 0.000000000000000000 ) ) ;
#2994 = DIRECTION ( 'NONE',  ( -0.000000000000000000, -1.000000000000000000, -0.000000000000000000 ) ) ;
#2995 = VERTEX_POINT ( 'NONE', #41014 ) ;
#2996 = FACE_OUTER_BOUND ( 'NONE', #31978, .T. ) ;
#2997 = CARTESIAN_POINT ( 'NONE',  ( -35.00000000000000000, 0.000000000000000000, 0.000000000000000000 ) ) ;
#2998 = CARTESIAN_POINT ( 'NONE',  ( 3.152665057734040488, 0.000000000000000000, 0.000000000000000000 ) ) ;
#2999 = AXIS2_PLACEMENT_3D ( 'NONE', #45318, #35327, #55639 ) ;
#3000 = CARTESIAN_POINT ( 'NONE',  ( 16.78995969943013478, -34.48221411999237773, -5.258039666742740259 ) ) ;
#3001 = EDGE_CURVE ( 'NONE', #62601, #58400, #42628, .T. ) ;
#3002 = EDGE_CURVE ( 'NONE', #14430, #37563, #32339, .T. ) ;
#3003 = DIRECTION ( 'NONE',  ( 1.000000000000000000, 0.000000000000000000, -0.000000000000000000 ) ) ;
#3004 = ORIENTED_EDGE ( 'NONE', *, *, #26985, .F. ) ;
#3005 = CARTESIAN_POINT ( 'NONE',  ( -35.00000000000000000, -8.551552972817024312, -8.052525312709976291 ) ) ;
#3006 = FACE_OUTER_BOUND ( 'NONE', #47177, .T. ) ;
#3007 = CARTESIAN_POINT ( 'NONE',  ( -35.00000000000000000, 10.01317267707896441, -6.946017217729827387 ) ) ;
#3008 = ADVANCED_FACE ( 'NONE', ( #56663 ), #15727, .T. ) ;
#3009 = EDGE_CURVE ( 'NONE', #46698, #18117, #54352, .T. ) ;
#3010 = VERTEX_POINT ( 'NONE', #46023 ) ;
#3011 = ORIENTED_EDGE ( 'NONE', *, *, #23262, .F. ) ;
#3012 = CARTESIAN_POINT ( 'NONE',  ( 36.00000000000000711, 4.824807283154290971, 11.80185301892974969 ) ) ;
#3013 = ORIENTED_EDGE ( 'NONE', *, *, #11270, .F. ) ;
#3014 = CARTESIAN_POINT ( 'NONE',  ( 5.514970785353741078, 0.001117786416802556615, 0.004588761610585030681 ) ) ;
#3015 = CARTESIAN_POINT ( 'NONE',  ( 0.2648978790185584908, -10.67083876753496341, 6.008231198268946471 ) ) ;
#3016 = CARTESIAN_POINT ( 'NONE',  ( 35.00000000000000000, 11.95840593935204765, 2.346765782874299155 ) ) ;
#3018 = CARTESIAN_POINT ( 'NONE',  ( 35.00000000000000000, 11.61175578952788356, 1.771820996347031940 ) ) ;
#3017 = VECTOR ( 'NONE', #2565, 1000.000000000000000 ) ;
#3019 = DIRECTION ( 'NONE',  ( 0.000000000000000000, 0.01356324068817991828, -0.9999080150203990547 ) ) ;
#3020 = ORIENTED_EDGE ( 'NONE', *, *, #57969, .F. ) ;
#3021 = EDGE_CURVE ( 'NONE', #40781, #57018, #62826, .T. ) ;
#3022 = ORIENTED_EDGE ( 'NONE', *, *, #52424, .T. ) ;
#3023 = ORIENTED_EDGE ( 'NONE', *, *, #181, .F. ) ;
#3024 = CARTESIAN_POINT ( 'NONE',  ( 2.305787727787085295, 7.249469779319941409, -2.461236246750998724 ) ) ;
#3025 = AXIS2_PLACEMENT_3D ( 'NONE', #40471, #10534, #49813 ) ;
#3026 = DIRECTION ( 'NONE',  ( -1.000000000000000000, 0.000000000000000000, 0.000000000000000000 ) ) ;
#3027 = ORIENTED_EDGE ( 'NONE', *, *, #51591, .F. ) ;
#3028 = FACE_OUTER_BOUND ( 'NONE', #17338, .T. ) ;
#3029 = CARTESIAN_POINT ( 'NONE',  ( 2.990245332647884169, -7.587819667496408016, 3.789007530133533752 ) ) ;
#3030 = VERTEX_POINT ( 'NONE', #16415 ) ;
#3031 = AXIS2_PLACEMENT_3D ( 'NONE', #11825, #32108, #47434 ) ;
#3032 = CARTESIAN_POINT ( 'NONE',  ( 2.440552418640494992, 7.166505277347731351, 2.818488640081600938 ) ) ;
#3034 = EDGE_CURVE ( 'NONE', #58117, #10303, #51351, .T. ) ;
#3033 = LINE ( 'NONE', #63198, #22237 ) ;
#3035 = CARTESIAN_POINT ( 'NONE',  ( 1.719304012338401133, 5.690355757826538685, 11.38834240361399885 ) ) ;
#3036 = VERTEX_POINT ( 'NONE', #16065 ) ;
#3037 = VERTEX_POINT ( 'NONE', #11406 ) ;
#3038 = CARTESIAN_POINT ( 'NONE',  ( 1.948354844646311479, 3.407825014329756819, -11.46941405766637345 ) ) ;
#3040 = ORIENTED_EDGE ( 'NONE', *, *, #50249, .F. ) ;
#3039 = ADVANCED_FACE ( 'NONE', ( #36356 ), #55149, .F. ) ;
#3041 = CYLINDRICAL_SURFACE ( 'NONE', #52851, 12.75000000000000178 ) ;
#3042 = VERTEX_POINT ( 'NONE', #42295 ) ;
#3043 = AXIS2_PLACEMENT_3D ( 'NONE', #50798, #20542, #31175 ) ;
#3044 = CARTESIAN_POINT ( 'NONE',  ( 2.245754705088395031, 3.721112460997019866, 6.667819336165956123 ) ) ;
#3045 = EDGE_CURVE ( 'NONE', #35492, #37945, #26709, .T. ) ;
#3046 = CARTESIAN_POINT ( 'NONE',  ( 2.034671305877419734, -3.325478336156925341, -11.19279775166577551 ) ) ;
#3047 = CARTESIAN_POINT ( 'NONE',  ( -22.27218376572352554, 0.9890213205919790029, 3.547715993389650713 ) ) ;
#3048 = CARTESIAN_POINT ( 'NONE',  ( -22.28415773361649954, 3.586804264761564109, 0.9182279841529663589 ) ) ;
#3049 = DIRECTION ( 'NONE',  ( 0.3902440745007897949, -0.000000000000000000, 0.9207114435679737419 ) ) ;
#3050 = DIRECTION ( 'NONE',  ( -1.000000000000000000, -0.000000000000000000, -0.000000000000000000 ) ) ;
#3051 = VERTEX_POINT ( 'NONE', #21739 ) ;
#3052 = EDGE_CURVE ( 'NONE', #17260, #55082, #48040, .T. ) ;
#3053 = CARTESIAN_POINT ( 'NONE',  ( 37.00000000000000711, -1.457575200925456560, 12.66641127287626745 ) ) ;
#3054 = ORIENTED_EDGE ( 'NONE', *, *, #47180, .F. ) ;
#3055 = CARTESIAN_POINT ( 'NONE',  ( 35.00000000000000000, -9.557269938331497627, 7.561043153948066475 ) ) ;
#3056 = CARTESIAN_POINT ( 'NONE',  ( 2.241352910868908310, 6.652881166698511706, 3.744764251557016532 ) ) ;
#3057 = EDGE_CURVE ( 'NONE', #62587, #11696, #27743, .T. ) ;
#3058 = ORIENTED_EDGE ( 'NONE', *, *, #18484, .T. ) ;
#3059 = CARTESIAN_POINT ( 'NONE',  ( 24.97632970311353162, 10.66122974065908657, -8.283959357202872908 ) ) ;
#3060 = CARTESIAN_POINT ( 'NONE',  ( 0.2801149460245143108, 6.294737133725796241, 10.51028947658246260 ) ) ;
#3061 = DIRECTION ( 'NONE',  ( 1.000000000000000000, 0.000000000000000000, 0.000000000000000000 ) ) ;
#3062 = ORIENTED_EDGE ( 'NONE', *, *, #1434, .F. ) ;
#3063 = AXIS2_PLACEMENT_3D ( 'NONE', #16, #19667, #20946 ) ;
#3064 = VERTEX_POINT ( 'NONE', #23358 ) ;
#3065 = CARTESIAN_POINT ( 'NONE',  ( -35.00000000000000000, 11.53507381115580444, 2.216820770815288721 ) ) ;
#3066 = AXIS2_PLACEMENT_3D ( 'NONE', #32125, #42413, #7513 ) ;
#3067 = VERTEX_POINT ( 'NONE', #27677 ) ;
#3068 = DIRECTION ( 'NONE',  ( -0.000000000000000000, -1.000000000000000000, -0.000000000000000000 ) ) ;
#3069 = CARTESIAN_POINT ( 'NONE',  ( 26.34661844826604593, -11.53221627053866527, 3.317828791472333005 ) ) ;
#3070 = CARTESIAN_POINT ( 'NONE',  ( -35.00000000000000000, -3.805206332242558886, 12.16893194857548721 ) ) ;
#3071 = CARTESIAN_POINT ( 'NONE',  ( -3.543971956890883401, 9.152513797769646686, 7.771635824158136252 ) ) ;
#3072 = CARTESIAN_POINT ( 'NONE',  ( -17.63957941232862225, -7.319940456796631523, 9.513823268653226251 ) ) ;
#3073 = ORIENTED_EDGE ( 'NONE', *, *, #46770, .F. ) ;
#3074 = B_SPLINE_CURVE_WITH_KNOTS ( 'NONE', 3,
 ( #28394, #23087, #23411, #29379, #8780, #33707, #13107, #9095, #38029, #54002, #28719, #49372, #24071, #12756, #18098, #49033 ),
 .UNSPECIFIED., .F., .F.,
 ( 4, 3, 3, 3, 3, 4 ),
 ( 0.000000000000000000, 6.991367980366392898E-05, 0.0001398269368981362607, 0.0002097400188389099591, 0.0002811534801551364318, 0.0003526297678872489867 ),
 .UNSPECIFIED. ) ;
#3075 = CARTESIAN_POINT ( 'NONE',  ( 2.000000000000001776, -3.224464355699781848, -6.771471746882029130 ) ) ;
#3076 = VECTOR ( 'NONE', #18172, 1000.000000000000000 ) ;
#3077 = EDGE_CURVE ( 'NONE', #3342, #1280, #55378, .T. ) ;
#3078 = EDGE_CURVE ( 'NONE', #48048, #35612, #28132, .T. ) ;
#3079 = AXIS2_PLACEMENT_3D ( 'NONE', #33922, #3713, #64199 ) ;
#3080 = DIRECTION ( 'NONE',  ( -1.000000000000000000, 0.000000000000000000, 0.000000000000000000 ) ) ;
#3081 = CARTESIAN_POINT ( 'NONE',  ( 5.520433897694421610, 0.01329351892498004811, 0.007082458259338615496 ) ) ;
#3083 = VECTOR ( 'NONE', #21615, 1000.000000000000000 ) ;
#3082 = CARTESIAN_POINT ( 'NONE',  ( -27.08418322526031119, -0.8335872080609559864, 2.134267017050457849 ) ) ;
#3084 = DIRECTION ( 'NONE',  ( -0.4298323628305344979, -0.9029087107030918657, 0.000000000000000000 ) ) ;
#3085 = DIRECTION ( 'NONE',  ( 0.000000000000000000, -0.01356324068817991828, 0.9999080150203990547 ) ) ;
#3086 = CARTESIAN_POINT ( 'NONE',  ( -10.00000000000000178, 0.000000000000000000, 0.000000000000000000 ) ) ;
#3087 = ADVANCED_FACE ( 'NONE', ( #60156 ), #47984, .T. ) ;
#3088 = ORIENTED_EDGE ( 'NONE', *, *, #10282, .F. ) ;
#3089 = CARTESIAN_POINT ( 'NONE',  ( 12.70099391640234465, -11.34186981777373759, -3.924130698594886280 ) ) ;
#3090 = ORIENTED_EDGE ( 'NONE', *, *, #18942, .F. ) ;
#3091 = CARTESIAN_POINT ( 'NONE',  ( 0.2767916011545413779, 1.940025653809002826, -12.09541651105893756 ) ) ;
#3092 = CARTESIAN_POINT ( 'NONE',  ( 8.937200413559443390, 4.476360154859203355, -11.13383131558893346 ) ) ;
#3093 = CARTESIAN_POINT ( 'NONE',  ( 35.00000000000000000, 4.705694406421931860E-17, -3.469127814946512892E-15 ) ) ;
#3094 = ORIENTED_EDGE ( 'NONE', *, *, #21650, .F. ) ;
#3095 = CARTESIAN_POINT ( 'NONE',  ( 22.68139259647346861, 3.158742727684421769, -13.12595410559641529 ) ) ;
#3096 = LINE ( 'NONE', #43630, #12897 ) ;
#3097 = EDGE_LOOP ( 'NONE', ( #52112, #62138, #26968, #41318 ) ) ;
#3098 = ADVANCED_FACE ( 'NONE', ( #38658 ), #32988, .T. ) ;
#3099 = ORIENTED_EDGE ( 'NONE', *, *, #9674, .F. ) ;
#3100 = ORIENTED_EDGE ( 'NONE', *, *, #31329, .T. ) ;
#3101 = CARTESIAN_POINT ( 'NONE',  ( 0.2759803524722208579, -7.727919584673380804, -9.504501710971684503 ) ) ;
#3102 = ADVANCED_FACE ( 'NONE', ( #28346 ), #14275, .T. ) ;
#3103 = CARTESIAN_POINT ( 'NONE',  ( 2.259025283528085293, -7.131631878998414109, 2.741148848567739105 ) ) ;
#3104 = AXIS2_PLACEMENT_3D ( 'NONE', #48862, #3317, #23591 ) ;
#3105 = VERTEX_POINT ( 'NONE', #8077 ) ;
#3106 = DIRECTION ( 'NONE',  ( 0.000000000000000000, -0.01356324068817998940, 0.9999080150203990547 ) ) ;
#3107 = CARTESIAN_POINT ( 'NONE',  ( 2.373367633546870969, -2.795365972209121974, 7.151506276328619016 ) ) ;
#3108 = CARTESIAN_POINT ( 'NONE',  ( 2.000000000000001776, -4.604744433234713163, 5.919993978425451608 ) ) ;
#3109 = DIRECTION ( 'NONE',  ( -1.000000000000000000, 0.000000000000000000, 0.000000000000000000 ) ) ;
#3110 = ORIENTED_EDGE ( 'NONE', *, *, #36810, .T. ) ;
#3111 = CARTESIAN_POINT ( 'NONE',  ( 3.152665057734040488, 0.000000000000000000, 0.000000000000000000 ) ) ;
#3112 = AXIS2_PLACEMENT_3D ( 'NONE', #57338, #36724, #37711 ) ;
#3113 = CARTESIAN_POINT ( 'NONE',  ( 37.00000000000000711, -11.61175578952786758, -1.771820996347120092 ) ) ;
#3114 = FACE_OUTER_BOUND ( 'NONE', #20761, .T. ) ;
#3116 = ORIENTED_EDGE ( 'NONE', *, *, #64620, .F. ) ;
#3115 = DIRECTION ( 'NONE',  ( 1.000000000000000000, -0.000000000000000000, -0.000000000000000000 ) ) ;
#3117 = DIRECTION ( 'NONE',  ( -1.000000000000000000, 0.000000000000000000, 0.000000000000000000 ) ) ;
#3118 = ORIENTED_EDGE ( 'NONE', *, *, #39032, .F. ) ;
#3119 = DIRECTION ( 'NONE',  ( -1.000000000000000000, 0.000000000000000000, -0.000000000000000000 ) ) ;
#3120 = VERTEX_POINT ( 'NONE', #4312 ) ;
#3121 = CARTESIAN_POINT ( 'NONE',  ( 2.241528039335009215, 7.179411278563588183, -2.596349773934808702 ) ) ;
#3122 = CARTESIAN_POINT ( 'NONE',  ( -37.00000000000000711, -2.021542716731318912, -12.01765980939844169 ) ) ;
#3123 = EDGE_CURVE ( 'NONE', #46997, #34941, #52958, .T. ) ;
#3124 = VECTOR ( 'NONE', #1200, 1000.000000000000227 ) ;
#3125 = FACE_OUTER_BOUND ( 'NONE', #60137, .T. ) ;
#3126 = DIRECTION ( 'NONE',  ( -1.000000000000000000, 0.000000000000000000, 0.000000000000000000 ) ) ;
#3127 = FACE_OUTER_BOUND ( 'NONE', #29561, .T. ) ;
#3128 = CARTESIAN_POINT ( 'NONE',  ( -10.65303786363494964, -5.744948954241079875, -12.22272377441934665 ) ) ;
#3129 = CARTESIAN_POINT ( 'NONE',  ( -22.31328051695926007, -3.685074213229319717, -0.8849444482788241251 ) ) ;
#3130 = EDGE_CURVE ( 'NONE', #24709, #29997, #23039, .T. ) ;
#3131 = AXIS2_PLACEMENT_3D ( 'NONE', #63324, #26783, #16797 ) ;
#3132 =( BOUNDED_SURFACE ( )  B_SPLINE_SURFACE ( 3, 1, ( 
 ( #55098, #30479 ),
 ( #20179, #44453 ),
 ( #24855, #14204 ),
 ( #50777, #54470 ) ),
 .UNSPECIFIED., .F., .F., .F. ) 
 B_SPLINE_SURFACE_WITH_KNOTS ( ( 4, 4 ),
 ( 2, 2 ),
 ( 0.000000000000000000, 1.000000000000000000 ),
 ( 0.000000000000000000, 1.000000000000000000 ),
 .UNSPECIFIED. ) 
 GEOMETRIC_REPRESENTATION_ITEM ( )  RATIONAL_B_SPLINE_SURFACE ( (
 ( 1.000000000000000000, 1.000000000000000000),
 ( 0.6933888150995267674, 0.9895912004443193632),
 ( 0.6933888150995267674, 0.9895912004443193632),
 ( 1.000000000000000000, 1.000000000000000000) ) ) 
 REPRESENTATION_ITEM ( '' )  SURFACE ( )  );
#3133 = ORIENTED_EDGE ( 'NONE', *, *, #13676, .T. ) ;
#3134 = DIRECTION ( 'NONE',  ( -1.000000000000000000, 0.000000000000000000, -0.000000000000000000 ) ) ;
#3135 = ORIENTED_EDGE ( 'NONE', *, *, #16718, .F. ) ;
#3136 = EDGE_CURVE ( 'NONE', #3037, #23216, #36240, .T. ) ;
#3137 = ORIENTED_EDGE ( 'NONE', *, *, #29275, .F. ) ;
#3138 = CARTESIAN_POINT ( 'NONE',  ( 5.514624014163232779, -0.001255375129357695543, 0.003946330869975248588 ) ) ;
#3139 = AXIS2_PLACEMENT_3D ( 'NONE', #59983, #46975, #61929 ) ;
#3140 = DIRECTION ( 'NONE',  ( -1.000000000000000000, -0.000000000000000000, -0.000000000000000000 ) ) ;
#3141 = CARTESIAN_POINT ( 'NONE',  ( 0.2834382757447979073, -10.50792790568173274, 6.300836243950126203 ) ) ;
#3142 = CARTESIAN_POINT ( 'NONE',  ( 5.530133899448235191, -0.008946569461392248762, 0.01324661008606526670 ) ) ;
#3143 = DIRECTION ( 'NONE',  ( -1.000000000000000000, -0.000000000000000000, 0.000000000000000000 ) ) ;
#3144 = EDGE_CURVE ( 'NONE', #46242, #60760, #3096, .T. ) ;
#3145 = CYLINDRICAL_SURFACE ( 'NONE', #48263, 12.74999999999999822 ) ;
#3146 = VERTEX_POINT ( 'NONE', #18392 ) ;
#3147 = DIRECTION ( 'NONE',  ( 0.000000000000000000, -0.1081190184239488317, 0.9941379571543589311 ) ) ;
#3148 = DIRECTION ( 'NONE',  ( -1.000000000000000000, 0.000000000000000000, 0.000000000000000000 ) ) ;
#3149 = CARTESIAN_POINT ( 'NONE',  ( 35.00000000000000000, -5.710938531231789739, -11.39945968423469402 ) ) ;
#3150 = CARTESIAN_POINT ( 'NONE',  ( 2.244591118396560780, -4.825158615932929607, 5.917635828475974691 ) ) ;
#3151 = FACE_OUTER_BOUND ( 'NONE', #10072, .T. ) ;
#3152 = AXIS2_PLACEMENT_3D ( 'NONE', #48782, #28811, #49123 ) ;
#3153 = EDGE_CURVE ( 'NONE', #18713, #38075, #19265, .T. ) ;
#3154 = VECTOR ( 'NONE', #21270, 1000.000000000000000 ) ;
#3155 = CARTESIAN_POINT ( 'NONE',  ( -35.00000000000000000, -2.346765782874520312, 11.95840593935200680 ) ) ;
#3156 = CARTESIAN_POINT ( 'NONE',  ( -10.86457796283016997, -6.815227495106873867, 11.65522549784055073 ) ) ;
#3157 = VERTEX_POINT ( 'NONE', #49863 ) ;
#3158 = CARTESIAN_POINT ( 'NONE',  ( 0.9232058338315048962, -3.908895078357443875, -11.84276737136204716 ) ) ;
#3159 = CARTESIAN_POINT ( 'NONE',  ( 0.000000000000000000, -1.145812388885072863, -6.715725538143620277 ) ) ;
#3160 = CARTESIAN_POINT ( 'NONE',  ( 5.520433897694421610, -0.01006947824912430428, 0.01120198501134832270 ) ) ;
#3161 = CARTESIAN_POINT ( 'NONE',  ( -27.28563798457901868, -0.04047623855282859312, 2.896153581097021590 ) ) ;
#3162 = DIRECTION ( 'NONE',  ( -0.000000000000000000, -0.000000000000000000, -1.000000000000000000 ) ) ;
#3163 = CIRCLE ( 'NONE', #29707, 4.999999999999999112 ) ;
#3164 = ORIENTED_EDGE ( 'NONE', *, *, #65294, .T. ) ;
#3165 = CARTESIAN_POINT ( 'NONE',  ( 2.000000000000001776, -1.865193240757054394, -6.552473556515217012 ) ) ;
#3166 = CARTESIAN_POINT ( 'NONE',  ( 0.3106921474978498465, 9.239619355094145448, 8.060345844326317177 ) ) ;
#3167 = CARTESIAN_POINT ( 'NONE',  ( -17.68998094701642643, 2.870745959822725624, -11.65346102617277602 ) ) ;
#3168 = VERTEX_POINT ( 'NONE', #40525 ) ;
#3169 = CARTESIAN_POINT ( 'NONE',  ( 0.2915757698887287419, 2.339174865979285034, 12.02962099476164148 ) ) ;
#3170 = CARTESIAN_POINT ( 'NONE',  ( -35.00000000000000000, -0.7536123767499333104, 11.72195762423409704 ) ) ;
#3171 = VERTEX_POINT ( 'NONE', #9949 ) ;
#3172 = ADVANCED_FACE ( 'NONE', ( #15259 ), #60821, .T. ) ;
#3173 = AXIS2_PLACEMENT_3D ( 'NONE', #2721, #27614, #28942 ) ;
#3175 = ORIENTED_EDGE ( 'NONE', *, *, #34362, .T. ) ;
#3174 = B_SPLINE_CURVE_WITH_KNOTS ( 'NONE', 3,
 ( #46841, #26890, #63117, #32507, #1306, #21585, #16591, #22217, #31854, #17579, #36859, #1948, #52813, #57157, #37847, #27873 ),
 .UNSPECIFIED., .F., .F.,
 ( 4, 3, 3, 3, 3, 4 ),
 ( 0.000000000000000000, 0.0003017745587525276323, 0.0006035491769808768846, 0.0009053241094668227533, 0.001207275924539981740, 0.001510325902532936703 ),
 .UNSPECIFIED. ) ;
#3176 = CARTESIAN_POINT ( 'NONE',  ( -35.00000000000000000, 0.000000000000000000, 0.000000000000000000 ) ) ;
#3177 = ADVANCED_FACE ( 'NONE', ( #25563 ), #61793, .T. ) ;
#3178 = ORIENTED_EDGE ( 'NONE', *, *, #27782, .F. ) ;
#3179 = DIRECTION ( 'NONE',  ( 0.000000000000000000, 0.3554799084908970563, 0.9346839223284539866 ) ) ;
#3180 = CARTESIAN_POINT ( 'NONE',  ( -35.00000000000000000, 7.717887834988368390, -8.854740511458771834 ) ) ;
#3181 = DIRECTION ( 'NONE',  ( -1.000000000000000000, 0.000000000000000000, 0.000000000000000000 ) ) ;
#3182 = DIRECTION ( 'NONE',  ( 0.3939253465568943180, -0.8669868725995597547, 0.3052156353794235888 ) ) ;
#3183 = CARTESIAN_POINT ( 'NONE',  ( 1.194176325881342038, 11.96454551582842996, 3.807610977966959798 ) ) ;
#3185 = EDGE_LOOP ( 'NONE', ( #13472, #483, #28093, #47344 ) ) ;
#3184 = CARTESIAN_POINT ( 'NONE',  ( 1.283627346226433819, 0.5505361391623041500, 12.57362488724968053 ) ) ;
#3186 = DIRECTION ( 'NONE',  ( -1.000000000000000000, 0.000000000000000000, -0.000000000000000000 ) ) ;
#3187 = B_SPLINE_CURVE_WITH_KNOTS ( 'NONE', 3,
 ( #12074, #42994, #37346, #47350, #33354, #22731, #53317, #53652, #48000, #47659, #27366, #23053, #62602, #43313, #8091, #17064, #57657, #58647, #1791, #28359, #57315, #42310 ),
 .UNSPECIFIED., .F., .F.,
 ( 4, 3, 3, 3, 3, 3, 3, 4 ),
 ( 2.474737474518078493E-18, 4.449119708436613866E-05, 6.626296329540155904E-05, 8.803456484962335078E-05, 0.0001098060367612770858, 0.0001315774408628463013, 0.0001760698110411093511, 0.0001829697163287823721 ),
 .UNSPECIFIED. ) ;
#3188 = EDGE_LOOP ( 'NONE', ( #60521, #17682, #30246, #63034 ) ) ;
#3189 = CARTESIAN_POINT ( 'NONE',  ( 0.2648978790185602672, 10.53870023327872474, -6.237101853238436355 ) ) ;
#3190 = ORIENTED_EDGE ( 'NONE', *, *, #42347, .F. ) ;
#3191 = ORIENTED_EDGE ( 'NONE', *, *, #8600, .T. ) ;
#3192 = CARTESIAN_POINT ( 'NONE',  ( -2.532614230583023041, -12.88560382747352584, 4.026315189028235153 ) ) ;
#3193 = CARTESIAN_POINT ( 'NONE',  ( -6.227954140665750593, -28.64022186353238553, 12.80077302199559419 ) ) ;
#3194 = ADVANCED_FACE ( 'NONE', ( #15576 ), #5459, .F. ) ;
#3195 = CARTESIAN_POINT ( 'NONE',  ( -25.54417658651491863, 7.498517398407837931, 11.22596262356930197 ) ) ;
#3196 = CIRCLE ( 'NONE', #34021, 5.000000000000000000 ) ;
#3197 = AXIS2_PLACEMENT_3D ( 'NONE', #12274, #7283, #42862 ) ;
#3198 = CARTESIAN_POINT ( 'NONE',  ( 22.57855258442565116, 3.026812727784649493, -11.61199400236326973 ) ) ;
#3199 = DIRECTION ( 'NONE',  ( 0.000000000000000000, 0.000000000000000000, 1.000000000000000000 ) ) ;
#3200 = LINE ( 'NONE', #63040, #44751 ) ;
#3201 = VERTEX_POINT ( 'NONE', #50529 ) ;
#3202 = DIRECTION ( 'NONE',  ( -1.000000000000000000, 0.000000000000000000, 0.000000000000000000 ) ) ;
#3203 = CARTESIAN_POINT ( 'NONE',  ( 1.459561108992815992, -3.725588117663614973, 12.08294179906916810 ) ) ;
#3204 = CYLINDRICAL_SURFACE ( 'NONE', #24218, 12.18650000000000055 ) ;
#3205 = ORIENTED_EDGE ( 'NONE', *, *, #39463, .F. ) ;
#3206 = DIRECTION ( 'NONE',  ( -1.000000000000000000, 0.000000000000000000, 0.000000000000000000 ) ) ;
#3207 = ORIENTED_EDGE ( 'NONE', *, *, #43430, .F. ) ;
#3208 = DIRECTION ( 'NONE',  ( 0.000000000000000000, 0.000000000000000000, 1.000000000000000000 ) ) ;
#3209 = CARTESIAN_POINT ( 'NONE',  ( 25.00000000000000355, -9.999999999999998224, 1.530808498934191521E-15 ) ) ;
#3210 = CARTESIAN_POINT ( 'NONE',  ( 10.75853767213705225, 7.830989516993144051, 25.00000000000000000 ) ) ;
#3211 = CARTESIAN_POINT ( 'NONE',  ( 29.03457606387295087, 7.862146963512124387, 10.97436308512422265 ) ) ;
#3212 = ADVANCED_FACE ( 'NONE', ( #26228 ), #55837, .T. ) ;
#3213 = CARTESIAN_POINT ( 'NONE',  ( -47.00000000000000711, 0.000000000000000000, 0.000000000000000000 ) ) ;
#3214 = DIRECTION ( 'NONE',  ( 0.000000000000000000, 0.000000000000000000, -1.000000000000000000 ) ) ;
#3215 = LINE ( 'NONE', #28793, #9992 ) ;
#3216 = AXIS2_PLACEMENT_3D ( 'NONE', #7572, #37835, #52498 ) ;
#3217 = ORIENTED_EDGE ( 'NONE', *, *, #46388, .T. ) ;
#3218 = CARTESIAN_POINT ( 'NONE',  ( 0.000000000000000000, -2.562706407243573459, -6.312399813420393357 ) ) ;
#3219 = ORIENTED_EDGE ( 'NONE', *, *, #48908, .T. ) ;
#3220 = CARTESIAN_POINT ( 'NONE',  ( -37.00000000000000711, -10.32377448871672598, 6.475373545682264975 ) ) ;
#3221 = CARTESIAN_POINT ( 'NONE',  ( -37.00000000000000711, -6.018036132182241538, 11.24036214326518390 ) ) ;
#3222 = AXIS2_PLACEMENT_3D ( 'NONE', #31865, #52185, #57498 ) ;
#3223 = DIRECTION ( 'NONE',  ( -1.000000000000000000, -0.000000000000000000, 0.000000000000000000 ) ) ;
#3224 = DIRECTION ( 'NONE',  ( 1.000000000000000000, 0.000000000000000000, 0.000000000000000000 ) ) ;
#3225 = CARTESIAN_POINT ( 'NONE',  ( -28.14458306582303848, 12.90557762884671433, -3.973285507432364305 ) ) ;
#3226 = EDGE_CURVE ( 'NONE', #61808, #25415, #11841, .T. ) ;
#3227 = ORIENTED_EDGE ( 'NONE', *, *, #61, .T. ) ;
#3228 = CYLINDRICAL_SURFACE ( 'NONE', #51129, 12.75000000000000178 ) ;
#3229 = CARTESIAN_POINT ( 'NONE',  ( 10.16774168188999816, 8.043487525566618501, 8.909738100526366722 ) ) ;
#3230 = CARTESIAN_POINT ( 'NONE',  ( 2.242418902651939216, 1.423836467585349652, 7.500817491983885255 ) ) ;
#3231 = EDGE_CURVE ( 'NONE', #36273, #32360, #48744, .T. ) ;
#3232 = CARTESIAN_POINT ( 'NONE',  ( 2.717984159220022011, -5.223388265380124906, -5.783767685176870899 ) ) ;
#3233 = ORIENTED_EDGE ( 'NONE', *, *, #37897, .F. ) ;
#3234 = DIRECTION ( 'NONE',  ( -1.000000000000000000, 0.000000000000000000, 0.000000000000000000 ) ) ;
#3235 = DIRECTION ( 'NONE',  ( 0.000000000000000000, -0.01356324068817998940, 0.9999080150203990547 ) ) ;
#3236 = DIRECTION ( 'NONE',  ( 1.000000000000000000, 0.000000000000000000, 0.000000000000000000 ) ) ;
#3237 = DIRECTION ( 'NONE',  ( -1.000000000000000000, 0.000000000000000000, 0.000000000000000000 ) ) ;
#3238 = VECTOR ( 'NONE', #61130, 1000.000000000000000 ) ;
#3239 = AXIS2_PLACEMENT_3D ( 'NONE', #19149, #34442, #54744 ) ;
#3240 = AXIS2_PLACEMENT_3D ( 'NONE', #42259, #17358, #63872 ) ;
#3241 = EDGE_CURVE ( 'NONE', #32833, #3673, #51525, .T. ) ;
#3242 = AXIS2_PLACEMENT_3D ( 'NONE', #44208, #18947, #30229 ) ;
#3243 = CARTESIAN_POINT ( 'NONE',  ( 2.305787727787083519, -3.682701754025559993, 6.711944854845811825 ) ) ;
#3244 = CARTESIAN_POINT ( 'NONE',  ( -28.23740090307966355, -10.53170506870664624, -5.760529898918337111 ) ) ;
#3245 = ORIENTED_EDGE ( 'NONE', *, *, #47251, .F. ) ;
#3246 = CARTESIAN_POINT ( 'NONE',  ( -27.08417473062937120, 1.729223128152643341, -1.503027223283694092 ) ) ;
#3247 = CARTESIAN_POINT ( 'NONE',  ( 1.452237505248555660, 11.24427360515642071, 5.807998527925930965 ) ) ;
#3248 = CARTESIAN_POINT ( 'NONE',  ( 4.261270162784661863, -31.40576903066106240, -14.03034928007075344 ) ) ;
#3249 = ORIENTED_EDGE ( 'NONE', *, *, #23214, .F. ) ;
#3250 = CARTESIAN_POINT ( 'NONE',  ( 0.2655924914740778742, 12.06787830249865223, 2.083162675473652747 ) ) ;
#3251 = CARTESIAN_POINT ( 'NONE',  ( 1.719304012338239485, 12.38166659046522788, 2.961219984258211202 ) ) ;
#3252 = DIRECTION ( 'NONE',  ( -1.000000000000000000, 0.000000000000000000, 0.000000000000000000 ) ) ;
#3253 = EDGE_CURVE ( 'NONE', #10208, #28435, #7584, .T. ) ;
#3254 = DIRECTION ( 'NONE',  ( 0.000000000000000000, 0.01356324068817998940, -0.9999080150203990547 ) ) ;
#3255 = LINE ( 'NONE', #17561, #52176 ) ;
#3256 = AXIS2_PLACEMENT_3D ( 'NONE', #53321, #43316, #32027 ) ;
#3257 = CARTESIAN_POINT ( 'NONE',  ( 0.8320506296491568810, 12.17395768195220640, -2.535206712041328636 ) ) ;
#3258 = ORIENTED_EDGE ( 'NONE', *, *, #51060, .T. ) ;
#3259 = AXIS2_PLACEMENT_3D ( 'NONE', #105, #16702, #45996 ) ;
#3260 = CARTESIAN_POINT ( 'NONE',  ( -22.31328051695926007, 0.8849444482788259014, -3.685074213229314388 ) ) ;
#3261 = CARTESIAN_POINT ( 'NONE',  ( 0.000000000000000000, 6.906413915731199005, -0.6453518998146886565 ) ) ;
#3262 = CARTESIAN_POINT ( 'NONE',  ( 0.2647959493198559500, -9.474789498086940043, -7.758440170207265396 ) ) ;
#3263 = CARTESIAN_POINT ( 'NONE',  ( 2.844750968616399422, -4.777247819183459754, 6.210802026112522078 ) ) ;
#3264 = CARTESIAN_POINT ( 'NONE',  ( -22.27706485742869091, 3.358064672837120401, 1.508175983031588840 ) ) ;
#3265 = DIRECTION ( 'NONE',  ( 0.000000000000000000, 0.9847383929261610547, -0.1740410799127650732 ) ) ;
#3266 = DIRECTION ( 'NONE',  ( 0.000000000000000000, 0.01356324068817992175, -0.9999080150203990547 ) ) ;
#3267 = DIRECTION ( 'NONE',  ( -1.000000000000000000, 0.000000000000000000, 0.000000000000000000 ) ) ;
#3268 = EDGE_LOOP ( 'NONE', ( #2961, #42320, #27202, #45516 ) ) ;
#3269 = EDGE_LOOP ( 'NONE', ( #12065, #2099, #53228, #46921 ) ) ;
#3270 = CARTESIAN_POINT ( 'NONE',  ( -19.69476066079020171, -4.201994156881551312, -11.24025111398909615 ) ) ;
#3271 = VECTOR ( 'NONE', #52281, 1000.000000000000000 ) ;
#3272 = EDGE_LOOP ( 'NONE', ( #36581, #11343, #10174, #24060 ) ) ;
#3273 = CARTESIAN_POINT ( 'NONE',  ( -22.31328051695926007, 2.608921479762127849, -2.748895659348120635 ) ) ;
#3274 = CARTESIAN_POINT ( 'NONE',  ( 2.000000000000001776, 0.000000000000000000, 0.000000000000000000 ) ) ;
#3275 = CARTESIAN_POINT ( 'NONE',  ( -20.79170840334646542, -12.91784323155722269, -3.921648409140116698 ) ) ;
#3276 = ORIENTED_EDGE ( 'NONE', *, *, #14531, .F. ) ;
#3278 = CARTESIAN_POINT ( 'NONE',  ( -35.04643116707788408, 0.009112266603805360687, -0.008094444324502694799 ) ) ;
#3277 = CIRCLE ( 'NONE', #21291, 12.75000000000000178 ) ;
#3279 = CARTESIAN_POINT ( 'NONE',  ( 2.000000000000001776, 6.470132594555819239, 2.133363481234098469 ) ) ;
#3280 = DIRECTION ( 'NONE',  ( 1.000000000000000000, -0.000000000000000000, -0.000000000000000000 ) ) ;
#3281 = ORIENTED_EDGE ( 'NONE', *, *, #55116, .F. ) ;
#3282 = ORIENTED_EDGE ( 'NONE', *, *, #26792, .F. ) ;
#3283 = CARTESIAN_POINT ( 'NONE',  ( 3.152665057734040488, 0.000000000000000000, 0.000000000000000000 ) ) ;
#3284 = VERTEX_POINT ( 'NONE', #5972 ) ;
#3285 = CYLINDRICAL_SURFACE ( 'NONE', #63068, 1.500000000000000444 ) ;
#3286 = ORIENTED_EDGE ( 'NONE', *, *, #17301, .T. ) ;
#3287 = ORIENTED_EDGE ( 'NONE', *, *, #52505, .T. ) ;
#3288 = FACE_OUTER_BOUND ( 'NONE', #38240, .T. ) ;
#3289 = CARTESIAN_POINT ( 'NONE',  ( -27.10307689719148527, -1.615391801699804120, 1.703783570823879323 ) ) ;
#3290 = ADVANCED_FACE ( 'NONE', ( #4656 ), #44732, .F. ) ;
#3292 = CIRCLE ( 'NONE', #12849, 7.499999999999988454 ) ;
#3291 = CARTESIAN_POINT ( 'NONE',  ( 0.3341166715381344576, 10.49680960898235149, -6.352033667906496817 ) ) ;
#3293 = CARTESIAN_POINT ( 'NONE',  ( 37.00000000000000711, -1.030638227056475120, 12.14284015767850811 ) ) ;
#3294 = CARTESIAN_POINT ( 'NONE',  ( 18.00005080000000035, 0.000000000000000000, 0.000000000000000000 ) ) ;
#3295 = VECTOR ( 'NONE', #47182, 1000.000000000000000 ) ;
#3296 = CARTESIAN_POINT ( 'NONE',  ( -35.00000000000000000, 0.000000000000000000, 0.000000000000000000 ) ) ;
#3297 = VERTEX_POINT ( 'NONE', #1629 ) ;
#3298 = CARTESIAN_POINT ( 'NONE',  ( 2.241352910868909643, -1.407733736974916772, 7.503490710578227585 ) ) ;
#3299 = AXIS2_PLACEMENT_3D ( 'NONE', #41370, #36726, #26420 ) ;
#3300 = DIRECTION ( 'NONE',  ( 0.000000000000000000, 0.000000000000000000, 1.000000000000000000 ) ) ;
#3301 = CARTESIAN_POINT ( 'NONE',  ( 2.000000000000001776, 6.662861565602072211, 1.421313227905651289 ) ) ;
#3302 = CARTESIAN_POINT ( 'NONE',  ( 2.241352910868908310, -2.689314586382399952, 7.145045428366567641 ) ) ;
#3303 = CARTESIAN_POINT ( 'NONE',  ( 0.3474126878361817328, -8.085727498271713998, -9.233692382639453911 ) ) ;
#3304 = CARTESIAN_POINT ( 'NONE',  ( 22.86336934118476805, 2.804796819963978560, 13.20738486019996927 ) ) ;
#3305 = CARTESIAN_POINT ( 'NONE',  ( 35.00000000000000000, 4.705694406421931860E-17, -3.469127814946512892E-15 ) ) ;
#3306 = CARTESIAN_POINT ( 'NONE',  ( -28.85619398320021745, 3.750539801530000439, -12.96855624952673836 ) ) ;
#3307 = CARTESIAN_POINT ( 'NONE',  ( 35.00000000000000000, 10.01317267707886671, -6.946017217729977489 ) ) ;
#3308 = AXIS2_PLACEMENT_3D ( 'NONE', #41002, #30040, #61283 ) ;
#3309 = EDGE_CURVE ( 'NONE', #332, #61330, #6614, .T. ) ;
#3310 = VERTEX_POINT ( 'NONE', #21902 ) ;
#3311 = CARTESIAN_POINT ( 'NONE',  ( -18.58686583997219799, 5.411564556385481062, -10.71438573093091051 ) ) ;
#3312 = AXIS2_PLACEMENT_3D ( 'NONE', #60212, #20949, #61511 ) ;
#3313 = AXIS2_PLACEMENT_3D ( 'NONE', #65255, #60586, #10055 ) ;
#3314 =( BOUNDED_SURFACE ( )  B_SPLINE_SURFACE ( 3, 1, ( 
 ( #56284, #1762 ),
 ( #11077, #31021 ),
 ( #61593, #31351 ),
 ( #37653, #57950 ) ),
 .UNSPECIFIED., .F., .F., .F. ) 
 B_SPLINE_SURFACE_WITH_KNOTS ( ( 4, 4 ),
 ( 2, 2 ),
 ( 0.000000000000000000, 1.000000000000000000 ),
 ( 0.000000000000000000, 1.000000000000000000 ),
 .UNSPECIFIED. ) 
 GEOMETRIC_REPRESENTATION_ITEM ( )  RATIONAL_B_SPLINE_SURFACE ( (
 ( 1.000000000000000000, 1.000000000000000000),
 ( 0.8716676215708681896, 0.8964445200148167814),
 ( 0.8716676215708681896, 0.8964445200148167814),
 ( 1.000000000000000000, 1.000000000000000000) ) ) 
 REPRESENTATION_ITEM ( '' )  SURFACE ( )  );
#3315 = VERTEX_POINT ( 'NONE', #26544 ) ;
#3316 = EDGE_CURVE ( 'NONE', #41887, #25967, #30106, .T. ) ;
#3317 = DIRECTION ( 'NONE',  ( 1.000000000000000000, 0.000000000000000000, 0.000000000000000000 ) ) ;
#3318 = CARTESIAN_POINT ( 'NONE',  ( 0.2706063244538033374, -0.1752385892652840171, 12.24670371972918304 ) ) ;
#3319 = CARTESIAN_POINT ( 'NONE',  ( 12.85737776239257357, -12.70266831868442736, -4.575077721476746184 ) ) ;
#3320 = CIRCLE ( 'NONE', #26692, 12.73084802173761787 ) ;
#3321 = DIRECTION ( 'NONE',  ( 0.000000000000000000, 0.000000000000000000, 1.000000000000000000 ) ) ;
#3322 = EDGE_CURVE ( 'NONE', #62589, #14872, #24572, .T. ) ;
#3323 = CARTESIAN_POINT ( 'NONE',  ( 3.031336079629838753, 5.388626255827111855, 5.773872239512813032 ) ) ;
#3324 = ORIENTED_EDGE ( 'NONE', *, *, #32858, .T. ) ;
#3325 = LINE ( 'NONE', #23930, #30325 ) ;
#3327 = AXIS2_PLACEMENT_3D ( 'NONE', #49266, #38937, #22667 ) ;
#3326 = CARTESIAN_POINT ( 'NONE',  ( 2.273267844204863053, -3.690689057641665993, 6.695181685739943767 ) ) ;
#3328 = DIRECTION ( 'NONE',  ( 0.000000000000000000, -0.01356324068817998940, 0.9999080150203990547 ) ) ;
#3329 = CARTESIAN_POINT ( 'NONE',  ( 14.80527133490444314, -33.90607016887765468, -8.874040421132026069 ) ) ;
#3330 = B_SPLINE_CURVE_WITH_KNOTS ( 'NONE', 3,
 ( #42277, #46643, #6417, #11707, #16397, #26691, #37313 ),
 .UNSPECIFIED., .F., .F.,
 ( 4, 3, 4 ),
 ( 4.939146456270413598E-15, 0.002398160485434625965, 0.005002426799381625919 ),
 .UNSPECIFIED. ) ;
#3331 = EDGE_CURVE ( 'NONE', #60562, #10633, #32500, .T. ) ;
#3332 = CIRCLE ( 'NONE', #12839, 12.18649999999999878 ) ;
#3333 = DIRECTION ( 'NONE',  ( 0.000000000000000000, 0.000000000000000000, 1.000000000000000000 ) ) ;
#3334 = ORIENTED_EDGE ( 'NONE', *, *, #17797, .T. ) ;
#3335 = EDGE_CURVE ( 'NONE', #48435, #15604, #60700, .T. ) ;
#3336 = DIRECTION ( 'NONE',  ( -1.000000000000000000, 0.000000000000000000, 0.000000000000000000 ) ) ;
#3337 = AXIS2_PLACEMENT_3D ( 'NONE', #10418, #25395, #9425 ) ;
#3338 = DIRECTION ( 'NONE',  ( -1.000000000000000000, 0.000000000000000000, 0.000000000000000000 ) ) ;
#3339 = CARTESIAN_POINT ( 'NONE',  ( -35.00000000000000000, 12.46157735505192932, -2.696588552978924636 ) ) ;
#3340 = CIRCLE ( 'NONE', #40469, 12.75000000000000178 ) ;
#3341 = CIRCLE ( 'NONE', #16074, 12.18649999999999878 ) ;
#3342 = VERTEX_POINT ( 'NONE', #62435 ) ;
#3343 = ORIENTED_EDGE ( 'NONE', *, *, #39453, .F. ) ;
#3345 = ADVANCED_FACE ( 'NONE', ( #31848 ), #16897, .T. ) ;
#3344 = CARTESIAN_POINT ( 'NONE',  ( 0.000000000000000000, 3.155844197800107498, 6.177028383390443800 ) ) ;
#3346 = EDGE_LOOP ( 'NONE', ( #32467, #58061, #4704, #33924 ) ) ;
#3347 = LINE ( 'NONE', #43886, #62674 ) ;
#3348 = CARTESIAN_POINT ( 'NONE',  ( 2.000000000000001776, -6.796153407501424049, -1.388283512725909219 ) ) ;
#3349 = DIRECTION ( 'NONE',  ( 0.000000000000000000, -0.9105187689795998240, 0.4134677391718418193 ) ) ;
#3350 = CARTESIAN_POINT ( 'NONE',  ( 0.2767916011545385468, 9.260929738915347542, -8.018602152763769197 ) ) ;
#3351 = EDGE_CURVE ( 'NONE', #15607, #56731, #46385, .T. ) ;
#3352 = CARTESIAN_POINT ( 'NONE',  ( 5.516018279890452902, -0.0009545156522404840260, 0.006707902355168859562 ) ) ;
#3353 = ORIENTED_EDGE ( 'NONE', *, *, #44055, .F. ) ;
#3354 = ORIENTED_EDGE ( 'NONE', *, *, #10018, .T. ) ;
#3355 = ORIENTED_EDGE ( 'NONE', *, *, #16756, .T. ) ;
#3356 = CARTESIAN_POINT ( 'NONE',  ( 2.276198483117261251, 7.236140649716396922, -2.469789406312159041 ) ) ;
#3357 = CIRCLE ( 'NONE', #59640, 2.899999999999995914 ) ;
#3358 = DIRECTION ( 'NONE',  ( -1.000000000000000000, 0.000000000000000000, 0.000000000000000000 ) ) ;
#3359 = B_SPLINE_CURVE_WITH_KNOTS ( 'NONE', 3,
 ( #58207, #12975, #32905, #17970, #63829, #52882, #38227, #18648, #2707, #38908, #22967, #43221, #54201, #7315, #47903, #8644, #27599, #53218, #57897, #49234, #2364, #22636 ),
 .UNSPECIFIED., .F., .F.,
 ( 4, 3, 3, 3, 3, 3, 3, 4 ),
 ( 0.000000000000000000, 4.447697177976180934E-05, 6.624143997791020252E-05, 8.800576886943984461E-05, 0.0001097699864780857134, 0.0001315341395364307139, 0.0001760120188223187525, 0.0001867971373174701869 ),
 .UNSPECIFIED. ) ;
#3360 = ORIENTED_EDGE ( 'NONE', *, *, #23685, .F. ) ;
#3361 = DIRECTION ( 'NONE',  ( -1.000000000000000000, 0.000000000000000000, 0.000000000000000000 ) ) ;
#3362 = CIRCLE ( 'NONE', #6579, 12.18650000000000055 ) ;
#3363 = CARTESIAN_POINT ( 'NONE',  ( -22.28939870658739864, -0.2834927284407604553, -3.707376022556866602 ) ) ;
#3364 = VERTEX_POINT ( 'NONE', #7237 ) ;
#3365 = DIRECTION ( 'NONE',  ( 1.000000000000000000, -0.000000000000000000, -0.000000000000000000 ) ) ;
#3366 = DIRECTION ( 'NONE',  ( 1.000000000000000000, 0.000000000000000000, 0.000000000000000000 ) ) ;
#3367 = CARTESIAN_POINT ( 'NONE',  ( -14.11589373245165469, 8.250315036047107142, 25.00000000000000000 ) ) ;
#3368 = ORIENTED_EDGE ( 'NONE', *, *, #33397, .F. ) ;
#3369 = CIRCLE ( 'NONE', #24608, 12.18650000000000055 ) ;
#3370 = ORIENTED_EDGE ( 'NONE', *, *, #14006, .F. ) ;
#3371 = DIRECTION ( 'NONE',  ( -1.000000000000000000, 0.000000000000000000, 0.000000000000000000 ) ) ;
#3372 = ORIENTED_EDGE ( 'NONE', *, *, #60318, .T. ) ;
#3373 = CYLINDRICAL_SURFACE ( 'NONE', #3079, 4.999999999999999112 ) ;
#3374 = VERTEX_POINT ( 'NONE', #11903 ) ;
#3375 = CIRCLE ( 'NONE', #53244, 5.000000000000000888 ) ;
#3376 = ORIENTED_EDGE ( 'NONE', *, *, #57570, .F. ) ;
#3377 = CARTESIAN_POINT ( 'NONE',  ( 2.249013661412228693, 3.714035584818222713, 6.673008335691879012 ) ) ;
#3378 = FACE_OUTER_BOUND ( 'NONE', #10579, .T. ) ;
#3379 = CARTESIAN_POINT ( 'NONE',  ( 37.00000000000000711, 4.983891302653743693, 11.73555825188270596 ) ) ;
#3380 = ADVANCED_FACE ( 'NONE', ( #41842 ), #47184, .T. ) ;
#3381 = CARTESIAN_POINT ( 'NONE',  ( -22.27878402819508707, 3.562981801125752135, 0.9457981527432224311 ) ) ;
#3382 = CARTESIAN_POINT ( 'NONE',  ( 1.104777566491141672, 11.59867774809550589, -4.729982681549413925 ) ) ;
#3383 = CARTESIAN_POINT ( 'NONE',  ( 0.3675815128205894289, -9.235491948680062180, 8.093875121226046687 ) ) ;
#3384 = VERTEX_POINT ( 'NONE', #1940 ) ;
#3385 = DIRECTION ( 'NONE',  ( 1.000000000000000000, 0.000000000000000000, -0.000000000000000000 ) ) ;
#3386 = AXIS2_PLACEMENT_3D ( 'NONE', #51473, #29829, #40816 ) ;
#3387 = ORIENTED_EDGE ( 'NONE', *, *, #9032, .F. ) ;
#3388 = CARTESIAN_POINT ( 'NONE',  ( 2.284126774967660811, -2.764365694977838572, 7.131638985093299965 ) ) ;
#3389 = DIRECTION ( 'NONE',  ( 0.000000000000000000, 0.2618041379715563277, -0.9651210252299812220 ) ) ;
#3390 = VERTEX_POINT ( 'NONE', #22207 ) ;
#3391 = EDGE_CURVE ( 'NONE', #45562, #42237, #62131, .T. ) ;
#3392 = DIRECTION ( 'NONE',  ( -1.000000000000000000, 0.000000000000000000, 0.000000000000000000 ) ) ;
#3393 = CARTESIAN_POINT ( 'NONE',  ( 0.2956976708475461679, 3.984495122852575566, 11.59055635407402463 ) ) ;
#3394 = CARTESIAN_POINT ( 'NONE',  ( 0.3632410797595302943, -2.390576695689024866, -12.04386719438561926 ) ) ;
#3395 = ORIENTED_EDGE ( 'NONE', *, *, #61859, .T. ) ;
#3396 = AXIS2_PLACEMENT_3D ( 'NONE', #63332, #17799, #38060 ) ;
#3397 = AXIS2_PLACEMENT_3D ( 'NONE', #54729, #14943, #35571 ) ;
#3398 = CIRCLE ( 'NONE', #63877, 12.18649999999999878 ) ;
#3399 = EDGE_CURVE ( 'NONE', #20070, #49500, #8684, .T. ) ;
#3400 = VERTEX_POINT ( 'NONE', #22556 ) ;
#3401 = DIRECTION ( 'NONE',  ( 0.000000000000000000, -0.2355298848897378061, -0.9718671068226493182 ) ) ;
#3402 = VERTEX_POINT ( 'NONE', #37510 ) ;
#3403 = CARTESIAN_POINT ( 'NONE',  ( 35.00000000000000000, -12.08216339958901564, -1.591260454995201412 ) ) ;
#3404 = DIRECTION ( 'NONE',  ( 1.000000000000000000, 0.000000000000000000, 0.000000000000000000 ) ) ;
#3405 = DIRECTION ( 'NONE',  ( 1.000000000000000000, -0.000000000000000000, 0.000000000000000000 ) ) ;
#3406 = PLANE ( 'NONE',  #52142 ) ;
#3407 = ADVANCED_FACE ( 'NONE', ( #16585 ), #57815, .T. ) ;
#3408 = CARTESIAN_POINT ( 'NONE',  ( 0.9232167919969156422, -9.278116382137428175, 8.324955738482442413 ) ) ;
#3409 = VERTEX_POINT ( 'NONE', #42818 ) ;
#3410 = CARTESIAN_POINT ( 'NONE',  ( -14.11589373245165469, 8.250315036047107142, 25.00000000000000000 ) ) ;
#3411 = CIRCLE ( 'NONE', #41632, 5.000000000000000888 ) ;
#3412 = CIRCLE ( 'NONE', #38400, 5.000000000000000888 ) ;
#3413 = CIRCLE ( 'NONE', #59681, 5.000000000000000888 ) ;
#3414 = CARTESIAN_POINT ( 'NONE',  ( 19.56743653832047158, -30.00000000000000000, -5.000000000000000888 ) ) ;
#3415 = ADVANCED_FACE ( 'NONE', ( #37839 ), #36532, .T. ) ;
#3416 = AXIS2_PLACEMENT_3D ( 'NONE', #39568, #10606, #14294 ) ;
#3417 = CARTESIAN_POINT ( 'NONE',  ( 2.406456491626458138, -2.970787154400910346, 10.00134798414774373 ) ) ;
#3418 = FACE_OUTER_BOUND ( 'NONE', #12804, .T. ) ;
#3419 = EDGE_CURVE ( 'NONE', #50728, #42390, #19320, .T. ) ;
#3420 = CARTESIAN_POINT ( 'NONE',  ( 5.516018279890452902, 0.0009545156522407046611, 0.006707902355169304519 ) ) ;
#3421 = CARTESIAN_POINT ( 'NONE',  ( 5.650264051100599261, -9.979872282089162994, -6.674586346603469167 ) ) ;
#3422 = DIRECTION ( 'NONE',  ( -1.000000000000000000, -0.000000000000000000, -0.000000000000000000 ) ) ;
#3423 = AXIS2_PLACEMENT_3D ( 'NONE', #18091, #16769, #58011 ) ;
#3424 = EDGE_CURVE ( 'NONE', #82, #12941, #13849, .T. ) ;
#3425 = ORIENTED_EDGE ( 'NONE', *, *, #58231, .F. ) ;
#3426 = EDGE_CURVE ( 'NONE', #1201, #62360, #24499, .T. ) ;
#3427 = CARTESIAN_POINT ( 'NONE',  ( 12.18694916440639631, -11.65410571009191365, -2.865109251948741775 ) ) ;
#3428 = EDGE_CURVE ( 'NONE', #11425, #26907, #24627, .T. ) ;
#3429 = CIRCLE ( 'NONE', #46930, 12.74999999999999822 ) ;
#3430 = EDGE_LOOP ( 'NONE', ( #56406, #32269, #624, #3471 ) ) ;
#3431 = DIRECTION ( 'NONE',  ( 0.000000000000000000, 0.01356324068817998940, -0.9999080150203989437 ) ) ;
#3432 = CARTESIAN_POINT ( 'NONE',  ( -22.28629837673888048, 3.697248502489085098, -0.2936941584814282136 ) ) ;
#3433 = CARTESIAN_POINT ( 'NONE',  ( 0.2650492433740059273, 6.218175523534292815, 10.54996000109277432 ) ) ;
#3434 = EDGE_CURVE ( 'NONE', #1207, #38878, #21788, .T. ) ;
#3435 = CARTESIAN_POINT ( 'NONE',  ( 0.2652384770603680719, -12.24598129987881379, -0.06606665821610741007 ) ) ;
#3436 = ORIENTED_EDGE ( 'NONE', *, *, #53366, .F. ) ;
#3437 = AXIS2_PLACEMENT_3D ( 'NONE', #40793, #61375, #25826 ) ;
#3438 = ORIENTED_EDGE ( 'NONE', *, *, #40843, .F. ) ;
#3439 = ORIENTED_EDGE ( 'NONE', *, *, #47419, .T. ) ;
#3440 = CARTESIAN_POINT ( 'NONE',  ( 0.3106921474978474040, -7.699584408545827152, -9.542334142800539709 ) ) ;
#3441 = AXIS2_PLACEMENT_3D ( 'NONE', #3176, #63999, #54702 ) ;
#3442 = DIRECTION ( 'NONE',  ( 0.000000000000000000, -0.01356324068817998940, 0.9999080150203990547 ) ) ;
#3443 = CIRCLE ( 'NONE', #37385, 5.000000000000000000 ) ;
#3444 = AXIS2_PLACEMENT_3D ( 'NONE', #65419, #19888, #55799 ) ;
#3445 = ORIENTED_EDGE ( 'NONE', *, *, #61614, .T. ) ;
#3446 = DIRECTION ( 'NONE',  ( 1.000000000000000000, 0.000000000000000000, 0.000000000000000000 ) ) ;
#3447 = CARTESIAN_POINT ( 'NONE',  ( 3.100650473569514620, -3.129198107107880933, 7.276570693048374672 ) ) ;
#3448 = CARTESIAN_POINT ( 'NONE',  ( 0.3106921474978470710, 10.49891314301085998, 6.333448016104091138 ) ) ;
#3449 = CARTESIAN_POINT ( 'NONE',  ( 0.2646305136544072623, -11.46223899740603436, 4.312539723326094254 ) ) ;
#3450 = ORIENTED_EDGE ( 'NONE', *, *, #20426, .T. ) ;
#3451 = DIRECTION ( 'NONE',  ( -1.000000000000000000, 0.000000000000000000, 0.000000000000000000 ) ) ;
#3452 = CYLINDRICAL_SURFACE ( 'NONE', #50059, 12.18649999999999878 ) ;
#3453 = DIRECTION ( 'NONE',  ( 0.000000000000000000, 0.000000000000000000, -1.000000000000000000 ) ) ;
#3455 = ORIENTED_EDGE ( 'NONE', *, *, #34362, .F. ) ;
#3454 = CARTESIAN_POINT ( 'NONE',  ( 0.3665391374699467075, 2.392238720110619443, -12.04754782681755110 ) ) ;
#3456 = DIRECTION ( 'NONE',  ( 0.000000000000000000, 0.000000000000000000, -1.000000000000000000 ) ) ;
#3457 = B_SPLINE_CURVE_WITH_KNOTS ( 'NONE', 3,
 ( #15365, #6066, #45617, #51294, #35307, #41938, #1064, #56250, #6381, #10692, #46295, #55620, #41613, #61900, #46943, #16359, #36633, #56937, #11355, #5077, #20689, #50952, #5400, #21683, #35639, #62225 ),
 .UNSPECIFIED., .F., .F.,
 ( 4, 2, 2, 2, 2, 2, 2, 2, 2, 2, 2, 2, 4 ),
 ( 0.02137397820462155415, 0.02270922547143531048, 0.02404447273824906334, 0.02671496727187657599, 0.02805021453869033232, 0.02938546180550408865, 0.03205595633913160825, 0.03472645087275912090, 0.03606169813957287723, 0.03739694540638663356, 0.03873219267320038989, 0.04006743994001414622, 0.04273793447364165887 ),
 .UNSPECIFIED. ) ;
#3458 = ORIENTED_EDGE ( 'NONE', *, *, #63498, .T. ) ;
#3459 = DIRECTION ( 'NONE',  ( 0.000000000000000000, -0.9987865678893282917, 0.04924826701373502535 ) ) ;
#3460 = ORIENTED_EDGE ( 'NONE', *, *, #14689, .F. ) ;
#3461 = CYLINDRICAL_SURFACE ( 'NONE', #29492, 12.18650000000000055 ) ;
#3462 = VECTOR ( 'NONE', #61075, 1000.000000000000000 ) ;
#3463 = CARTESIAN_POINT ( 'NONE',  ( 0.2915757698887302407, 3.989025639548790192, -11.58754481235182432 ) ) ;
#3464 = DIRECTION ( 'NONE',  ( 0.000000000000000000, -0.01356324068817991828, 0.9999080150203990547 ) ) ;
#3465 = CARTESIAN_POINT ( 'NONE',  ( 0.2801149460245159206, -4.005169813315180072, 11.57793225195135278 ) ) ;
#3466 = AXIS2_PLACEMENT_3D ( 'NONE', #33656, #12699, #13048 ) ;
#3467 = EDGE_CURVE ( 'NONE', #25430, #65138, #64947, .T. ) ;
#3468 = CARTESIAN_POINT ( 'NONE',  ( 0.2650492433740059828, -11.46945725111970660, 4.291726136518509094 ) ) ;
#3469 = DIRECTION ( 'NONE',  ( 0.000000000000000000, 0.4935949184179262983, -0.8696919319575183716 ) ) ;
#3470 = CARTESIAN_POINT ( 'NONE',  ( 9.687175622948609899, 13.48729812737144940, -0.5854820436212360146 ) ) ;
#3471 = ORIENTED_EDGE ( 'NONE', *, *, #11070, .T. ) ;
#3472 = CARTESIAN_POINT ( 'NONE',  ( -35.00000000000000000, 0.000000000000000000, 0.000000000000000000 ) ) ;
#3473 = VERTEX_POINT ( 'NONE', #28505 ) ;
#3474 = AXIS2_PLACEMENT_3D ( 'NONE', #54478, #2960, #48835 ) ;
#3475 = ORIENTED_EDGE ( 'NONE', *, *, #55381, .F. ) ;
#3476 = ADVANCED_FACE ( 'NONE', ( #63418 ), #5417, .T. ) ;
#3477 = CARTESIAN_POINT ( 'NONE',  ( -37.00000000000000711, 11.24036214326520700, 6.018036132182202458 ) ) ;
#3478 = CARTESIAN_POINT ( 'NONE',  ( 35.00000000000000000, 4.705694406421931860E-17, -3.469127814946512892E-15 ) ) ;
#3479 = CARTESIAN_POINT ( 'NONE',  ( -37.00000000000000711, 11.96656215839369253, 4.400442035670988794 ) ) ;
#3480 = CARTESIAN_POINT ( 'NONE',  ( -22.27704833740210333, 2.142029987820972980, 2.993786163585769877 ) ) ;
#3481 = FACE_OUTER_BOUND ( 'NONE', #62582, .T. ) ;
#3482 = LINE ( 'NONE', #44999, #17210 ) ;
#3483 = CARTESIAN_POINT ( 'NONE',  ( -34.00000000000000000, -11.99999999999999822, 0.000000000000000000 ) ) ;
#3484 = AXIS2_PLACEMENT_3D ( 'NONE', #3301, #14229, #54815 ) ;
#3485 = ORIENTED_EDGE ( 'NONE', *, *, #58362, .F. ) ;
#3486 = PLANE ( 'NONE',  #58248 ) ;
#3487 = CARTESIAN_POINT ( 'NONE',  ( 2.259830038565000532, -5.763537486834636070, -5.015955067335985618 ) ) ;
#3488 = CARTESIAN_POINT ( 'NONE',  ( -17.83419946441818027, -9.720786832536937538, 9.367833439828872955 ) ) ;
#3489 = EDGE_CURVE ( 'NONE', #29012, #24593, #48949, .T. ) ;
#3490 = VECTOR ( 'NONE', #18959, 1000.000000000000114 ) ;
#3491 = AXIS2_PLACEMENT_3D ( 'NONE', #38739, #49700, #4145 ) ;
#3492 = DIRECTION ( 'NONE',  ( 0.000000000000000000, 0.1387779952735747335, -0.9903235168508560671 ) ) ;
#3493 = AXIS2_PLACEMENT_3D ( 'NONE', #781, #35999, #10748 ) ;
#3494 = CARTESIAN_POINT ( 'NONE',  ( -8.333162451619710254, -1.931509586269193113, 13.36158470235419493 ) ) ;
#3495 = CARTESIAN_POINT ( 'NONE',  ( -10.39029797936073862, -5.035631434083518876, 12.53173546626830692 ) ) ;
#3496 = ORIENTED_EDGE ( 'NONE', *, *, #19271, .T. ) ;
#3497 = DIRECTION ( 'NONE',  ( 0.000000000000000000, 0.01356324068817998940, -0.9999080150203990547 ) ) ;
#3498 = CARTESIAN_POINT ( 'NONE',  ( 2.889800649504073782, 3.118861721612566029, 5.267262008933680129 ) ) ;
#3499 = DIRECTION ( 'NONE',  ( 1.000000000000000000, -0.000000000000000000, 0.000000000000000000 ) ) ;
#3500 = EDGE_CURVE ( 'NONE', #27117, #18739, #9038, .T. ) ;
#3501 = EDGE_CURVE ( 'NONE', #65490, #26404, #35079, .T. ) ;
#3502 = AXIS2_PLACEMENT_3D ( 'NONE', #4655, #16584, #37168 ) ;
#3503 = EDGE_CURVE ( 'NONE', #48169, #32449, #28197, .T. ) ;
#3504 = DIRECTION ( 'NONE',  ( 0.000000000000000000, 0.000000000000000000, 1.000000000000000000 ) ) ;
#3505 = DIRECTION ( 'NONE',  ( 1.000000000000000000, 0.000000000000000000, 0.000000000000000000 ) ) ;
#3506 = VERTEX_POINT ( 'NONE', #43462 ) ;
#3507 = CARTESIAN_POINT ( 'NONE',  ( 0.2638984909335716500, -10.70468911391668243, 5.950360275955019596 ) ) ;
#3508 = LINE ( 'NONE', #54693, #52319 ) ;
#3509 = VECTOR ( 'NONE', #62543, 1000.000000000000227 ) ;
#3510 = CARTESIAN_POINT ( 'NONE',  ( -18.58686583997219799, 4.913588802969568903, -10.95106697391550021 ) ) ;
#3511 = ORIENTED_EDGE ( 'NONE', *, *, #35759, .T. ) ;
#3512 = EDGE_CURVE ( 'NONE', #29524, #25246, #13872, .T. ) ;
#3513 = CARTESIAN_POINT ( 'NONE',  ( 22.80793912684299229, 11.57402466465492097, -6.956843576774104143 ) ) ;
#3514 = CARTESIAN_POINT ( 'NONE',  ( 0.2651627682582897716, -4.271106202749196612, -11.47719223137564803 ) ) ;
#3515 = ORIENTED_EDGE ( 'NONE', *, *, #40168, .F. ) ;
#3516 = ORIENTED_EDGE ( 'NONE', *, *, #14940, .T. ) ;
#3517 = CARTESIAN_POINT ( 'NONE',  ( -22.66110217412718697, 0.1747008913564316313, -4.941631093908251948 ) ) ;
#3518 = VERTEX_POINT ( 'NONE', #63742 ) ;
#3519 = CARTESIAN_POINT ( 'NONE',  ( 0.4626703367445907378, -12.07256244737118145, -2.416235258139934672 ) ) ;
#3520 = CARTESIAN_POINT ( 'NONE',  ( -35.00000000000000000, 11.65150730582932503, 1.488153103997165605 ) ) ;
#3521 = CARTESIAN_POINT ( 'NONE',  ( 2.000000000000001776, 5.814643797626930954, 3.550179297009575574 ) ) ;
#3522 = DIRECTION ( 'NONE',  ( 1.000000000000000000, 0.000000000000000000, 0.000000000000000000 ) ) ;
#3523 =( BOUNDED_CURVE ( )  B_SPLINE_CURVE ( 3, ( #52338, #6779, #52663, #7088 ),
 .UNSPECIFIED., .F., .F. ) 
 B_SPLINE_CURVE_WITH_KNOTS ( ( 4, 4 ),
 ( 4.347126718975509618, 4.378220820213373443 ),
 .UNSPECIFIED. ) 
 CURVE ( )  GEOMETRIC_REPRESENTATION_ITEM ( )  RATIONAL_B_SPLINE_CURVE ( ( 1.000000000000000000, 0.9999194313618959828, 0.9999194313618959828, 1.000000000000000000 ) ) 
 REPRESENTATION_ITEM ( '' )  );
#3524 = B_SPLINE_CURVE_WITH_KNOTS ( 'NONE', 3,
 ( #22726, #3107, #37995, #38982, #33985, #23049, #58973, #58643, #22372, #33669, #28676, #43309, #48989, #42638, #3447, #62943 ),
 .UNSPECIFIED., .F., .F.,
 ( 4, 3, 3, 3, 3, 4 ),
 ( 4.336808689942017736E-19, 0.0002176109881720242952, 0.0004352086762394619134, 0.0006528017811446884837, 0.0007615147961451716263, 0.0009453342004943081529 ),
 .UNSPECIFIED. ) ;
#3525 = DIRECTION ( 'NONE',  ( 1.000000000000000000, 0.000000000000000000, 0.000000000000000000 ) ) ;
#3527 = ORIENTED_EDGE ( 'NONE', *, *, #24110, .F. ) ;
#3526 = FACE_OUTER_BOUND ( 'NONE', #40539, .T. ) ;
#3528 = DIRECTION ( 'NONE',  ( 1.000000000000000000, 0.000000000000000000, 0.000000000000000000 ) ) ;
#3529 = ORIENTED_EDGE ( 'NONE', *, *, #43547, .T. ) ;
#3530 = AXIS2_PLACEMENT_3D ( 'NONE', #42470, #2937, #27206 ) ;
#3531 = CARTESIAN_POINT ( 'NONE',  ( 35.00000000000000000, -1.771820996347075017, 11.61175578952787113 ) ) ;
#3532 = ORIENTED_EDGE ( 'NONE', *, *, #7872, .T. ) ;
#3533 = VECTOR ( 'NONE', #14513, 1000.000000000000000 ) ;
#3534 = ORIENTED_EDGE ( 'NONE', *, *, #37135, .F. ) ;
#3535 = CARTESIAN_POINT ( 'NONE',  ( -17.47216009470839282, 7.641999522472164408, 11.13043964233116334 ) ) ;
#3536 = CARTESIAN_POINT ( 'NONE',  ( -11.13200843151504849, -27.92871652161695550, 13.87829993151233943 ) ) ;
#3538 = CARTESIAN_POINT ( 'NONE',  ( -37.00000000000000711, 6.584150480049697940, -10.25474254703946109 ) ) ;
#3537 = AXIS2_PLACEMENT_3D ( 'NONE', #37145, #1914, #62408 ) ;
#3539 = EDGE_CURVE ( 'NONE', #60178, #37749, #16931, .T. ) ;
#3540 = DIRECTION ( 'NONE',  ( 0.000000000000000000, 0.6876994588534192099, 0.7259954919231347281 ) ) ;
#3541 = CARTESIAN_POINT ( 'NONE',  ( -37.00000000000000711, 8.366449238204365813, 9.621072037177027525 ) ) ;
#3542 = CARTESIAN_POINT ( 'NONE',  ( 2.288423627606496868, 5.962686897378696393, 4.792733268640499311 ) ) ;
#3543 = ORIENTED_EDGE ( 'NONE', *, *, #61845, .F. ) ;
#3544 = EDGE_CURVE ( 'NONE', #44459, #12705, #29180, .T. ) ;
#3545 = LINE ( 'NONE', #18815, #65467 ) ;
#3546 = EDGE_LOOP ( 'NONE', ( #7831, #26719, #1155, #24190 ) ) ;
#3547 = CARTESIAN_POINT ( 'NONE',  ( 35.00000000000000000, 4.705694406421931860E-17, -3.469127814946512892E-15 ) ) ;
#3548 = VECTOR ( 'NONE', #27012, 1000.000000000000000 ) ;
#3549 = DIRECTION ( 'NONE',  ( 0.000000000000000000, 0.000000000000000000, 1.000000000000000000 ) ) ;
#3550 = ORIENTED_EDGE ( 'NONE', *, *, #58564, .T. ) ;
#3551 = AXIS2_PLACEMENT_3D ( 'NONE', #1830, #17113, #2502 ) ;
#3552 = EDGE_CURVE ( 'NONE', #36795, #34842, #51024, .T. ) ;
#3553 = DIRECTION ( 'NONE',  ( 0.000000000000000000, -0.9718671068226434340, 0.2355298848897617037 ) ) ;
#3554 = CARTESIAN_POINT ( 'NONE',  ( 0.3106921474978440734, -10.49891314301081735, -6.333448016104161304 ) ) ;
#3555 = DIRECTION ( 'NONE',  ( 0.000000000000000000, 0.000000000000000000, 1.000000000000000000 ) ) ;
#3556 = CARTESIAN_POINT ( 'NONE',  ( 29.51976981715666781, 7.690765383426390045, 11.09513982864076276 ) ) ;
#3557 = AXIS2_PLACEMENT_3D ( 'NONE', #51444, #57389, #11816 ) ;
#3558 = CYLINDRICAL_SURFACE ( 'NONE', #45832, 5.000000000000000888 ) ;
#3559 = CARTESIAN_POINT ( 'NONE',  ( 2.241311220309555097, 3.897297589552074282, -6.564680916077756834 ) ) ;
#3560 = ORIENTED_EDGE ( 'NONE', *, *, #15162, .T. ) ;
#3561 = EDGE_LOOP ( 'NONE', ( #1606, #2702, #10604, #22563 ) ) ;
#3562 = VECTOR ( 'NONE', #15614, 1000.000000000000000 ) ;
#3563 = EDGE_CURVE ( 'NONE', #39575, #47639, #22456, .T. ) ;
#3564 = DIRECTION ( 'NONE',  ( 1.000000000000000000, 0.000000000000000000, 0.000000000000000000 ) ) ;
#3565 = EDGE_CURVE ( 'NONE', #52756, #35052, #34053, .T. ) ;
#3566 = DIRECTION ( 'NONE',  ( -1.000000000000000000, 0.000000000000000000, 0.000000000000000000 ) ) ;
#3567 = DIRECTION ( 'NONE',  ( 1.000000000000000000, 0.000000000000000000, -0.000000000000000000 ) ) ;
#3568 = EDGE_CURVE ( 'NONE', #54893, #21752, #50276, .T. ) ;
#3569 = DIRECTION ( 'NONE',  ( -1.000000000000000000, 0.000000000000000000, 0.000000000000000000 ) ) ;
#3570 = CIRCLE ( 'NONE', #48129, 5.000000000000000888 ) ;
#3571 = CARTESIAN_POINT ( 'NONE',  ( -27.69104391824479805, 10.87192706255359909, -8.023814012560558595 ) ) ;
#3572 = CARTESIAN_POINT ( 'NONE',  ( -47.00000000000000711, 0.000000000000000000, 0.000000000000000000 ) ) ;
#3573 = CARTESIAN_POINT ( 'NONE',  ( 2.241528039335008327, 5.858435878248576145, -4.895273998033944807 ) ) ;
#3574 = B_SPLINE_CURVE_WITH_KNOTS ( 'NONE', 3,
 ( #63001, #56378, #10825, #42055, #36426, #62338, #31110, #37066, #5873, #46406, #11794, #851, #17128, #52392, #6839, #47405, #1842, #38386, #23774, #44039, #17464, #54360, #43362, #13755 ),
 .UNSPECIFIED., .F., .F.,
 ( 4, 2, 2, 2, 2, 2, 2, 2, 2, 2, 2, 4 ),
 ( 0.000000000000000000, 0.0005610479560808320819, 0.001122095912161664164, 0.001683143868242496137, 0.002244191824323328328, 0.003366287736484988805, 0.003927335692565820345, 0.004488383648646649716, 0.005610479560808312796, 0.006732575472969976743, 0.007854671385131640690, 0.008976767297293304637 ),
 .UNSPECIFIED. ) ;
#3575 = CARTESIAN_POINT ( 'NONE',  ( 2.288423627607476973, 1.486973602181149712, 7.504187945869062126 ) ) ;
#3576 = CARTESIAN_POINT ( 'NONE',  ( 2.368238019615382495, -5.070835960312986224, -5.763545178420198312 ) ) ;
#3577 = B_SPLINE_CURVE_WITH_KNOTS ( 'NONE', 3,
 ( #64189, #33914, #3032, #24270, #43906, #34246, #23297, #59526, #8986, #44536, #38590, #58906, #53891, #8328, #64816, #19294 ),
 .UNSPECIFIED., .F., .F.,
 ( 4, 3, 3, 3, 3, 4 ),
 ( 0.000000000000000000, 0.0002176109881720251354, 0.0004352086762394620219, 0.0006528017811446910857, 0.0007615147961451749874, 0.0009453342004947290402 ),
 .UNSPECIFIED. ) ;
#3578 = ORIENTED_EDGE ( 'NONE', *, *, #18077, .F. ) ;
#3579 = AXIS2_PLACEMENT_3D ( 'NONE', #43688, #13112, #47703 ) ;
#3580 = CARTESIAN_POINT ( 'NONE',  ( -20.79170840334646542, 11.34110549087207076, -3.921648409140116698 ) ) ;
#3581 = CARTESIAN_POINT ( 'NONE',  ( -22.31328051695926007, -2.608921479762108753, 2.748895659348124187 ) ) ;
#3582 = CIRCLE ( 'NONE', #36490, 12.18649999999999700 ) ;
#3583 = DIRECTION ( 'NONE',  ( 0.000000000000000000, 0.01356324068817998940, -0.9999080150203990547 ) ) ;
#3584 = EDGE_CURVE ( 'NONE', #1539, #36570, #21294, .T. ) ;
#3585 = CIRCLE ( 'NONE', #36442, 12.74999999999999822 ) ;
#3586 = AXIS2_PLACEMENT_3D ( 'NONE', #43141, #7928, #3265 ) ;
#3587 = EDGE_CURVE ( 'NONE', #12178, #60093, #52113, .T. ) ;
#3588 = CARTESIAN_POINT ( 'NONE',  ( 2.242418902651939216, -0.09970190380427686183, -7.634109827927233027 ) ) ;
#3589 = CARTESIAN_POINT ( 'NONE',  ( 2.242819959140646358, -5.913965034148185751, 4.828731837260215265 ) ) ;
#3590 = EDGE_LOOP ( 'NONE', ( #62897, #38164, #17334, #15130 ) ) ;
#3591 = CARTESIAN_POINT ( 'NONE',  ( -22.66110217412718697, 4.941631093908234185, 0.1747008913564567778 ) ) ;
#3592 = CARTESIAN_POINT ( 'NONE',  ( 29.69944545120181090, 10.33295084604707448, 8.690866588745604915 ) ) ;
#3593 = AXIS2_PLACEMENT_3D ( 'NONE', #30922, #51571, #51885 ) ;
#3594 = CARTESIAN_POINT ( 'NONE',  ( -0.4223990570890304164, -27.81390085543024426, -12.58355210400658564 ) ) ;
#3595 = ORIENTED_EDGE ( 'NONE', *, *, #2287, .T. ) ;
#3596 = CARTESIAN_POINT ( 'NONE',  ( -11.13234721864718679, -5.599044822695524282, -12.29123017578099208 ) ) ;
#3597 = FACE_OUTER_BOUND ( 'NONE', #50287, .T. ) ;
#3598 = CARTESIAN_POINT ( 'NONE',  ( 17.30586438374871250, -10.58231581927869058, 8.416062268768557786 ) ) ;
#3599 = VECTOR ( 'NONE', #53857, 1000.000000000000000 ) ;
#3600 = CARTESIAN_POINT ( 'NONE',  ( 0.3675815128205894289, -8.093875121226139058, 9.235491948679980467 ) ) ;
#3601 = CARTESIAN_POINT ( 'NONE',  ( -9.368646887739329188, -10.53974709387553865, -8.470498924738002700 ) ) ;
#3602 = AXIS2_PLACEMENT_3D ( 'NONE', #33086, #57732, #52735 ) ;
#3603 = B_SPLINE_CURVE_WITH_KNOTS ( 'NONE', 3,
 ( #13066, #53313, #33350, #28354, #53960, #57978, #18057, #2101, #2450, #38321, #48340, #23369, #43638, #63928, #12388, #47655, #47996, #18729 ),
 .UNSPECIFIED., .F., .F.,
 ( 4, 2, 2, 2, 2, 2, 2, 2, 4 ),
 ( 0.000000000000000000, 0.002646377093913540243, 0.003307971367391926605, 0.003969565640870312967, 0.005292754187827087425, 0.006615942734783859282, 0.007939131281740631138, 0.009262319828697403862, 0.01058550837565417659 ),
 .UNSPECIFIED. ) ;
#3604 = DIRECTION ( 'NONE',  ( -1.000000000000000000, 0.000000000000000000, 0.000000000000000000 ) ) ;
#3605 = ORIENTED_EDGE ( 'NONE', *, *, #42483, .F. ) ;
#3606 = CYLINDRICAL_SURFACE ( 'NONE', #18532, 4.500000000000000888 ) ;
#3607 = DIRECTION ( 'NONE',  ( 0.000000000000000000, -0.01356324068817992522, 0.9999080150203990547 ) ) ;
#3608 = CARTESIAN_POINT ( 'NONE',  ( 0.000000000000000000, 0.000000000000000000, 0.000000000000000000 ) ) ;
#3609 = DIRECTION ( 'NONE',  ( 0.000000000000000000, -0.9868265225415244757, -0.1617819965527746984 ) ) ;
#3610 = CARTESIAN_POINT ( 'NONE',  ( 35.00000000000000000, -1.463443770872862482, -12.09831040184923978 ) ) ;
#3611 = LINE ( 'NONE', #44442, #49244 ) ;
#3612 = VECTOR ( 'NONE', #350, 1000.000000000000000 ) ;
#3613 = DIRECTION ( 'NONE',  ( -1.000000000000000000, 0.000000000000000000, 0.000000000000000000 ) ) ;
#3614 = CARTESIAN_POINT ( 'NONE',  ( -27.16408673750832747, -8.649729821182791767, -8.318274995791206550 ) ) ;
#3615 = EDGE_LOOP ( 'NONE', ( #11405, #58441, #39249, #9010 ) ) ;
#3616 = ORIENTED_EDGE ( 'NONE', *, *, #38696, .F. ) ;
#3617 = CARTESIAN_POINT ( 'NONE',  ( -19.42173080018139331, -4.342950793773034057, -11.18689537328631012 ) ) ;
#3618 = VERTEX_POINT ( 'NONE', #65698 ) ;
#3619 = CYLINDRICAL_SURFACE ( 'NONE', #39737, 12.74999999999999822 ) ;
#3620 = CARTESIAN_POINT ( 'NONE',  ( 35.00000000000000000, -10.30098186818245409, 5.644643009979177783 ) ) ;
#3621 = AXIS2_PLACEMENT_3D ( 'NONE', #13550, #48502, #2954 ) ;
#3622 = CARTESIAN_POINT ( 'NONE',  ( -22.29115169517546136, -1.614783311161199109, 3.355084543108113326 ) ) ;
#3623 = VERTEX_POINT ( 'NONE', #51102 ) ;
#3624 = CARTESIAN_POINT ( 'NONE',  ( 0.2739690278137255630, 5.965352196073746782, -10.69833303470758601 ) ) ;
#3625 = EDGE_CURVE ( 'NONE', #29278, #19802, #1135, .T. ) ;
#3626 = CARTESIAN_POINT ( 'NONE',  ( 0.3665391374699465965, -11.62960183138724446, -3.952034409876413079 ) ) ;
#3627 = CARTESIAN_POINT ( 'NONE',  ( 24.84806924723610067, -1.530817552018350014, 13.41866073552183103 ) ) ;
#3628 = ORIENTED_EDGE ( 'NONE', *, *, #25198, .F. ) ;
#3629 = ORIENTED_EDGE ( 'NONE', *, *, #55805, .T. ) ;
#3630 = DIRECTION ( 'NONE',  ( -1.000000000000000000, 0.000000000000000000, 0.000000000000000000 ) ) ;
#3632 = CARTESIAN_POINT ( 'NONE',  ( 37.00000000000000711, 12.38385022362086119, 3.033604067594442899 ) ) ;
#3631 = AXIS2_PLACEMENT_3D ( 'NONE', #25626, #40927, #3492 ) ;
#3633 = CIRCLE ( 'NONE', #18480, 4.999999999999998224 ) ;
#3634 = EDGE_LOOP ( 'NONE', ( #21382, #38910, #34269, #39006 ) ) ;
#3635 = VERTEX_POINT ( 'NONE', #46118 ) ;
#3636 = CARTESIAN_POINT ( 'NONE',  ( -35.00000000000000000, 0.000000000000000000, 0.000000000000000000 ) ) ;
#3637 = DIRECTION ( 'NONE',  ( 0.000000000000000000, -0.6745969609292555846, -0.7381862504172050921 ) ) ;
#3638 = AXIS2_PLACEMENT_3D ( 'NONE', #48796, #38133, #58443 ) ;
#3639 = CARTESIAN_POINT ( 'NONE',  ( 35.00000000000000000, 4.705694406421931860E-17, -3.469127814946512892E-15 ) ) ;
#3641 = EDGE_CURVE ( 'NONE', #46339, #56916, #40441, .T. ) ;
#3640 = CARTESIAN_POINT ( 'NONE',  ( 0.2648321136542728382, 7.979621084888234961, -9.289286523730330813 ) ) ;
#3642 = CARTESIAN_POINT ( 'NONE',  ( 2.000000000000001776, 1.058508696394974358, 6.730038252034905355 ) ) ;
#3643 = LINE ( 'NONE', #23908, #59888 ) ;
#3644 = ORIENTED_EDGE ( 'NONE', *, *, #18240, .T. ) ;
#3645 = CARTESIAN_POINT ( 'NONE',  ( 37.00000000000000711, -10.80631716521670427, -4.603882218679513194 ) ) ;
#3647 = CARTESIAN_POINT ( 'NONE',  ( -15.47692202957099461, 7.964177873487604309, 8.976325883789177951 ) ) ;
#3646 = VECTOR ( 'NONE', #54082, 1000.000000000000000 ) ;
#3648 = CARTESIAN_POINT ( 'NONE',  ( 0.2653519890538384995, 1.477274386607676477E-15, 12.24619734961521189 ) ) ;
#3649 = CARTESIAN_POINT ( 'NONE',  ( 2.000000000000001776, -5.662015959325143122, -4.918493191654053298 ) ) ;
#3650 = CARTESIAN_POINT ( 'NONE',  ( -16.66082797316812503, -33.00000000000000000, 4.257284274447473926 ) ) ;
#3651 = AXIS2_PLACEMENT_3D ( 'NONE', #41736, #5871, #26127 ) ;
#3652 = CARTESIAN_POINT ( 'NONE',  ( -27.08588607604449550, 1.616144682268094268, -1.631236259433592073 ) ) ;
#3653 = DIRECTION ( 'NONE',  ( -1.000000000000000000, 0.000000000000000000, 0.000000000000000000 ) ) ;
#3654 = CARTESIAN_POINT ( 'NONE',  ( 22.36482863261543486, -11.96441317219524514, -0.9234811557364158707 ) ) ;
#3655 = CARTESIAN_POINT ( 'NONE',  ( 1.549075743843706832, 5.743768701987367109, 11.29795072957420032 ) ) ;
#3656 = AXIS2_PLACEMENT_3D ( 'NONE', #63929, #33351, #58644 ) ;
#3657 = ORIENTED_EDGE ( 'NONE', *, *, #19108, .F. ) ;
#3658 = CARTESIAN_POINT ( 'NONE',  ( -16.86326112465461335, 8.068804307413738997, -8.883526352222181899 ) ) ;
#3659 = ORIENTED_EDGE ( 'NONE', *, *, #17187, .T. ) ;
#3660 = CYLINDRICAL_SURFACE ( 'NONE', #9377, 5.000000000000000888 ) ;
#3661 = CARTESIAN_POINT ( 'NONE',  ( 35.00000000000000000, -8.052525312709825300, 8.551552972817161091 ) ) ;
#3662 = AXIS2_PLACEMENT_3D ( 'NONE', #50150, #61098, #4605 ) ;
#3663 = LINE ( 'NONE', #38204, #33489 ) ;
#3664 = CARTESIAN_POINT ( 'NONE',  ( -25.64778288570172649, -7.682669607182212701, 11.10295593026794592 ) ) ;
#3665 = CARTESIAN_POINT ( 'NONE',  ( 2.305787727787084407, 5.047606869483056258, 5.756228004061473946 ) ) ;
#3666 = ORIENTED_EDGE ( 'NONE', *, *, #6794, .F. ) ;
#3667 = CARTESIAN_POINT ( 'NONE',  ( -22.27834755396594346, 3.643689482009642155, -0.5583491773602359265 ) ) ;
#3668 = DIRECTION ( 'NONE',  ( 1.000000000000000000, 0.000000000000000000, 0.000000000000000000 ) ) ;
#3669 = CARTESIAN_POINT ( 'NONE',  ( -37.00000000000000711, 0.000000000000000000, 0.000000000000000000 ) ) ;
#3670 = ADVANCED_FACE ( 'NONE', ( #5558 ), #45121, .T. ) ;
#3671 = AXIS2_PLACEMENT_3D ( 'NONE', #45984, #4784, #25047 ) ;
#3672 = CARTESIAN_POINT ( 'NONE',  ( 2.000000000000001776, 6.767909380267608022, -0.7805499053121014441 ) ) ;
#3673 = VERTEX_POINT ( 'NONE', #19533 ) ;
#3674 = CARTESIAN_POINT ( 'NONE',  ( 0.000000000000000000, 0.000000000000000000, 0.000000000000000000 ) ) ;
#3675 = ORIENTED_EDGE ( 'NONE', *, *, #42785, .T. ) ;
#3676 = CARTESIAN_POINT ( 'NONE',  ( 2.717984159218978402, 5.783767685176879780, -5.223388265379605322 ) ) ;
#3677 = CARTESIAN_POINT ( 'NONE',  ( 35.00000000000000000, -10.25474254703957477, -6.584150480049516752 ) ) ;
#3678 = AXIS2_PLACEMENT_3D ( 'NONE', #13140, #29722, #24759 ) ;
#3679 = CIRCLE ( 'NONE', #16418, 2.899999999999995470 ) ;
#3680 = CARTESIAN_POINT ( 'NONE',  ( 35.00000000000000000, 4.705694406421931860E-17, -3.469127814946512892E-15 ) ) ;
#3681 = CARTESIAN_POINT ( 'NONE',  ( 1.719304012339819332, -7.581471372739574832, 10.22720798541442555 ) ) ;
#3682 = ADVANCED_FACE ( 'NONE', ( #40791 ), #19847, .T. ) ;
#3683 = ORIENTED_EDGE ( 'NONE', *, *, #32481, .F. ) ;
#3684 = VERTEX_POINT ( 'NONE', #40108 ) ;
#3685 = CARTESIAN_POINT ( 'NONE',  ( 2.000000000000001776, 0.000000000000000000, 0.000000000000000000 ) ) ;
#3686 = CARTESIAN_POINT ( 'NONE',  ( 2.266490820343017631, 5.023127813992001478, 5.760233951938614538 ) ) ;
#3688 = VECTOR ( 'NONE', #23494, 1000.000000000000000 ) ;
#3687 = CARTESIAN_POINT ( 'NONE',  ( 35.00000000000000000, 10.42955799785319648, -6.303578524886984447 ) ) ;
#3689 = CARTESIAN_POINT ( 'NONE',  ( 0.2759803524722211909, 12.24828167798667522, 0.1894460813476448457 ) ) ;
#3690 = CARTESIAN_POINT ( 'NONE',  ( 3.152665057735501097, 6.622010822086128456, -4.377619405893580229 ) ) ;
#3691 = CARTESIAN_POINT ( 'NONE',  ( 5.536195898058073439, -0.007485416011287833460, 0.004027525919832407840 ) ) ;
#3692 = ORIENTED_EDGE ( 'NONE', *, *, #5414, .F. ) ;
#3693 = ORIENTED_EDGE ( 'NONE', *, *, #63432, .T. ) ;
#3694 = ORIENTED_EDGE ( 'NONE', *, *, #19384, .F. ) ;
#3695 = CARTESIAN_POINT ( 'NONE',  ( 2.268878695253353506, 7.231932316093202751, -2.474564429974424495 ) ) ;
#3696 = CIRCLE ( 'NONE', #40832, 12.75000000000000178 ) ;
#3697 = CARTESIAN_POINT ( 'NONE',  ( 35.00000000000000000, -11.73555825188272728, 4.983891302653700173 ) ) ;
#3698 = EDGE_CURVE ( 'NONE', #50756, #18994, #31917, .T. ) ;
#3699 = ORIENTED_EDGE ( 'NONE', *, *, #37989, .T. ) ;
#3700 = CARTESIAN_POINT ( 'NONE',  ( 0.000000000000000000, 3.224464355699827145, 6.771471746881979392 ) ) ;
#3701 = CARTESIAN_POINT ( 'NONE',  ( 35.00000000000000000, 4.705694406421931860E-17, -3.469127814946512892E-15 ) ) ;
#3702 = ORIENTED_EDGE ( 'NONE', *, *, #15172, .T. ) ;
#3703 = CARTESIAN_POINT ( 'NONE',  ( -23.18047892478189098, 2.738168160732706191, -3.933989833240143064 ) ) ;
#3704 = ADVANCED_FACE ( 'NONE', ( #10505 ), #31766, .T. ) ;
#3705 = AXIS2_PLACEMENT_3D ( 'NONE', #45704, #51383, #2471 ) ;
#3706 = CARTESIAN_POINT ( 'NONE',  ( 37.00000000000000711, 3.473736367725426266, 12.26766708251987836 ) ) ;
#3707 = DIRECTION ( 'NONE',  ( -1.000000000000000000, 0.000000000000000000, 0.000000000000000000 ) ) ;
#3708 = VERTEX_POINT ( 'NONE', #27440 ) ;
#3709 = ORIENTED_EDGE ( 'NONE', *, *, #39769, .F. ) ;
#3710 = CARTESIAN_POINT ( 'NONE',  ( 2.298277635560274756, 2.461898367585382719, 7.246601281227234459 ) ) ;
#3711 = ADVANCED_FACE ( 'NONE', ( #16506 ), #42076, .F. ) ;
#3712 = ORIENTED_EDGE ( 'NONE', *, *, #47263, .T. ) ;
#3713 = DIRECTION ( 'NONE',  ( 1.000000000000000000, 0.000000000000000000, 0.000000000000000000 ) ) ;
#3714 = ORIENTED_EDGE ( 'NONE', *, *, #50463, .T. ) ;
#3715 = ORIENTED_EDGE ( 'NONE', *, *, #33858, .T. ) ;
#3716 = EDGE_LOOP ( 'NONE', ( #26940, #57656, #59420, #63941 ) ) ;
#3717 = CARTESIAN_POINT ( 'NONE',  ( 35.00000000000000000, -0.01609748574436820068, 11.74614673114903596 ) ) ;
#3718 = CARTESIAN_POINT ( 'NONE',  ( -15.84367078532069861, -34.24835312396456999, -7.333865081863226720 ) ) ;
#3719 = AXIS2_PLACEMENT_3D ( 'NONE', #13896, #20206, #44177 ) ;
#3720 = DIRECTION ( 'NONE',  ( -0.3865475372811021937, 0.5778504531711138315, -0.7187975063895625238 ) ) ;
#3722 = EDGE_CURVE ( 'NONE', #51469, #36018, #12783, .T. ) ;
#3721 = CARTESIAN_POINT ( 'NONE',  ( 1.283627346227174337, 11.62704807385648209, -4.817767733507369421 ) ) ;
#3723 = CARTESIAN_POINT ( 'NONE',  ( 0.9296196016834723519, -0.4155906739599753430, 12.46069139398446168 ) ) ;
#3724 = ORIENTED_EDGE ( 'NONE', *, *, #20601, .F. ) ;
#3725 = CARTESIAN_POINT ( 'NONE',  ( 2.268878695253353062, -7.130600918714364411, -2.752970156154558978 ) ) ;
#3726 =( BOUNDED_SURFACE ( )  B_SPLINE_SURFACE ( 3, 1, ( 
 ( #47380, #28076 ),
 ( #37376, #43342 ),
 ( #47694, #7437 ),
 ( #27727, #58680 ) ),
 .UNSPECIFIED., .F., .F., .F. ) 
 B_SPLINE_SURFACE_WITH_KNOTS ( ( 4, 4 ),
 ( 2, 2 ),
 ( 0.000000000000000000, 1.000000000000000000 ),
 ( 0.000000000000000000, 1.000000000000000000 ),
 .UNSPECIFIED. ) 
 GEOMETRIC_REPRESENTATION_ITEM ( )  RATIONAL_B_SPLINE_SURFACE ( (
 ( 1.000000000000000000, 1.000000000000000000),
 ( 0.6933888150995267674, 0.9895912004443193632),
 ( 0.6933888150995267674, 0.9895912004443193632),
 ( 1.000000000000000000, 1.000000000000000000) ) ) 
 REPRESENTATION_ITEM ( '' )  SURFACE ( )  );
#3727 = ORIENTED_EDGE ( 'NONE', *, *, #57185, .T. ) ;
#3728 = FACE_OUTER_BOUND ( 'NONE', #24247, .T. ) ;
#3729 = EDGE_CURVE ( 'NONE', #58346, #32993, #57067, .T. ) ;
#3730 = DIRECTION ( 'NONE',  ( 0.000000000000000000, 0.000000000000000000, 1.000000000000000000 ) ) ;
#3731 = PRESENTATION_LAYER_ASSIGNMENT (  '', '', ( #31316 ) ) ;
#3732 = EDGE_LOOP ( 'NONE', ( #4401, #20527, #60849, #45202 ) ) ;
#3733 = CARTESIAN_POINT ( 'NONE',  ( 24.82652845881425208, 10.42385221765396608, -8.578654028722157321 ) ) ;
#3734 = CARTESIAN_POINT ( 'NONE',  ( 27.76606509001456047, 10.82004123774806104, 5.203714701047107205 ) ) ;
#3735 = CARTESIAN_POINT ( 'NONE',  ( 0.2651627682582899381, -9.437482589529922805, -7.803986935114110679 ) ) ;
#3736 = ORIENTED_EDGE ( 'NONE', *, *, #30183, .T. ) ;
#3737 = ORIENTED_EDGE ( 'NONE', *, *, #58121, .F. ) ;
#3738 = CARTESIAN_POINT ( 'NONE',  ( 0.9232167919969059833, 6.587352952801155404, 10.58277433962383718 ) ) ;
#3739 = EDGE_CURVE ( 'NONE', #43940, #42272, #871, .T. ) ;
#3740 = AXIS2_PLACEMENT_3D ( 'NONE', #6168, #63307, #57034 ) ;
#3741 = ORIENTED_EDGE ( 'NONE', *, *, #65425, .F. ) ;
#3742 = CARTESIAN_POINT ( 'NONE',  ( 35.00000000000000000, 7.817610399097634222, 8.766823244861901898 ) ) ;
#3743 = FACE_OUTER_BOUND ( 'NONE', #27761, .T. ) ;
#3744 = CARTESIAN_POINT ( 'NONE',  ( 5.514970785353741078, 0.004694330894494709236, 0.0005190732562555246078 ) ) ;
#3745 = CARTESIAN_POINT ( 'NONE',  ( 3.092491956585309953, 4.340140213817062609, 6.622742949902756138 ) ) ;
#3746 = CARTESIAN_POINT ( 'NONE',  ( 12.10998784662220729, 8.443435280036798218, -8.526922110106905706 ) ) ;
#3747 = VERTEX_POINT ( 'NONE', #11496 ) ;
#3748 = CARTESIAN_POINT ( 'NONE',  ( -37.00000000000000711, 11.73555825188283741, -4.983891302653459476 ) ) ;
#3749 = CARTESIAN_POINT ( 'NONE',  ( 2.177405672431837136, -10.01846874164949774, -5.005033771131442322 ) ) ;
#3750 = CIRCLE ( 'NONE', #19678, 1.499999999999998224 ) ;
#3751 = CARTESIAN_POINT ( 'NONE',  ( -17.37639885904427217, -8.896818990903957669, 8.082699191722323206 ) ) ;
#3752 = CARTESIAN_POINT ( 'NONE',  ( -22.65999102136915511, 4.797155153747065803, 0.5917351393134848703 ) ) ;
#3753 = CARTESIAN_POINT ( 'NONE',  ( 0.2650492433740060938, 7.955688793816089621, 9.309907554970001442 ) ) ;
#3754 = CARTESIAN_POINT ( 'NONE',  ( -35.00000000000000000, 0.000000000000000000, 0.000000000000000000 ) ) ;
#3755 = LINE ( 'NONE', #45266, #20498 ) ;
#3756 = B_SPLINE_CURVE_WITH_KNOTS ( 'NONE', 3,
 ( #16101, #41361, #46691, #45375, #1149, #4841, #30414, #50395 ),
 .UNSPECIFIED., .F., .F.,
 ( 4, 2, 2, 4 ),
 ( 8.673617379884035472E-19, 0.002119351272183964390, 0.003179026908275949404, 0.004238702544367933985 ),
 .UNSPECIFIED. ) ;
#3757 = ADVANCED_FACE ( 'NONE', ( #21142 ), #17484, .T. ) ;
#3758 = AXIS2_PLACEMENT_3D ( 'NONE', #10391, #45326, #34991 ) ;
#3759 = ORIENTED_EDGE ( 'NONE', *, *, #64613, .T. ) ;
#3760 = DIRECTION ( 'NONE',  ( -1.000000000000000000, 0.000000000000000000, 0.000000000000000000 ) ) ;
#3761 = ORIENTED_EDGE ( 'NONE', *, *, #40239, .T. ) ;
#3762 = DIRECTION ( 'NONE',  ( 0.000000000000000000, 0.01356324068817998940, -0.9999080150203989437 ) ) ;
#3763 = CARTESIAN_POINT ( 'NONE',  ( 36.00000000000000711, 12.71517666308947980, -0.9416912585474879194 ) ) ;
#3764 = CARTESIAN_POINT ( 'NONE',  ( 0.2651627682582916035, 6.199212018117441936, 10.56115808354085317 ) ) ;
#3765 = CARTESIAN_POINT ( 'NONE',  ( -36.00000000000000711, -8.235637554476577193, -9.733281772932251386 ) ) ;
#3766 = ORIENTED_EDGE ( 'NONE', *, *, #26056, .F. ) ;
#3767 = PRODUCT_DEFINITION_FORMATION_WITH_SPECIFIED_SOURCE ( 'ANY', '', #33856, .NOT_KNOWN. ) ;
#3768 = EDGE_LOOP ( 'NONE', ( #43729, #12929, #2649, #45049, #41030, #14374, #10511 ) ) ;
#3769 = ORIENTED_EDGE ( 'NONE', *, *, #55650, .T. ) ;
#3770 = CARTESIAN_POINT ( 'NONE',  ( 29.72939054355411770, -10.04502241635329618, 9.030387493296032630 ) ) ;
#3771 = EDGE_CURVE ( 'NONE', #42318, #41624, #9601, .T. ) ;
#3772 = ORIENTED_EDGE ( 'NONE', *, *, #53219, .T. ) ;
#3773 = CARTESIAN_POINT ( 'NONE',  ( -22.27713295444592845, -2.530364014314296472, -2.673940016109019879 ) ) ;
#3774 = CARTESIAN_POINT ( 'NONE',  ( 0.000000000000000000, 2.480520636974283821, -6.345145617221223944 ) ) ;
#3775 = CARTESIAN_POINT ( 'NONE',  ( 0.2834382757447981294, -9.254160138069011055, 8.029794915379529385 ) ) ;
#3776 = CARTESIAN_POINT ( 'NONE',  ( 5.514624014163232779, 0.004104370840204214776, -0.0005510299962886395586 ) ) ;
#3777 = EDGE_LOOP ( 'NONE', ( #65203, #65443, #9866, #50058 ) ) ;
#3778 = AXIS2_PLACEMENT_3D ( 'NONE', #57873, #7295, #47878 ) ;
#3779 = CARTESIAN_POINT ( 'NONE',  ( 35.00000000000000000, 3.213188559034240832, -11.29812557209478285 ) ) ;
#3780 = ADVANCED_FACE ( 'NONE', ( #47099 ), #42725, .T. ) ;
#3781 = CARTESIAN_POINT ( 'NONE',  ( 19.56743653832047869, -28.99999999999999289, 4.999999999999984901 ) ) ;
#3782 = DIRECTION ( 'NONE',  ( 0.000000000000000000, -0.01356324068818000848, 0.9999080150203990547 ) ) ;
#3784 = EDGE_LOOP ( 'NONE', ( #18917, #35647, #59782, #31930 ) ) ;
#3783 = CARTESIAN_POINT ( 'NONE',  ( 0.9232058338315048962, 2.536181247095527613, -12.21058493388770927 ) ) ;
#3785 = CARTESIAN_POINT ( 'NONE',  ( 0.3665391374699464300, -12.13918562134719714, 1.872534962004759551 ) ) ;
#3786 = ADVANCED_FACE ( 'NONE', ( #1554 ), #37758, .T. ) ;
#3787 = ORIENTED_EDGE ( 'NONE', *, *, #20519, .T. ) ;
#3788 = DIRECTION ( 'NONE',  ( -1.000000000000000000, 0.000000000000000000, 0.000000000000000000 ) ) ;
#3789 = ORIENTED_EDGE ( 'NONE', *, *, #32404, .F. ) ;
#3790 = DIRECTION ( 'NONE',  ( -1.000000000000000000, -0.000000000000000000, 0.000000000000000000 ) ) ;
#3791 = CARTESIAN_POINT ( 'NONE',  ( 0.3654063281920744699, 3.951404032559424184, -11.62642356802257559 ) ) ;
#3792 = CIRCLE ( 'NONE', #9071, 12.74999999999999822 ) ;
#3793 = FACE_OUTER_BOUND ( 'NONE', #15978, .T. ) ;
#3794 = DIRECTION ( 'NONE',  ( -1.000000000000000000, -1.836970198721029688E-16, -0.000000000000000000 ) ) ;
#3795 = CARTESIAN_POINT ( 'NONE',  ( 0.2958664285830430174, 9.529149585189953697, 7.708042451272207884 ) ) ;
#3796 = EDGE_CURVE ( 'NONE', #8191, #32188, #23289, .T. ) ;
#3797 = DIRECTION ( 'NONE',  ( 0.000000000000000000, -0.01356324068817991828, 0.9999080150203990547 ) ) ;
#3798 = CARTESIAN_POINT ( 'NONE',  ( 0.2869720083484345041, -3.994435966589990450, -11.58405933820305300 ) ) ;
#3800 = ORIENTED_EDGE ( 'NONE', *, *, #53495, .T. ) ;
#3799 = CARTESIAN_POINT ( 'NONE',  ( 0.2648978790185584908, -12.08224454301450201, 1.996248716311589400 ) ) ;
#3801 = VERTEX_POINT ( 'NONE', #1862 ) ;
#3802 = CARTESIAN_POINT ( 'NONE',  ( 0.000000000000000000, 6.777474576704075382, -0.6925993764990371337 ) ) ;
#3803 = ORIENTED_EDGE ( 'NONE', *, *, #57741, .F. ) ;
#3804 = EDGE_CURVE ( 'NONE', #46970, #28685, #22131, .T. ) ;
#3805 = EDGE_LOOP ( 'NONE', ( #45295, #41670, #183, #28266 ) ) ;
#3806 = CARTESIAN_POINT ( 'NONE',  ( 0.2655924914740778187, 6.161287456391830730, -10.58356227062103017 ) ) ;
#3807 = FACE_OUTER_BOUND ( 'NONE', #34565, .T. ) ;
#3808 = FACE_OUTER_BOUND ( 'NONE', #56333, .T. ) ;
#3809 = DIRECTION ( 'NONE',  ( -0.3865475372811021937, 0.01937500237528418795, 0.9220659470476462172 ) ) ;
#3810 = EDGE_CURVE ( 'NONE', #40981, #64820, #53048, .T. ) ;
#3811 = CARTESIAN_POINT ( 'NONE',  ( 0.2655924914740778187, -7.838010948424984470, -9.409507842006103573 ) ) ;
#3812 = CARTESIAN_POINT ( 'NONE',  ( 0.2706063244538042811, 10.69357582853954902, -5.971590789837406987 ) ) ;
#3813 = AXIS2_PLACEMENT_3D ( 'NONE', #63470, #49206, #53851 ) ;
#3814 = CARTESIAN_POINT ( 'NONE',  ( -35.00000000000000000, 0.000000000000000000, 0.000000000000000000 ) ) ;
#3815 = EDGE_CURVE ( 'NONE', #125, #10128, #57733, .T. ) ;
#3816 = ORIENTED_EDGE ( 'NONE', *, *, #62229, .F. ) ;
#3817 = DIRECTION ( 'NONE',  ( -1.000000000000000000, 0.000000000000000000, 0.000000000000000000 ) ) ;
#3818 = ADVANCED_FACE ( 'NONE', ( #28425 ), #13143, .T. ) ;
#3819 = CARTESIAN_POINT ( 'NONE',  ( 2.290907136833253421, -5.755317856506250607, -5.041121061899964673 ) ) ;
#3820 = CARTESIAN_POINT ( 'NONE',  ( -17.34810147968408955, -8.828308823152831053, 10.23480574679286548 ) ) ;
#3821 = VERTEX_POINT ( 'NONE', #29102 ) ;
#3822 = CIRCLE ( 'NONE', #21843, 2.899999999999994582 ) ;
#3823 = CARTESIAN_POINT ( 'NONE',  ( 25.00000000000000711, -3.797884998337192286, -25.00000000000000000 ) ) ;
#3824 = CARTESIAN_POINT ( 'NONE',  ( -37.00000000000000711, -0.1414404973751262617, -12.74921544981111410 ) ) ;
#3825 = VERTEX_POINT ( 'NONE', #43384 ) ;
#3826 = CYLINDRICAL_SURFACE ( 'NONE', #63790, 4.999999999999999112 ) ;
#3827 = LINE ( 'NONE', #3498, #18715 ) ;
#3828 = DIRECTION ( 'NONE',  ( 1.000000000000000000, 0.000000000000000000, 0.000000000000000000 ) ) ;
#3829 = ADVANCED_FACE ( 'NONE', ( #38745 ), #19113, .T. ) ;
#3830 = CARTESIAN_POINT ( 'NONE',  ( -47.00000000000000711, 0.000000000000000000, 0.000000000000000000 ) ) ;
#3831 = DIRECTION ( 'NONE',  ( -1.000000000000000000, -0.000000000000000000, 0.000000000000000000 ) ) ;
#3832 = ORIENTED_EDGE ( 'NONE', *, *, #46902, .F. ) ;
#3833 = DIRECTION ( 'NONE',  ( -1.000000000000000000, -0.000000000000000000, 0.000000000000000000 ) ) ;
#3834 = CARTESIAN_POINT ( 'NONE',  ( -9.792688973508125727, -10.81058943113889015, -5.226288967600182467 ) ) ;
#3835 = DIRECTION ( 'NONE',  ( -1.000000000000000000, 0.000000000000000000, 0.000000000000000000 ) ) ;
#3836 = ORIENTED_EDGE ( 'NONE', *, *, #6757, .F. ) ;
#3837 = CARTESIAN_POINT ( 'NONE',  ( 0.000000000000000000, 0.000000000000000000, 0.000000000000000000 ) ) ;
#3838 = CARTESIAN_POINT ( 'NONE',  ( 0.2653141617321015944, -4.147035654172644747, -11.52265685897333647 ) ) ;
#3839 = ORIENTED_EDGE ( 'NONE', *, *, #20406, .F. ) ;
#3840 = EDGE_CURVE ( 'NONE', #3821, #38649, #55802, .T. ) ;
#3841 = ORIENTED_EDGE ( 'NONE', *, *, #37598, .F. ) ;
#3842 = DIRECTION ( 'NONE',  ( 0.000000000000000000, -0.01356324068818000328, 0.9999080150203990547 ) ) ;
#3843 = EDGE_CURVE ( 'NONE', #61427, #9266, #48729, .T. ) ;
#3844 = ORIENTED_EDGE ( 'NONE', *, *, #16582, .F. ) ;
#3845 = CARTESIAN_POINT ( 'NONE',  ( 0.6511581176963612272, -12.12498040206541994, -2.473966499148246179 ) ) ;
#3846 = CARTESIAN_POINT ( 'NONE',  ( 37.00000000000000711, 0.9416912585476251429, 12.71517666308946382 ) ) ;
#3847 = CARTESIAN_POINT ( 'NONE',  ( 0.2956976708475438365, -6.317697191869704021, 10.50256636126824361 ) ) ;
#3848 = CARTESIAN_POINT ( 'NONE',  ( 35.00000000000000000, 4.705694406421931860E-17, -3.469127814946512892E-15 ) ) ;
#3849 = CARTESIAN_POINT ( 'NONE',  ( -22.28506771379528573, -3.348518833762381686, -1.636577531579577416 ) ) ;
#3851 = ORIENTED_EDGE ( 'NONE', *, *, #17190, .T. ) ;
#3850 = DIRECTION ( 'NONE',  ( 0.000000000000000000, -0.2960891610144378849, -0.9551603052523520709 ) ) ;
#3852 = CYLINDRICAL_SURFACE ( 'NONE', #59649, 12.75000000000000178 ) ;
#3853 = ADVANCED_FACE ( 'NONE', ( #7484 ), #33087, .F. ) ;
#3854 = ORIENTED_EDGE ( 'NONE', *, *, #3002, .F. ) ;
#3855 = DIRECTION ( 'NONE',  ( 1.000000000000000000, 0.000000000000000000, 0.000000000000000000 ) ) ;
#3856 = ORIENTED_EDGE ( 'NONE', *, *, #59311, .F. ) ;
#3857 = ORIENTED_EDGE ( 'NONE', *, *, #39106, .F. ) ;
#3858 = LINE ( 'NONE', #13465, #33688 ) ;
#3859 = CARTESIAN_POINT ( 'NONE',  ( 2.128776824815523216, -26.59425375115992907, 16.16470972310802523 ) ) ;
#3860 = CARTESIAN_POINT ( 'NONE',  ( -3.762642749413128485, 7.436900049367464405, 9.428156105167504464 ) ) ;
#3861 = CARTESIAN_POINT ( 'NONE',  ( 24.05602761403608270, -2.477051208052090558, 11.74280428119080355 ) ) ;
#3862 = AXIS2_PLACEMENT_3D ( 'NONE', #16676, #54232, #64206 ) ;
#3863 = CARTESIAN_POINT ( 'NONE',  ( 35.00000000000000000, -5.672855678558609505, 10.28547182238013669 ) ) ;
#3864 = CARTESIAN_POINT ( 'NONE',  ( 2.273267844203308741, 5.952585402746135124, 4.797225296801178374 ) ) ;
#3865 = VERTEX_POINT ( 'NONE', #18489 ) ;
#3866 = ORIENTED_EDGE ( 'NONE', *, *, #48987, .F. ) ;
#3867 = CARTESIAN_POINT ( 'NONE',  ( -27.05874794189610455, 1.836970198720914070E-16, -1.500000000000008882 ) ) ;
#3868 = ORIENTED_EDGE ( 'NONE', *, *, #11142, .T. ) ;
#3869 = DIRECTION ( 'NONE',  ( 0.000000000000000000, 0.4380125133593913422, -0.8989688749565187820 ) ) ;
#3870 = DIRECTION ( 'NONE',  ( 0.000000000000000000, 0.000000000000000000, 1.000000000000000000 ) ) ;
#3871 = CYLINDRICAL_SURFACE ( 'NONE', #62863, 2.899999999999994582 ) ;
#3872 = EDGE_CURVE ( 'NONE', #9460, #815, #53390, .T. ) ;
#3873 = CARTESIAN_POINT ( 'NONE',  ( 35.00000000000000000, 9.926225166347027340, -6.280308599560179061 ) ) ;
#3874 = FACE_OUTER_BOUND ( 'NONE', #25209, .T. ) ;
#3875 = EDGE_CURVE ( 'NONE', #30274, #48764, #26612, .T. ) ;
#3876 = CARTESIAN_POINT ( 'NONE',  ( 22.36482863261543486, 25.00000000000000000, -0.9234811557364158707 ) ) ;
#3877 = VERTEX_POINT ( 'NONE', #23118 ) ;
#3878 = VERTEX_POINT ( 'NONE', #18797 ) ;
#3879 = EDGE_CURVE ( 'NONE', #24723, #27863, #22330, .T. ) ;
#3880 = CARTESIAN_POINT ( 'NONE',  ( 0.9296196016823239372, 3.871279966920111448, 11.85136013468979144 ) ) ;
#3881 = CARTESIAN_POINT ( 'NONE',  ( 2.000000000000001776, -5.769711778877296027, -4.791703871138604853 ) ) ;
#3882 = CARTESIAN_POINT ( 'NONE',  ( -34.00000000000000000, 11.99999999999999822, 1.469576158976823750E-15 ) ) ;
#3883 = ORIENTED_EDGE ( 'NONE', *, *, #40939, .F. ) ;
#3884 = CARTESIAN_POINT ( 'NONE',  ( -28.21800245578230815, 12.11161220946422290, -5.971072691807515653 ) ) ;
#3885 = CARTESIAN_POINT ( 'NONE',  ( -8.782159582855564750, -2.870306520432511554, -11.65443128345066626 ) ) ;
#3886 = CARTESIAN_POINT ( 'NONE',  ( -37.00000000000000711, 0.000000000000000000, 0.000000000000000000 ) ) ;
#3887 = CYLINDRICAL_SURFACE ( 'NONE', #165, 7.499999999999988454 ) ;
#3888 = DIRECTION ( 'NONE',  ( -1.000000000000000000, 0.000000000000000000, -0.000000000000000000 ) ) ;
#3889 = VERTEX_POINT ( 'NONE', #38408 ) ;
#3890 = LINE ( 'NONE', #59735, #16567 ) ;
#3891 = CARTESIAN_POINT ( 'NONE',  ( 0.2646305136544065406, -12.03696649559613263, -2.256625640822439216 ) ) ;
#3892 = DIRECTION ( 'NONE',  ( -1.000000000000000000, 0.000000000000000000, 0.000000000000000000 ) ) ;
#3893 = B_SPLINE_CURVE_WITH_KNOTS ( 'NONE', 3,
 ( #8354, #28971, #63873, #12348, #18010, #38947, #37951, #33941, #32951, #53261, #28313, #54250, #18689, #58595, #33301, #57935 ),
 .UNSPECIFIED., .F., .F.,
 ( 4, 3, 3, 3, 3, 4 ),
 ( 2.799023667439389453E-15, 0.0002126834539180046070, 0.0004253519300366957962, 0.0006380165497225226412, 0.0007442707582429485729, 0.0009453531351410136277 ),
 .UNSPECIFIED. ) ;
#3894 = EDGE_CURVE ( 'NONE', #12199, #11505, #11743, .T. ) ;
#3895 = AXIS2_PLACEMENT_3D ( 'NONE', #44058, #64326, #29100 ) ;
#3896 = CARTESIAN_POINT ( 'NONE',  ( 2.368238019615179990, -3.681632831800436101, 6.736275681109117563 ) ) ;
#3897 = EDGE_CURVE ( 'NONE', #7867, #29014, #23794, .T. ) ;
#3898 = CARTESIAN_POINT ( 'NONE',  ( 2.268878695253352618, -5.949442550447433753, 4.798796461778030320 ) ) ;
#3899 =( BOUNDED_SURFACE ( )  B_SPLINE_SURFACE ( 3, 1, ( 
 ( #35912, #19349 ),
 ( #14982, #35606 ),
 ( #45927, #10019 ),
 ( #35271, #34615 ) ),
 .UNSPECIFIED., .F., .F., .F. ) 
 B_SPLINE_SURFACE_WITH_KNOTS ( ( 4, 4 ),
 ( 2, 2 ),
 ( 0.000000000000000000, 1.000000000000000000 ),
 ( 0.000000000000000000, 1.000000000000000000 ),
 .UNSPECIFIED. ) 
 GEOMETRIC_REPRESENTATION_ITEM ( )  RATIONAL_B_SPLINE_SURFACE ( (
 ( 1.000000000000000000, 1.000000000000000000),
 ( 0.9257577194822556033, 0.9980522942447415113),
 ( 0.9257577194822556033, 0.9980522942447415113),
 ( 1.000000000000000000, 1.000000000000000000) ) ) 
 REPRESENTATION_ITEM ( '' )  SURFACE ( )  );
#3900 = ORIENTED_EDGE ( 'NONE', *, *, #53832, .T. ) ;
#3901 = CARTESIAN_POINT ( 'NONE',  ( 5.516018279890452902, -0.005752102158674371642, -0.003580555109620855384 ) ) ;
#3902 = CARTESIAN_POINT ( 'NONE',  ( -11.13200843151504849, -27.03228069553586010, -13.43438493493725616 ) ) ;
#3903 = VERTEX_POINT ( 'NONE', #8155 ) ;
#3904 = CARTESIAN_POINT ( 'NONE',  ( 0.4626703367443995019, -6.399577980714719061, 10.51809671647419364 ) ) ;
#3905 = DIRECTION ( 'NONE',  ( -1.000000000000000000, 0.000000000000000000, 0.000000000000000000 ) ) ;
#3906 = CARTESIAN_POINT ( 'NONE',  ( 16.78263030916553333, -12.17295508002144011, 5.836879698929882565 ) ) ;
#3907 = EDGE_CURVE ( 'NONE', #5798, #48006, #44060, .T. ) ;
#3908 = CARTESIAN_POINT ( 'NONE',  ( -47.00000000000000711, 0.000000000000000000, 0.000000000000000000 ) ) ;
#3909 = CARTESIAN_POINT ( 'NONE',  ( -37.00000000000000711, -2.216820770815165265, 11.53507381115582575 ) ) ;
#3910 = DIRECTION ( 'NONE',  ( 0.000000000000000000, -0.8515178078024812081, 0.5243256840888652626 ) ) ;
#3911 = ORIENTED_EDGE ( 'NONE', *, *, #24453, .F. ) ;
#3912 = CARTESIAN_POINT ( 'NONE',  ( 2.290907136833250313, -7.243397831411269472, 2.463690939638650601 ) ) ;
#3913 = CARTESIAN_POINT ( 'NONE',  ( 0.9232058338315048962, -2.536181247095447677, 12.21058493388772881 ) ) ;
#3914 = DIRECTION ( 'NONE',  ( -1.000000000000000000, 0.000000000000000000, -0.000000000000000000 ) ) ;
#3915 = CARTESIAN_POINT ( 'NONE',  ( 1.719304012339869514, -10.22720798541492471, 7.581471372739622794 ) ) ;
#3916 = CARTESIAN_POINT ( 'NONE',  ( 2.241352910868909643, 7.532448145350525870, -1.243507963608017075 ) ) ;
#3917 = DIRECTION ( 'NONE',  ( 0.000000000000000000, -0.9847383929261599445, 0.1740410799127720953 ) ) ;
#3918 = CARTESIAN_POINT ( 'NONE',  ( -29.28143770085004505, 2.978801202832155326, -11.65275938077009066 ) ) ;
#3919 = DIRECTION ( 'NONE',  ( 0.000000000000000000, -1.000000000000000000, 0.000000000000000000 ) ) ;
#3920 = ORIENTED_EDGE ( 'NONE', *, *, #25974, .F. ) ;
#3921 = EDGE_CURVE ( 'NONE', #36432, #3157, #13773, .T. ) ;
#3922 = ORIENTED_EDGE ( 'NONE', *, *, #54696, .F. ) ;
#3923 = LINE ( 'NONE', #58818, #22566 ) ;
#3924 = VERTEX_POINT ( 'NONE', #55008 ) ;
#3925 = EDGE_CURVE ( 'NONE', #14535, #41991, #42536, .T. ) ;
#3926 = DIRECTION ( 'NONE',  ( -1.000000000000000000, 0.000000000000000000, 0.000000000000000000 ) ) ;
#3927 = LINE ( 'NONE', #34490, #17099 ) ;
#3928 = ORIENTED_EDGE ( 'NONE', *, *, #5131, .F. ) ;
#3929 = CARTESIAN_POINT ( 'NONE',  ( 2.276905613633646297, 6.543460433228703188, -3.955794200962136298 ) ) ;
#3930 = DIRECTION ( 'NONE',  ( -1.000000000000000000, -0.000000000000000000, 0.000000000000000000 ) ) ;
#3931 = ORIENTED_EDGE ( 'NONE', *, *, #32100, .F. ) ;
#3932 = ORIENTED_EDGE ( 'NONE', *, *, #11915, .T. ) ;
#3933 = LINE ( 'NONE', #20187, #7717 ) ;
#3934 = DIRECTION ( 'NONE',  ( 1.000000000000000000, 0.000000000000000000, 0.000000000000000000 ) ) ;
#3935 = ORIENTED_EDGE ( 'NONE', *, *, #24653, .F. ) ;
#3936 = CIRCLE ( 'NONE', #753, 5.000000000000001776 ) ;
#3937 = CARTESIAN_POINT ( 'NONE',  ( -35.00000000000000000, -12.66641127287624968, -1.457575200925677494 ) ) ;
#3938 = ORIENTED_EDGE ( 'NONE', *, *, #2595, .T. ) ;
#3939 = CARTESIAN_POINT ( 'NONE',  ( -19.56743653832047158, -33.00000000000000000, 5.000000000000000888 ) ) ;
#3940 = ADVANCED_FACE ( 'NONE', ( #20094 ), #54708, .F. ) ;
#3941 = CARTESIAN_POINT ( 'NONE',  ( 2.000000000000001776, 0.000000000000000000, 7.500000000000000000 ) ) ;
#3942 = CARTESIAN_POINT ( 'NONE',  ( 2.705197763288542667, -4.134294772209968549, 6.601241161176667482 ) ) ;
#3943 = CARTESIAN_POINT ( 'NONE',  ( 37.00000000000000711, -10.01317267707881342, 6.946017217730045878 ) ) ;
#3944 = CIRCLE ( 'NONE', #26241, 12.74999999999999822 ) ;
#3945 = EDGE_CURVE ( 'NONE', #56656, #42237, #49456, .T. ) ;
#3946 = CARTESIAN_POINT ( 'NONE',  ( 0.2767916011545359933, 11.57477803659173254, 4.010899340181466322 ) ) ;
#3947 = ORIENTED_EDGE ( 'NONE', *, *, #28526, .T. ) ;
#3948 = CARTESIAN_POINT ( 'NONE',  ( 2.268878695253353506, -1.472930498387327480, 7.500319319173580190 ) ) ;
#3949 = CARTESIAN_POINT ( 'NONE',  ( -15.95528719064657075, 7.880328173109766965, 9.049993051904070995 ) ) ;
#3950 = ADVANCED_FACE ( 'NONE', ( #10429 ), #4153, .T. ) ;
#3951 = CARTESIAN_POINT ( 'NONE',  ( 37.00000000000000711, -8.366449238204431538, -9.621072037176967129 ) ) ;
#3952 = DIRECTION ( 'NONE',  ( 0.000000000000000000, -0.01356324068817998940, 0.9999080150203990547 ) ) ;
#3953 = CARTESIAN_POINT ( 'NONE',  ( 2.241352910868908310, -7.503490710578242684, 1.407733736974842165 ) ) ;
#3954 = CARTESIAN_POINT ( 'NONE',  ( 23.55545670043567341, -3.418074724591041669, 13.06318810598877356 ) ) ;
#3955 = CARTESIAN_POINT ( 'NONE',  ( -27.10719052120871098, 2.295785794152562787, 0.5475695427849293084 ) ) ;
#3956 = DIRECTION ( 'NONE',  ( -1.000000000000000000, 0.000000000000000000, 0.000000000000000000 ) ) ;
#3957 = FACE_OUTER_BOUND ( 'NONE', #17320, .T. ) ;
#3958 = ORIENTED_EDGE ( 'NONE', *, *, #5883, .T. ) ;
#3959 = CARTESIAN_POINT ( 'NONE',  ( 35.00000000000000000, 4.705694406421931860E-17, -3.469127814946512892E-15 ) ) ;
#3960 = VERTEX_POINT ( 'NONE', #9780 ) ;
#3961 = CARTESIAN_POINT ( 'NONE',  ( 2.305787727787083519, -7.566723232958080914, 1.164987321564707967 ) ) ;
#3962 = DIRECTION ( 'NONE',  ( 0.000000000000000000, 0.01356324068817998940, -0.9999080150203989437 ) ) ;
#3963 = CARTESIAN_POINT ( 'NONE',  ( 2.241528039335008327, -4.919377664485136137, 5.838210500619361198 ) ) ;
#3964 = DIRECTION ( 'NONE',  ( -1.000000000000000000, 0.000000000000000000, 0.000000000000000000 ) ) ;
#3965 = CARTESIAN_POINT ( 'NONE',  ( 2.000000000000001776, -1.018311147294196806, 6.861346417234461370 ) ) ;
#3966 = EDGE_LOOP ( 'NONE', ( #4762, #13373, #52001, #43164 ) ) ;
#3967 = CARTESIAN_POINT ( 'NONE',  ( -35.00000000000000000, -6.280308599560071592, -9.926225166347094842 ) ) ;
#3968 = LINE ( 'NONE', #32885, #35289 ) ;
#3969 = LINE ( 'NONE', #24233, #43918 ) ;
#3970 = CARTESIAN_POINT ( 'NONE',  ( 16.25676674326364335, -34.36623312464833191, -6.550321452248093479 ) ) ;
#3971 = EDGE_CURVE ( 'NONE', #38388, #60470, #24799, .T. ) ;
#3972 = DIRECTION ( 'NONE',  ( -1.000000000000000000, 0.000000000000000000, 0.000000000000000000 ) ) ;
#3973 = CIRCLE ( 'NONE', #36851, 12.18649999999999878 ) ;
#3974 = VERTEX_POINT ( 'NONE', #19780 ) ;
#3975 = CARTESIAN_POINT ( 'NONE',  ( 0.2655924914740778742, -6.084990060696584102, 10.62761259256415158 ) ) ;
#3976 = ORIENTED_EDGE ( 'NONE', *, *, #63079, .F. ) ;
#3977 = CARTESIAN_POINT ( 'NONE',  ( -35.04643116707788408, -0.001845126042319261694, -0.01204777744935776884 ) ) ;
#3978 = CARTESIAN_POINT ( 'NONE',  ( -17.05023968204110929, -34.50000000000000000, 4.356789313881321846 ) ) ;
#3979 = CIRCLE ( 'NONE', #28369, 12.18650000000000055 ) ;
#3980 = CARTESIAN_POINT ( 'NONE',  ( 37.00000000000000711, -12.63095688309027764, 1.738225594540123708 ) ) ;
#3981 = LINE ( 'NONE', #25226, #21401 ) ;
#3982 = EDGE_CURVE ( 'NONE', #30390, #46189, #44689, .T. ) ;
#3983 = VERTEX_POINT ( 'NONE', #30065 ) ;
#3984 = ORIENTED_EDGE ( 'NONE', *, *, #6838, .F. ) ;
#3985 = CARTESIAN_POINT ( 'NONE',  ( -27.08776759928964850, 2.217308861843129364, -0.6183458186125485589 ) ) ;
#3986 = CYLINDRICAL_SURFACE ( 'NONE', #25527, 7.499999999999988454 ) ;
#3987 = CARTESIAN_POINT ( 'NONE',  ( -35.00000000000000000, 9.677500615117999416, -6.657191900728212985 ) ) ;
#3988 = CARTESIAN_POINT ( 'NONE',  ( 0.3401186441510245517, 12.26845925752607158, 0.2556125181570270688 ) ) ;
#3989 = FACE_OUTER_BOUND ( 'NONE', #14522, .T. ) ;
#3990 = CARTESIAN_POINT ( 'NONE',  ( 2.000000000000001776, 0.000000000000000000, 0.000000000000000000 ) ) ;
#3991 = CARTESIAN_POINT ( 'NONE',  ( -18.11249319439446737, -11.56825399538298882, 3.263832109282014393 ) ) ;
#3992 = EDGE_LOOP ( 'NONE', ( #30418, #17987, #62430, #32757 ) ) ;
#3993 = EDGE_CURVE ( 'NONE', #10675, #44838, #28818, .T. ) ;
#3994 = ORIENTED_EDGE ( 'NONE', *, *, #15090, .F. ) ;
#3995 = ORIENTED_EDGE ( 'NONE', *, *, #61519, .F. ) ;
#3996 = CARTESIAN_POINT ( 'NONE',  ( -16.66082797316812503, -33.00000000000000000, -4.257284274447473926 ) ) ;
#3997 = ADVANCED_FACE ( 'NONE', ( #10117 ), #30396, .T. ) ;
#3998 = CARTESIAN_POINT ( 'NONE',  ( 2.655192694324852720, 9.584054627284606553, -0.5793947661800037396 ) ) ;
#3999 = ORIENTED_EDGE ( 'NONE', *, *, #14250, .T. ) ;
#4000 = CARTESIAN_POINT ( 'NONE',  ( -35.00000000000000000, 0.000000000000000000, 0.000000000000000000 ) ) ;
#4001 = ORIENTED_EDGE ( 'NONE', *, *, #52857, .F. ) ;
#4002 = CARTESIAN_POINT ( 'NONE',  ( -27.35552965826137140, 1.773915698030573473, -2.548625910254528559 ) ) ;
#4003 = DIRECTION ( 'NONE',  ( 0.000000000000000000, -0.01356324068817998940, 0.9999080150203990547 ) ) ;
#4004 = DIRECTION ( 'NONE',  ( -1.000000000000000000, 0.000000000000000000, 0.000000000000000000 ) ) ;
#4005 = ORIENTED_EDGE ( 'NONE', *, *, #64620, .T. ) ;
#4006 = ORIENTED_EDGE ( 'NONE', *, *, #51893, .T. ) ;
#4007 = CARTESIAN_POINT ( 'NONE',  ( 2.268878695253353506, 2.474564429974497326, 7.231932316093173441 ) ) ;
#4008 = B_SPLINE_CURVE_WITH_KNOTS ( 'NONE', 3,
 ( #63960, #8116, #14068, #28709, #59638, #53991, #28387, #3141, #44323, #12749, #34356, #38021, #18438, #23400, #28073, #33035, #43671, #17767, #48371, #38701, #39013, #2821 ),
 .UNSPECIFIED., .F., .F.,
 ( 4, 3, 3, 3, 3, 3, 3, 4 ),
 ( 3.157244383156456744E-18, 4.449119708436542037E-05, 6.626296329539970234E-05, 8.803456484962158895E-05, 0.0001098060367612736842, 0.0001315774408628445666, 0.0001760698110411097305, 0.0001829697163287816945 ),
 .UNSPECIFIED. ) ;
#4009 = ORIENTED_EDGE ( 'NONE', *, *, #28726, .F. ) ;
#4010 = CARTESIAN_POINT ( 'NONE',  ( 36.00000000000000711, -0.4871980014160596784, 12.74068829017554094 ) ) ;
#4011 = EDGE_LOOP ( 'NONE', ( #8472, #41353 ) ) ;
#4012 = ADVANCED_BREP_SHAPE_REPRESENTATION ( '', ( #7246, #24966 ), #5855 ) ;
#4013 = ORIENTED_EDGE ( 'NONE', *, *, #41975, .F. ) ;
#4014 = ORIENTED_EDGE ( 'NONE', *, *, #18863, .F. ) ;
#4015 = DIRECTION ( 'NONE',  ( -1.000000000000000000, -1.836970198721029688E-16, -0.000000000000000000 ) ) ;
#4016 = EDGE_CURVE ( 'NONE', #45368, #8244, #2504, .T. ) ;
#4017 = DIRECTION ( 'NONE',  ( 1.000000000000000000, 0.000000000000000000, -0.000000000000000000 ) ) ;
#4018 = FACE_OUTER_BOUND ( 'NONE', #19946, .T. ) ;
#4019 = DIRECTION ( 'NONE',  ( -1.000000000000000000, -0.000000000000000000, -0.000000000000000000 ) ) ;
#4020 = ORIENTED_EDGE ( 'NONE', *, *, #9691, .F. ) ;
#4021 = DIRECTION ( 'NONE',  ( 0.000000000000000000, -0.01356324068818000848, 0.9999080150203990547 ) ) ;
#4022 = AXIS2_PLACEMENT_3D ( 'NONE', #62808, #16939, #52540 ) ;
#4023 = ORIENTED_EDGE ( 'NONE', *, *, #50393, .F. ) ;
#4024 = DIRECTION ( 'NONE',  ( -1.000000000000000000, 0.000000000000000000, 0.000000000000000000 ) ) ;
#4025 = CARTESIAN_POINT ( 'NONE',  ( -17.83717122027472612, -8.628852110296120870, -10.38608613287006044 ) ) ;
#4026 = ORIENTED_EDGE ( 'NONE', *, *, #24613, .F. ) ;
#4027 = CARTESIAN_POINT ( 'NONE',  ( -16.48583967416821494, 8.235227529897704457, 8.728494452408142479 ) ) ;
#4028 = CYLINDRICAL_SURFACE ( 'NONE', #13826, 12.18650000000000055 ) ;
#4029 = CARTESIAN_POINT ( 'NONE',  ( 2.297017764050090172, -6.708511771223851561, -3.682881532880156072 ) ) ;
#4030 = CIRCLE ( 'NONE', #43262, 4.999999999999999112 ) ;
#4032 = EDGE_CURVE ( 'NONE', #63155, #33997, #44094, .T. ) ;
#4031 = VERTEX_POINT ( 'NONE', #40037 ) ;
#4033 = ORIENTED_EDGE ( 'NONE', *, *, #4631, .F. ) ;
#4034 = VECTOR ( 'NONE', #25844, 1000.000000000000000 ) ;
#4035 = CARTESIAN_POINT ( 'NONE',  ( 0.8320506296491532172, 6.546053790694177366, 10.57268643647776862 ) ) ;
#4036 = ORIENTED_EDGE ( 'NONE', *, *, #33420, .T. ) ;
#4037 = DIRECTION ( 'NONE',  ( 0.000000000000000000, 0.01356324068817998940, -0.9999080150203990547 ) ) ;
#4038 = CARTESIAN_POINT ( 'NONE',  ( -25.54417658651491863, 25.00000000000000000, 11.22596262356930197 ) ) ;
#4039 = CARTESIAN_POINT ( 'NONE',  ( 2.899286259009685285, 6.972741252562111747, -3.614094927251865208 ) ) ;
#4040 = CARTESIAN_POINT ( 'NONE',  ( -37.00000000000000711, 1.039216533673073206, -11.70009620280410445 ) ) ;
#4041 = CARTESIAN_POINT ( 'NONE',  ( 35.00000000000000000, 4.705694406421931860E-17, -3.469127814946512892E-15 ) ) ;
#4042 = ORIENTED_EDGE ( 'NONE', *, *, #32715, .F. ) ;
#4043 = CARTESIAN_POINT ( 'NONE',  ( 2.241451721903216399, 3.869794645251212195, -6.581017239736924651 ) ) ;
#4044 = CARTESIAN_POINT ( 'NONE',  ( 0.5572780756282654790, 1.841882550626922299, 12.20533540249701510 ) ) ;
#4045 = EDGE_CURVE ( 'NONE', #3673, #52526, #29625, .T. ) ;
#4046 = FACE_OUTER_BOUND ( 'NONE', #63130, .T. ) ;
#4047 = CARTESIAN_POINT ( 'NONE',  ( 37.25000000000000711, 5.493969937218003549E-16, -4.500000000000000888 ) ) ;
#4048 = ADVANCED_FACE ( 'NONE', ( #42640 ), #21408, .F. ) ;
#4049 = CARTESIAN_POINT ( 'NONE',  ( 2.297017764050091948, -5.967068736727081379, -4.791851130936033876 ) ) ;
#4050 = CYLINDRICAL_SURFACE ( 'NONE', #21934, 12.18650000000000055 ) ;
#4051 = DIRECTION ( 'NONE',  ( 1.000000000000000000, -0.000000000000000000, 0.000000000000000000 ) ) ;
#4052 = CIRCLE ( 'NONE', #47574, 6.936499999999989008 ) ;
#4053 = EDGE_CURVE ( 'NONE', #6027, #3315, #27985, .T. ) ;
#4054 = ORIENTED_EDGE ( 'NONE', *, *, #44399, .F. ) ;
#4055 = CARTESIAN_POINT ( 'NONE',  ( -30.18541646480307250, -1.416020129149132112, 11.91616074890920096 ) ) ;
#4056 = AXIS2_PLACEMENT_3D ( 'NONE', #11702, #62908, #43602 ) ;
#4057 = VERTEX_POINT ( 'NONE', #5814 ) ;
#4058 = FACE_OUTER_BOUND ( 'NONE', #41489, .T. ) ;
#4059 = CARTESIAN_POINT ( 'NONE',  ( -35.04660725145885891, -0.003326400506010091657, 0.01184012236745035987 ) ) ;
#4060 = CARTESIAN_POINT ( 'NONE',  ( 2.373367633546871414, -7.275198254387427177, 2.455525055524864886 ) ) ;
#4061 = VECTOR ( 'NONE', #54326, 1000.000000000000000 ) ;
#4062 = DIRECTION ( 'NONE',  ( 0.000000000000000000, 0.000000000000000000, -1.000000000000000000 ) ) ;
#4063 = VERTEX_POINT ( 'NONE', #51685 ) ;
#4064 = EDGE_CURVE ( 'NONE', #28784, #29441, #32234, .T. ) ;
#4065 = ORIENTED_EDGE ( 'NONE', *, *, #42941, .F. ) ;
#4066 = ORIENTED_EDGE ( 'NONE', *, *, #43284, .F. ) ;
#4067 = DIRECTION ( 'NONE',  ( -1.000000000000000000, 0.000000000000000000, 0.000000000000000000 ) ) ;
#4068 = CARTESIAN_POINT ( 'NONE',  ( -27.75688124897997966, 10.82714900795144253, -5.182596736677783866 ) ) ;
#4069 = ORIENTED_EDGE ( 'NONE', *, *, #6633, .F. ) ;
#4070 = DIRECTION ( 'NONE',  ( -1.000000000000000000, 0.000000000000000000, 0.000000000000000000 ) ) ;
#4071 = DIRECTION ( 'NONE',  ( 0.000000000000000000, -0.01356324068817991828, 0.9999080150203990547 ) ) ;
#4072 = CARTESIAN_POINT ( 'NONE',  ( 37.00000000000000711, -9.430788938293991563, 7.718225330433904574 ) ) ;
#4073 = DIRECTION ( 'NONE',  ( -1.000000000000000000, -0.000000000000000000, -0.000000000000000000 ) ) ;
#4074 = EDGE_LOOP ( 'NONE', ( #17907, #37943, #45108, #58361 ) ) ;
#4075 =( BOUNDED_CURVE ( )  B_SPLINE_CURVE ( 3, ( #1540, #5880, #26137, #46415 ),
 .UNSPECIFIED., .F., .F. ) 
 B_SPLINE_CURVE_WITH_KNOTS ( ( 4, 4 ),
 ( 4.422350118998207513, 4.437400365793983781 ),
 .UNSPECIFIED. ) 
 CURVE ( )  GEOMETRIC_REPRESENTATION_ITEM ( )  RATIONAL_B_SPLINE_CURVE ( ( 1.000000000000000000, 0.9999811242616895024, 0.9999811242616895024, 1.000000000000000000 ) ) 
 REPRESENTATION_ITEM ( '' )  );
#4076 = DIRECTION ( 'NONE',  ( 0.3939253465568944290, -0.9190910618577644575, -0.009718094113436328077 ) ) ;
#4077 = CARTESIAN_POINT ( 'NONE',  ( -6.227954140666513538, -28.64022186353147248, -12.80077302199831557 ) ) ;
#4078 = CARTESIAN_POINT ( 'NONE',  ( -29.58114640908272364, -2.918339774162580280, -11.64592837444328666 ) ) ;
#4080 = ORIENTED_EDGE ( 'NONE', *, *, #16052, .T. ) ;
#4079 = DIRECTION ( 'NONE',  ( 1.000000000000000000, -0.000000000000000000, 0.000000000000000000 ) ) ;
#4081 = CARTESIAN_POINT ( 'NONE',  ( 22.61491127797214062, 25.00000000000000000, 9.376349503825034404 ) ) ;
#4082 = ORIENTED_EDGE ( 'NONE', *, *, #36041, .F. ) ;
#4083 = CARTESIAN_POINT ( 'NONE',  ( 1.109979610370815939, -9.898186741522138732, 7.679283534372324027 ) ) ;
#4084 = ORIENTED_EDGE ( 'NONE', *, *, #50522, .T. ) ;
#4085 = PLANE ( 'NONE',  #41034 ) ;
#4086 = CARTESIAN_POINT ( 'NONE',  ( 32.00000000000000000, 1.230770033143089974E-14, 0.000000000000000000 ) ) ;
#4087 = DIRECTION ( 'NONE',  ( -1.000000000000000000, 0.000000000000000000, 0.000000000000000000 ) ) ;
#4088 = LINE ( 'NONE', #14685, #22740 ) ;
#4090 = CARTESIAN_POINT ( 'NONE',  ( 0.2648978790185619880, 9.465406350830608773, 7.769924372105235122 ) ) ;
#4089 = VECTOR ( 'NONE', #6896, 1000.000000000000000 ) ;
#4091 = DIRECTION ( 'NONE',  ( -0.3939253465568944290, 0.009718094113433240269, 0.9190910618577644575 ) ) ;
#4092 = CARTESIAN_POINT ( 'NONE',  ( 1.719304012338831678, -5.066286238785654206, 11.67935079956403044 ) ) ;
#4094 = ORIENTED_EDGE ( 'NONE', *, *, #17276, .T. ) ;
#4093 = DIRECTION ( 'NONE',  ( 0.000000000000000000, 0.7196168960969817618, 0.6943713148249613942 ) ) ;
#4095 = ORIENTED_EDGE ( 'NONE', *, *, #44938, .T. ) ;
#4096 = AXIS2_PLACEMENT_3D ( 'NONE', #42756, #52444, #12492 ) ;
#4097 = CARTESIAN_POINT ( 'NONE',  ( 0.3665391374699467075, -12.13918562134719892, 1.872534962004761327 ) ) ;
#4098 = EDGE_LOOP ( 'NONE', ( #8112, #51549, #52752, #49493 ) ) ;
#4099 = ORIENTED_EDGE ( 'NONE', *, *, #12002, .T. ) ;
#4100 = CARTESIAN_POINT ( 'NONE',  ( 0.7400311444011717921, 1.803686700615571459, -12.27261279799596316 ) ) ;
#4101 = FACE_OUTER_BOUND ( 'NONE', #23994, .T. ) ;
#4102 = B_SPLINE_CURVE_WITH_KNOTS ( 'NONE', 3,
 ( #19561, #45147, #65405, #15203, #14852, #65723, #20534, #14529, #20195, #25507, #50479, #40817, #9887, #25183, #39824, #5586, #4922, #40468, #19873 ),
 .UNSPECIFIED., .F., .F.,
 ( 4, 3, 3, 3, 3, 3, 4 ),
 ( 6.269651592512720910E-18, 2.825908398831185141E-05, 4.208813692483835759E-05, 5.591713746943659783E-05, 6.279584083231569099E-05, 9.105792820296166852E-05, 0.0001153131102488848627 ),
 .UNSPECIFIED. ) ;
#4103 = CARTESIAN_POINT ( 'NONE',  ( -27.35552965826136429, -1.320216934008378473, -2.810569013793753346 ) ) ;
#4104 = CYLINDRICAL_SURFACE ( 'NONE', #29932, 4.999999999999999112 ) ;
#4105 = CARTESIAN_POINT ( 'NONE',  ( -22.31213670151048944, 1.669817926839938460, -3.398324501467284708 ) ) ;
#4106 = ADVANCED_FACE ( 'NONE', ( #16428 ), #56993, .T. ) ;
#4107 = DIRECTION ( 'NONE',  ( -1.000000000000000000, 0.000000000000000000, 0.000000000000000000 ) ) ;
#4108 = CARTESIAN_POINT ( 'NONE',  ( 35.00000000000000000, -11.05394794832825767, 5.130401251914841865 ) ) ;
#4109 = VECTOR ( 'NONE', #22187, 1000.000000000000000 ) ;
#4110 = CIRCLE ( 'NONE', #12579, 12.75000000000000178 ) ;
#4111 = ORIENTED_EDGE ( 'NONE', *, *, #53102, .T. ) ;
#4112 = DIRECTION ( 'NONE',  ( 0.000000000000000000, 0.2960891610144510966, 0.9551603052523478521 ) ) ;
#4113 = CARTESIAN_POINT ( 'NONE',  ( 2.889800649504073782, 5.774917447012996696, 2.030191121417155742 ) ) ;
#4114 = AXIS2_PLACEMENT_3D ( 'NONE', #54241, #53911, #23986 ) ;
#4115 = CARTESIAN_POINT ( 'NONE',  ( 0.2650492433740058718, -7.955688793816027449, -9.309907554970058285 ) ) ;
#4116 = ORIENTED_EDGE ( 'NONE', *, *, #55631, .F. ) ;
#4117 = VECTOR ( 'NONE', #3564, 1000.000000000000000 ) ;
#4118 = ADVANCED_FACE ( 'NONE', ( #31688 ), #27363, .T. ) ;
#4119 = B_SPLINE_CURVE_WITH_KNOTS ( 'NONE', 3,
 ( #43937, #13986, #18687, #40233, #45554, #25954, #25275, #15306, #9642, #54889, #60522, #35582, #45901, #55876, #10308, #19965, #45239, #40570, #34593 ),
 .UNSPECIFIED., .F., .F.,
 ( 4, 3, 3, 3, 3, 3, 4 ),
 ( 8.282800797427508197E-18, 4.457896483015377895E-05, 6.639290541542518080E-05, 8.820687556479407708E-05, 0.0001100173248779025482, 0.0001545671401658153549, 0.0001830328308068586039 ),
 .UNSPECIFIED. ) ;
#4120 = CARTESIAN_POINT ( 'NONE',  ( -5.873305616363168724, -0.9854497472355991938, 13.46436504529688349 ) ) ;
#4121 = EDGE_CURVE ( 'NONE', #48838, #42404, #43930, .T. ) ;
#4122 = CARTESIAN_POINT ( 'NONE',  ( 35.00000000000000000, 11.66664283989686979, 5.143145423404150485 ) ) ;
#4123 = EDGE_CURVE ( 'NONE', #15834, #36605, #59828, .T. ) ;
#4124 = ORIENTED_EDGE ( 'NONE', *, *, #43841, .T. ) ;
#4125 = LINE ( 'NONE', #49680, #61662 ) ;
#4126 = DIRECTION ( 'NONE',  ( 0.000000000000000000, -0.9999080150203988326, -0.01356324068819046366 ) ) ;
#4127 = CARTESIAN_POINT ( 'NONE',  ( 3.153349365415208716, 2.981698431668006410, 11.62552590921464990 ) ) ;
#4128 = B_SPLINE_CURVE_WITH_KNOTS ( 'NONE', 3,
 ( #3823, #53694, #19086, #44658, #13113, #23417, #39353, #54680, #29382, #24389, #64945, #39692, #59987, #14405, #34681, #54978, #60295, #56641, #46329, #25712, #65286, #26047, #5780, #110, #40670, #20066, #30677, #50986, #35671, #20392, #45011, #25062, #31022, #769, #56285, #14719, #45657, #55306, #5109, #10089, #65591, #60967, #34998, #31352, #45331, #50349, #9749, #15400, #40328, #30036, #50665, #21031, #51655, #4797 ),
 .UNSPECIFIED., .F., .F.,
 ( 4, 2, 2, 2, 2, 2, 2, 2, 2, 2, 2, 2, 2, 2, 2, 2, 2, 2, 2, 2, 2, 2, 2, 2, 2, 2, 4 ),
 ( 0.000000000000000000, 0.004909564951003675057, 0.007364347426505513453, 0.009819129902007351848, 0.01472869485301103037, 0.01718347732851286530, 0.01963825980401470023, 0.02454782475501837702, 0.02700260723052020501, 0.02945738970602204340, 0.03191217218152387486, 0.03313956341927479232, 0.03436695465702570979, 0.03927651960802938658, 0.04173130208353122844, 0.04295869332128214590, 0.04418608455903306337, 0.04909564951003673322, 0.05155043198553856121, 0.05400521446104038920, 0.05891477941204405905, 0.06382434436304772196, 0.06627912683854955689, 0.06873390931405140569, 0.07364347426505506167, 0.07609825674055691047, 0.07855303921605873152 ),
 .UNSPECIFIED. ) ;
#4129 = AXIS2_PLACEMENT_3D ( 'NONE', #65505, #50582, #50898 ) ;
#4130 = EDGE_CURVE ( 'NONE', #13640, #12912, #27284, .T. ) ;
#4131 = LINE ( 'NONE', #35679, #5523 ) ;
#4132 = LINE ( 'NONE', #50014, #61681 ) ;
#4133 = EDGE_LOOP ( 'NONE', ( #52201, #31547, #59214, #35250 ) ) ;
#4134 = CIRCLE ( 'NONE', #63588, 12.18650000000000055 ) ;
#4135 = DIRECTION ( 'NONE',  ( 1.000000000000000000, 0.000000000000000000, 0.000000000000000000 ) ) ;
#4136 = EDGE_CURVE ( 'NONE', #39957, #29408, #4640, .T. ) ;
#4137 = CARTESIAN_POINT ( 'NONE',  ( 0.2657645697724686507, -12.08564806881063092, 1.977350809428493505 ) ) ;
#4138 = CARTESIAN_POINT ( 'NONE',  ( 35.00000000000000000, -3.511814412392203266, -11.66953048682398730 ) ) ;
#4139 = ORIENTED_EDGE ( 'NONE', *, *, #28623, .T. ) ;
#4140 = CARTESIAN_POINT ( 'NONE',  ( 8.437200413559441614, 4.476360154859203355, 12.73625532737111143 ) ) ;
#4141 = DIRECTION ( 'NONE',  ( 0.000000000000000000, -0.01356324068817998940, 0.9999080150203990547 ) ) ;
#4142 = EDGE_LOOP ( 'NONE', ( #48265, #50609, #32135, #63906 ) ) ;
#4143 = VERTEX_POINT ( 'NONE', #31051 ) ;
#4144 = ORIENTED_EDGE ( 'NONE', *, *, #11926, .T. ) ;
#4145 = DIRECTION ( 'NONE',  ( 0.000000000000000000, 0.01356324068817998940, -0.9999080150203989437 ) ) ;
#4146 = AXIS2_PLACEMENT_3D ( 'NONE', #37457, #56432, #16197 ) ;
#4147 = ORIENTED_EDGE ( 'NONE', *, *, #33585, .T. ) ;
#4148 = ADVANCED_FACE ( 'NONE', ( #22054 ), #56316, .T. ) ;
#4149 = CARTESIAN_POINT ( 'NONE',  ( -36.00000000000000711, 10.93004082984018588, 6.564808257521810297 ) ) ;
#4150 = CYLINDRICAL_SURFACE ( 'NONE', #2855, 10.20557198542813815 ) ;
#4151 = AXIS2_PLACEMENT_3D ( 'NONE', #4799, #25064, #25714 ) ;
#4152 = FACE_OUTER_BOUND ( 'NONE', #54205, .T. ) ;
#4153 = CYLINDRICAL_SURFACE ( 'NONE', #35411, 12.18650000000000055 ) ;
#4155 = EDGE_CURVE ( 'NONE', #48840, #42334, #62600, .T. ) ;
#4154 = CARTESIAN_POINT ( 'NONE',  ( -15.30016555129190792, -28.05832310202213620, 10.91616026484521385 ) ) ;
#4156 = CARTESIAN_POINT ( 'NONE',  ( 2.241506898688418126, 0.03933068055390912671, 7.634383346098562839 ) ) ;
#4158 = ORIENTED_EDGE ( 'NONE', *, *, #47404, .T. ) ;
#4157 = CARTESIAN_POINT ( 'NONE',  ( 1.109979610369143277, 7.679283534372506992, 9.898186741521291410 ) ) ;
#4159 = CARTESIAN_POINT ( 'NONE',  ( -47.00000000000000711, 0.000000000000000000, 0.000000000000000000 ) ) ;
#4160 = ORIENTED_EDGE ( 'NONE', *, *, #44087, .F. ) ;
#4161 = FACE_OUTER_BOUND ( 'NONE', #60835, .T. ) ;
#4162 = ORIENTED_EDGE ( 'NONE', *, *, #23764, .T. ) ;
#4163 = AXIS2_PLACEMENT_3D ( 'NONE', #61032, #19814, #4858 ) ;
#4164 = ORIENTED_EDGE ( 'NONE', *, *, #21724, .F. ) ;
#4165 = CARTESIAN_POINT ( 'NONE',  ( -27.35552965826137140, 2.548625910254547655, 1.773915698030531951 ) ) ;
#4166 = CARTESIAN_POINT ( 'NONE',  ( -5.813762929211682362, -31.14503107145061378, 14.54886001617130553 ) ) ;
#4167 = CARTESIAN_POINT ( 'NONE',  ( -35.00000000000000000, 2.905556151562625811, 11.38112321385051651 ) ) ;
#4168 = CARTESIAN_POINT ( 'NONE',  ( 5.514970785353741078, 0.003415090918276138688, -0.003262412238248723392 ) ) ;
#4169 = B_SPLINE_CURVE_WITH_KNOTS ( 'NONE', 3,
 ( #8974, #3991, #20248, #64801, #25240, #24590, #44524, #65462 ),
 .UNSPECIFIED., .F., .F.,
 ( 4, 2, 2, 4 ),
 ( 8.673617379884035472E-19, 0.002049566690290811118, 0.003074350035436216894, 0.004099133380581623104 ),
 .UNSPECIFIED. ) ;
#4170 = CARTESIAN_POINT ( 'NONE',  ( -37.00000000000000711, -12.18359334611896472, -0.2661492558804631203 ) ) ;
#4171 = CARTESIAN_POINT ( 'NONE',  ( 2.259025283526323147, 5.939720477911452967, 4.805599953369094735 ) ) ;
#4172 = ORIENTED_EDGE ( 'NONE', *, *, #11777, .T. ) ;
#4173 = ORIENTED_EDGE ( 'NONE', *, *, #15625, .T. ) ;
#4174 = DIRECTION ( 'NONE',  ( -1.000000000000000000, -0.000000000000000000, -0.000000000000000000 ) ) ;
#4175 = ORIENTED_EDGE ( 'NONE', *, *, #21479, .T. ) ;
#4176 = CARTESIAN_POINT ( 'NONE',  ( 2.244591118396558116, -7.500068934084582750, 1.431619869711830084 ) ) ;
#4177 = CARTESIAN_POINT ( 'NONE',  ( 0.3160775863651117401, 0.2401734240704574974, -12.26075464248083158 ) ) ;
#4178 = DIRECTION ( 'NONE',  ( -1.000000000000000000, 0.000000000000000000, 0.000000000000000000 ) ) ;
#4179 = CARTESIAN_POINT ( 'NONE',  ( -22.27720412283625961, 1.161733799004190049, -3.493592264983214513 ) ) ;
#4180 = EDGE_CURVE ( 'NONE', #45226, #58319, #38610, .T. ) ;
#4181 = PLANE ( 'NONE',  #27785 ) ;
#4182 = AXIS2_PLACEMENT_3D ( 'NONE', #9656, #4373, #4719 ) ;
#4183 = CARTESIAN_POINT ( 'NONE',  ( -36.00000000000000711, 8.366449238204365813, 9.621072037177027525 ) ) ;
#4184 = ORIENTED_EDGE ( 'NONE', *, *, #30714, .T. ) ;
#4185 = AXIS2_PLACEMENT_3D ( 'NONE', #62549, #41954, #37635 ) ;
#4186 = VERTEX_POINT ( 'NONE', #38323 ) ;
#4187 = CARTESIAN_POINT ( 'NONE',  ( -27.28563798457900091, 1.413023339712129678, 2.528380693767707577 ) ) ;
#4188 = SURFACE_SIDE_STYLE ('',( #49743 ) ) ;
#4189 = ADVANCED_FACE ( 'NONE', ( #17407 ), #33002, .T. ) ;
#4190 = DIRECTION ( 'NONE',  ( 0.000000000000000000, 0.3554799084908899509, 0.9346839223284567622 ) ) ;
#4191 = VECTOR ( 'NONE', #36169, 1000.000000000000000 ) ;
#4192 = DIRECTION ( 'NONE',  ( -1.000000000000000000, 0.000000000000000000, 0.000000000000000000 ) ) ;
#4193 = EDGE_CURVE ( 'NONE', #59561, #50772, #14145, .T. ) ;
#4194 = DIRECTION ( 'NONE',  ( 1.000000000000000000, -0.000000000000000000, 0.000000000000000000 ) ) ;
#4195 = CIRCLE ( 'NONE', #45578, 12.74999999999999822 ) ;
#4196 = CARTESIAN_POINT ( 'NONE',  ( 6.992580758904643368, -4.514504415418986838, -12.72890816843052697 ) ) ;
#4197 = CARTESIAN_POINT ( 'NONE',  ( 37.00000000000000711, 11.78745411414844035, 3.093009498343795460 ) ) ;
#4198 = CARTESIAN_POINT ( 'NONE',  ( 2.241352910868908310, -5.794346703933879184, 4.970878533273742406 ) ) ;
#4199 = DIRECTION ( 'NONE',  ( 1.000000000000000000, -0.000000000000000000, 0.000000000000000000 ) ) ;
#4200 = ADVANCED_FACE ( 'NONE', ( #23051 ), #33988, .T. ) ;
#4201 = ORIENTED_EDGE ( 'NONE', *, *, #37915, .F. ) ;
#4202 = CARTESIAN_POINT ( 'NONE',  ( 2.556980015512952065, -6.074557383032423985, -4.795979673457674508 ) ) ;
#4203 = CARTESIAN_POINT ( 'NONE',  ( 0.3675815128205894289, 10.76447900494940235, 5.910255304480483751 ) ) ;
#4204 = CARTESIAN_POINT ( 'NONE',  ( 21.90174657591892071, 13.47998113580524659, -0.7349207973210680755 ) ) ;
#4205 = VECTOR ( 'NONE', #59552, 1000.000000000000227 ) ;
#4206 = CARTESIAN_POINT ( 'NONE',  ( 2.573738926104376379, -6.586859681822632595, -4.074516960797446963 ) ) ;
#4207 = CARTESIAN_POINT ( 'NONE',  ( -27.75187954703365634, -11.73910552422975861, -2.553580313601046203 ) ) ;
#4208 = EDGE_LOOP ( 'NONE', ( #64650, #65545, #55244, #61218 ) ) ;
#4209 = CARTESIAN_POINT ( 'NONE',  ( 35.00000000000000000, -11.66664283989683426, -5.143145423404237526 ) ) ;
#4210 = CARTESIAN_POINT ( 'NONE',  ( 5.520433897694421610, 0.002108682515300482584, -0.01491416502703863875 ) ) ;
#4211 = EDGE_CURVE ( 'NONE', #24405, #2547, #22673, .T. ) ;
#4212 = CARTESIAN_POINT ( 'NONE',  ( 2.128776824815522772, -25.76454106360162299, -15.60647423695309222 ) ) ;
#4213 = ORIENTED_EDGE ( 'NONE', *, *, #6171, .F. ) ;
#4214 = CARTESIAN_POINT ( 'NONE',  ( -37.00000000000000711, 1.488153103997124971, -11.65150730582933036 ) ) ;
#4215 = CARTESIAN_POINT ( 'NONE',  ( -35.00000000000000000, 7.608228585767725427, 10.23119532541075216 ) ) ;
#4216 = CYLINDRICAL_SURFACE ( 'NONE', #36498, 2.899999999999994582 ) ;
#4217 = EDGE_CURVE ( 'NONE', #60024, #18352, #60917, .T. ) ;
#4218 = B_SPLINE_CURVE_WITH_KNOTS ( 'NONE', 3,
 ( #56938, #40297, #20031, #36294, #10058, #70, #6069, #1065, #55936, #5402 ),
 .UNSPECIFIED., .F., .F.,
 ( 4, 3, 3, 4 ),
 ( 3.556024639816093331E-05, 0.0005177888728809999395, 0.002588944364542827056, 0.005045323458346599385 ),
 .UNSPECIFIED. ) ;
#4219 = CARTESIAN_POINT ( 'NONE',  ( 35.00000000000000000, -9.060822531525994705, 7.474872387601095625 ) ) ;
#4220 = DIRECTION ( 'NONE',  ( 1.000000000000000000, 0.000000000000000000, 0.000000000000000000 ) ) ;
#4221 = ADVANCED_FACE ( 'NONE', ( #52970 ), #53315, .T. ) ;
#4222 = CIRCLE ( 'NONE', #5273, 4.999999999999999112 ) ;
#4223 = AXIS2_PLACEMENT_3D ( 'NONE', #55461, #25519, #46155 ) ;
#4224 = CARTESIAN_POINT ( 'NONE',  ( 1.633930747255852411, 12.36466318969160127, -2.909970528253460031 ) ) ;
#4225 = ADVANCED_FACE ( 'NONE', ( #7403 ), #27691, .T. ) ;
#4226 = VERTEX_POINT ( 'NONE', #2792 ) ;
#4227 = CARTESIAN_POINT ( 'NONE',  ( 2.259830038564997867, -7.225713255971560223, 2.483392345594741979 ) ) ;
#4228 = CARTESIAN_POINT ( 'NONE',  ( -2.532614230583026593, -5.020478806276874373, 10.89930238848911337 ) ) ;
#4229 = CARTESIAN_POINT ( 'NONE',  ( -47.00000000000000711, 0.000000000000000000, 0.000000000000000000 ) ) ;
#4230 = CARTESIAN_POINT ( 'NONE',  ( 2.491965175174677416, -4.796682362486693663, 6.046355957631128319 ) ) ;
#4231 = CARTESIAN_POINT ( 'NONE',  ( 41.00000000000000711, -1.694065894508793271E-18, 4.500000000000001776 ) ) ;
#4233 = CYLINDRICAL_SURFACE ( 'NONE', #46052, 2.899999999999994582 ) ;
#4232 = VECTOR ( 'NONE', #49031, 1000.000000000000000 ) ;
#4234 = ADVANCED_FACE ( 'NONE', ( #18060 ), #22728, .T. ) ;
#4235 = DIRECTION ( 'NONE',  ( 0.000000000000000000, -0.01356324068817998940, 0.9999080150203990547 ) ) ;
#4236 = CARTESIAN_POINT ( 'NONE',  ( -27.01437459610461644, -8.723448335974111956, -8.240233560378637634 ) ) ;
#4237 = ORIENTED_EDGE ( 'NONE', *, *, #56944, .F. ) ;
#4238 = ORIENTED_EDGE ( 'NONE', *, *, #21607, .T. ) ;
#4239 = CARTESIAN_POINT ( 'NONE',  ( -17.83857753042823902, -8.695343837413979315, -8.292117721727052526 ) ) ;
#4240 = EDGE_LOOP ( 'NONE', ( #2745, #13939, #33885, #15924 ) ) ;
#4241 = CIRCLE ( 'NONE', #19092, 4.999999999999999112 ) ;
#4242 = CARTESIAN_POINT ( 'NONE',  ( -35.00000000000000000, -12.00000000000000000, 0.000000000000000000 ) ) ;
#4243 = DIRECTION ( 'NONE',  ( 1.000000000000000000, -0.000000000000000000, 0.000000000000000000 ) ) ;
#4245 = VERTEX_POINT ( 'NONE', #17738 ) ;
#4244 = AXIS2_PLACEMENT_3D ( 'NONE', #34852, #55161, #9590 ) ;
#4246 = CARTESIAN_POINT ( 'NONE',  ( 0.2671309869109493862, 5.982543484153372226, -10.68612389951470831 ) ) ;
#4247 = CARTESIAN_POINT ( 'NONE',  ( -10.00000000000000178, 0.000000000000000000, 0.000000000000000000 ) ) ;
#4248 = CARTESIAN_POINT ( 'NONE',  ( 37.00000000000000711, 7.882940143791775434, -10.02106554660711701 ) ) ;
#4249 = ORIENTED_EDGE ( 'NONE', *, *, #15145, .F. ) ;
#4251 = ORIENTED_EDGE ( 'NONE', *, *, #12653, .T. ) ;
#4250 = B_SPLINE_CURVE_WITH_KNOTS ( 'NONE', 3,
 ( #64876, #35277, #60551, #55587, #45269, #40262, #29004, #10026, #14989, #65527, #19994, #30306, #24997, #54621, #19022, #54915, #49312, #19355, #24016 ),
 .UNSPECIFIED., .F., .F.,
 ( 4, 3, 3, 3, 3, 3, 4 ),
 ( 0.000000000000000000, 2.836829842861096206E-05, 4.224792512343923038E-05, 5.612066614708679683E-05, 6.998859278152698427E-05, 9.832141287889580906E-05, 0.0001178161482480330561 ),
 .UNSPECIFIED. ) ;
#4252 = CARTESIAN_POINT ( 'NONE',  ( 2.994568964204211703, 0.3996732855055812328, -7.875338388187465455 ) ) ;
#4253 = CARTESIAN_POINT ( 'NONE',  ( -37.00000000000000711, -1.171570255487366152, -11.68758509253249400 ) ) ;
#4254 = ORIENTED_EDGE ( 'NONE', *, *, #45022, .F. ) ;
#4255 = VECTOR ( 'NONE', #53500, 1000.000000000000000 ) ;
#4256 = CARTESIAN_POINT ( 'NONE',  ( -37.00000000000000711, -11.72195762423409349, -0.7536123767499773862 ) ) ;
#4257 = ORIENTED_EDGE ( 'NONE', *, *, #33036, .T. ) ;
#4258 = CYLINDRICAL_SURFACE ( 'NONE', #60696, 12.18650000000000055 ) ;
#4259 = CARTESIAN_POINT ( 'NONE',  ( -35.00000000000000000, 11.59095880812008161, -1.903127969211228621 ) ) ;
#4260 = EDGE_CURVE ( 'NONE', #10291, #40353, #59006, .T. ) ;
#4261 = FACE_OUTER_BOUND ( 'NONE', #54065, .T. ) ;
#4262 = CYLINDRICAL_SURFACE ( 'NONE', #40150, 2.899999999999994582 ) ;
#4263 = CYLINDRICAL_SURFACE ( 'NONE', #13170, 8.549672981451799103 ) ;
#4264 = ORIENTED_EDGE ( 'NONE', *, *, #37117, .F. ) ;
#4265 = DIRECTION ( 'NONE',  ( 0.000000000000000000, -0.01356324068817992175, 0.9999080150203990547 ) ) ;
#4266 = CARTESIAN_POINT ( 'NONE',  ( 35.00000000000000000, 4.705694406421931860E-17, -3.469127814946512892E-15 ) ) ;
#4267 = CARTESIAN_POINT ( 'NONE',  ( 37.00000000000000711, 4.705694406421931860E-17, -3.469127814946512892E-15 ) ) ;
#4268 = LINE ( 'NONE', #58852, #30621 ) ;
#4269 = DIRECTION ( 'NONE',  ( 1.000000000000000000, 0.000000000000000000, 0.000000000000000000 ) ) ;
#4270 = CARTESIAN_POINT ( 'NONE',  ( -27.09833916700336331, 1.609723001518233998, -1.689564470273829055 ) ) ;
#4271 = CARTESIAN_POINT ( 'NONE',  ( 2.000000000000001776, 2.480520636974191895, 6.345145617221231049 ) ) ;
#4272 = DIRECTION ( 'NONE',  ( 1.000000000000000000, 0.000000000000000000, 0.000000000000000000 ) ) ;
#4273 = ADVANCED_FACE ( 'NONE', ( #28679 ), #9700, .F. ) ;
#4274 = CARTESIAN_POINT ( 'NONE',  ( 2.000000000000001776, -5.585096664091960150, 4.113602740025890547 ) ) ;
#4275 = CIRCLE ( 'NONE', #13787, 5.000000000000000000 ) ;
#4276 = EDGE_LOOP ( 'NONE', ( #47308, #10753, #9120, #57788 ) ) ;
#4277 = CARTESIAN_POINT ( 'NONE',  ( 0.3654063281920718054, 0.2633658439603340229, 12.27672420655578911 ) ) ;
#4278 =( BOUNDED_SURFACE ( )  B_SPLINE_SURFACE ( 3, 1, ( 
 ( #40634, #20994 ),
 ( #60928, #45965 ),
 ( #30340, #51621 ),
 ( #11040, #21333 ) ),
 .UNSPECIFIED., .F., .F., .F. ) 
 B_SPLINE_SURFACE_WITH_KNOTS ( ( 4, 4 ),
 ( 2, 2 ),
 ( 0.000000000000000000, 1.000000000000000000 ),
 ( 0.000000000000000000, 1.000000000000000000 ),
 .UNSPECIFIED. ) 
 GEOMETRIC_REPRESENTATION_ITEM ( )  RATIONAL_B_SPLINE_SURFACE ( (
 ( 1.000000000000000000, 1.000000000000000000),
 ( 0.9856612449720755231, 0.9999558406602322425),
 ( 0.9856612449720755231, 0.9999558406602322425),
 ( 1.000000000000000000, 1.000000000000000000) ) ) 
 REPRESENTATION_ITEM ( '' )  SURFACE ( )  );
#4279 = VERTEX_POINT ( 'NONE', #18731 ) ;
#4280 = CARTESIAN_POINT ( 'NONE',  ( 5.514970785353741078, 0.004324946436530184915, 0.001897634820904495461 ) ) ;
#4281 = CARTESIAN_POINT ( 'NONE',  ( 2.258463476536642478, -7.499249607179731214, -1.460294809171017727 ) ) ;
#4282 = CARTESIAN_POINT ( 'NONE',  ( 5.516018279890452902, -0.005331956019561682678, 0.004180585980735035401 ) ) ;
#4283 = DIRECTION ( 'NONE',  ( 0.000000000000000000, -0.01356324068817998940, 0.9999080150203990547 ) ) ;
#4284 = CARTESIAN_POINT ( 'NONE',  ( 2.524535260912991852, 5.135322114976021979, 5.776056274541075730 ) ) ;
#4285 = EDGE_CURVE ( 'NONE', #37470, #62166, #54522, .T. ) ;
#4286 = EDGE_LOOP ( 'NONE', ( #15085, #60183, #25685, #45669 ) ) ;
#4287 = CARTESIAN_POINT ( 'NONE',  ( 2.000000000000001776, 0.000000000000000000, 0.000000000000000000 ) ) ;
#4288 = CARTESIAN_POINT ( 'NONE',  ( 2.000000000000001776, -2.664846396702436948, -6.404188155573047325 ) ) ;
#4289 = CARTESIAN_POINT ( 'NONE',  ( 35.00000000000000000, 2.497432891016841960, -11.47758908105695319 ) ) ;
#4290 = DIRECTION ( 'NONE',  ( 0.000000000000000000, -0.9937233664769772323, 0.1118654143051511785 ) ) ;
#4291 = ADVANCED_FACE ( 'NONE', ( #54931 ), #39642, .T. ) ;
#4292 = CIRCLE ( 'NONE', #43526, 12.18649999999999878 ) ;
#4293 = VECTOR ( 'NONE', #65377, 1000.000000000000000 ) ;
#4294 = DIRECTION ( 'NONE',  ( -1.000000000000000000, 0.000000000000000000, 0.000000000000000000 ) ) ;
#4295 = ORIENTED_EDGE ( 'NONE', *, *, #11269, .F. ) ;
#4296 = DIRECTION ( 'NONE',  ( 1.000000000000000000, 0.000000000000000000, 0.000000000000000000 ) ) ;
#4297 = ORIENTED_EDGE ( 'NONE', *, *, #64865, .F. ) ;
#4298 = CARTESIAN_POINT ( 'NONE',  ( 0.2872850955227758685, -0.2089153415334024932, -12.25172867346922878 ) ) ;
#4299 = LINE ( 'NONE', #24574, #44807 ) ;
#4300 = AXIS2_PLACEMENT_3D ( 'NONE', #26328, #42578, #6720 ) ;
#4301 = CARTESIAN_POINT ( 'NONE',  ( -2.676156797222401185, -7.839276155712920691, 10.99183054655307856 ) ) ;
#4302 = CARTESIAN_POINT ( 'NONE',  ( 2.000000000000001776, 6.470132594555819239, 2.133363481234098469 ) ) ;
#4303 = ADVANCED_FACE ( 'NONE', ( #10351 ), #55920, .T. ) ;
#4304 = VERTEX_POINT ( 'NONE', #14669 ) ;
#4305 = EDGE_LOOP ( 'NONE', ( #4172, #9214, #35617, #52439 ) ) ;
#4306 = CARTESIAN_POINT ( 'NONE',  ( -27.09342121492585420, 2.227768580955217903, -0.6436068655225335444 ) ) ;
#4307 = EDGE_CURVE ( 'NONE', #1585, #3924, #54578, .T. ) ;
#4308 = ORIENTED_EDGE ( 'NONE', *, *, #8547, .F. ) ;
#4309 = AXIS2_PLACEMENT_3D ( 'NONE', #21509, #26816, #38687 ) ;
#4310 = CARTESIAN_POINT ( 'NONE',  ( 0.3040950598368144520, 4.428852722102886830, -11.43390362554248618 ) ) ;
#4311 = DIRECTION ( 'NONE',  ( 0.000000000000000000, 0.1118654143051615590, 0.9937233664769760111 ) ) ;
#4312 = CARTESIAN_POINT ( 'NONE',  ( 2.000000000000001776, 5.662015959325201742, 4.918493191653995567 ) ) ;
#4313 = DIRECTION ( 'NONE',  ( 1.000000000000000000, 0.000000000000000000, -0.000000000000000000 ) ) ;
#4314 = CARTESIAN_POINT ( 'NONE',  ( 0.2648978790185610999, 9.295532325666560070, -7.972372351882934360 ) ) ;
#4315 = EDGE_CURVE ( 'NONE', #47209, #43940, #31185, .T. ) ;
#4316 = FACE_OUTER_BOUND ( 'NONE', #58075, .T. ) ;
#4317 = CARTESIAN_POINT ( 'NONE',  ( -37.00000000000000711, 2.865935305911801123, -12.42372387097879383 ) ) ;
#4318 = VERTEX_POINT ( 'NONE', #64565 ) ;
#4319 = VECTOR ( 'NONE', #3182, 1000.000000000000114 ) ;
#4320 = ORIENTED_EDGE ( 'NONE', *, *, #41373, .F. ) ;
#4321 = EDGE_LOOP ( 'NONE', ( #19942, #277, #21052, #65669 ) ) ;
#4322 = CARTESIAN_POINT ( 'NONE',  ( 1.547277799339514370, -2.861188171559366111, -12.34637640861339314 ) ) ;
#4324 = CARTESIAN_POINT ( 'NONE',  ( 0.2655924914740778187, -2.169924872618142153, 12.05257978623653159 ) ) ;
#4323 = AXIS2_PLACEMENT_3D ( 'NONE', #2256, #63723, #2917 ) ;
#4325 = CIRCLE ( 'NONE', #64809, 5.000000000000000888 ) ;
#4326 = AXIS2_PLACEMENT_3D ( 'NONE', #14273, #58888, #43542 ) ;
#4328 = EDGE_CURVE ( 'NONE', #14909, #59342, #39964, .T. ) ;
#4327 = VERTEX_POINT ( 'NONE', #59943 ) ;
#4329 = FACE_BOUND ( 'NONE', #40938, .T. ) ;
#4330 = VERTEX_POINT ( 'NONE', #20013 ) ;
#4331 = DIRECTION ( 'NONE',  ( 0.000000000000000000, 0.1740410799127614649, 0.9847383929261618318 ) ) ;
#4332 = B_SPLINE_CURVE_WITH_KNOTS ( 'NONE', 3,
 ( #36693, #16078, #27052, #46352, #61971, #17059, #31049, #56313, #11732, #31381, #46668, #31686, #6125, #26721, #1471, #47346, #10762, #56991, #20752, #41339, #11417, #62598 ),
 .UNSPECIFIED., .F., .F.,
 ( 4, 3, 3, 3, 3, 3, 3, 4 ),
 ( 0.000000000000000000, 4.455945684386706894E-05, 6.636307477203974396E-05, 8.816671873158892945E-05, 0.0001099660380492610182, 0.0001317545563165296125, 0.0001762613022895047734, 0.0001867992666138396194 ),
 .UNSPECIFIED. ) ;
#4333 = CARTESIAN_POINT ( 'NONE',  ( 0.2655924914740778187, 2.169924872618221201, -12.05257978623651560 ) ) ;
#4334 = CARTESIAN_POINT ( 'NONE',  ( -27.08588607604433562, -2.220764381377023700, -0.5840042213197168541 ) ) ;
#4335 = VERTEX_POINT ( 'NONE', #35294 ) ;
#4336 = EDGE_LOOP ( 'NONE', ( #48501, #2751, #32442, #57647, #9148, #13174 ) ) ;
#4337 = CARTESIAN_POINT ( 'NONE',  ( 2.835339799623981083, -6.941489812670547543, 3.628068688271650188 ) ) ;
#4338 = ORIENTED_EDGE ( 'NONE', *, *, #40602, .F. ) ;
#4339 = DIRECTION ( 'NONE',  ( 0.000000000000000000, 0.000000000000000000, 1.000000000000000000 ) ) ;
#4340 = ORIENTED_EDGE ( 'NONE', *, *, #19130, .F. ) ;
#4341 = ORIENTED_EDGE ( 'NONE', *, *, #26273, .T. ) ;
#4342 = ORIENTED_EDGE ( 'NONE', *, *, #40179, .T. ) ;
#4343 = VECTOR ( 'NONE', #29342, 1000.000000000000114 ) ;
#4344 = DIRECTION ( 'NONE',  ( 1.000000000000000000, -0.000000000000000000, -0.000000000000000000 ) ) ;
#4345 = CARTESIAN_POINT ( 'NONE',  ( -8.868684597672961800, -31.89901926473567784, -13.46243262194695944 ) ) ;
#4346 = CIRCLE ( 'NONE', #62745, 4.999999999999997335 ) ;
#4347 = FACE_BOUND ( 'NONE', #55657, .T. ) ;
#4348 = CYLINDRICAL_SURFACE ( 'NONE', #13252, 5.000000000000000888 ) ;
#4349 = ORIENTED_EDGE ( 'NONE', *, *, #18952, .T. ) ;
#4350 = AXIS2_PLACEMENT_3D ( 'NONE', #42380, #52730, #27124 ) ;
#4351 = CARTESIAN_POINT ( 'NONE',  ( 2.255723233588633470, -2.488140745366235418, -7.222632368701038530 ) ) ;
#4352 = AXIS2_PLACEMENT_3D ( 'NONE', #30337, #44974, #60927 ) ;
#4353 = ADVANCED_FACE ( 'NONE', ( #9361 ), #34951, .T. ) ;
#4354 = ORIENTED_EDGE ( 'NONE', *, *, #29039, .T. ) ;
#4355 = DIRECTION ( 'NONE',  ( 0.000000000000000000, 0.2618041379715635442, -0.9651210252299794456 ) ) ;
#4356 = DIRECTION ( 'NONE',  ( -1.000000000000000000, 0.000000000000000000, 0.000000000000000000 ) ) ;
#4357 = AXIS2_PLACEMENT_3D ( 'NONE', #4271, #40145, #44482 ) ;
#4358 = VERTEX_POINT ( 'NONE', #9697 ) ;
#4359 = CARTESIAN_POINT ( 'NONE',  ( 1.937114397841932290, 7.182898292393913309, -10.63710405811926307 ) ) ;
#4360 = DIRECTION ( 'NONE',  ( -1.000000000000000000, 0.000000000000000000, -0.000000000000000000 ) ) ;
#4361 = VECTOR ( 'NONE', #36884, 1000.000000000000000 ) ;
#4362 = CYLINDRICAL_SURFACE ( 'NONE', #65194, 7.499999999999988454 ) ;
#4363 = ORIENTED_EDGE ( 'NONE', *, *, #44501, .T. ) ;
#4364 = ORIENTED_EDGE ( 'NONE', *, *, #22030, .F. ) ;
#4365 = CARTESIAN_POINT ( 'NONE',  ( -35.00000000000000000, 9.196955404009424129, -8.830544224262844466 ) ) ;
#4366 = CIRCLE ( 'NONE', #40455, 12.74999999999999822 ) ;
#4367 = ORIENTED_EDGE ( 'NONE', *, *, #42678, .T. ) ;
#4368 = CARTESIAN_POINT ( 'NONE',  ( 0.000000000000000000, -0.2704997240205401221, 6.931223712253438585 ) ) ;
#4369 = CARTESIAN_POINT ( 'NONE',  ( -18.49080574448724690, -13.49999999999999822, -2.827202046691532642E-15 ) ) ;
#4370 = CARTESIAN_POINT ( 'NONE',  ( -0.5028117989624503181, -26.55343892596427224, 16.22424428316958256 ) ) ;
#4372 = AXIS2_PLACEMENT_3D ( 'NONE', #63328, #12784, #43714 ) ;
#4371 = CARTESIAN_POINT ( 'NONE',  ( 2.241352910868908310, -3.744764251556946366, -6.652881166698550786 ) ) ;
#4373 = DIRECTION ( 'NONE',  ( 1.000000000000000000, 0.000000000000000000, 0.000000000000000000 ) ) ;
#4374 = EDGE_CURVE ( 'NONE', #29266, #41816, #65240, .T. ) ;
#4375 = EDGE_CURVE ( 'NONE', #32447, #1539, #51403, .T. ) ;
#4376 = ORIENTED_EDGE ( 'NONE', *, *, #22938, .F. ) ;
#4377 = DIRECTION ( 'NONE',  ( 0.000000000000000000, -0.3807014730195086849, 0.9246979985058776386 ) ) ;
#4378 = CARTESIAN_POINT ( 'NONE',  ( -37.00000000000000711, 12.73293890771483383, 0.6593684648220944355 ) ) ;
#4379 = DIRECTION ( 'NONE',  ( 1.000000000000000000, 0.000000000000000000, 0.000000000000000000 ) ) ;
#4380 = EDGE_CURVE ( 'NONE', #50839, #65109, #44958, .T. ) ;
#4381 = CIRCLE ( 'NONE', #51076, 5.000000000000000888 ) ;
#4382 = AXIS2_PLACEMENT_3D ( 'NONE', #42780, #16865, #33138 ) ;
#4383 = CIRCLE ( 'NONE', #50029, 12.73084802173761787 ) ;
#4384 = CARTESIAN_POINT ( 'NONE',  ( -4.047649113456406766, -26.73415408998408083, -15.95376587162192905 ) ) ;
#4385 = CIRCLE ( 'NONE', #25583, 12.18650000000000055 ) ;
#4386 = FACE_OUTER_BOUND ( 'NONE', #42998, .T. ) ;
#4387 = CARTESIAN_POINT ( 'NONE',  ( 2.305787727787084407, -5.970480882365190034, -4.792270232040956479 ) ) ;
#4388 = CARTESIAN_POINT ( 'NONE',  ( -35.00000000000000000, 6.946017217729938409, 10.01317267707888981 ) ) ;
#4389 = DIRECTION ( 'NONE',  ( -1.000000000000000000, 0.000000000000000000, 0.000000000000000000 ) ) ;
#4390 = AXIS2_PLACEMENT_3D ( 'NONE', #4757, #35299, #32194 ) ;
#4391 = EDGE_CURVE ( 'NONE', #62601, #50166, #60246, .T. ) ;
#4392 = AXIS2_PLACEMENT_3D ( 'NONE', #32326, #17383, #52640 ) ;
#4393 = ORIENTED_EDGE ( 'NONE', *, *, #59501, .T. ) ;
#4394 = DIRECTION ( 'NONE',  ( 1.000000000000000000, 0.000000000000000000, -0.000000000000000000 ) ) ;
#4395 = AXIS2_PLACEMENT_3D ( 'NONE', #2334, #22610, #42875 ) ;
#4396 = VERTEX_POINT ( 'NONE', #55260 ) ;
#4397 = CYLINDRICAL_SURFACE ( 'NONE', #60769, 12.75000000000000178 ) ;
#4398 = CARTESIAN_POINT ( 'NONE',  ( -22.30625920655495165, 3.150098859949344909, -2.110841417170892242 ) ) ;
#4399 = DIRECTION ( 'NONE',  ( -0.000000000000000000, -1.000000000000000000, -0.000000000000000000 ) ) ;
#4400 = CARTESIAN_POINT ( 'NONE',  ( 2.268878695254622713, -1.181158368265835090, -7.551766617933176384 ) ) ;
#4401 = ORIENTED_EDGE ( 'NONE', *, *, #22350, .F. ) ;
#4402 = CIRCLE ( 'NONE', #50061, 1.499999999999997780 ) ;
#4403 = EDGE_LOOP ( 'NONE', ( #23586, #4349, #23661, #45279, #15482, #57855, #10341, #63344, #37520, #21399, #24518, #60034, #15934, #62861, #14353, #12038, #45225, #30767, #20046, #32763, #26079, #63278, #11612, #7262, #40695, #47433, #26396, #6541, #3999, #22414, #29465, #51739, #31227, #37025 ) ) ;
#4404 = ORIENTED_EDGE ( 'NONE', *, *, #2267, .F. ) ;
#4405 = CARTESIAN_POINT ( 'NONE',  ( 5.514970785353741078, -0.0005190732562555365340, 0.004694330894494709236 ) ) ;
#4406 = EDGE_CURVE ( 'NONE', #2022, #32570, #24005, .T. ) ;
#4407 = CARTESIAN_POINT ( 'NONE',  ( -35.00000000000000000, 8.534258022646220354, -8.699265615722891809 ) ) ;
#4408 = VERTEX_POINT ( 'NONE', #40952 ) ;
#4409 = DIRECTION ( 'NONE',  ( -1.000000000000000000, 0.000000000000000000, 0.000000000000000000 ) ) ;
#4410 = CARTESIAN_POINT ( 'NONE',  ( 37.00000000000000711, -3.640372113593465464, 12.21925492305365246 ) ) ;
#4411 = CARTESIAN_POINT ( 'NONE',  ( 0.2872850955227767566, -9.251080475901400035, 8.035297825011330275 ) ) ;
#4412 = VECTOR ( 'NONE', #5321, 1000.000000000000000 ) ;
#4413 = DIRECTION ( 'NONE',  ( 1.000000000000000000, 0.000000000000000000, 0.000000000000000000 ) ) ;
#4414 = ORIENTED_EDGE ( 'NONE', *, *, #59041, .T. ) ;
#4415 = FACE_OUTER_BOUND ( 'NONE', #6021, .T. ) ;
#4416 = CARTESIAN_POINT ( 'NONE',  ( 4.958255736528643709, -30.98164499407788242, -14.76282592124297288 ) ) ;
#4417 = CARTESIAN_POINT ( 'NONE',  ( 2.000000000000001776, 7.387287142779370264, -1.295372019972111932 ) ) ;
#4418 = EDGE_LOOP ( 'NONE', ( #11730, #60237, #23705, #42193 ) ) ;
#4419 = DIRECTION ( 'NONE',  ( -1.000000000000000000, 0.000000000000000000, 0.000000000000000000 ) ) ;
#4420 = ORIENTED_EDGE ( 'NONE', *, *, #48613, .F. ) ;
#4421 = CARTESIAN_POINT ( 'NONE',  ( 35.00000000000000000, 4.705694406421931860E-17, -3.469127814946512892E-15 ) ) ;
#4422 = ORIENTED_EDGE ( 'NONE', *, *, #32105, .T. ) ;
#4423 = CARTESIAN_POINT ( 'NONE',  ( -41.00000000000000711, -1.694065894508600678E-18, 0.000000000000000000 ) ) ;
#4424 = DIRECTION ( 'NONE',  ( -1.000000000000000000, 0.000000000000000000, 0.000000000000000000 ) ) ;
#4425 = CARTESIAN_POINT ( 'NONE',  ( -19.69476066079020171, -4.201994156881551312, 25.00000000000000000 ) ) ;
#4426 = DIRECTION ( 'NONE',  ( 0.000000000000000000, 0.01356324068817998940, -0.9999080150203990547 ) ) ;
#4427 = AXIS2_PLACEMENT_3D ( 'NONE', #65603, #61603, #11088 ) ;
#4428 = VECTOR ( 'NONE', #37054, 1000.000000000000000 ) ;
#4430 = AXIS2_PLACEMENT_3D ( 'NONE', #12364, #63241, #63556 ) ;
#4429 = CARTESIAN_POINT ( 'NONE',  ( -35.00000000000000000, 2.250029553613936528, -12.54989509947648862 ) ) ;
#4431 = CARTESIAN_POINT ( 'NONE',  ( 5.514624014163232779, 0.0005510299962886269819, 0.004104370840204215644 ) ) ;
#4432 = DIRECTION ( 'NONE',  ( -1.000000000000000000, -0.000000000000000000, 0.000000000000000000 ) ) ;
#4433 = CARTESIAN_POINT ( 'NONE',  ( 0.2657645697724695943, -4.045961170622937253, -11.55867655367625346 ) ) ;
#4435 = ORIENTED_EDGE ( 'NONE', *, *, #19827, .T. ) ;
#4434 = DIRECTION ( 'NONE',  ( -1.000000000000000000, 0.000000000000000000, 0.000000000000000000 ) ) ;
#4436 = ADVANCED_FACE ( 'NONE', ( #6702 ), #51608, .T. ) ;
#4437 = EDGE_LOOP ( 'NONE', ( #9980, #33598, #11430, #64585 ) ) ;
#4438 = CARTESIAN_POINT ( 'NONE',  ( -35.00000000000000000, 0.000000000000000000, 0.000000000000000000 ) ) ;
#4439 = ORIENTED_EDGE ( 'NONE', *, *, #58564, .F. ) ;
#4440 = EDGE_CURVE ( 'NONE', #40547, #21398, #61861, .T. ) ;
#4441 = ORIENTED_EDGE ( 'NONE', *, *, #528, .F. ) ;
#4442 = DIRECTION ( 'NONE',  ( 1.000000000000000000, 0.000000000000000000, 0.000000000000000000 ) ) ;
#4443 = CARTESIAN_POINT ( 'NONE',  ( 35.00000000000000000, 4.705694406421931860E-17, -3.469127814946512892E-15 ) ) ;
#4444 = CARTESIAN_POINT ( 'NONE',  ( 0.000000000000000000, -3.152010634611648321, -6.039758645301327000 ) ) ;
#4445 = DIRECTION ( 'NONE',  ( -1.000000000000000000, -0.000000000000000000, -0.000000000000000000 ) ) ;
#4446 = LINE ( 'NONE', #19738, #26364 ) ;
#4447 = AXIS2_PLACEMENT_3D ( 'NONE', #29878, #25551, #64788 ) ;
#4448 = CARTESIAN_POINT ( 'NONE',  ( -35.00000000000000000, -11.29812557209474733, -3.213188559034363401 ) ) ;
#4449 = ADVANCED_FACE ( 'NONE', ( #1714 ), #20980, .T. ) ;
#4450 = FACE_OUTER_BOUND ( 'NONE', #6377, .T. ) ;
#4451 = CONICAL_SURFACE ( 'NONE', #39438, 7.938172270156617749, 1.280189991382167047 ) ;
#4452 = ORIENTED_EDGE ( 'NONE', *, *, #8794, .F. ) ;
#4453 = FACE_OUTER_BOUND ( 'NONE', #29006, .T. ) ;
#4454 = AXIS2_PLACEMENT_3D ( 'NONE', #41269, #29654, #30331 ) ;
#4455 = CARTESIAN_POINT ( 'NONE',  ( -19.47984447937493613, -3.750539801530005768, 11.39883551934753925 ) ) ;
#4456 = CARTESIAN_POINT ( 'NONE',  ( -18.89779455570165467, -4.072785471668618484, 12.87288005866979290 ) ) ;
#4457 = ADVANCED_FACE ( 'NONE', ( #26978 ), #6368, .T. ) ;
#4458 = EDGE_CURVE ( 'NONE', #40836, #31528, #20424, .T. ) ;
#4459 = ORIENTED_EDGE ( 'NONE', *, *, #15976, .F. ) ;
#4460 = B_SPLINE_CURVE_WITH_KNOTS ( 'NONE', 3,
 ( #14586, #17732, #33345, #34864, #2447, #53957, #55173, #8396 ),
 .UNSPECIFIED., .F., .F.,
 ( 4, 2, 2, 4 ),
 ( 0.000000000000000000, 0.0003639104015150018061, 0.0007278208030300036121, 0.001455641606060007224 ),
 .UNSPECIFIED. ) ;
#4461 = CIRCLE ( 'NONE', #19315, 5.000000000000000000 ) ;
#4462 = CARTESIAN_POINT ( 'NONE',  ( -4.989057617119008192, -0.9162120371760335003, 13.46887357958837406 ) ) ;
#4463 = B_SPLINE_CURVE_WITH_KNOTS ( 'NONE', 3,
 ( #4140, #24406, #9768, #44674, #34052, #39706, #24752, #55327, #65302, #14424, #35363, #30386, #19769, #40027, #60313, #50680, #35686, #57892 ),
 .UNSPECIFIED., .F., .F.,
 ( 4, 2, 2, 2, 2, 2, 2, 2, 4 ),
 ( 0.004907007814975161697, 0.005737531593967190244, 0.006568055372959219658, 0.007398579151951248205, 0.008229102930943277619, 0.009059626709935306166, 0.009890150488927336447, 0.01072067426791936673, 0.01155119804691139528 ),
 .UNSPECIFIED. ) ;
#4464 = CARTESIAN_POINT ( 'NONE',  ( 35.00000000000000000, -11.29812557209478996, -3.213188559034203529 ) ) ;
#4465 = CARTESIAN_POINT ( 'NONE',  ( 0.000000000000000000, -33.00000000000000000, 0.000000000000000000 ) ) ;
#4466 = ORIENTED_EDGE ( 'NONE', *, *, #37652, .T. ) ;
#4467 = CARTESIAN_POINT ( 'NONE',  ( 2.290907136833252977, 6.705538900522879153, -3.684064771923190484 ) ) ;
#4468 = CARTESIAN_POINT ( 'NONE',  ( 10.04668509498937645, -32.26295471732144193, 12.85148783289558239 ) ) ;
#4469 = DIRECTION ( 'NONE',  ( -1.000000000000000000, 0.000000000000000000, 0.000000000000000000 ) ) ;
#4470 = AXIS2_PLACEMENT_3D ( 'NONE', #38398, #32089, #53385 ) ;
#4471 = VECTOR ( 'NONE', #15929, 1000.000000000000114 ) ;
#4472 = AXIS2_PLACEMENT_3D ( 'NONE', #53703, #8137, #7461 ) ;
#4473 = CARTESIAN_POINT ( 'NONE',  ( 37.00000000000000711, 7.251710744571704836, 9.240395740215555875 ) ) ;
#4474 = DIRECTION ( 'NONE',  ( -1.000000000000000000, 0.000000000000000000, -0.000000000000000000 ) ) ;
#4475 =( BOUNDED_SURFACE ( )  B_SPLINE_SURFACE ( 3, 1, ( 
 ( #48389, #7809 ),
 ( #43035, #38038 ),
 ( #58345, #7132 ),
 ( #28401, #12767 ) ),
 .UNSPECIFIED., .F., .F., .F. ) 
 B_SPLINE_SURFACE_WITH_KNOTS ( ( 4, 4 ),
 ( 2, 2 ),
 ( 0.000000000000000000, 1.000000000000000000 ),
 ( 0.000000000000000000, 1.000000000000000000 ),
 .UNSPECIFIED. ) 
 GEOMETRIC_REPRESENTATION_ITEM ( )  RATIONAL_B_SPLINE_SURFACE ( (
 ( 1.000000000000000000, 1.000000000000000000),
 ( 0.6933888150995267674, 0.9895912004443193632),
 ( 0.6933888150995267674, 0.9895912004443193632),
 ( 1.000000000000000000, 1.000000000000000000) ) ) 
 REPRESENTATION_ITEM ( '' )  SURFACE ( )  );
#4476 = ORIENTED_EDGE ( 'NONE', *, *, #14771, .T. ) ;
#4477 = CARTESIAN_POINT ( 'NONE',  ( 2.256373768223415510, 0.1329433694244317177, 7.638251659827612450 ) ) ;
#4478 = CARTESIAN_POINT ( 'NONE',  ( -22.27715239060371744, 3.521735673127126542, 1.072868796692219240 ) ) ;
#4479 = LINE ( 'NONE', #60311, #15893 ) ;
#4480 = EDGE_LOOP ( 'NONE', ( #3883, #34523, #31116, #17431 ) ) ;
#4481 = CARTESIAN_POINT ( 'NONE',  ( -27.45775109278351067, 11.83395752356219077, -1.989333891161980894 ) ) ;
#4482 = DIRECTION ( 'NONE',  ( -1.000000000000000000, 0.000000000000000000, 0.000000000000000000 ) ) ;
#4483 = ORIENTED_EDGE ( 'NONE', *, *, #33472, .T. ) ;
#4484 = EDGE_CURVE ( 'NONE', #44370, #29968, #21320, .T. ) ;
#4485 = VERTEX_POINT ( 'NONE', #25999 ) ;
#4486 = ORIENTED_EDGE ( 'NONE', *, *, #8419, .F. ) ;
#4487 = AXIS2_PLACEMENT_3D ( 'NONE', #18748, #39005, #29357 ) ;
#4488 = ADVANCED_FACE ( 'NONE', ( #31614 ), #42231, .T. ) ;
#4489 = AXIS2_PLACEMENT_3D ( 'NONE', #45754, #40776, #47083 ) ;
#4490 = ORIENTED_EDGE ( 'NONE', *, *, #16136, .F. ) ;
#4491 = AXIS2_PLACEMENT_3D ( 'NONE', #5448, #52312, #27026 ) ;
#4492 = DIRECTION ( 'NONE',  ( -1.000000000000000000, 0.000000000000000000, 0.000000000000000000 ) ) ;
#4493 = FACE_OUTER_BOUND ( 'NONE', #2919, .T. ) ;
#4494 = FACE_OUTER_BOUND ( 'NONE', #12581, .T. ) ;
#4495 = CARTESIAN_POINT ( 'NONE',  ( 6.361445718264521432, -4.355102044641763648, 11.18181944858514498 ) ) ;
#4496 = CARTESIAN_POINT ( 'NONE',  ( -15.98984497772178770, -34.99999999818471963, 5.008554314762531767 ) ) ;
#4497 = CARTESIAN_POINT ( 'NONE',  ( 11.86852745065355741, -10.64790170674533165, -8.300198448557058128 ) ) ;
#4499 = ORIENTED_EDGE ( 'NONE', *, *, #26117, .F. ) ;
#4498 = CYLINDRICAL_SURFACE ( 'NONE', #19180, 5.000000000000000888 ) ;
#4500 = LINE ( 'NONE', #34411, #55403 ) ;
#4501 = ORIENTED_EDGE ( 'NONE', *, *, #45939, .T. ) ;
#4502 = DIRECTION ( 'NONE',  ( -0.000000000000000000, -1.000000000000000000, -0.000000000000000000 ) ) ;
#4503 = ORIENTED_EDGE ( 'NONE', *, *, #18439, .F. ) ;
#4504 = ORIENTED_EDGE ( 'NONE', *, *, #55773, .F. ) ;
#4505 = CARTESIAN_POINT ( 'NONE',  ( -22.30398854582848145, -0.8844201765542077931, 3.656532484463041577 ) ) ;
#4506 = CARTESIAN_POINT ( 'NONE',  ( 16.03117610287102579, -29.21144266226587760, 10.60889071582655241 ) ) ;
#4507 = CARTESIAN_POINT ( 'NONE',  ( -35.00000000000000000, -8.389074212634351824, 8.839356091080015076 ) ) ;
#4508 = ADVANCED_FACE ( 'NONE', ( #41602 ), #51280, .T. ) ;
#4509 = CARTESIAN_POINT ( 'NONE',  ( -47.00000000000000711, 0.000000000000000000, 0.000000000000000000 ) ) ;
#4510 = FACE_OUTER_BOUND ( 'NONE', #38978, .T. ) ;
#4511 = CARTESIAN_POINT ( 'NONE',  ( 35.00000000000000000, 8.839356091080166067, 8.389074212634184846 ) ) ;
#4512 = ORIENTED_EDGE ( 'NONE', *, *, #6769, .T. ) ;
#4513 = AXIS2_PLACEMENT_3D ( 'NONE', #54156, #29516, #49819 ) ;
#4514 = EDGE_CURVE ( 'NONE', #33155, #16289, #45924, .T. ) ;
#4515 = ORIENTED_EDGE ( 'NONE', *, *, #64778, .F. ) ;
#4516 = DIRECTION ( 'NONE',  ( -1.000000000000000000, 0.000000000000000000, 0.000000000000000000 ) ) ;
#4517 = ORIENTED_EDGE ( 'NONE', *, *, #18521, .T. ) ;
#4518 = EDGE_CURVE ( 'NONE', #17303, #7978, #57612, .T. ) ;
#4519 = ORIENTED_EDGE ( 'NONE', *, *, #8270, .T. ) ;
#4521 = VECTOR ( 'NONE', #54462, 1000.000000000000000 ) ;
#4520 = DIRECTION ( 'NONE',  ( 1.000000000000000000, 0.000000000000000000, 0.000000000000000000 ) ) ;
#4522 = CARTESIAN_POINT ( 'NONE',  ( 0.2706063244538030599, 0.1752385892653718358, -12.24670371972918126 ) ) ;
#4523 = CARTESIAN_POINT ( 'NONE',  ( 18.78313359089984402, -1.065647145831489118, 12.00131809889008316 ) ) ;
#4524 = CARTESIAN_POINT ( 'NONE',  ( -22.27722015946439171, 1.271715168852085132, -3.455127654605127496 ) ) ;
#4525 = CIRCLE ( 'NONE', #15125, 5.000000000000000888 ) ;
#4526 = FACE_OUTER_BOUND ( 'NONE', #52474, .T. ) ;
#4527 = VECTOR ( 'NONE', #24748, 1000.000000000000000 ) ;
#4528 = EDGE_CURVE ( 'NONE', #32831, #55569, #39546, .T. ) ;
#4529 = CARTESIAN_POINT ( 'NONE',  ( 1.719304012341412724, 1.452142814149018690, -12.64775761152637301 ) ) ;
#4530 = ORIENTED_EDGE ( 'NONE', *, *, #8419, .T. ) ;
#4531 = ADVANCED_FACE ( 'NONE', ( #62210 ), #15658, .T. ) ;
#4532 = VERTEX_POINT ( 'NONE', #37263 ) ;
#4533 = DIRECTION ( 'NONE',  ( -1.000000000000000000, 0.000000000000000000, 0.000000000000000000 ) ) ;
#4534 = DIRECTION ( 'NONE',  ( -0.5446691071471760903, 0.8386510381079236298, 0.000000000000000000 ) ) ;
#4535 = DIRECTION ( 'NONE',  ( -1.000000000000000000, 0.000000000000000000, 0.000000000000000000 ) ) ;
#4536 = VECTOR ( 'NONE', #53489, 1000.000000000000000 ) ;
#4537 = AXIS2_PLACEMENT_3D ( 'NONE', #14494, #50439, #4884 ) ;
#4538 = CARTESIAN_POINT ( 'NONE',  ( -35.00000000000000000, 0.000000000000000000, 0.000000000000000000 ) ) ;
#4539 = CARTESIAN_POINT ( 'NONE',  ( -28.08328025583519860, 11.67727086453252028, -6.780915823467608128 ) ) ;
#4540 = EDGE_CURVE ( 'NONE', #16636, #15834, #7017, .T. ) ;
#4541 = VECTOR ( 'NONE', #11345, 1000.000000000000000 ) ;
#4542 = CARTESIAN_POINT ( 'NONE',  ( 7.298320481653675529, -6.062943420091013280, -12.06387388335232735 ) ) ;
#4543 = LINE ( 'NONE', #18841, #9890 ) ;
#4544 = AXIS2_PLACEMENT_3D ( 'NONE', #51548, #15920, #17259 ) ;
#4545 = DIRECTION ( 'NONE',  ( 0.000000000000000000, 0.9903235168508555120, 0.1387779952735782862 ) ) ;
#4546 = CARTESIAN_POINT ( 'NONE',  ( 3.455388140186490986, 8.284410676190358203, 8.681632586536974117 ) ) ;
#4547 = ORIENTED_EDGE ( 'NONE', *, *, #3501, .T. ) ;
#4548 = CARTESIAN_POINT ( 'NONE',  ( 2.368238019614961054, -5.994627685102860148, -4.795442552788027335 ) ) ;
#4549 = CARTESIAN_POINT ( 'NONE',  ( 22.78424990826529495, -4.691658877507584258, -11.04575192261954264 ) ) ;
#4550 = CARTESIAN_POINT ( 'NONE',  ( 22.36482863261543486, 11.96441317219527889, -0.9234811557364158707 ) ) ;
#4551 = CARTESIAN_POINT ( 'NONE',  ( -4.348075857621052087, -31.41176936172981726, -14.02665938296879844 ) ) ;
#4552 = AXIS2_PLACEMENT_3D ( 'NONE', #25407, #56318, #146 ) ;
#4553 = CARTESIAN_POINT ( 'NONE',  ( 0.9232167919969166414, -4.649596781010333579, -11.56588005394303131 ) ) ;
#4554 = ORIENTED_EDGE ( 'NONE', *, *, #34292, .T. ) ;
#4555 = CARTESIAN_POINT ( 'NONE',  ( 35.00000000000000000, 4.705694406421931860E-17, -3.469127814946512892E-15 ) ) ;
#4556 = CARTESIAN_POINT ( 'NONE',  ( 2.373367633546856759, 6.557448619657638034, 3.994744114396107104 ) ) ;
#4557 = CARTESIAN_POINT ( 'NONE',  ( -0.4156926711315701573, -31.03628804997841684, -14.44394305974772408 ) ) ;
#4558 = EDGE_LOOP ( 'NONE', ( #23336, #42826, #32160, #14044 ) ) ;
#4559 = CARTESIAN_POINT ( 'NONE',  ( -27.01437459610461644, -11.79277645698183186, -2.220455681983952267 ) ) ;
#4560 = CARTESIAN_POINT ( 'NONE',  ( -35.00000000000000000, -10.63508530065525370, 4.986700593229667078 ) ) ;
#4561 = AXIS2_PLACEMENT_3D ( 'NONE', #35012, #4135, #14419 ) ;
#4562 = AXIS2_PLACEMENT_3D ( 'NONE', #41596, #31611, #55916 ) ;
#4563 = CARTESIAN_POINT ( 'NONE',  ( 0.3002738374340793714, -8.050654058169927296, 9.243462099800803244 ) ) ;
#4564 = CARTESIAN_POINT ( 'NONE',  ( 0.000000000000000000, 0.000000000000000000, 0.000000000000000000 ) ) ;
#4565 = VECTOR ( 'NONE', #57791, 1000.000000000000000 ) ;
#4566 = ADVANCED_FACE ( 'NONE', ( #57574 ), #724, .T. ) ;
#4567 = CIRCLE ( 'NONE', #41716, 2.899999999999996803 ) ;
#4568 = CARTESIAN_POINT ( 'NONE',  ( 1.000000000000000888, 6.936109781200682889, 2.853135311045038591 ) ) ;
#4569 = VERTEX_POINT ( 'NONE', #57238 ) ;
#4570 = FACE_OUTER_BOUND ( 'NONE', #20764, .T. ) ;
#4571 = DIRECTION ( 'NONE',  ( 0.000000000000000000, 0.000000000000000000, 1.000000000000000000 ) ) ;
#4572 = CARTESIAN_POINT ( 'NONE',  ( -14.24546914926061625, 8.298873997449982554, -10.64811974057628952 ) ) ;
#4573 = CARTESIAN_POINT ( 'NONE',  ( 1.375507693220225480, -1.606074886184773787, -12.51366828189718738 ) ) ;
#4574 = DIRECTION ( 'NONE',  ( 1.000000000000000000, 0.000000000000000000, 0.000000000000000000 ) ) ;
#4575 = CYLINDRICAL_SURFACE ( 'NONE', #502, 12.18649999999999878 ) ;
#4576 = DIRECTION ( 'NONE',  ( 1.000000000000000000, 0.000000000000000000, -0.000000000000000000 ) ) ;
#4577 = ORIENTED_EDGE ( 'NONE', *, *, #53382, .T. ) ;
#4578 = ORIENTED_EDGE ( 'NONE', *, *, #54969, .T. ) ;
#4579 = CARTESIAN_POINT ( 'NONE',  ( 2.245754705088395031, -4.993005209687621182, 5.777230445738523734 ) ) ;
#4580 = VECTOR ( 'NONE', #46393, 1000.000000000000000 ) ;
#4581 = ORIENTED_EDGE ( 'NONE', *, *, #45464, .F. ) ;
#4582 = VECTOR ( 'NONE', #58203, 1000.000000000000000 ) ;
#4583 = CARTESIAN_POINT ( 'NONE',  ( -37.00000000000000711, 0.000000000000000000, 0.000000000000000000 ) ) ;
#4584 = ADVANCED_FACE ( 'NONE', ( #11665 ), #31939, .T. ) ;
#4585 = CARTESIAN_POINT ( 'NONE',  ( -37.00000000000000711, 5.710938531231712467, 11.39945968423473666 ) ) ;
#4586 = ORIENTED_EDGE ( 'NONE', *, *, #63632, .F. ) ;
#4587 = DIRECTION ( 'NONE',  ( 1.000000000000000000, -0.000000000000000000, -0.000000000000000000 ) ) ;
#4588 = CARTESIAN_POINT ( 'NONE',  ( 11.05611852032334319, 11.87696910296720532, -1.718393329984558626 ) ) ;
#4589 = EDGE_CURVE ( 'NONE', #21047, #36610, #63653, .T. ) ;
#4591 = B_SPLINE_CURVE_WITH_KNOTS ( 'NONE', 3,
 ( #40856, #5280, #55490, #20232, #627, #25550, #35828, #20889, #4298, #14263, #29877, #55154, #24907, #14568, #15565, #40175, #45184, #9938, #34543, #45844, #50834, #40512 ),
 .UNSPECIFIED., .F., .F.,
 ( 4, 3, 3, 3, 3, 3, 3, 4 ),
 ( 1.230521702633870283E-18, 4.449119708436919475E-05, 6.626296329540433730E-05, 8.803456484962549208E-05, 0.0001098060367612784546, 0.0001315774408628484155, 0.0001760698110411127392, 0.0001829697163287819926 ),
 .UNSPECIFIED. ) ;
#4590 = CARTESIAN_POINT ( 'NONE',  ( 29.51976981715666781, 7.690765383426390045, 11.09513982864076276 ) ) ;
#4592 = ORIENTED_EDGE ( 'NONE', *, *, #9241, .T. ) ;
#4593 = AXIS2_PLACEMENT_3D ( 'NONE', #54405, #40644, #50642 ) ;
#4594 = ORIENTED_EDGE ( 'NONE', *, *, #38046, .T. ) ;
#4595 = CYLINDRICAL_SURFACE ( 'NONE', #36371, 12.18650000000000055 ) ;
#4596 = EDGE_CURVE ( 'NONE', #2241, #43998, #40645, .T. ) ;
#4597 = ORIENTED_EDGE ( 'NONE', *, *, #62553, .T. ) ;
#4598 = CARTESIAN_POINT ( 'NONE',  ( -27.08430792439081003, 0.6005833784282779142, -2.211452765398048914 ) ) ;
#4599 = ORIENTED_EDGE ( 'NONE', *, *, #16761, .F. ) ;
#4600 = CARTESIAN_POINT ( 'NONE',  ( -10.00000000000000178, 0.000000000000000000, 0.000000000000000000 ) ) ;
#4601 = CARTESIAN_POINT ( 'NONE',  ( -27.09861164373112885, 1.025570525056652693, -2.097104182796081240 ) ) ;
#4602 = CARTESIAN_POINT ( 'NONE',  ( 2.835339799623977086, -4.197472173747748059, 6.612744557053419570 ) ) ;
#4603 = DIRECTION ( 'NONE',  ( -1.000000000000000000, 0.000000000000000000, 0.000000000000000000 ) ) ;
#4604 = VECTOR ( 'NONE', #36065, 1000.000000000000000 ) ;
#4605 = DIRECTION ( 'NONE',  ( 0.000000000000000000, 0.000000000000000000, 1.000000000000000000 ) ) ;
#4606 = ORIENTED_EDGE ( 'NONE', *, *, #27251, .T. ) ;
#4607 = CARTESIAN_POINT ( 'NONE',  ( 1.462291587749944943, -12.08418494300879509, 3.724645088506750135 ) ) ;
#4608 = EDGE_CURVE ( 'NONE', #52575, #33456, #43904, .T. ) ;
#4609 = DIRECTION ( 'NONE',  ( 1.000000000000000000, 0.000000000000000000, 0.000000000000000000 ) ) ;
#4610 = CARTESIAN_POINT ( 'NONE',  ( 35.00000000000000000, 4.705694406421931860E-17, -3.469127814946512892E-15 ) ) ;
#4611 = EDGE_CURVE ( 'NONE', #56955, #27835, #33912, .T. ) ;
#4612 = DIRECTION ( 'NONE',  ( 0.000000000000000000, 0.01356324068817992175, -0.9999080150203990547 ) ) ;
#4614 = CARTESIAN_POINT ( 'NONE',  ( 2.241451721903215066, -7.528807736569459230, 1.265761656830178161 ) ) ;
#4613 = CIRCLE ( 'NONE', #23691, 4.999999999999999112 ) ;
#4615 = CARTESIAN_POINT ( 'NONE',  ( 0.6511581176971041884, 0.3309006379880005677, -12.37037447926147138 ) ) ;
#4616 = CARTESIAN_POINT ( 'NONE',  ( -27.28573687977896611, 2.862048090118431976, 0.4470060700698362810 ) ) ;
#4617 = CARTESIAN_POINT ( 'NONE',  ( 35.00000000000000000, 4.705694406421931860E-17, -3.469127814946512892E-15 ) ) ;
#4618 = AXIS2_PLACEMENT_3D ( 'NONE', #44377, #64655, #19124 ) ;
#4619 = CARTESIAN_POINT ( 'NONE',  ( 37.00000000000000711, -9.821084925794620446, -7.215058775251224077 ) ) ;
#4620 = EDGE_CURVE ( 'NONE', #45757, #57898, #27170, .T. ) ;
#4621 = AXIS2_PLACEMENT_3D ( 'NONE', #25068, #4469, #54356 ) ;
#4622 = AXIS2_PLACEMENT_3D ( 'NONE', #25238, #65776, #55839 ) ;
#4623 = ORIENTED_EDGE ( 'NONE', *, *, #7872, .F. ) ;
#4624 = CARTESIAN_POINT ( 'NONE',  ( 0.2834382757447986845, 0.2027202995056993362, 12.25055062943085282 ) ) ;
#4625 = EDGE_CURVE ( 'NONE', #35019, #34453, #21652, .T. ) ;
#4626 = ORIENTED_EDGE ( 'NONE', *, *, #58715, .F. ) ;
#4627 = CARTESIAN_POINT ( 'NONE',  ( -2.532614230583022152, -11.30437021680553222, 4.026315189028233377 ) ) ;
#4628 = CARTESIAN_POINT ( 'NONE',  ( -22.27704833740210333, -3.663709865074144201, 0.3581593033281248450 ) ) ;
#4629 = CARTESIAN_POINT ( 'NONE',  ( 5.530133899448235191, -0.01550764871776214027, -0.003876417824003597183 ) ) ;
#4630 = AXIS2_PLACEMENT_3D ( 'NONE', #7361, #18694, #43266 ) ;
#4631 = EDGE_CURVE ( 'NONE', #7848, #53238, #47914, .T. ) ;
#4632 = DIRECTION ( 'NONE',  ( -1.000000000000000000, 0.000000000000000000, 0.000000000000000000 ) ) ;
#4633 = CARTESIAN_POINT ( 'NONE',  ( 3.152665057734130638, 7.609997527621177760, -2.258875078502145861 ) ) ;
#4634 = ORIENTED_EDGE ( 'NONE', *, *, #47403, .T. ) ;
#4635 = DIRECTION ( 'NONE',  ( 0.000000000000000000, 0.000000000000000000, 1.000000000000000000 ) ) ;
#4636 = CARTESIAN_POINT ( 'NONE',  ( 3.031336079628980329, 2.306006909710660580, -7.553623348802083193 ) ) ;
#4637 = CARTESIAN_POINT ( 'NONE',  ( 10.09892164510067580, 1.646990700008696518, 11.88792003737877145 ) ) ;
#4638 = CARTESIAN_POINT ( 'NONE',  ( 35.00000000000000000, -11.60979404548631777, 3.704519465651427534 ) ) ;
#4639 = CARTESIAN_POINT ( 'NONE',  ( 35.00000000000000000, -8.352657516904727686, -8.258652103341406203 ) ) ;
#4640 = CIRCLE ( 'NONE', #20573, 12.18650000000000055 ) ;
#4641 = ORIENTED_EDGE ( 'NONE', *, *, #40737, .F. ) ;
#4642 = DIRECTION ( 'NONE',  ( -1.000000000000000000, -0.000000000000000000, -0.000000000000000000 ) ) ;
#4643 = ORIENTED_EDGE ( 'NONE', *, *, #11728, .F. ) ;
#4644 = DIRECTION ( 'NONE',  ( 1.000000000000000000, 0.000000000000000000, -0.000000000000000000 ) ) ;
#4645 = CYLINDRICAL_SURFACE ( 'NONE', #28870, 12.74999999999999822 ) ;
#4646 = CARTESIAN_POINT ( 'NONE',  ( 10.75853767213705225, 7.830989516993144051, -9.092612561015865680 ) ) ;
#4647 = DIRECTION ( 'NONE',  ( 1.000000000000000000, 0.000000000000000000, 0.000000000000000000 ) ) ;
#4648 = EDGE_CURVE ( 'NONE', #63364, #64117, #22649, .T. ) ;
#4649 = CIRCLE ( 'NONE', #57767, 4.999999999999999112 ) ;
#4650 = ORIENTED_EDGE ( 'NONE', *, *, #10647, .T. ) ;
#4651 = VERTEX_POINT ( 'NONE', #4674 ) ;
#4652 = CARTESIAN_POINT ( 'NONE',  ( -27.09229696323321335, 2.225368503508855067, -0.6397626223479118135 ) ) ;
#4653 = ORIENTED_EDGE ( 'NONE', *, *, #44835, .T. ) ;
#4654 = DIRECTION ( 'NONE',  ( 0.000000000000000000, 0.01356324068817998940, -0.9999080150203989437 ) ) ;
#4655 = CARTESIAN_POINT ( 'NONE',  ( 35.00000000000000000, -7.717887834988180984, 8.854740511458926377 ) ) ;
#4656 = FACE_OUTER_BOUND ( 'NONE', #14761, .T. ) ;
#4657 = CYLINDRICAL_SURFACE ( 'NONE', #2478, 2.899999999999994582 ) ;
#4658 = CARTESIAN_POINT ( 'NONE',  ( 2.524535260912970536, 6.580044328001175558, -4.054303386867658787 ) ) ;
#4659 = DIRECTION ( 'NONE',  ( 0.000000000000000000, 0.000000000000000000, 1.000000000000000000 ) ) ;
#4660 = CARTESIAN_POINT ( 'NONE',  ( 12.93723047338301058, 4.476360154859203355, 25.00000000000000000 ) ) ;
#4661 = VERTEX_POINT ( 'NONE', #64813 ) ;
#4662 = AXIS2_PLACEMENT_3D ( 'NONE', #49038, #24983, #61205 ) ;
#4663 = ADVANCED_FACE ( 'NONE', ( #35553 ), #64494, .T. ) ;
#4664 = AXIS2_PLACEMENT_3D ( 'NONE', #50708, #62614, #17423 ) ;
#4666 = ORIENTED_EDGE ( 'NONE', *, *, #6181, .T. ) ;
#4665 = CARTESIAN_POINT ( 'NONE',  ( 0.3002738374340858107, -12.03040002643110284, -2.350339881555072008 ) ) ;
#4667 = ORIENTED_EDGE ( 'NONE', *, *, #13485, .F. ) ;
#4668 = B_SPLINE_CURVE_WITH_KNOTS ( 'NONE', 3,
 ( #59740, #59102, #33491, #24821, #50097, #54762, #3244, #19510, #53782, #23515, #13829, #8216, #4207, #39779 ),
 .UNSPECIFIED., .F., .F.,
 ( 4, 2, 2, 2, 2, 2, 4 ),
 ( 2.453269466693398698E-18, 0.001897844907058980971, 0.002846767360588470155, 0.003795689814117958905, 0.004744612267647447222, 0.005693534721176935973, 0.007591379628235916943 ),
 .UNSPECIFIED. ) ;
#4669 = CYLINDRICAL_SURFACE ( 'NONE', #43627, 5.000000000000000888 ) ;
#4670 = VECTOR ( 'NONE', #9499, 1000.000000000000000 ) ;
#4671 = CARTESIAN_POINT ( 'NONE',  ( -15.69195845145067736, -33.00000000000000000, 4.009712365929964051 ) ) ;
#4672 = EDGE_CURVE ( 'NONE', #57650, #65336, #43827, .T. ) ;
#4673 = ORIENTED_EDGE ( 'NONE', *, *, #2867, .F. ) ;
#4674 = CARTESIAN_POINT ( 'NONE',  ( 35.00000000000000000, -10.64792938439759595, -5.927257550915285833 ) ) ;
#4675 = ORIENTED_EDGE ( 'NONE', *, *, #44741, .T. ) ;
#4676 = CARTESIAN_POINT ( 'NONE',  ( 2.000000000000001776, 2.664846396702499121, 6.404188155572998475 ) ) ;
#4677 = DIRECTION ( 'NONE',  ( 0.000000000000000000, 0.01356324068817998940, -0.9999080150203990547 ) ) ;
#4678 = B_SPLINE_CURVE_WITH_KNOTS ( 'NONE', 3,
 ( #27486, #11542, #18187, #22855, #53443, #43106, #37803, #42116, #43428, #27173, #1907, #38115, #63383, #6902, #22175, #7888, #62400, #48131, #37136 ),
 .UNSPECIFIED., .F., .F.,
 ( 4, 3, 3, 3, 3, 3, 4 ),
 ( 0.000000000000000000, 2.836829842860724867E-05, 4.224792512343544923E-05, 5.612066614708095569E-05, 6.998859278152062813E-05, 9.832141287889069976E-05, 0.0001178161482480190834 ),
 .UNSPECIFIED. ) ;
#4679 = CARTESIAN_POINT ( 'NONE',  ( 37.00000000000000711, -10.42955799785315563, 6.303578524887051948 ) ) ;
#4680 = CARTESIAN_POINT ( 'NONE',  ( 2.556980015513660831, 7.190718924764508913, -2.862731173723810141 ) ) ;
#4681 = ORIENTED_EDGE ( 'NONE', *, *, #50536, .F. ) ;
#4682 = CIRCLE ( 'NONE', #25879, 12.18650000000000055 ) ;
#4683 = ORIENTED_EDGE ( 'NONE', *, *, #28314, .T. ) ;
#4684 = DIRECTION ( 'NONE',  ( 1.000000000000000000, -0.000000000000000000, -0.000000000000000000 ) ) ;
#4685 = ADVANCED_FACE ( 'NONE', ( #30247 ), #36899, .F. ) ;
#4686 = VERTEX_POINT ( 'NONE', #18963 ) ;
#4687 = CARTESIAN_POINT ( 'NONE',  ( 0.3218525148189846363, 11.60666749448229496, -3.964374483810531924 ) ) ;
#4688 = ORIENTED_EDGE ( 'NONE', *, *, #24378, .T. ) ;
#4689 = AXIS2_PLACEMENT_3D ( 'NONE', #5191, #25458, #10482 ) ;
#4690 = VERTEX_POINT ( 'NONE', #34872 ) ;
#4691 = ORIENTED_EDGE ( 'NONE', *, *, #26416, .F. ) ;
#4692 = DIRECTION ( 'NONE',  ( 0.000000000000000000, 0.1740410799127614649, 0.9847383929261618318 ) ) ;
#4693 = AXIS2_PLACEMENT_3D ( 'NONE', #9779, #45040, #8814 ) ;
#4694 = CARTESIAN_POINT ( 'NONE',  ( -0.4967434119545920956, -25.72578597719286719, 15.66300405139958407 ) ) ;
#4695 = CYLINDRICAL_SURFACE ( 'NONE', #56360, 4.999999999999999112 ) ;
#4696 = CARTESIAN_POINT ( 'NONE',  ( -22.46509356695198889, -2.840174833751764272, 3.157489876851286681 ) ) ;
#4697 = ORIENTED_EDGE ( 'NONE', *, *, #30812, .F. ) ;
#4698 = DIRECTION ( 'NONE',  ( -1.000000000000000000, 0.000000000000000000, 0.000000000000000000 ) ) ;
#4699 = VERTEX_POINT ( 'NONE', #59524 ) ;
#4700 =( BOUNDED_CURVE ( )  B_SPLINE_CURVE ( 3, ( #4204, #54757, #49455, #64694 ),
 .UNSPECIFIED., .F., .F. ) 
 B_SPLINE_CURVE_WITH_KNOTS ( ( 4, 4 ),
 ( 1.625261828949994269, 1.639255800632265947 ),
 .UNSPECIFIED. ) 
 CURVE ( )  GEOMETRIC_REPRESENTATION_ITEM ( )  RATIONAL_B_SPLINE_CURVE ( ( 1.000000000000000000, 0.9999836807962925178, 0.9999836807962925178, 1.000000000000000000 ) ) 
 REPRESENTATION_ITEM ( '' )  );
#4701 = CARTESIAN_POINT ( 'NONE',  ( -17.54726996257253191, -11.36053454945672136, 3.865003848717349033 ) ) ;
#4702 = AXIS2_PLACEMENT_3D ( 'NONE', #25511, #25188, #19565 ) ;
#4703 = DIRECTION ( 'NONE',  ( -1.000000000000000000, 0.000000000000000000, 0.000000000000000000 ) ) ;
#4704 = ORIENTED_EDGE ( 'NONE', *, *, #37989, .F. ) ;
#4705 = FACE_OUTER_BOUND ( 'NONE', #19790, .T. ) ;
#4706 = CARTESIAN_POINT ( 'NONE',  ( 0.2657645697724702050, 4.045961170623010972, 11.55867655367622326 ) ) ;
#4707 = CARTESIAN_POINT ( 'NONE',  ( 2.269879328256726669, -6.692746930935540739, -3.692763753156722561 ) ) ;
#4708 = EDGE_CURVE ( 'NONE', #50294, #34584, #15140, .T. ) ;
#4709 = CIRCLE ( 'NONE', #24853, 12.73084802173761787 ) ;
#4710 = VERTEX_POINT ( 'NONE', #60171 ) ;
#4711 = DIRECTION ( 'NONE',  ( 0.000000000000000000, -0.07632122047555053856, 0.9970832820307050648 ) ) ;
#4712 = EDGE_CURVE ( 'NONE', #9845, #13243, #33189, .T. ) ;
#4713 = ORIENTED_EDGE ( 'NONE', *, *, #42221, .T. ) ;
#4714 = DIRECTION ( 'NONE',  ( -1.000000000000000000, -0.000000000000000000, -0.000000000000000000 ) ) ;
#4715 = CARTESIAN_POINT ( 'NONE',  ( 0.000000000000000000, 0.000000000000000000, 0.000000000000000000 ) ) ;
#4716 = CARTESIAN_POINT ( 'NONE',  ( 2.770579946183333142, 6.910873157406283163, -3.639932028439744727 ) ) ;
#4717 = EDGE_CURVE ( 'NONE', #49616, #16668, #23671, .T. ) ;
#4718 = CARTESIAN_POINT ( 'NONE',  ( 2.247206125382658737, -3.717496781928407046, -6.670391186503415781 ) ) ;
#4719 = DIRECTION ( 'NONE',  ( 0.000000000000000000, 0.01356324068817998940, -0.9999080150203989437 ) ) ;
#4720 = ORIENTED_EDGE ( 'NONE', *, *, #65519, .F. ) ;
#4721 = AXIS2_PLACEMENT_3D ( 'NONE', #63337, #53387, #36771 ) ;
#4722 = CIRCLE ( 'NONE', #32255, 2.899999999999995914 ) ;
#4723 = CARTESIAN_POINT ( 'NONE',  ( 2.241317068080775243, -4.836852665784620697, 5.906676463196279592 ) ) ;
#4724 = CARTESIAN_POINT ( 'NONE',  ( 35.00000000000000000, -5.300372733891561161, 11.59605747147791632 ) ) ;
#4725 = CARTESIAN_POINT ( 'NONE',  ( -37.00000000000000711, 0.000000000000000000, 0.000000000000000000 ) ) ;
#4726 = DIRECTION ( 'NONE',  ( 0.000000000000000000, 0.01356324068817998940, -0.9999080150203989437 ) ) ;
#4727 = CARTESIAN_POINT ( 'NONE',  ( 0.2739690278137274504, -12.09341522051407836, -1.946552041163031488 ) ) ;
#4728 = CARTESIAN_POINT ( 'NONE',  ( 1.000000000000000888, 0.7281529553922073683, 7.464569195442786409 ) ) ;
#4729 = CARTESIAN_POINT ( 'NONE',  ( 2.260457164927183182, -5.941202713844071504, -4.804526096743075847 ) ) ;
#4730 = DIRECTION ( 'NONE',  ( 1.000000000000000000, 0.000000000000000000, 0.000000000000000000 ) ) ;
#4731 = DIRECTION ( 'NONE',  ( -1.000000000000000000, 0.000000000000000000, 0.000000000000000000 ) ) ;
#4732 = CIRCLE ( 'NONE', #13199, 7.938172270156617749 ) ;
#4733 = CIRCLE ( 'NONE', #25940, 12.18649999999999878 ) ;
#4734 = ADVANCED_FACE ( 'NONE', ( #34566, #44534, #40200, #54863, #60834, #44223, #9286, #49878, #19292, #55181, #4329, #54554, #39560, #24601, #8984, #44879, #4988 ), #59863, .T. ) ;
#4735 = ORIENTED_EDGE ( 'NONE', *, *, #43142, .T. ) ;
#4736 = CARTESIAN_POINT ( 'NONE',  ( 1.719304012339893051, -12.70777170743898310, 0.7661785589588769874 ) ) ;
#4737 = ADVANCED_FACE ( 'NONE', ( #14593 ), #45522, .T. ) ;
#4738 = ORIENTED_EDGE ( 'NONE', *, *, #37842, .F. ) ;
#4739 = CYLINDRICAL_SURFACE ( 'NONE', #14051, 4.999999999999999112 ) ;
#4740 = DIRECTION ( 'NONE',  ( 0.000000000000000000, 0.9987865678893278476, -0.04924826701374234589 ) ) ;
#4741 = CARTESIAN_POINT ( 'NONE',  ( 0.000000000000000000, -6.586971819220299729, -3.586335490831473738 ) ) ;
#4742 = VECTOR ( 'NONE', #46053, 1000.000000000000000 ) ;
#4743 = VERTEX_POINT ( 'NONE', #14923 ) ;
#4744 = EDGE_CURVE ( 'NONE', #58586, #47206, #35216, .T. ) ;
#4745 = ORIENTED_EDGE ( 'NONE', *, *, #49036, .T. ) ;
#4746 = ORIENTED_EDGE ( 'NONE', *, *, #52842, .F. ) ;
#4747 = CARTESIAN_POINT ( 'NONE',  ( -35.00000000000000000, -1.262958560998674429, -12.12087942037211086 ) ) ;
#4748 = CARTESIAN_POINT ( 'NONE',  ( 3.152665057735807075, 3.546019893115007537, -7.102135024646828221 ) ) ;
#4749 = ORIENTED_EDGE ( 'NONE', *, *, #36121, .T. ) ;
#4750 = CARTESIAN_POINT ( 'NONE',  ( 1.719304012341317467, -0.7661785589597189805, -12.70777170743969009 ) ) ;
#4751 = DIRECTION ( 'NONE',  ( 1.000000000000000000, 0.000000000000000000, -0.000000000000000000 ) ) ;
#4752 = CARTESIAN_POINT ( 'NONE',  ( 2.717984159219611673, -2.397195612260686559, 7.415470774236992746 ) ) ;
#4753 = VERTEX_POINT ( 'NONE', #22819 ) ;
#4754 = CARTESIAN_POINT ( 'NONE',  ( -22.28236030719477512, 0.3108070568283993751, 3.683993210674375351 ) ) ;
#4755 = CARTESIAN_POINT ( 'NONE',  ( -2.112161198360044789, -26.60281475960666953, -16.15113466974405654 ) ) ;
#4756 = DIRECTION ( 'NONE',  ( 1.000000000000000000, 0.000000000000000000, -0.000000000000000000 ) ) ;
#4758 = ORIENTED_EDGE ( 'NONE', *, *, #29791, .F. ) ;
#4757 = CARTESIAN_POINT ( 'NONE',  ( 19.56743653832047514, -33.00000000000000000, 5.000000000000001776 ) ) ;
#4759 = DIRECTION ( 'NONE',  ( 0.000000000000000000, -0.01356324068817998940, 0.9999080150203990547 ) ) ;
#4760 = EDGE_CURVE ( 'NONE', #21349, #55219, #36712, .T. ) ;
#4761 = EDGE_CURVE ( 'NONE', #53826, #28860, #59728, .T. ) ;
#4762 = ORIENTED_EDGE ( 'NONE', *, *, #32702, .F. ) ;
#4763 = AXIS2_PLACEMENT_3D ( 'NONE', #46667, #17735, #16425 ) ;
#4764 = CARTESIAN_POINT ( 'NONE',  ( 0.3057689695767505378, -6.328747727191121442, -10.49983108339466398 ) ) ;
#4765 = ORIENTED_EDGE ( 'NONE', *, *, #22860, .F. ) ;
#4766 = DIRECTION ( 'NONE',  ( -1.000000000000000000, 0.000000000000000000, -0.000000000000000000 ) ) ;
#4767 = CARTESIAN_POINT ( 'NONE',  ( 2.000000000000001776, 3.979254915827449945, -5.681598592373734213 ) ) ;
#4768 = ADVANCED_FACE ( 'NONE', ( #30556, #50859 ), #27791, .F. ) ;
#4769 = CARTESIAN_POINT ( 'NONE',  ( 0.3665391374699467075, -8.095513416941292562, 9.237363111276739147 ) ) ;
#4770 = CARTESIAN_POINT ( 'NONE',  ( 0.3675815128205894289, -6.367184624550092487, -10.50067073900658521 ) ) ;
#4771 = CARTESIAN_POINT ( 'NONE',  ( -26.97057981164311968, -10.82588076752199768, 5.177076099659926989 ) ) ;
#4772 = CARTESIAN_POINT ( 'NONE',  ( 0.2739690278137261736, -12.24770428423990687, 0.1830199730326978469 ) ) ;
#4773 = LINE ( 'NONE', #30988, #26606 ) ;
#4774 = CARTESIAN_POINT ( 'NONE',  ( -27.08954555554413446, -0.1819824474943325943, -2.300063521504153830 ) ) ;
#4775 = CYLINDRICAL_SURFACE ( 'NONE', #41738, 8.049672981451799103 ) ;
#4777 = ORIENTED_EDGE ( 'NONE', *, *, #63713, .F. ) ;
#4776 = CARTESIAN_POINT ( 'NONE',  ( 12.90763733317001538, 13.13803547055557175, -3.111388515484440731 ) ) ;
#4778 = VERTEX_POINT ( 'NONE', #35856 ) ;
#4779 = CARTESIAN_POINT ( 'NONE',  ( 13.40087876459804050, -12.56852956566119239, -4.932660016159226224 ) ) ;
#4780 = VERTEX_POINT ( 'NONE', #32437 ) ;
#4781 = ORIENTED_EDGE ( 'NONE', *, *, #60447, .T. ) ;
#4782 = DIRECTION ( 'NONE',  ( 0.000000000000000000, 0.9551603052523468529, -0.2960891610144544828 ) ) ;
#4783 = DIRECTION ( 'NONE',  ( -1.000000000000000000, -0.000000000000000000, 0.000000000000000000 ) ) ;
#4784 = DIRECTION ( 'NONE',  ( -1.000000000000000000, 0.000000000000000000, 0.000000000000000000 ) ) ;
#4785 = CARTESIAN_POINT ( 'NONE',  ( 35.00000000000000000, -1.791059740004336875, 12.05416472667166694 ) ) ;
#4786 = EDGE_CURVE ( 'NONE', #33447, #31123, #51200, .T. ) ;
#4787 = CIRCLE ( 'NONE', #56804, 5.000000000000001776 ) ;
#4788 = CARTESIAN_POINT ( 'NONE',  ( -17.29244623348158783, 2.525873743887551814, 25.00000000000000000 ) ) ;
#4789 = FACE_OUTER_BOUND ( 'NONE', #36677, .T. ) ;
#4790 = ADVANCED_FACE ( 'NONE', ( #326 ), #43690, .F. ) ;
#4791 = ORIENTED_EDGE ( 'NONE', *, *, #65136, .T. ) ;
#4792 = CARTESIAN_POINT ( 'NONE',  ( 2.440552418640494547, -6.024135401262400435, 4.797131306497546710 ) ) ;
#4793 = CARTESIAN_POINT ( 'NONE',  ( 35.00000000000000000, -0.8294751490778421443, 12.15823808070322976 ) ) ;
#4794 = CYLINDRICAL_SURFACE ( 'NONE', #25416, 2.899999999999994582 ) ;
#4795 = ORIENTED_EDGE ( 'NONE', *, *, #24188, .T. ) ;
#4796 = CIRCLE ( 'NONE', #52587, 5.000000000000002665 ) ;
#4797 = CARTESIAN_POINT ( 'NONE',  ( 25.00000000000000355, -3.797884998337192286, 24.99999999999999289 ) ) ;
#4798 = LINE ( 'NONE', #45332, #37363 ) ;
#4799 = CARTESIAN_POINT ( 'NONE',  ( -35.00000000000000000, 1.456211999474342766, 11.65554240571057854 ) ) ;
#4800 = EDGE_LOOP ( 'NONE', ( #40724, #32651, #1782, #54523 ) ) ;
#4801 = CARTESIAN_POINT ( 'NONE',  ( 2.251139882113960766, 6.675617500148649519, -3.710800524304753267 ) ) ;
#4802 = CIRCLE ( 'NONE', #29186, 5.000000000000000000 ) ;
#4803 = LINE ( 'NONE', #26054, #64349 ) ;
#4804 = CARTESIAN_POINT ( 'NONE',  ( 35.00000000000000000, 4.705694406421931860E-17, -3.469127814946512892E-15 ) ) ;
#4805 = FACE_OUTER_BOUND ( 'NONE', #17669, .T. ) ;
#4806 = CARTESIAN_POINT ( 'NONE',  ( 0.3040950598368152291, -10.74226959800787284, -5.912066680610724489 ) ) ;
#4807 = EDGE_CURVE ( 'NONE', #5728, #41912, #37402, .T. ) ;
#4808 = CIRCLE ( 'NONE', #29239, 4.999999999999999112 ) ;
#4809 = ORIENTED_EDGE ( 'NONE', *, *, #29158, .T. ) ;
#4810 = CARTESIAN_POINT ( 'NONE',  ( 0.3218525148189859131, -12.11874253990390038, 1.888670068297610971 ) ) ;
#4811 = CARTESIAN_POINT ( 'NONE',  ( 1.937114397841935398, 5.620553190833136092, -11.53912442307249542 ) ) ;
#4812 = ORIENTED_EDGE ( 'NONE', *, *, #41396, .F. ) ;
#4813 = CARTESIAN_POINT ( 'NONE',  ( 21.48709468929590827, 12.93615662171536584, -3.881105879424552985 ) ) ;
#4814 = CARTESIAN_POINT ( 'NONE',  ( 2.241352910868908310, 6.652881166698511706, 3.744764251557016532 ) ) ;
#4815 = ORIENTED_EDGE ( 'NONE', *, *, #46436, .T. ) ;
#4816 = VERTEX_POINT ( 'NONE', #1803 ) ;
#4817 = ORIENTED_EDGE ( 'NONE', *, *, #49370, .T. ) ;
#4818 = AXIS2_PLACEMENT_3D ( 'NONE', #18735, #59609, #38327 ) ;
#4819 = ADVANCED_FACE ( 'NONE', ( #32035 ), #47360, .T. ) ;
#4820 = ORIENTED_EDGE ( 'NONE', *, *, #4761, .F. ) ;
#4821 = CARTESIAN_POINT ( 'NONE',  ( 37.00000000000000711, -7.215058775251181444, 9.821084925794645315 ) ) ;
#4822 = FACE_OUTER_BOUND ( 'NONE', #40884, .T. ) ;
#4823 = CARTESIAN_POINT ( 'NONE',  ( -37.00000000000000711, -2.865935305911713638, 12.42372387097881514 ) ) ;
#4824 = CARTESIAN_POINT ( 'NONE',  ( -35.00000000000000000, 1.456211999474342766, 11.65554240571057854 ) ) ;
#4825 = CARTESIAN_POINT ( 'NONE',  ( -12.31125281582930064, -29.30934768819192371, 5.548768499314465252 ) ) ;
#4826 = DIRECTION ( 'NONE',  ( 0.000000000000000000, 0.000000000000000000, -1.000000000000000000 ) ) ;
#4828 = ORIENTED_EDGE ( 'NONE', *, *, #18900, .T. ) ;
#4827 = CARTESIAN_POINT ( 'NONE',  ( 0.000000000000000000, 1.956810415765277922, -6.654767106875532967 ) ) ;
#4829 = CARTESIAN_POINT ( 'NONE',  ( 12.52750123246316072, 0.4973700281276248192, 25.00000000000000000 ) ) ;
#4830 = EDGE_CURVE ( 'NONE', #12988, #46103, #24206, .T. ) ;
#4831 = ORIENTED_EDGE ( 'NONE', *, *, #65276, .F. ) ;
#4832 = LINE ( 'NONE', #25098, #11495 ) ;
#4833 = ORIENTED_EDGE ( 'NONE', *, *, #48499, .T. ) ;
#4834 = ORIENTED_EDGE ( 'NONE', *, *, #18181, .T. ) ;
#4835 = DIRECTION ( 'NONE',  ( 0.000000000000000000, -0.8515178078024923103, 0.5243256840888473880 ) ) ;
#4836 = CARTESIAN_POINT ( 'NONE',  ( 4.532733354134460768, -28.39821948934986651, 13.34103783736875215 ) ) ;
#4837 = EDGE_CURVE ( 'NONE', #9689, #50060, #25745, .T. ) ;
#4838 = CARTESIAN_POINT ( 'NONE',  ( -10.48620311856347875, -9.720786832536937538, 25.00000000000000000 ) ) ;
#4839 = AXIS2_PLACEMENT_3D ( 'NONE', #60211, #15628, #50584 ) ;
#4840 = CARTESIAN_POINT ( 'NONE',  ( -37.00000000000000711, -10.84030624090602046, -6.711949091238257559 ) ) ;
#4841 = CARTESIAN_POINT ( 'NONE',  ( -19.31276997470573775, 11.98635249372530254, -0.6547996305031958952 ) ) ;
#4842 = CARTESIAN_POINT ( 'NONE',  ( 2.241317068080790342, 5.906676463195350557, 4.836852665785724703 ) ) ;
#4843 = ORIENTED_EDGE ( 'NONE', *, *, #56908, .F. ) ;
#4844 = ORIENTED_EDGE ( 'NONE', *, *, #28406, .T. ) ;
#4845 = CARTESIAN_POINT ( 'NONE',  ( -37.00000000000000711, -1.456211999474261054, -11.65554240571058742 ) ) ;
#4846 = VERTEX_POINT ( 'NONE', #1141 ) ;
#4847 = VERTEX_POINT ( 'NONE', #21765 ) ;
#4848 = CARTESIAN_POINT ( 'NONE',  ( 35.00000000000000000, 4.705694406421931860E-17, -3.469127814946512892E-15 ) ) ;
#4849 = CARTESIAN_POINT ( 'NONE',  ( 0.3474126878361829540, 10.49748369253940972, -6.359473273659596693 ) ) ;
#4850 = DIRECTION ( 'NONE',  ( 0.000000000000000000, -0.1081190184239489566, 0.9941379571543588201 ) ) ;
#4851 = CARTESIAN_POINT ( 'NONE',  ( -37.00000000000000711, 11.72397916322013600, -0.7214809346827312231 ) ) ;
#4852 = DIRECTION ( 'NONE',  ( 0.000000000000000000, -0.01356324068818000848, 0.9999080150203990547 ) ) ;
#4853 = EDGE_CURVE ( 'NONE', #36886, #17119, #18361, .T. ) ;
#4854 = CARTESIAN_POINT ( 'NONE',  ( -10.70196691523763732, -4.522197807754633203, -11.12215661015785884 ) ) ;
#4855 = CARTESIAN_POINT ( 'NONE',  ( -37.00000000000000711, 0.7214809346828596759, 11.72397916322012712 ) ) ;
#4856 = ORIENTED_EDGE ( 'NONE', *, *, #16070, .F. ) ;
#4857 = ORIENTED_EDGE ( 'NONE', *, *, #16047, .T. ) ;
#4858 = DIRECTION ( 'NONE',  ( 0.000000000000000000, -0.01356324068817999114, 0.9999080150203989437 ) ) ;
#4859 = CARTESIAN_POINT ( 'NONE',  ( 2.242418902651939216, 7.500817491983897689, -1.423836467585266385 ) ) ;
#4860 = DIRECTION ( 'NONE',  ( 0.000000000000000000, 0.000000000000000000, 1.000000000000000000 ) ) ;
#4861 = AXIS2_PLACEMENT_3D ( 'NONE', #50051, #14448, #49088 ) ;
#4862 = ADVANCED_FACE ( 'NONE', ( #62613 ), #57326, .T. ) ;
#4863 = DIRECTION ( 'NONE',  ( 0.000000000000000000, 0.2960891610144510966, 0.9551603052523478521 ) ) ;
#4864 = CARTESIAN_POINT ( 'NONE',  ( -22.51237073810381162, -4.218051923713588280, 1.333315726166073967 ) ) ;
#4865 =( BOUNDED_SURFACE ( )  B_SPLINE_SURFACE ( 3, 1, ( 
 ( #30447, #61050 ),
 ( #50745, #25462 ),
 ( #15480, #208 ),
 ( #51424, #11163 ) ),
 .UNSPECIFIED., .F., .F., .F. ) 
 B_SPLINE_SURFACE_WITH_KNOTS ( ( 4, 4 ),
 ( 2, 2 ),
 ( 0.000000000000000000, 1.000000000000000000 ),
 ( 0.000000000000000000, 1.000000000000000000 ),
 .UNSPECIFIED. ) 
 GEOMETRIC_REPRESENTATION_ITEM ( )  RATIONAL_B_SPLINE_SURFACE ( (
 ( 1.000000000000000000, 1.000000000000000000),
 ( 0.9856612449720755231, 0.9999558406602322425),
 ( 0.9856612449720755231, 0.9999558406602322425),
 ( 1.000000000000000000, 1.000000000000000000) ) ) 
 REPRESENTATION_ITEM ( '' )  SURFACE ( )  );
#4866 = DIRECTION ( 'NONE',  ( 1.000000000000000000, 0.000000000000000000, -0.000000000000000000 ) ) ;
#4867 = CARTESIAN_POINT ( 'NONE',  ( -36.00000000000000711, -12.74921544981111055, 0.1414404973751696992 ) ) ;
#4868 = CARTESIAN_POINT ( 'NONE',  ( -27.08426571771018487, -2.098821047392069428, -0.9198084705429488972 ) ) ;
#4869 = ORIENTED_EDGE ( 'NONE', *, *, #14006, .T. ) ;
#4870 = CARTESIAN_POINT ( 'NONE',  ( 2.705197763288548440, -0.2797837188786904128, 7.783989928191465957 ) ) ;
#4871 = DIRECTION ( 'NONE',  ( 1.000000000000000000, 0.000000000000000000, 0.000000000000000000 ) ) ;
#4872 = CARTESIAN_POINT ( 'NONE',  ( 13.23110845410259451, -34.10188054478469155, 9.409930202772073926 ) ) ;
#4873 = AXIS2_PLACEMENT_3D ( 'NONE', #15864, #6582, #56811 ) ;
#4874 = CARTESIAN_POINT ( 'NONE',  ( 3.047904605210419948, -6.622084192655463220, -4.313929735713934122 ) ) ;
#4875 = CARTESIAN_POINT ( 'NONE',  ( 2.907497136250919656, -7.252103438786975609, 3.021847490615727327 ) ) ;
#4876 = EDGE_CURVE ( 'NONE', #20288, #27619, #52984, .T. ) ;
#4877 = ORIENTED_EDGE ( 'NONE', *, *, #46840, .F. ) ;
#4878 = CARTESIAN_POINT ( 'NONE',  ( 36.00000000000000711, -3.033604067594489528, 12.38385022362084698 ) ) ;
#4879 = CARTESIAN_POINT ( 'NONE',  ( 5.530133899448235191, -0.001124651387254880456, -0.01594518557925637958 ) ) ;
#4880 = CARTESIAN_POINT ( 'NONE',  ( 14.81496943876074290, -34.66917994667981162, -7.369609160621835464 ) ) ;
#4881 = ORIENTED_EDGE ( 'NONE', *, *, #44741, .F. ) ;
#4882 = EDGE_CURVE ( 'NONE', #36323, #56883, #55504, .T. ) ;
#4883 = CARTESIAN_POINT ( 'NONE',  ( 0.000000000000000000, 5.888698556700818543, -3.665823448873358981 ) ) ;
#4884 = DIRECTION ( 'NONE',  ( 0.000000000000000000, 0.8276889981568879007, 0.5611870653623863836 ) ) ;
#4885 = CARTESIAN_POINT ( 'NONE',  ( 5.514970785353741078, 0.003929719953530069060, 0.002619824551223233922 ) ) ;
#4887 = ORIENTED_EDGE ( 'NONE', *, *, #36857, .T. ) ;
#4886 = DIRECTION ( 'NONE',  ( -1.000000000000000000, 0.000000000000000000, 0.000000000000000000 ) ) ;
#4888 = CYLINDRICAL_SURFACE ( 'NONE', #61784, 4.999999999999999112 ) ;
#4889 = B_SPLINE_CURVE_WITH_KNOTS ( 'NONE', 3,
 ( #27521, #47185, #12891, #22557, #58131, #12237, #21903 ),
 .UNSPECIFIED., .F., .F.,
 ( 4, 3, 4 ),
 ( 8.338150981373126328E-05, 9.911389841680512771E-05, 0.0001667630577588621215 ),
 .UNSPECIFIED. ) ;
#4890 = EDGE_CURVE ( 'NONE', #20337, #30460, #16750, .T. ) ;
#4891 = AXIS2_PLACEMENT_3D ( 'NONE', #24051, #23735, #33368 ) ;
#4892 = DIRECTION ( 'NONE',  ( 0.000000000000000000, -0.5987040770935562195, 0.8009703041134254020 ) ) ;
#4893 = VERTEX_POINT ( 'NONE', #17421 ) ;
#4894 = CARTESIAN_POINT ( 'NONE',  ( -47.00000000000000711, 0.000000000000000000, 0.000000000000000000 ) ) ;
#4895 = CARTESIAN_POINT ( 'NONE',  ( -27.08954555554373300, 1.307633183325747739, 1.900922216191343717 ) ) ;
#4897 = CIRCLE ( 'NONE', #35670, 2.899999999999995914 ) ;
#4896 = CARTESIAN_POINT ( 'NONE',  ( 0.3610902822527236600, -9.572034936626840462, -7.689482111308950429 ) ) ;
#4898 = DIRECTION ( 'NONE',  ( 1.000000000000000000, 0.000000000000000000, 0.000000000000000000 ) ) ;
#4899 = CARTESIAN_POINT ( 'NONE',  ( -35.00000000000000000, 9.493370459201697642, 6.917234959366862057 ) ) ;
#4900 = CARTESIAN_POINT ( 'NONE',  ( -18.58686583997218378, 5.151216734910788908, 12.47858029384653555 ) ) ;
#4901 = CARTESIAN_POINT ( 'NONE',  ( 27.62838931380291996, 25.00000000000000000, -3.066727421130092779 ) ) ;
#4902 = EDGE_CURVE ( 'NONE', #29799, #21899, #44711, .T. ) ;
#4903 = ORIENTED_EDGE ( 'NONE', *, *, #47319, .F. ) ;
#4904 = FACE_OUTER_BOUND ( 'NONE', #63253, .T. ) ;
#4905 = ORIENTED_EDGE ( 'NONE', *, *, #52253, .F. ) ;
#4906 = B_SPLINE_CURVE_WITH_KNOTS ( 'NONE', 3,
 ( #10234, #40837, #55470, #55136, #30511, #44832, #4942, #5262, #25203, #14552, #282, #61113, #29857, #30200, #15548, #4627 ),
 .UNSPECIFIED., .F., .F.,
 ( 4, 2, 2, 2, 2, 2, 2, 4 ),
 ( 0.000000000000000000, 0.002440323270129363641, 0.003660484905194043726, 0.004880646540258723812, 0.006100808175323402596, 0.007320969810388081381, 0.008541131445452760165, 0.009761293080517437215 ),
 .UNSPECIFIED. ) ;
#4907 = VECTOR ( 'NONE', #23737, 1000.000000000000000 ) ;
#4908 = CARTESIAN_POINT ( 'NONE',  ( 0.3218525148189780305, 11.43947393562877046, 4.423735011438867382 ) ) ;
#4909 = EDGE_CURVE ( 'NONE', #52455, #23780, #36220, .T. ) ;
#4910 = CYLINDRICAL_SURFACE ( 'NONE', #62744, 7.011478057721953761 ) ;
#4911 = VERTEX_POINT ( 'NONE', #37698 ) ;
#4912 = FACE_OUTER_BOUND ( 'NONE', #11363, .T. ) ;
#4913 = DIRECTION ( 'NONE',  ( 0.000000000000000000, -0.01356324068818000848, 0.9999080150203990547 ) ) ;
#4914 = LINE ( 'NONE', #45448, #25503 ) ;
#4915 = VERTEX_POINT ( 'NONE', #27705 ) ;
#4916 = VERTEX_POINT ( 'NONE', #7418 ) ;
#4917 = CARTESIAN_POINT ( 'NONE',  ( -14.47334165536100059, 0.000000000000000000, 0.000000000000000000 ) ) ;
#4918 = ORIENTED_EDGE ( 'NONE', *, *, #10334, .T. ) ;
#4919 = DIRECTION ( 'NONE',  ( -1.000000000000000000, 0.000000000000000000, 0.000000000000000000 ) ) ;
#4920 = CARTESIAN_POINT ( 'NONE',  ( -27.08588607604433562, 0.5840042213197134124, -2.220764381377025476 ) ) ;
#4921 = DIRECTION ( 'NONE',  ( 1.000000000000000000, -0.000000000000000000, -0.000000000000000000 ) ) ;
#4922 = CARTESIAN_POINT ( 'NONE',  ( 2.242418902651940993, 7.139616612143419694, -2.704708480794735248 ) ) ;
#4923 = CARTESIAN_POINT ( 'NONE',  ( 3.100650473569748211, -4.345221797103555161, 6.622643684997368219 ) ) ;
#4924 = DIRECTION ( 'NONE',  ( -1.000000000000000000, 0.000000000000000000, 0.000000000000000000 ) ) ;
#4925 = CARTESIAN_POINT ( 'NONE',  ( 0.3474126878361755710, 11.61929161290146162, 3.953748424960682240 ) ) ;
#4926 = ORIENTED_EDGE ( 'NONE', *, *, #2714, .T. ) ;
#4927 = CARTESIAN_POINT ( 'NONE',  ( 2.297017764050091948, 7.651182381906872720, -0.1647869190092008940 ) ) ;
#4928 = CARTESIAN_POINT ( 'NONE',  ( -35.00000000000000000, 10.70999494708501132, -5.814360711498173018 ) ) ;
#4929 = CARTESIAN_POINT ( 'NONE',  ( 2.241449424704146320, 5.887589908049645437, 4.860179885671820799 ) ) ;
#4930 = DIRECTION ( 'NONE',  ( 0.000000000000000000, -0.8276889981568955612, 0.5611870653623749483 ) ) ;
#4931 = CARTESIAN_POINT ( 'NONE',  ( -2.532614230583026593, 7.965877694534055031, 10.89930238848911337 ) ) ;
#4932 = DIRECTION ( 'NONE',  ( -1.000000000000000000, 0.000000000000000000, 0.000000000000000000 ) ) ;
#4933 = CYLINDRICAL_SURFACE ( 'NONE', #3719, 5.000000000000000888 ) ;
#4934 = B_SPLINE_CURVE_WITH_KNOTS ( 'NONE', 3,
 ( #13330, #48593, #43572, #63855, #33616, #990, #61824, #30263, #16279, #60852, #19950, #26257, #15292, #35570, #50235, #50560, #15927, #36211, #41203, #14941, #35233, #50877, #4694, #40559, #9629, #55197, #29927, #55536, #9984, #5322, #5004, #55864, #56177, #24955, #10295, #15609, #30572, #10613, #65805, #25597, #45228, #45891, #61488, #20279, #25262, #30899 ),
 .UNSPECIFIED., .F., .F.,
 ( 4, 2, 2, 2, 2, 2, 2, 2, 2, 2, 2, 2, 2, 2, 2, 2, 2, 2, 2, 2, 2, 2, 4 ),
 ( 0.000000000000000000, 0.002978983955370559291, 0.004468475933055836118, 0.005957967910741112511, 0.007447459888426388036, 0.008936951866111665296, 0.01191593582148221461, 0.01489491977685276219, 0.01787390373222331325, 0.02085288768759386083, 0.02234237966527913288, 0.02383187164296440841, 0.02681085559833495946, 0.02830034757602023499, 0.02978983955370551051, 0.03276882350907605462, 0.03574780746444660567, 0.03872679141981715673, 0.04170577537518770778, 0.04319526735287298330, 0.04468475933055825883, 0.04617425130824354129, 0.04766374328592882376 ),
 .UNSPECIFIED. ) ;
#4935 = DIRECTION ( 'NONE',  ( 1.000000000000000000, 0.000000000000000000, 0.000000000000000000 ) ) ;
#4936 = ADVANCED_FACE ( 'NONE', ( #21421 ), #809, .T. ) ;
#4937 = ORIENTED_EDGE ( 'NONE', *, *, #35605, .T. ) ;
#4938 = CARTESIAN_POINT ( 'NONE',  ( 5.520433897694421610, 0.009283255140285181714, 0.01186170453199828639 ) ) ;
#4939 = AXIS2_PLACEMENT_3D ( 'NONE', #9435, #64976, #143 ) ;
#4940 = AXIS2_PLACEMENT_3D ( 'NONE', #29965, #50918, #5363 ) ;
#4941 = VERTEX_POINT ( 'NONE', #52677 ) ;
#4942 = CARTESIAN_POINT ( 'NONE',  ( -3.484441229472478252, -8.595929743150758640, 8.383143565561299582 ) ) ;
#4943 = CARTESIAN_POINT ( 'NONE',  ( 2.245754705088395475, -7.499730934370265167, -1.435454129948283031 ) ) ;
#4944 = CARTESIAN_POINT ( 'NONE',  ( -17.69233425103264423, 6.603005964784629533, -11.77702021843230007 ) ) ;
#4945 = CARTESIAN_POINT ( 'NONE',  ( -37.00000000000000711, 1.030638227056741574, -12.14284015767849034 ) ) ;
#4946 = DIRECTION ( 'NONE',  ( -1.000000000000000000, 0.000000000000000000, 0.000000000000000000 ) ) ;
#4947 = ORIENTED_EDGE ( 'NONE', *, *, #32895, .T. ) ;
#4948 = CARTESIAN_POINT ( 'NONE',  ( 35.00000000000000000, 8.766823244861988940, -7.817610399097547180 ) ) ;
#4949 = CARTESIAN_POINT ( 'NONE',  ( 2.844750968615495257, 2.364925124214210861, -7.470159816919067275 ) ) ;
#4950 = CARTESIAN_POINT ( 'NONE',  ( -27.09150307427401927, 2.085162835056709518, 1.001311209615645570 ) ) ;
#4951 = CARTESIAN_POINT ( 'NONE',  ( -25.86628395826706850, -8.041618865309574815, 10.84354029019568522 ) ) ;
#4952 = EDGE_CURVE ( 'NONE', #34891, #20989, #56692, .T. ) ;
#4953 = CARTESIAN_POINT ( 'NONE',  ( 1.452237505248552996, 4.880303821311168022, -11.67686475128074797 ) ) ;
#4954 = LINE ( 'NONE', #56821, #25524 ) ;
#4955 = VERTEX_POINT ( 'NONE', #46686 ) ;
#4956 = EDGE_CURVE ( 'NONE', #38662, #27609, #30907, .T. ) ;
#4957 = CARTESIAN_POINT ( 'NONE',  ( -27.08639648637162267, -0.5801562253464774832, 2.223359598375754587 ) ) ;
#4958 = ORIENTED_EDGE ( 'NONE', *, *, #26947, .T. ) ;
#4959 = EDGE_CURVE ( 'NONE', #35685, #7749, #51099, .T. ) ;
#4960 = CARTESIAN_POINT ( 'NONE',  ( 35.00000000000000000, -4.603882218679472338, 10.80631716521671493 ) ) ;
#4961 = CARTESIAN_POINT ( 'NONE',  ( 35.00000000000000000, -11.73808581813437613, 0.4353888892049613824 ) ) ;
#4962 = B_SPLINE_CURVE_WITH_KNOTS ( 'NONE', 3,
 ( #42175, #12262, #46866, #62462, #37194, #37541, #21604, #37866, #2307, #58157, #32854, #53162, #7608, #57847, #26573, #2654, #22915, #17914, #38176, #62157, #16929, #8580 ),
 .UNSPECIFIED., .F., .F.,
 ( 4, 3, 3, 3, 3, 3, 3, 4 ),
 ( 0.000000000000000000, 6.990956068646398400E-05, 0.0001398191187764043859, 0.0002097286751720219781, 0.0002796382307041368601, 0.0003495477861619817792, 0.0004194573423310291168, 0.0005586102576333201340 ),
 .UNSPECIFIED. ) ;
#4963 = DIRECTION ( 'NONE',  ( 0.000000000000000000, 0.000000000000000000, 1.000000000000000000 ) ) ;
#4964 = CARTESIAN_POINT ( 'NONE',  ( 6.361445718264521432, -4.355102044641763648, 12.77822703589027320 ) ) ;
#4965 = EDGE_LOOP ( 'NONE', ( #18528, #35963, #37243, #8002 ) ) ;
#4967 = ORIENTED_EDGE ( 'NONE', *, *, #10550, .T. ) ;
#4966 = ADVANCED_FACE ( 'NONE', ( #2466 ), #49006, .T. ) ;
#4968 = CARTESIAN_POINT ( 'NONE',  ( -27.09833916700227618, 2.238843247505183598, -0.6583442518269285726 ) ) ;
#4969 = ORIENTED_EDGE ( 'NONE', *, *, #46621, .T. ) ;
#4970 = CARTESIAN_POINT ( 'NONE',  ( 2.245754705088392811, -6.556487589645213276, -3.913944702466338299 ) ) ;
#4971 = FACE_OUTER_BOUND ( 'NONE', #32078, .T. ) ;
#4972 = CARTESIAN_POINT ( 'NONE',  ( 5.536195898058073439, -0.001224473329857922455, 0.008411485181669254088 ) ) ;
#4973 = CARTESIAN_POINT ( 'NONE',  ( -37.00000000000000711, -7.971186206369537786, 9.217970097227697224 ) ) ;
#4974 = DIRECTION ( 'NONE',  ( 1.000000000000000000, 0.000000000000000000, -0.000000000000000000 ) ) ;
#4975 = EDGE_CURVE ( 'NONE', #15890, #7338, #59586, .T. ) ;
#4976 = CARTESIAN_POINT ( 'NONE',  ( 37.00000000000000711, 6.917234959366825642, -9.493370459201726064 ) ) ;
#4977 = CARTESIAN_POINT ( 'NONE',  ( 1.634816307076184971, -12.68239325670201900, -0.7191532042400472502 ) ) ;
#4978 = ORIENTED_EDGE ( 'NONE', *, *, #54572, .T. ) ;
#4979 = CARTESIAN_POINT ( 'NONE',  ( 2.507146904658101416, -2.437115546363171958, -7.328382489803296984 ) ) ;
#4980 = ORIENTED_EDGE ( 'NONE', *, *, #3434, .T. ) ;
#4981 = AXIS2_PLACEMENT_3D ( 'NONE', #37938, #17677, #26992 ) ;
#4982 = CYLINDRICAL_SURFACE ( 'NONE', #45772, 5.000000000000000888 ) ;
#4983 = EDGE_CURVE ( 'NONE', #42237, #25922, #17018, .T. ) ;
#4984 = CARTESIAN_POINT ( 'NONE',  ( 37.00000000000000711, 11.01837265713073144, -6.415447294506746445 ) ) ;
#4985 = ORIENTED_EDGE ( 'NONE', *, *, #1807, .T. ) ;
#4986 = VECTOR ( 'NONE', #9054, 1000.000000000000000 ) ;
#4987 = ADVANCED_FACE ( 'NONE', ( #17750 ), #33684, .T. ) ;
#4988 = FACE_BOUND ( 'NONE', #41732, .T. ) ;
#4989 = ORIENTED_EDGE ( 'NONE', *, *, #27853, .T. ) ;
#4990 = DIRECTION ( 'NONE',  ( -0.9748757316300199482, 0.000000000000000000, 0.2227494284590502138 ) ) ;
#4991 = DIRECTION ( 'NONE',  ( 1.000000000000000000, 0.000000000000000000, 0.000000000000000000 ) ) ;
#4992 = CARTESIAN_POINT ( 'NONE',  ( 16.78263030916553333, 10.48479066935627202, 5.836879698929882565 ) ) ;
#4993 = CARTESIAN_POINT ( 'NONE',  ( 4.833640382554417414, -10.56051903602595132, 5.701708524974907988 ) ) ;
#4994 = VERTEX_POINT ( 'NONE', #58659 ) ;
#4996 = ADVANCED_FACE ( 'NONE', ( #53329 ), #48668, .T. ) ;
#4995 = ORIENTED_EDGE ( 'NONE', *, *, #22585, .F. ) ;
#4997 = CARTESIAN_POINT ( 'NONE',  ( -35.00000000000000000, 11.23004253107764505, 4.732539170486304236 ) ) ;
#4998 = ORIENTED_EDGE ( 'NONE', *, *, #11770, .F. ) ;
#4999 = CARTESIAN_POINT ( 'NONE',  ( 2.897545437445938920E-15, -45.00000000000000000, 23.66025403784440684 ) ) ;
#5000 = VERTEX_POINT ( 'NONE', #23732 ) ;
#5001 = ORIENTED_EDGE ( 'NONE', *, *, #36863, .T. ) ;
#5002 = VERTEX_POINT ( 'NONE', #3122 ) ;
#5003 = CARTESIAN_POINT ( 'NONE',  ( 2.524535260911856316, -5.776056274541021551, 5.135322114975514829 ) ) ;
#5004 = CARTESIAN_POINT ( 'NONE',  ( 7.856790134851106444, -26.39165916151114288, 14.61432118582567874 ) ) ;
#5005 = CARTESIAN_POINT ( 'NONE',  ( 2.931247277082685621, -0.9994150891045774365, -7.800615791174665858 ) ) ;
#5006 = CARTESIAN_POINT ( 'NONE',  ( 35.00000000000000000, 9.908974237959730758, 6.307491713048920090 ) ) ;
#5007 = DIRECTION ( 'NONE',  ( 0.000000000000000000, 0.9985334138511237079, 0.05413890858542116241 ) ) ;
#5008 = ORIENTED_EDGE ( 'NONE', *, *, #53074, .T. ) ;
#5009 = CARTESIAN_POINT ( 'NONE',  ( 2.268878695252931621, -2.474564429974762891, -7.231932316092929192 ) ) ;
#5010 = VERTEX_POINT ( 'NONE', #28692 ) ;
#5011 = CARTESIAN_POINT ( 'NONE',  ( 35.00000000000000000, 2.220215194442072271, 11.98254675519225287 ) ) ;
#5012 = CARTESIAN_POINT ( 'NONE',  ( 2.000000000000001776, -6.662861565602053560, -1.421313227905724341 ) ) ;
#5013 = ORIENTED_EDGE ( 'NONE', *, *, #45355, .F. ) ;
#5014 = CARTESIAN_POINT ( 'NONE',  ( 1.719304012341584365, 10.22720798541559439, -7.581471372738991299 ) ) ;
#5015 = CARTESIAN_POINT ( 'NONE',  ( 2.259025283528079076, -6.683966451873007308, -3.701170455111045587 ) ) ;
#5016 = ADVANCED_FACE ( 'NONE', ( #28057 ), #44000, .T. ) ;
#5017 = ADVANCED_FACE ( 'NONE', ( #23386 ), #45838, .F. ) ;
#5018 = ORIENTED_EDGE ( 'NONE', *, *, #31461, .F. ) ;
#5019 = CARTESIAN_POINT ( 'NONE',  ( 2.257661810676421688, -7.638648121130933610, 0.1348365785570732611 ) ) ;
#5020 = AXIS2_PLACEMENT_3D ( 'NONE', #4443, #9729, #24714 ) ;
#5021 = ORIENTED_EDGE ( 'NONE', *, *, #53336, .F. ) ;
#5022 = CARTESIAN_POINT ( 'NONE',  ( 0.2801149460245124789, 10.70654700624303324, 5.954809120985752102 ) ) ;
#5023 = DIRECTION ( 'NONE',  ( -1.000000000000000000, 0.000000000000000000, 0.000000000000000000 ) ) ;
#5024 = CARTESIAN_POINT ( 'NONE',  ( -10.77421046970567353, -27.84620353580639573, 14.04190754122876506 ) ) ;
#5025 = CARTESIAN_POINT ( 'NONE',  ( 2.276198483116797622, -3.688810392808719030, -6.697332984100004438 ) ) ;
#5026 = DIRECTION ( 'NONE',  ( 0.000000000000000000, -0.01356324068817998940, 0.9999080150203990547 ) ) ;
#5027 = EDGE_LOOP ( 'NONE', ( #48748, #32294, #20041, #549 ) ) ;
#5028 = EDGE_CURVE ( 'NONE', #6695, #16592, #21319, .T. ) ;
#5029 = CARTESIAN_POINT ( 'NONE',  ( 37.00000000000000711, -11.65150730582935523, -1.488153103996925797 ) ) ;
#5030 = LINE ( 'NONE', #60538, #41798 ) ;
#5031 = DIRECTION ( 'NONE',  ( 0.000000000000000000, 0.01356324068817998940, -0.9999080150203990547 ) ) ;
#5032 = VECTOR ( 'NONE', #57919, 1000.000000000000000 ) ;
#5033 = DIRECTION ( 'NONE',  ( -1.000000000000000000, 0.000000000000000000, 0.000000000000000000 ) ) ;
#5034 = EDGE_CURVE ( 'NONE', #25959, #40797, #64836, .T. ) ;
#5035 = AXIS2_PLACEMENT_3D ( 'NONE', #64812, #29264, #55765 ) ;
#5036 = CARTESIAN_POINT ( 'NONE',  ( 0.2647959493198560055, -12.08462848595693373, -1.981611532097670381 ) ) ;
#5037 = DIRECTION ( 'NONE',  ( 1.000000000000000000, -0.000000000000000000, -0.000000000000000000 ) ) ;
#5038 = ADVANCED_FACE ( 'NONE', ( #35306 ), #50630, .T. ) ;
#5039 = DIRECTION ( 'NONE',  ( -1.000000000000000000, -0.000000000000000000, 0.000000000000000000 ) ) ;
#5040 = CARTESIAN_POINT ( 'NONE',  ( 2.268878695253351285, 0.1481365927654600123, -7.642144312464377087 ) ) ;
#5041 = ORIENTED_EDGE ( 'NONE', *, *, #26778, .T. ) ;
#5042 =( BOUNDED_CURVE ( )  B_SPLINE_CURVE ( 3, ( #27197, #62758, #58123, #47489 ),
 .UNSPECIFIED., .F., .F. ) 
 B_SPLINE_CURVE_WITH_KNOTS ( ( 4, 4 ),
 ( 2.475131039105764152, 2.535910263743374582 ),
 .UNSPECIFIED. ) 
 CURVE ( )  GEOMETRIC_REPRESENTATION_ITEM ( )  RATIONAL_B_SPLINE_CURVE ( ( 1.000000000000000000, 0.9996921808454459768, 0.9996921808454459768, 1.000000000000000000 ) ) 
 REPRESENTATION_ITEM ( '' )  );
#5043 = ORIENTED_EDGE ( 'NONE', *, *, #9364, .T. ) ;
#5044 = CARTESIAN_POINT ( 'NONE',  ( -18.25006854224444908, -9.443202773001939221, -7.404452808139720510 ) ) ;
#5045 = CARTESIAN_POINT ( 'NONE',  ( -35.04709527796842394, -0.001003525937983557048, 0.01232256164995608472 ) ) ;
#5046 = DIRECTION ( 'NONE',  ( -1.000000000000000000, -0.000000000000000000, 0.000000000000000000 ) ) ;
#5047 = EDGE_CURVE ( 'NONE', #36605, #9429, #15024, .T. ) ;
#5048 = CARTESIAN_POINT ( 'NONE',  ( 5.514970785353741078, -0.002619824551223732222, -0.003929719953530097683 ) ) ;
#5049 = ORIENTED_EDGE ( 'NONE', *, *, #10407, .T. ) ;
#5050 = EDGE_CURVE ( 'NONE', #39295, #27713, #24496, .T. ) ;
#5051 = VERTEX_POINT ( 'NONE', #25671 ) ;
#5052 = ORIENTED_EDGE ( 'NONE', *, *, #31788, .T. ) ;
#5053 = CARTESIAN_POINT ( 'NONE',  ( 28.56560408307198884, -10.68382391369774709, 5.468123827008506410 ) ) ;
#5054 = EDGE_CURVE ( 'NONE', #11425, #20378, #45615, .T. ) ;
#5055 = B_SPLINE_CURVE_WITH_KNOTS ( 'NONE', 3,
 ( #60558, #394, #34310, #30617, #9045, #50929, #44594, #34625, #20669, #24669 ),
 .UNSPECIFIED., .F., .F.,
 ( 4, 3, 3, 4 ),
 ( 1.226634733346699349E-18, 6.607638129004437383E-05, 9.911389841680539876E-05, 0.0001667630577588623112 ),
 .UNSPECIFIED. ) ;
#5056 = AXIS2_PLACEMENT_3D ( 'NONE', #45296, #65553, #31317 ) ;
#5057 = DIRECTION ( 'NONE',  ( -1.000000000000000000, 0.000000000000000000, -0.000000000000000000 ) ) ;
#5058 = ORIENTED_EDGE ( 'NONE', *, *, #57463, .F. ) ;
#5059 = ADVANCED_FACE ( 'NONE', ( #45299 ), #57297, .F. ) ;
#5060 = DIRECTION ( 'NONE',  ( -1.000000000000000000, 0.000000000000000000, 0.000000000000000000 ) ) ;
#5061 = CARTESIAN_POINT ( 'NONE',  ( -37.00000000000000711, 2.080187960898737476, -12.57916205664479214 ) ) ;
#5062 = CARTESIAN_POINT ( 'NONE',  ( 2.969415267404556413, -2.326350273511729849, 7.525730903320692278 ) ) ;
#5064 = VERTEX_POINT ( 'NONE', #14683 ) ;
#5063 = AXIS2_PLACEMENT_3D ( 'NONE', #6652, #46235, #61833 ) ;
#5065 = DIRECTION ( 'NONE',  ( 0.000000000000000000, 0.01356324068817992175, -0.9999080150203990547 ) ) ;
#5066 = CARTESIAN_POINT ( 'NONE',  ( 5.786001662379491428, -26.94056086434354924, -15.63186719136363756 ) ) ;
#5067 = CARTESIAN_POINT ( 'NONE',  ( 35.00000000000000000, -10.63508530065518443, 4.986700593229810963 ) ) ;
#5068 = ORIENTED_EDGE ( 'NONE', *, *, #14772, .T. ) ;
#5069 = EDGE_CURVE ( 'NONE', #26347, #4941, #25026, .T. ) ;
#5070 = CARTESIAN_POINT ( 'NONE',  ( -25.86628395826706850, 8.041618865309581921, 10.84354029019568522 ) ) ;
#5071 = ORIENTED_EDGE ( 'NONE', *, *, #11926, .F. ) ;
#5072 = CARTESIAN_POINT ( 'NONE',  ( 1.549075743845332420, -10.12891450359508916, 7.618376504787018888 ) ) ;
#5073 = EDGE_LOOP ( 'NONE', ( #57638, #38829, #1222, #51521 ) ) ;
#5074 = CIRCLE ( 'NONE', #42205, 4.999999999999999112 ) ;
#5075 = FACE_OUTER_BOUND ( 'NONE', #15166, .T. ) ;
#5076 = CARTESIAN_POINT ( 'NONE',  ( -35.04834644901396956, -0.009049049589492451362, 0.01046409687783809300 ) ) ;
#5077 = CARTESIAN_POINT ( 'NONE',  ( -14.08345347783795987, -34.41374607521820650, 8.401505689979551050 ) ) ;
#5078 = DIRECTION ( 'NONE',  ( 1.000000000000000000, 0.000000000000000000, 0.000000000000000000 ) ) ;
#5079 = CARTESIAN_POINT ( 'NONE',  ( 2.000000000000001776, -3.230174184210014232, -5.998318953995379843 ) ) ;
#5080 = LINE ( 'NONE', #25676, #31452 ) ;
#5081 = AXIS2_PLACEMENT_3D ( 'NONE', #11122, #17075, #6139 ) ;
#5082 = CARTESIAN_POINT ( 'NONE',  ( 35.00000000000000000, -11.23004253107767880, -4.732539170486222524 ) ) ;
#5083 = CARTESIAN_POINT ( 'NONE',  ( -27.08417568107323703, 2.261355310631424587, -0.3682236895270699639 ) ) ;
#5084 = LINE ( 'NONE', #60269, #22684 ) ;
#5086 = EDGE_LOOP ( 'NONE', ( #24967, #20366, #22670, #24591 ) ) ;
#5085 = CARTESIAN_POINT ( 'NONE',  ( -36.00000000000000711, 9.733281772932279807, -8.235637554476541666 ) ) ;
#5087 = CARTESIAN_POINT ( 'NONE',  ( 3.152665057736252940, 7.609997527622067715, 2.258875078500286016 ) ) ;
#5088 = EDGE_LOOP ( 'NONE', ( #2988, #24299, #37985, #56306 ) ) ;
#5089 = FACE_OUTER_BOUND ( 'NONE', #403, .T. ) ;
#5090 = ORIENTED_EDGE ( 'NONE', *, *, #40336, .T. ) ;
#5091 = VERTEX_POINT ( 'NONE', #20688 ) ;
#5092 = CARTESIAN_POINT ( 'NONE',  ( 0.3164563675027597944, 8.065346584422250942, 9.237806174449792351 ) ) ;
#5093 = CARTESIAN_POINT ( 'NONE',  ( -27.08419797710328325, 0.3221715127608066331, 2.268561579780434379 ) ) ;
#5094 = CARTESIAN_POINT ( 'NONE',  ( 0.2646305136544065406, -11.46223899740597219, -4.312539723326248797 ) ) ;
#5095 = DIRECTION ( 'NONE',  ( 0.000000000000000000, -0.7790879021242441693, 0.6269146997508066033 ) ) ;
#5096 = CARTESIAN_POINT ( 'NONE',  ( 11.74548640120467979, 8.775604215601129354, -8.184666801472349817 ) ) ;
#5097 = EDGE_CURVE ( 'NONE', #15837, #7744, #9711, .T. ) ;
#5098 = CARTESIAN_POINT ( 'NONE',  ( -36.00000000000000711, -11.73555825188280011, 4.983891302653541189 ) ) ;
#5099 = EDGE_CURVE ( 'NONE', #37413, #38593, #55305, .T. ) ;
#5100 = ORIENTED_EDGE ( 'NONE', *, *, #30597, .F. ) ;
#5101 = DIRECTION ( 'NONE',  ( 0.000000000000000000, 0.000000000000000000, -1.000000000000000000 ) ) ;
#5102 = DIRECTION ( 'NONE',  ( 0.000000000000000000, 0.000000000000000000, 1.000000000000000000 ) ) ;
#5103 = CARTESIAN_POINT ( 'NONE',  ( 1.287602823385394668, 12.28793447239681136, 2.727479899219913850 ) ) ;
#5104 = ORIENTED_EDGE ( 'NONE', *, *, #23948, .T. ) ;
#5105 = EDGE_CURVE ( 'NONE', #37124, #49993, #52019, .T. ) ;
#5106 = CARTESIAN_POINT ( 'NONE',  ( 37.00000000000000711, -12.02534193257717732, 4.237174932027349961 ) ) ;
#5107 = CIRCLE ( 'NONE', #28439, 6.936499999999990784 ) ;
#5108 = CIRCLE ( 'NONE', #12525, 2.899999999999994138 ) ;
#5109 = CARTESIAN_POINT ( 'NONE',  ( 46.22120612461745282, -0.7415077656649037285, 13.24100464050679449 ) ) ;
#5110 = CARTESIAN_POINT ( 'NONE',  ( 2.000000000000001776, 0.000000000000000000, 0.000000000000000000 ) ) ;
#5112 = AXIS2_PLACEMENT_3D ( 'NONE', #24058, #23074, #58996 ) ;
#5111 = CARTESIAN_POINT ( 'NONE',  ( -26.64924965067720208, -3.627973872667547450, -24.95916750106484372 ) ) ;
#5114 = ORIENTED_EDGE ( 'NONE', *, *, #28984, .T. ) ;
#5113 = EDGE_CURVE ( 'NONE', #49413, #51431, #6482, .T. ) ;
#5115 = CARTESIAN_POINT ( 'NONE',  ( 35.00000000000000000, -6.102719229070595830, 10.54834585426226390 ) ) ;
#5116 = DIRECTION ( 'NONE',  ( 0.000000000000000000, -0.01356324068817998940, 0.9999080150203990547 ) ) ;
#5117 = CARTESIAN_POINT ( 'NONE',  ( -37.00000000000000711, -9.913596905230058098, -8.017674001891892388 ) ) ;
#5118 = EDGE_CURVE ( 'NONE', #24342, #58016, #42244, .T. ) ;
#5119 = DIRECTION ( 'NONE',  ( -1.000000000000000000, 0.000000000000000000, 0.000000000000000000 ) ) ;
#5120 = DIRECTION ( 'NONE',  ( 0.000000000000000000, -1.000000000000000000, 0.000000000000000000 ) ) ;
#5121 = EDGE_LOOP ( 'NONE', ( #11839, #19611, #16092, #17241 ) ) ;
#5122 = CARTESIAN_POINT ( 'NONE',  ( 2.297017764050092392, 0.1647869190091743041, 7.651182381906873609 ) ) ;
#5123 = CARTESIAN_POINT ( 'NONE',  ( 2.879519832977797567, 3.585229973219939748, -11.45904250108715416 ) ) ;
#5124 = DIRECTION ( 'NONE',  ( -0.000000000000000000, -1.000000000000000000, -0.000000000000000000 ) ) ;
#5125 = ORIENTED_EDGE ( 'NONE', *, *, #9814, .T. ) ;
#5126 = CARTESIAN_POINT ( 'NONE',  ( 21.63147231831337791, 13.42138622850559138, -1.508105519309493658 ) ) ;
#5127 = DIRECTION ( 'NONE',  ( 0.000000000000000000, 0.01356324068817998940, -0.9999080150203990547 ) ) ;
#5128 = ORIENTED_EDGE ( 'NONE', *, *, #6637, .F. ) ;
#5129 = ORIENTED_EDGE ( 'NONE', *, *, #18926, .F. ) ;
#5130 = VERTEX_POINT ( 'NONE', #11354 ) ;
#5131 = EDGE_CURVE ( 'NONE', #44216, #37286, #1061, .T. ) ;
#5132 = B_SPLINE_CURVE_WITH_KNOTS ( 'NONE', 3,
 ( #41725, #21796, #32062, #2147, #16470, #6488, #42044, #37049, #31729, #36741, #7128, #16778, #31425, #47392, #58019, #42348, #57355, #26429, #47062 ),
 .UNSPECIFIED., .F., .F.,
 ( 4, 3, 3, 3, 3, 3, 4 ),
 ( 8.619918672207806447E-18, 4.457896483014664354E-05, 6.639290541541868914E-05, 8.820687556478665030E-05, 0.0001100173248778875862, 0.0001545671401658071692, 0.0001830328308068590647 ),
 .UNSPECIFIED. ) ;
#5133 = ORIENTED_EDGE ( 'NONE', *, *, #34679, .F. ) ;
#5134 = ADVANCED_FACE ( 'NONE', ( #16005 ), #10691, .T. ) ;
#5135 = DIRECTION ( 'NONE',  ( 0.000000000000000000, -0.8989688749565111214, -0.4380125133594070519 ) ) ;
#5136 = FACE_OUTER_BOUND ( 'NONE', #25904, .T. ) ;
#5137 = DIRECTION ( 'NONE',  ( -1.000000000000000000, 0.000000000000000000, 0.000000000000000000 ) ) ;
#5138 = CARTESIAN_POINT ( 'NONE',  ( -22.35190811654612375, -2.161847148103705152, -3.252894036332531602 ) ) ;
#5139 = CARTESIAN_POINT ( 'NONE',  ( 5.516018279890452902, -0.006629829924290984305, -0.001397286410094293998 ) ) ;
#5140 = CIRCLE ( 'NONE', #4096, 12.18649999999999878 ) ;
#5141 = CARTESIAN_POINT ( 'NONE',  ( -13.72965000697191584, -27.65230582893893896, 12.05355732046426809 ) ) ;
#5142 = CARTESIAN_POINT ( 'NONE',  ( 11.99003848479309831, -10.55797189877288922, -8.414293459742250292 ) ) ;
#5144 = VERTEX_POINT ( 'NONE', #21331 ) ;
#5143 = CARTESIAN_POINT ( 'NONE',  ( 0.2653519890518156732, -12.06015162724940737, -2.126521162241181706 ) ) ;
#5145 = EDGE_CURVE ( 'NONE', #44559, #34363, #9963, .T. ) ;
#5146 = DIRECTION ( 'NONE',  ( 1.000000000000000000, 0.000000000000000000, 0.000000000000000000 ) ) ;
#5147 = ORIENTED_EDGE ( 'NONE', *, *, #2815, .T. ) ;
#5148 = CYLINDRICAL_SURFACE ( 'NONE', #6247, 7.499999999999988454 ) ;
#5149 = ORIENTED_EDGE ( 'NONE', *, *, #55234, .F. ) ;
#5150 = ORIENTED_EDGE ( 'NONE', *, *, #56497, .F. ) ;
#5151 = CARTESIAN_POINT ( 'NONE',  ( 0.2759803524722280188, 9.504501710971712924, -7.727919584673335507 ) ) ;
#5152 = CARTESIAN_POINT ( 'NONE',  ( 18.88852658721791045, -29.92669765328983544, 6.766054962673704765 ) ) ;
#5153 = VECTOR ( 'NONE', #45804, 1000.000000000000000 ) ;
#5154 = DIRECTION ( 'NONE',  ( 0.000000000000000000, 0.1764146379942750642, 0.9843159429275485373 ) ) ;
#5155 = DIRECTION ( 'NONE',  ( 0.000000000000000000, -0.01356324068817991828, 0.9999080150203990547 ) ) ;
#5156 = EDGE_CURVE ( 'NONE', #6304, #39733, #56936, .T. ) ;
#5157 = CARTESIAN_POINT ( 'NONE',  ( 10.66583743953261809, 7.973724152180643010, 8.969682718315048930 ) ) ;
#5158 = CARTESIAN_POINT ( 'NONE',  ( 37.00000000000000711, -2.696588552979144460, -12.46157735505188491 ) ) ;
#5159 = ORIENTED_EDGE ( 'NONE', *, *, #685, .F. ) ;
#5160 = AXIS2_PLACEMENT_3D ( 'NONE', #23259, #54518, #64777 ) ;
#5161 = AXIS2_PLACEMENT_3D ( 'NONE', #18143, #3855, #44067 ) ;
#5162 = VERTEX_POINT ( 'NONE', #7027 ) ;
#5163 = CARTESIAN_POINT ( 'NONE',  ( -22.94572469358971034, -4.011883207821678177, -2.792384151940671799 ) ) ;
#5164 = ORIENTED_EDGE ( 'NONE', *, *, #19774, .T. ) ;
#5165 = AXIS2_PLACEMENT_3D ( 'NONE', #1735, #22002, #37288 ) ;
#5166 = ORIENTED_EDGE ( 'NONE', *, *, #35744, .T. ) ;
#5167 = DIRECTION ( 'NONE',  ( -1.000000000000000000, 0.000000000000000000, 0.000000000000000000 ) ) ;
#5168 = CARTESIAN_POINT ( 'NONE',  ( -37.00000000000000711, 6.917234959366964198, -9.493370459201624811 ) ) ;
#5169 = AXIS2_PLACEMENT_3D ( 'NONE', #43848, #23914, #60120 ) ;
#5170 = CARTESIAN_POINT ( 'NONE',  ( -35.00000000000000000, -4.018060380616481631, 11.50504120060941915 ) ) ;
#5171 = CARTESIAN_POINT ( 'NONE',  ( 16.90635187068963319, 9.959026633630651659, 6.781309966538392686 ) ) ;
#5172 = CARTESIAN_POINT ( 'NONE',  ( -22.27721038036499834, 1.315315479297517465, -3.438655654856780597 ) ) ;
#5173 = LINE ( 'NONE', #41374, #49081 ) ;
#5174 = PLANE ( 'NONE',  #52485 ) ;
#5175 = ADVANCED_FACE ( 'NONE', ( #6380 ), #26649, .T. ) ;
#5176 = ORIENTED_EDGE ( 'NONE', *, *, #52274, .F. ) ;
#5177 = ORIENTED_EDGE ( 'NONE', *, *, #29490, .T. ) ;
#5178 = DIRECTION ( 'NONE',  ( -1.000000000000000000, 0.000000000000000000, 0.000000000000000000 ) ) ;
#5179 = CARTESIAN_POINT ( 'NONE',  ( -37.00000000000000711, -3.640372113593639547, 12.21925492305360983 ) ) ;
#5180 = DIRECTION ( 'NONE',  ( 0.000000000000000000, 0.8835120444460240474, -0.4684084406997880423 ) ) ;
#5181 = CARTESIAN_POINT ( 'NONE',  ( -27.35552965826137140, -3.094132632038958608, -0.2619431035392160156 ) ) ;
#5182 = AXIS2_PLACEMENT_3D ( 'NONE', #53849, #64452, #23924 ) ;
#5183 = DIRECTION ( 'NONE',  ( 0.3865475372811021382, -0.8082200352954679312, 0.4442537292684300421 ) ) ;
#5184 = CYLINDRICAL_SURFACE ( 'NONE', #50079, 4.999999999999999112 ) ;
#5185 = CARTESIAN_POINT ( 'NONE',  ( 2.000000000000001776, 0.000000000000000000, 0.000000000000000000 ) ) ;
#5186 = LINE ( 'NONE', #60370, #41581 ) ;
#5187 = EDGE_CURVE ( 'NONE', #35366, #30999, #17341, .T. ) ;
#5188 = ORIENTED_EDGE ( 'NONE', *, *, #6526, .F. ) ;
#5189 = CARTESIAN_POINT ( 'NONE',  ( -18.08686583997275221, 5.151216734910927464, -12.47858029384662970 ) ) ;
#5190 = CARTESIAN_POINT ( 'NONE',  ( 22.57855258442564761, -4.427776684447072952, -11.15324139578564910 ) ) ;
#5191 = CARTESIAN_POINT ( 'NONE',  ( -35.00000000000000000, 0.000000000000000000, 0.000000000000000000 ) ) ;
#5192 = EDGE_CURVE ( 'NONE', #39732, #37109, #21020, .T. ) ;
#5193 = AXIS2_PLACEMENT_3D ( 'NONE', #1582, #10880, #31169 ) ;
#5194 = CARTESIAN_POINT ( 'NONE',  ( 37.00000000000000711, 4.705694406421931860E-17, -3.469127814946512892E-15 ) ) ;
#5195 = AXIS2_PLACEMENT_3D ( 'NONE', #2075, #17382, #17711 ) ;
#5196 = EDGE_LOOP ( 'NONE', ( #57397, #60145, #55905, #60991 ) ) ;
#5197 = CARTESIAN_POINT ( 'NONE',  ( -35.00000000000000000, 0.000000000000000000, 0.000000000000000000 ) ) ;
#5198 = CARTESIAN_POINT ( 'NONE',  ( 3.047904605210279616, 6.622084192655491641, 4.313929735713805336 ) ) ;
#5199 = CARTESIAN_POINT ( 'NONE',  ( 18.88852658721791045, -28.93036277062534012, -6.677752214540050524 ) ) ;
#5200 = EDGE_LOOP ( 'NONE', ( #36657, #4393, #31789, #12330 ) ) ;
#5201 = CIRCLE ( 'NONE', #56168, 2.899999999999996803 ) ;
#5202 = DIRECTION ( 'NONE',  ( 0.000000000000000000, -0.7621620551276425681, 0.6473862847818204758 ) ) ;
#5203 = CARTESIAN_POINT ( 'NONE',  ( -36.00000000000000711, -0.6593684648221369571, 12.73293890771483383 ) ) ;
#5204 = CARTESIAN_POINT ( 'NONE',  ( -22.28073302975500880, -0.9769664947681180323, -3.560599703067835797 ) ) ;
#5205 = AXIS2_PLACEMENT_3D ( 'NONE', #65015, #12844, #53438 ) ;
#5207 = ORIENTED_EDGE ( 'NONE', *, *, #23845, .F. ) ;
#5206 = CYLINDRICAL_SURFACE ( 'NONE', #1063, 12.18649999999999878 ) ;
#5208 = FACE_OUTER_BOUND ( 'NONE', #19290, .T. ) ;
#5209 = EDGE_CURVE ( 'NONE', #9622, #64587, #8605, .T. ) ;
#5210 = CARTESIAN_POINT ( 'NONE',  ( 3.152665057735657861, -7.609997527621795932, -2.258875078500884204 ) ) ;
#5211 = ORIENTED_EDGE ( 'NONE', *, *, #62630, .F. ) ;
#5212 = CARTESIAN_POINT ( 'NONE',  ( -1.734723475976807094E-15, -3.469446951953614189E-15, -11.99999999999998934 ) ) ;
#5213 = CARTESIAN_POINT ( 'NONE',  ( -9.027418811960407297, 12.84010590367175020, -4.182636090463161871 ) ) ;
#5214 = CARTESIAN_POINT ( 'NONE',  ( -16.82774105938391429, 8.087890278022925372, -10.80991447578766973 ) ) ;
#5215 = CARTESIAN_POINT ( 'NONE',  ( 8.813543937826676000, 6.315452948875024397, -11.93749476812985222 ) ) ;
#5216 = CYLINDRICAL_SURFACE ( 'NONE', #54551, 5.000000000000001776 ) ;
#5217 = CARTESIAN_POINT ( 'NONE',  ( 37.00000000000000711, 0.3137578094511062066, 12.74613886779084204 ) ) ;
#5218 = CARTESIAN_POINT ( 'NONE',  ( 37.00000000000000711, -7.238157050195554554, 10.49626516989278180 ) ) ;
#5219 = ORIENTED_EDGE ( 'NONE', *, *, #62885, .T. ) ;
#5220 = CARTESIAN_POINT ( 'NONE',  ( 2.258463476536645587, -5.014277205346500565, 5.764393264552618135 ) ) ;
#5221 = ORIENTED_EDGE ( 'NONE', *, *, #20402, .F. ) ;
#5222 = DIRECTION ( 'NONE',  ( 0.000000000000000000, 0.04924826701373895277, 0.9987865678893280696 ) ) ;
#5223 = EDGE_CURVE ( 'NONE', #51364, #52741, #20993, .T. ) ;
#5224 = CARTESIAN_POINT ( 'NONE',  ( 3.152665057735980714, 1.848755561853925533, 7.719888720907654545 ) ) ;
#5225 = CIRCLE ( 'NONE', #24335, 5.000000000000000000 ) ;
#5226 = CARTESIAN_POINT ( 'NONE',  ( -36.00000000000000711, 9.506317355798369562, 8.496612874013196759 ) ) ;
#5227 = ORIENTED_EDGE ( 'NONE', *, *, #5414, .T. ) ;
#5228 = DIRECTION ( 'NONE',  ( -1.000000000000000000, 0.000000000000000000, 0.000000000000000000 ) ) ;
#5229 = CARTESIAN_POINT ( 'NONE',  ( 12.17720086923866951, 9.239009060064711676, -7.666669395372703200 ) ) ;
#5230 = CIRCLE ( 'NONE', #41235, 2.899999999999994582 ) ;
#5231 = CARTESIAN_POINT ( 'NONE',  ( -22.27706485742869091, -1.508175983031604606, 3.358064672837097753 ) ) ;
#5232 = VERTEX_POINT ( 'NONE', #6065 ) ;
#5233 = ORIENTED_EDGE ( 'NONE', *, *, #42679, .T. ) ;
#5234 = DIRECTION ( 'NONE',  ( 0.000000000000000000, -0.01356324068817999114, 0.9999080150203989437 ) ) ;
#5235 = ORIENTED_EDGE ( 'NONE', *, *, #17726, .T. ) ;
#5236 = CYLINDRICAL_SURFACE ( 'NONE', #29557, 12.18649999999999878 ) ;
#5237 = DIRECTION ( 'NONE',  ( 0.000000000000000000, -0.01356324068817991828, 0.9999080150203990547 ) ) ;
#5238 = CARTESIAN_POINT ( 'NONE',  ( 37.00000000000000711, 4.018060380616396365, -11.50504120060944757 ) ) ;
#5239 = VECTOR ( 'NONE', #59750, 1000.000000000000000 ) ;
#5240 = DIRECTION ( 'NONE',  ( -1.000000000000000000, 0.000000000000000000, 0.000000000000000000 ) ) ;
#5241 = CARTESIAN_POINT ( 'NONE',  ( 2.000000000000001776, -6.253963800348206092, -4.139799123621114241 ) ) ;
#5242 = LINE ( 'NONE', #25510, #5153 ) ;
#5243 = CARTESIAN_POINT ( 'NONE',  ( -35.00000000000000000, 6.303578524886947143, 10.42955799785322490 ) ) ;
#5244 = VECTOR ( 'NONE', #44505, 1000.000000000000000 ) ;
#5245 = EDGE_CURVE ( 'NONE', #31059, #17057, #39276, .T. ) ;
#5246 = ORIENTED_EDGE ( 'NONE', *, *, #31498, .F. ) ;
#5247 =( BOUNDED_SURFACE ( )  B_SPLINE_SURFACE ( 3, 1, ( 
 ( #35037, #65627 ),
 ( #35705, #56002 ),
 ( #9788, #30072 ),
 ( #51026, #50385 ) ),
 .UNSPECIFIED., .F., .F., .F. ) 
 B_SPLINE_SURFACE_WITH_KNOTS ( ( 4, 4 ),
 ( 2, 2 ),
 ( 0.000000000000000000, 1.000000000000000000 ),
 ( 0.000000000000000000, 1.000000000000000000 ),
 .UNSPECIFIED. ) 
 GEOMETRIC_REPRESENTATION_ITEM ( )  RATIONAL_B_SPLINE_SURFACE ( (
 ( 1.000000000000000000, 1.000000000000000000),
 ( 0.9942764183789327692, 0.8450855930916585379),
 ( 0.9942764183789327692, 0.8450855930916585379),
 ( 1.000000000000000000, 1.000000000000000000) ) ) 
 REPRESENTATION_ITEM ( '' )  SURFACE ( )  );
#5248 = CARTESIAN_POINT ( 'NONE',  ( 2.266490820343223245, 7.641399530653804284, -0.1453321357832998706 ) ) ;
#5249 = EDGE_CURVE ( 'NONE', #56247, #50602, #63207, .T. ) ;
#5250 = CARTESIAN_POINT ( 'NONE',  ( 35.00000000000000000, -11.35427606708803161, 4.426194442447358490 ) ) ;
#5251 = CARTESIAN_POINT ( 'NONE',  ( 1.937114397841932290, -10.63710405811928794, -7.182898292393876893 ) ) ;
#5252 = CARTESIAN_POINT ( 'NONE',  ( 12.67839809834435805, 12.93864317191487778, -3.856941399089210076 ) ) ;
#5253 = LINE ( 'NONE', #21534, #20162 ) ;
#5254 = FACE_OUTER_BOUND ( 'NONE', #57256, .T. ) ;
#5255 = DIRECTION ( 'NONE',  ( 0.000000000000000000, 0.000000000000000000, 1.000000000000000000 ) ) ;
#5256 = CIRCLE ( 'NONE', #50920, 12.74999999999999822 ) ;
#5257 = CARTESIAN_POINT ( 'NONE',  ( 35.00000000000000000, 5.015831474386306610, -10.62137734850269943 ) ) ;
#5258 = ORIENTED_EDGE ( 'NONE', *, *, #43132, .T. ) ;
#5259 = ADVANCED_FACE ( 'NONE', ( #12999 ), #64091, .F. ) ;
#5260 = DIRECTION ( 'NONE',  ( 0.000000000000000000, 0.6051742151937610226, 0.7960930657056468629 ) ) ;
#5261 = ORIENTED_EDGE ( 'NONE', *, *, #10077, .T. ) ;
#5262 = CARTESIAN_POINT ( 'NONE',  ( -3.543624739456839645, -9.146489499550646940, 7.778742444933206102 ) ) ;
#5263 = CARTESIAN_POINT ( 'NONE',  ( 5.515539859299206427, -0.003740028639278314155, 0.004759416711442216591 ) ) ;
#5264 = CARTESIAN_POINT ( 'NONE',  ( 1.452237505248555660, 1.611965288198897506, -12.55261342181973738 ) ) ;
#5265 = DIRECTION ( 'NONE',  ( 0.000000000000000000, -0.9105187689795911643, 0.4134677391718609707 ) ) ;
#5266 = CYLINDRICAL_SURFACE ( 'NONE', #27569, 15.00000000000000000 ) ;
#5267 = EDGE_CURVE ( 'NONE', #41256, #28847, #36919, .T. ) ;
#5268 = ORIENTED_EDGE ( 'NONE', *, *, #4983, .T. ) ;
#5269 = CARTESIAN_POINT ( 'NONE',  ( -22.27384469013076185, 2.625926801827887846, -2.581192766446249731 ) ) ;
#5270 = LINE ( 'NONE', #51160, #8733 ) ;
#5271 = CARTESIAN_POINT ( 'NONE',  ( 35.00000000000000000, 11.61175578952788356, 1.771820996347031940 ) ) ;
#5272 = CARTESIAN_POINT ( 'NONE',  ( -22.27706485742869091, 2.580541389029920030, 2.625261754997667119 ) ) ;
#5273 = AXIS2_PLACEMENT_3D ( 'NONE', #24557, #64149, #18625 ) ;
#5274 = FACE_OUTER_BOUND ( 'NONE', #49786, .T. ) ;
#5275 = CARTESIAN_POINT ( 'NONE',  ( 2.269879328256730666, 2.753278809616109157, 7.130835954829854550 ) ) ;
#5276 = VERTEX_POINT ( 'NONE', #8340 ) ;
#5277 = CIRCLE ( 'NONE', #32876, 6.936499999999990784 ) ;
#5278 = CARTESIAN_POINT ( 'NONE',  ( -27.09125059358712306, -0.5611156659247565903, 2.243253600383845914 ) ) ;
#5279 = ORIENTED_EDGE ( 'NONE', *, *, #29490, .F. ) ;
#5280 = CARTESIAN_POINT ( 'NONE',  ( 0.2647959493198550618, -0.1469673141000716610, -12.24513905663510904 ) ) ;
#5281 = CARTESIAN_POINT ( 'NONE',  ( 47.00000000000000711, 4.705694406421931860E-17, -3.469127814946512892E-15 ) ) ;
#5282 = FACE_OUTER_BOUND ( 'NONE', #16550, .T. ) ;
#5283 = CARTESIAN_POINT ( 'NONE',  ( 0.3106921474978494579, -11.60027394202201378, 3.971572160646712479 ) ) ;
#5284 = CIRCLE ( 'NONE', #13753, 4.999999999999999112 ) ;
#5285 = B_SPLINE_CURVE_WITH_KNOTS ( 'NONE', 3,
 ( #28824, #39442, #54441, #18554, #34123, #54765, #60383, #59105, #8872, #65039, #34764, #33797, #40091, #59743, #35092, #64072, #49461, #43793, #24157 ),
 .UNSPECIFIED., .F., .F.,
 ( 4, 3, 3, 3, 3, 3, 4 ),
 ( 5.962126228860470552E-18, 2.825908398831331847E-05, 4.208813692484108843E-05, 5.591713746944027057E-05, 6.279584083232090871E-05, 9.105792820296878360E-05, 0.0001153131102488872209 ),
 .UNSPECIFIED. ) ;
#5286 = ORIENTED_EDGE ( 'NONE', *, *, #42675, .T. ) ;
#5287 = ORIENTED_EDGE ( 'NONE', *, *, #31216, .T. ) ;
#5288 = CARTESIAN_POINT ( 'NONE',  ( -16.98800322446194855, 2.922502605998049674, -13.17987020110343543 ) ) ;
#5289 = ORIENTED_EDGE ( 'NONE', *, *, #59908, .T. ) ;
#5290 = AXIS2_PLACEMENT_3D ( 'NONE', #22961, #53872, #53557 ) ;
#5291 = CARTESIAN_POINT ( 'NONE',  ( 35.00000000000000000, 4.705694406421931860E-17, -3.469127814946512892E-15 ) ) ;
#5292 = CYLINDRICAL_SURFACE ( 'NONE', #27930, 2.899999999999994582 ) ;
#5293 = CARTESIAN_POINT ( 'NONE',  ( -22.27721688985630166, -3.446999288411544349, -1.293557211780071103 ) ) ;
#5294 = DIRECTION ( 'NONE',  ( -1.000000000000000000, -0.000000000000000000, 0.000000000000000000 ) ) ;
#5295 = CARTESIAN_POINT ( 'NONE',  ( 1.633930747253262705, 9.253127167384784357, -8.702439996575780157 ) ) ;
#5296 = CARTESIAN_POINT ( 'NONE',  ( 0.3665391374699464300, -7.691255657244227883, -9.576575648339098024 ) ) ;
#5298 = DIRECTION ( 'NONE',  ( 0.000000000000000000, -0.7621620551276425681, 0.6473862847818204758 ) ) ;
#5297 = B_SPLINE_CURVE_WITH_KNOTS ( 'NONE', 3,
 ( #19094, #23775, #8797, #19434, #9111, #58704, #28737 ),
 .UNSPECIFIED., .F., .F.,
 ( 4, 3, 4 ),
 ( 0.000000000000000000, 0.001700533616330726855, 0.005002426799376749611 ),
 .UNSPECIFIED. ) ;
#5299 = ORIENTED_EDGE ( 'NONE', *, *, #62647, .F. ) ;
#5300 = CARTESIAN_POINT ( 'NONE',  ( 1.109979610370654735, -11.08130463534499910, 5.843815872356589836 ) ) ;
#5301 = CIRCLE ( 'NONE', #46726, 4.999999999999999112 ) ;
#5302 = ORIENTED_EDGE ( 'NONE', *, *, #27879, .F. ) ;
#5303 = DIRECTION ( 'NONE',  ( 1.000000000000000000, -0.000000000000000000, 0.000000000000000000 ) ) ;
#5304 = EDGE_CURVE ( 'NONE', #5000, #22716, #18703, .T. ) ;
#5305 = CARTESIAN_POINT ( 'NONE',  ( -27.08506889328327460, 1.872884652026870045, -1.324351020479947350 ) ) ;
#5306 = VERTEX_POINT ( 'NONE', #43920 ) ;
#5307 = CARTESIAN_POINT ( 'NONE',  ( 2.350038591457611847, -6.324706260080944276, -8.533611140766819148 ) ) ;
#5308 = VERTEX_POINT ( 'NONE', #52491 ) ;
#5309 = DIRECTION ( 'NONE',  ( 0.000000000000000000, 0.01356324068817992175, -0.9999080150203990547 ) ) ;
#5310 = CARTESIAN_POINT ( 'NONE',  ( -19.47984447937493613, -1.416020129149132334, 25.00000000000000000 ) ) ;
#5311 = CARTESIAN_POINT ( 'NONE',  ( 3.031336079629501690, 3.088871717871464639, 7.268683861177206218 ) ) ;
#5312 = CARTESIAN_POINT ( 'NONE',  ( 7.253112616783349509, -5.573154064202213931, 10.62982316258792537 ) ) ;
#5313 = ORIENTED_EDGE ( 'NONE', *, *, #57217, .T. ) ;
#5314 = ORIENTED_EDGE ( 'NONE', *, *, #55178, .F. ) ;
#5315 = CARTESIAN_POINT ( 'NONE',  ( 0.000000000000000000, 7.203928197742101247, 2.086484728383167564 ) ) ;
#5316 = ORIENTED_EDGE ( 'NONE', *, *, #47336, .F. ) ;
#5317 = CARTESIAN_POINT ( 'NONE',  ( 35.00000000000000000, 4.705694406421931860E-17, -3.469127814946512892E-15 ) ) ;
#5318 = EDGE_LOOP ( 'NONE', ( #56575, #8824, #13539, #46280 ) ) ;
#5319 = ORIENTED_EDGE ( 'NONE', *, *, #60575, .F. ) ;
#5320 = ORIENTED_EDGE ( 'NONE', *, *, #56146, .F. ) ;
#5321 = DIRECTION ( 'NONE',  ( -1.000000000000000000, -0.000000000000000000, 0.000000000000000000 ) ) ;
#5322 = CARTESIAN_POINT ( 'NONE',  ( 6.904443316226201333, -26.24011843744384009, 14.86481251185163366 ) ) ;
#5323 = CIRCLE ( 'NONE', #49932, 12.74999999999999822 ) ;
#5324 = ADVANCED_FACE ( 'NONE', ( #6924 ), #29803, .T. ) ;
#5326 = AXIS2_PLACEMENT_3D ( 'NONE', #41131, #14863, #55796 ) ;
#5325 = CARTESIAN_POINT ( 'NONE',  ( -35.00000000000000000, 0.000000000000000000, 0.000000000000000000 ) ) ;
#5327 = CARTESIAN_POINT ( 'NONE',  ( -26.74023318801843274, 3.035730054944089762, -1.425982498898162643 ) ) ;
#5328 = CARTESIAN_POINT ( 'NONE',  ( -22.28506771379528573, -1.636577531579579414, 3.348518833762379909 ) ) ;
#5329 = VERTEX_POINT ( 'NONE', #5960 ) ;
#5330 = CARTESIAN_POINT ( 'NONE',  ( 2.241311220309522234, -2.523702734785425061, -7.205198716057754638 ) ) ;
#5331 = VERTEX_POINT ( 'NONE', #11889 ) ;
#5332 = DIRECTION ( 'NONE',  ( -1.000000000000000000, -0.000000000000000000, 0.000000000000000000 ) ) ;
#5333 = ADVANCED_FACE ( 'NONE', ( #62755 ), #22542, .T. ) ;
#5334 = CARTESIAN_POINT ( 'NONE',  ( -3.550933850019966531, 11.20544481737731068, 7.538207320140815071 ) ) ;
#5335 = EDGE_CURVE ( 'NONE', #50397, #44716, #1166, .T. ) ;
#5336 = B_SPLINE_CURVE_WITH_KNOTS ( 'NONE', 3,
 ( #12289, #12953, #48548, #33236, #53546, #47881 ),
 .UNSPECIFIED., .F., .F.,
 ( 4, 2, 4 ),
 ( 0.004228585846910009986, 0.006274987364148632354, 0.008321388881387255590 ),
 .UNSPECIFIED. ) ;
#5337 = ORIENTED_EDGE ( 'NONE', *, *, #31735, .T. ) ;
#5338 = CARTESIAN_POINT ( 'NONE',  ( 37.00000000000000711, 6.564808257521771218, -10.93004082984021075 ) ) ;
#5339 = DIRECTION ( 'NONE',  ( 0.000000000000000000, 0.01356324068817998940, -0.9999080150203990547 ) ) ;
#5340 = CARTESIAN_POINT ( 'NONE',  ( 0.000000000000000000, 0.000000000000000000, 0.000000000000000000 ) ) ;
#5341 = AXIS2_PLACEMENT_3D ( 'NONE', #32504, #53138, #2629 ) ;
#5342 = ORIENTED_EDGE ( 'NONE', *, *, #61876, .F. ) ;
#5343 = ADVANCED_FACE ( 'NONE', ( #32490 ), #59425, .F. ) ;
#5344 = CARTESIAN_POINT ( 'NONE',  ( -37.00000000000000711, 0.000000000000000000, 0.000000000000000000 ) ) ;
#5345 = AXIS2_PLACEMENT_3D ( 'NONE', #61447, #65770, #5633 ) ;
#5346 = EDGE_LOOP ( 'NONE', ( #11701, #61492, #32104, #16570 ) ) ;
#5347 = EDGE_CURVE ( 'NONE', #55989, #63543, #9636, .T. ) ;
#5348 = CARTESIAN_POINT ( 'NONE',  ( -24.35585564769671407, -10.90390688210781356, 7.962067492493469345 ) ) ;
#5349 = CARTESIAN_POINT ( 'NONE',  ( 10.63650944684269639, -26.92414420718871071, -13.64813004266018481 ) ) ;
#5350 = FACE_OUTER_BOUND ( 'NONE', #51042, .T. ) ;
#5351 = CARTESIAN_POINT ( 'NONE',  ( 36.00000000000000711, -2.080187960898473243, 12.57916205664483122 ) ) ;
#5352 = CARTESIAN_POINT ( 'NONE',  ( 2.241528039335008327, 7.515727438420007900, 1.341200777944175027 ) ) ;
#5353 = ORIENTED_EDGE ( 'NONE', *, *, #7362, .F. ) ;
#5354 = CARTESIAN_POINT ( 'NONE',  ( 35.00000000000000000, 4.705694406421931860E-17, -3.469127814946512892E-15 ) ) ;
#5356 = AXIS2_PLACEMENT_3D ( 'NONE', #8494, #45304, #40969 ) ;
#5355 = CARTESIAN_POINT ( 'NONE',  ( 1.633930747253262261, 5.718685543473208455, -11.34237452761398757 ) ) ;
#5357 = FACE_OUTER_BOUND ( 'NONE', #43136, .T. ) ;
#5358 = CARTESIAN_POINT ( 'NONE',  ( 22.22366945088117518, -13.44460711623439941, -1.270151499113232774 ) ) ;
#5359 = ADVANCED_FACE ( 'NONE', ( #17225 ), #17558, .T. ) ;
#5360 = CARTESIAN_POINT ( 'NONE',  ( 0.2801149460245135892, 12.24954625471156255, -0.1962575296605837960 ) ) ;
#5361 = CARTESIAN_POINT ( 'NONE',  ( 2.241449424704146320, 2.668712484599962131, 7.152834201978770068 ) ) ;
#5362 = CARTESIAN_POINT ( 'NONE',  ( 0.2653519991613847440, -2.148211862902992486, 12.05632699103097139 ) ) ;
#5363 = DIRECTION ( 'NONE',  ( 0.000000000000000000, -0.01356324068817992175, 0.9999080150203990547 ) ) ;
#5364 = CARTESIAN_POINT ( 'NONE',  ( -35.00000000000000000, -11.37311665002361494, -2.936739658819992549 ) ) ;
#5365 = CIRCLE ( 'NONE', #58438, 5.000000000000000888 ) ;
#5366 = CIRCLE ( 'NONE', #51035, 12.00000000000000000 ) ;
#5367 = AXIS2_PLACEMENT_3D ( 'NONE', #36002, #17646, #51674 ) ;
#5368 = ORIENTED_EDGE ( 'NONE', *, *, #13546, .F. ) ;
#5369 = VERTEX_POINT ( 'NONE', #52151 ) ;
#5370 = CARTESIAN_POINT ( 'NONE',  ( -35.00000000000000000, -11.78745411414837818, -3.093009498344053032 ) ) ;
#5371 = CARTESIAN_POINT ( 'NONE',  ( 37.67868074218839070, -2.196220884325986500, 20.39261666198438405 ) ) ;
#5372 = DIRECTION ( 'NONE',  ( -1.000000000000000000, -0.000000000000000000, -0.000000000000000000 ) ) ;
#5373 = CARTESIAN_POINT ( 'NONE',  ( 2.259830038566062793, -1.190932096468327650, -7.547174990768978020 ) ) ;
#5374 = ORIENTED_EDGE ( 'NONE', *, *, #12286, .F. ) ;
#5375 = ORIENTED_EDGE ( 'NONE', *, *, #41754, .T. ) ;
#5376 = EDGE_LOOP ( 'NONE', ( #57279, #57840, #46225, #61713, #12806, #30994, #19463, #65482, #2347, #39806, #46203, #10129, #14736, #61394, #45973, #8508, #15397, #43632, #39988, #9520, #26057, #892, #51937, #22174, #49693, #32674, #1732, #24673, #5667, #22562, #17321, #33439, #23956, #45238, #2474, #22871, #875, #13979, #31224, #21692, #1653, #16822, #65304, #53043, #61555, #30576, #43178, #59131, #43652, #3164, #30861, #9813, #7442, #40855, #64714, #46141, #10389, #56317, #41397, #47915, #8913, #31584, #14679, #32001, #1133, #11489, #62606, #37301, #17912, #40627, #10640, #14770, #49210, #22658, #61141, #43679, #60172, #2851, #17419, #8160, #63061, #20158, #19354, #54482, #45603, #64549, #63230, #47257, #58445, #38656, #38678, #49185, #10903, #39271, #24580, #10437, #58646, #32682, #58413, #28703, #18069, #34789, #30047, #9065, #59694, #3496, #64925, #27643, #58910, #4795, #8637, #32656 ) ) ;
#5377 = B_SPLINE_CURVE_WITH_KNOTS ( 'NONE', 3,
 ( #64901, #28683, #8093, #53967, #8407, #38989, #13074, #59284, #49335, #13708, #14038, #49638, #43989, #38676, #24040, #28046, #44611, #48347, #7764 ),
 .UNSPECIFIED., .F., .F.,
 ( 4, 3, 3, 3, 3, 3, 4 ),
 ( 6.447129612864634281E-18, 2.825908398830911041E-05, 4.208813692483603334E-05, 5.591713746943527646E-05, 6.279584083231498626E-05, 9.105792820296256299E-05, 0.0001153131102488861502 ),
 .UNSPECIFIED. ) ;
#5378 = CARTESIAN_POINT ( 'NONE',  ( 0.3665391374699464300, 8.095513416941352958, -9.237363111276685856 ) ) ;
#5379 = CIRCLE ( 'NONE', #53182, 12.18650000000000055 ) ;
#5380 = EDGE_CURVE ( 'NONE', #62829, #39914, #32980, .T. ) ;
#5381 = DIRECTION ( 'NONE',  ( -1.000000000000000000, -0.000000000000000000, -0.000000000000000000 ) ) ;
#5382 = EDGE_LOOP ( 'NONE', ( #12078, #56682, #44010, #42765 ) ) ;
#5383 =( LENGTH_UNIT ( ) NAMED_UNIT ( * ) SI_UNIT ( .MILLI., .METRE. ) );
#5384 = DIRECTION ( 'NONE',  ( 0.000000000000000000, -0.7621620551276424571, 0.6473862847818206978 ) ) ;
#5385 = CIRCLE ( 'NONE', #23416, 6.936499999999989896 ) ;
#5386 = AXIS2_PLACEMENT_3D ( 'NONE', #13837, #23191, #17878 ) ;
#5387 = CARTESIAN_POINT ( 'NONE',  ( 2.491965175174155167, -2.439431489055726932, 7.322278065136082148 ) ) ;
#5388 = ORIENTED_EDGE ( 'NONE', *, *, #63224, .T. ) ;
#5389 = DIRECTION ( 'NONE',  ( 0.4838294062566934617, -0.000000000000000000, 0.8751623310228197061 ) ) ;
#5390 = EDGE_CURVE ( 'NONE', #7766, #4955, #27384, .T. ) ;
#5391 = CARTESIAN_POINT ( 'NONE',  ( -0.8948477690460417966, -30.54755392045676032, -15.29677453898885808 ) ) ;
#5392 = DIRECTION ( 'NONE',  ( 0.000000000000000000, -1.000000000000000000, 0.000000000000000000 ) ) ;
#5393 = EDGE_LOOP ( 'NONE', ( #61495, #51271, #36075, #15378 ) ) ;
#5394 = CARTESIAN_POINT ( 'NONE',  ( -25.64778288570173004, 7.682669607182226024, 11.10295593026793881 ) ) ;
#5395 = EDGE_LOOP ( 'NONE', ( #37409, #20370, #39695, #7081 ) ) ;
#5396 = DIRECTION ( 'NONE',  ( 1.000000000000000000, 0.000000000000000000, 0.000000000000000000 ) ) ;
#5397 = EDGE_CURVE ( 'NONE', #26006, #26098, #13846, .T. ) ;
#5398 = ORIENTED_EDGE ( 'NONE', *, *, #7792, .T. ) ;
#5399 = CARTESIAN_POINT ( 'NONE',  ( 13.15445328062423691, -9.891953278793183202, -6.796930734482528713 ) ) ;
#5400 = CARTESIAN_POINT ( 'NONE',  ( -15.05999060605047646, -34.74914171045048050, 6.965575872677295166 ) ) ;
#5401 = CARTESIAN_POINT ( 'NONE',  ( -35.00000000000000000, -11.60979404548637461, 3.704519465651263221 ) ) ;
#5402 = CARTESIAN_POINT ( 'NONE',  ( -22.71097035706203116, 4.965150228107710006, 0.4203397252017151420 ) ) ;
#5403 = CARTESIAN_POINT ( 'NONE',  ( 0.2647959493198550618, -12.24513905663510727, 0.1469673141001137107 ) ) ;
#5404 = EDGE_CURVE ( 'NONE', #45182, #30052, #43620, .T. ) ;
#5405 = CARTESIAN_POINT ( 'NONE',  ( 2.241317068080775687, 5.789053609344685825, -4.977030124433445835 ) ) ;
#5406 = DIRECTION ( 'NONE',  ( 1.000000000000000000, 0.000000000000000000, 0.000000000000000000 ) ) ;
#5407 = CARTESIAN_POINT ( 'NONE',  ( 8.450039533779039047, 4.867621807257259015, -10.97047568558763686 ) ) ;
#5409 = VERTEX_POINT ( 'NONE', #6273 ) ;
#5408 = CARTESIAN_POINT ( 'NONE',  ( -18.14857107993011809, 3.486035047582784596, -13.04429203975358398 ) ) ;
#5410 = FACE_OUTER_BOUND ( 'NONE', #61546, .T. ) ;
#5411 = ORIENTED_EDGE ( 'NONE', *, *, #20981, .F. ) ;
#5412 = CARTESIAN_POINT ( 'NONE',  ( 0.3160775863651066331, -4.419114254409969966, 11.43919651388224068 ) ) ;
#5413 = ORIENTED_EDGE ( 'NONE', *, *, #34278, .F. ) ;
#5414 = EDGE_CURVE ( 'NONE', #65324, #21734, #28777, .T. ) ;
#5415 = B_SPLINE_CURVE_WITH_KNOTS ( 'NONE', 3,
 ( #5224, #25491, #45782, #883, #20518, #40801, #15509, #56077, #30792, #7499, #52749, #63037, #27792, #31471, #48095, #57081 ),
 .UNSPECIFIED., .F., .F.,
 ( 4, 3, 3, 3, 3, 4 ),
 ( 2.855882139221416949E-15, 0.0002126834539179672833, 0.0004253519300366195768, 0.0006380165497224064147, 0.0007442707582428126139, 0.0009453531351418871694 ),
 .UNSPECIFIED. ) ;
#5416 = DIRECTION ( 'NONE',  ( 1.000000000000000000, 0.000000000000000000, -0.000000000000000000 ) ) ;
#5417 = CONICAL_SURFACE ( 'NONE', #15963, 7.938172270156617749, 1.280189991382167047 ) ;
#5418 = EDGE_CURVE ( 'NONE', #46803, #44248, #30846, .T. ) ;
#5419 = ORIENTED_EDGE ( 'NONE', *, *, #52269, .T. ) ;
#5420 = CARTESIAN_POINT ( 'NONE',  ( 0.3632410797595235774, 8.092233745354631580, 9.235006602299375089 ) ) ;
#5421 = CARTESIAN_POINT ( 'NONE',  ( 1.109979610372407999, 11.92772269523445772, -3.830786822172277617 ) ) ;
#5422 = CARTESIAN_POINT ( 'NONE',  ( 22.68177428654798433, -4.560196341733016467, 11.10067150598529473 ) ) ;
#5423 = CARTESIAN_POINT ( 'NONE',  ( -22.28023996335807411, 1.558279384310090387, -3.345627887484357021 ) ) ;
#5424 = CARTESIAN_POINT ( 'NONE',  ( 35.00000000000000000, 4.705694406421931860E-17, -3.469127814946512892E-15 ) ) ;
#5425 = CIRCLE ( 'NONE', #39375, 2.899999999999995026 ) ;
#5426 = AXIS2_PLACEMENT_3D ( 'NONE', #41840, #16246, #17567 ) ;
#5427 = ORIENTED_EDGE ( 'NONE', *, *, #56706, .F. ) ;
#5428 = CARTESIAN_POINT ( 'NONE',  ( 2.000000000000001776, -6.812627895098285258, 2.855765430652664971 ) ) ;
#5429 = CIRCLE ( 'NONE', #30887, 5.000000000000000000 ) ;
#5430 = ORIENTED_EDGE ( 'NONE', *, *, #41512, .T. ) ;
#5431 = EDGE_CURVE ( 'NONE', #14694, #21888, #14949, .T. ) ;
#5432 = PLANE ( 'NONE',  #1053 ) ;
#5433 = CARTESIAN_POINT ( 'NONE',  ( -35.00000000000000000, -0.7214809346827719683, -11.72397916322013245 ) ) ;
#5434 = CARTESIAN_POINT ( 'NONE',  ( 37.00000000000000711, -6.018036132182079889, 11.24036214326526562 ) ) ;
#5435 = EDGE_CURVE ( 'NONE', #53566, #52362, #57467, .T. ) ;
#5436 = EDGE_LOOP ( 'NONE', ( #40708, #37368, #33934, #63030 ) ) ;
#5437 = DIRECTION ( 'NONE',  ( 0.000000000000000000, 0.000000000000000000, 1.000000000000000000 ) ) ;
#5438 = EDGE_CURVE ( 'NONE', #16210, #13952, #54282, .T. ) ;
#5439 = VECTOR ( 'NONE', #19044, 1000.000000000000114 ) ;
#5440 = CIRCLE ( 'NONE', #29796, 4.999999999999999112 ) ;
#5441 = ADVANCED_FACE ( 'NONE', ( #38813 ), #8224, .F. ) ;
#5443 = ADVANCED_FACE ( 'NONE', ( #18859 ), #22355, .T. ) ;
#5442 = AXIS2_PLACEMENT_3D ( 'NONE', #55382, #30112, #4860 ) ;
#5444 =( BOUNDED_CURVE ( )  B_SPLINE_CURVE ( 3, ( #13359, #33646, #12044, #17378 ),
 .UNSPECIFIED., .F., .F. ) 
 B_SPLINE_CURVE_WITH_KNOTS ( ( 4, 4 ),
 ( 4.547159998450355900, 4.564492336233753278 ),
 .UNSPECIFIED. ) 
 CURVE ( )  GEOMETRIC_REPRESENTATION_ITEM ( )  RATIONAL_B_SPLINE_CURVE ( ( 1.000000000000000000, 0.9999749659955903258, 0.9999749659955903258, 1.000000000000000000 ) ) 
 REPRESENTATION_ITEM ( '' )  );
#5445 = CYLINDRICAL_SURFACE ( 'NONE', #14976, 4.999999999999999112 ) ;
#5446 = CIRCLE ( 'NONE', #28782, 12.18650000000000055 ) ;
#5447 = EDGE_CURVE ( 'NONE', #27171, #9320, #64079, .T. ) ;
#5448 = CARTESIAN_POINT ( 'NONE',  ( -35.00000000000000000, 11.17622378668011685, -3.614449339633368119 ) ) ;
#5449 = CARTESIAN_POINT ( 'NONE',  ( 2.889800649504073782, 4.732281052280366218, -3.882893708501999885 ) ) ;
#5450 = ORIENTED_EDGE ( 'NONE', *, *, #62567, .F. ) ;
#5451 = DIRECTION ( 'NONE',  ( 0.000000000000000000, 0.01356324068817998940, -0.9999080150203990547 ) ) ;
#5452 = DIRECTION ( 'NONE',  ( 0.3865475372811021937, 0.6075346789811209014, -0.6938894834606021966 ) ) ;
#5453 = CARTESIAN_POINT ( 'NONE',  ( 1.719304012339893051, -12.70777170743897422, -0.7661785589590540679 ) ) ;
#5454 = AXIS2_PLACEMENT_3D ( 'NONE', #6560, #51786, #6229 ) ;
#5455 = CARTESIAN_POINT ( 'NONE',  ( -27.19357181888462094, 25.00000000000000000, 5.138615876886901468 ) ) ;
#5456 = CARTESIAN_POINT ( 'NONE',  ( 0.000000000000000000, 1.779948802829910193, -6.576141558201243242 ) ) ;
#5457 = AXIS2_PLACEMENT_3D ( 'NONE', #2732, #22663, #37937 ) ;
#5458 = ORIENTED_EDGE ( 'NONE', *, *, #50357, .T. ) ;
#5459 =( BOUNDED_SURFACE ( )  B_SPLINE_SURFACE ( 3, 1, ( 
 ( #24923, #35842 ),
 ( #55166, #20592 ),
 ( #10263, #65774 ),
 ( #4972, #40868 ) ),
 .UNSPECIFIED., .F., .F., .F. ) 
 B_SPLINE_SURFACE_WITH_KNOTS ( ( 4, 4 ),
 ( 2, 2 ),
 ( 0.000000000000000000, 1.000000000000000000 ),
 ( 0.000000000000000000, 1.000000000000000000 ),
 .UNSPECIFIED. ) 
 GEOMETRIC_REPRESENTATION_ITEM ( )  RATIONAL_B_SPLINE_SURFACE ( (
 ( 1.000000000000000000, 1.000000000000000000),
 ( 0.6933888150995267674, 0.9895912004443193632),
 ( 0.6933888150995267674, 0.9895912004443193632),
 ( 1.000000000000000000, 1.000000000000000000) ) ) 
 REPRESENTATION_ITEM ( '' )  SURFACE ( )  );
#5460 = LINE ( 'NONE', #63251, #16223 ) ;
#5461 = CARTESIAN_POINT ( 'NONE',  ( 1.000000000000000888, -7.248432822490255667, 1.926193556692974429 ) ) ;
#5462 = CARTESIAN_POINT ( 'NONE',  ( -22.28415773361650309, 3.565377603762382108, -0.9981933716384956412 ) ) ;
#5463 = VERTEX_POINT ( 'NONE', #18561 ) ;
#5464 = CARTESIAN_POINT ( 'NONE',  ( 2.263328370261531663, -6.545781832005213907, 3.943189046766310213 ) ) ;
#5465 = AXIS2_PLACEMENT_3D ( 'NONE', #2850, #63010, #23109 ) ;
#5466 = CARTESIAN_POINT ( 'NONE',  ( 2.000000000000001776, 0.000000000000000000, 0.000000000000000000 ) ) ;
#5467 = EDGE_LOOP ( 'NONE', ( #31384, #55400, #57620, #22218 ) ) ;
#5468 = ORIENTED_EDGE ( 'NONE', *, *, #30287, .T. ) ;
#5469 = EDGE_LOOP ( 'NONE', ( #34415, #53575, #14295, #46360, #24275, #32953, #63104, #30932, #26037, #30852, #39708, #34775, #28048, #1088, #6110, #11929, #51609, #51790, #15018, #47170, #49594, #41111, #60627, #56449, #9267, #55526, #12707, #62761, #65333, #4820, #6437, #37804, #52289, #52245, #6691, #6662, #24756, #37032, #5993, #3249, #49660, #9529, #37534, #24678, #26274, #10519, #36822, #24634, #20118, #32559, #61475, #40950, #12251, #55104, #34347, #34884, #41993, #27796, #9534, #9830, #54822, #8695, #26749, #63070, #17139, #12597, #5967, #41778, #18055, #811, #46465, #17658, #15486, #22637, #38018, #32200, #59036, #38155, #6494, #58479, #52653, #53021, #51010, #41705, #48834, #21003, #9954, #21909, #23516, #4843, #64364, #56516, #39552, #32373, #64159, #25486, #43100, #24952, #4697, #18006, #43579, #20410, #37020, #59515, #53617, #25243, #36161, #24629, #34696, #22110, #55092, #25783, #59273, #35207, #54235, #13967, #21690, #52811, #11736, #52723, #59262, #63090, #36927, #65230, #45144, #17977, #26265, #58551, #46223, #40041, #10440, #33659, #65231, #36208, #2662, #54391, #62544, #63046, #42294, #45125, #63548, #34730, #24612, #15910, #17156, #31997, #56612, #17828, #43774, #53509, #13713, #22565, #10687, #38741, #42948, #15117, #28639, #20261, #53339, #14042, #43731, #30654, #862, #54916, #15644, #33082, #33896, #17668, #32059, #55663, #40045, #16410, #5580, #3455, #16172, #596, #54840, #54932, #13132, #36529, #48343, #33723, #26394, #11442, #6988, #58383, #7326, #33497, #17718, #23236, #27013, #52901, #10722, #46288, #56304, #46965, #19979, #55476, #64476, #20164, #51372, #57000, #30475, #51618, #4254, #35973, #7573, #65613, #20679, #16837, #27474, #15626, #54173, #50136, #37480, #21304, #45635, #12993, #8241, #27881, #60448, #47007, #26815, #45336, #15888, #59533, #7286, #54399, #11465, #44797, #26088, #54028, #51606, #10926, #54402, #13958, #23744 ) ) ;
#5470 = CIRCLE ( 'NONE', #137, 12.74999999999999822 ) ;
#5471 = EDGE_CURVE ( 'NONE', #62855, #35253, #59112, .T. ) ;
#5472 = VECTOR ( 'NONE', #10476, 1000.000000000000000 ) ;
#5473 = CIRCLE ( 'NONE', #37298, 4.500000000000000888 ) ;
#5474 = VERTEX_POINT ( 'NONE', #22878 ) ;
#5475 = CARTESIAN_POINT ( 'NONE',  ( 1.948354844647347983, 10.70340528294774529, 5.347695345040441417 ) ) ;
#5476 = CARTESIAN_POINT ( 'NONE',  ( 0.2652384529303112304, 6.065769141714355328, -10.63836770010960109 ) ) ;
#5477 = CARTESIAN_POINT ( 'NONE',  ( 2.000000000000001776, 6.812627895098307462, 0.04423456934733380197 ) ) ;
#5478 = CARTESIAN_POINT ( 'NONE',  ( 0.2653141334712560417, 4.147025708564583191, -11.52266042163702942 ) ) ;
#5479 = CARTESIAN_POINT ( 'NONE',  ( 37.00000000000000711, -2.865935305911543551, 12.42372387097884712 ) ) ;
#5480 = CARTESIAN_POINT ( 'NONE',  ( -9.974301738911194093, -29.01869747443698344, 8.904338584474110974 ) ) ;
#5481 = CARTESIAN_POINT ( 'NONE',  ( -35.00000000000000000, -6.102719229070750373, 10.54834585426218041 ) ) ;
#5483 = ORIENTED_EDGE ( 'NONE', *, *, #50683, .T. ) ;
#5482 = CARTESIAN_POINT ( 'NONE',  ( 0.3665391374699472626, 8.095513416941232165, 9.237363111276792438 ) ) ;
#5484 = CARTESIAN_POINT ( 'NONE',  ( 0.3675815128205912052, -11.44679196252406506, -4.447030445008294919 ) ) ;
#5485 = ORIENTED_EDGE ( 'NONE', *, *, #865, .T. ) ;
#5486 = DIRECTION ( 'NONE',  ( 0.000000000000000000, 0.000000000000000000, -1.000000000000000000 ) ) ;
#5487 = ORIENTED_EDGE ( 'NONE', *, *, #42795, .T. ) ;
#5488 = EDGE_CURVE ( 'NONE', #44279, #46540, #13522, .T. ) ;
#5489 = B_SPLINE_CURVE_WITH_KNOTS ( 'NONE', 3,
 ( #3414, #32321, #2072, #33317, #7059, #22341, #17709, #8062, #43956, #64230, #52942, #43604, #58265, #42609, #63897, #2421, #22698, #32628, #42962, #12686, #7725, #28012, #63555, #2766, #43278, #44929, #39278, #20311, #50593, #4384, #65211, #29310, #19985, #40255, #19346, #19681, #14008, #55576, #64539, #55232, #60222, #33959, #54607, #44268, #19012, #29961, #50267, #60543 ),
 .UNSPECIFIED., .F., .F.,
 ( 4, 2, 2, 2, 2, 2, 2, 2, 2, 2, 2, 2, 2, 2, 2, 2, 2, 2, 2, 2, 2, 2, 2, 4 ),
 ( 1.262897753262583006E-17, 0.001542731309856127829, 0.003085462619712243081, 0.004628193929568360718, 0.006170925239424478355, 0.009256387859136719701, 0.01234185047884896538, 0.01388458178870508909, 0.01542731309856121280, 0.01851277571827345328, 0.02005550702812957525, 0.02159823833798569723, 0.02468370095769793424, 0.02622643226755405621, 0.02776916357741017818, 0.03085462619712241866, 0.03394008881683466261, 0.03702555143654689962, 0.04011101405625914357, 0.04165374536611526207, 0.04319647667597138752, 0.04473920798582751296, 0.04628193929568363840, 0.04936740191539588929 ),
 .UNSPECIFIED. ) ;
#5490 = ORIENTED_EDGE ( 'NONE', *, *, #45293, .F. ) ;
#5491 = CARTESIAN_POINT ( 'NONE',  ( 0.2706063244538075008, 9.494160524941802848, -7.737788863017200924 ) ) ;
#5492 = AXIS2_PLACEMENT_3D ( 'NONE', #62696, #2554, #7859 ) ;
#5493 = CARTESIAN_POINT ( 'NONE',  ( 9.730232070128172595, -27.62176360438249390, 14.46115055101565972 ) ) ;
#5494 = CARTESIAN_POINT ( 'NONE',  ( 2.000000000000001776, 5.997115278587632936, 3.485633455389514523 ) ) ;
#5495 = CARTESIAN_POINT ( 'NONE',  ( 2.000000000000001776, -1.956810415765137368, -6.654767106875568494 ) ) ;
#5496 = DIRECTION ( 'NONE',  ( 0.000000000000000000, 0.01356324068817998940, -0.9999080150203990547 ) ) ;
#5498 = ORIENTED_EDGE ( 'NONE', *, *, #59713, .T. ) ;
#5497 = AXIS2_PLACEMENT_3D ( 'NONE', #64688, #50739, #54752 ) ;
#5499 = ORIENTED_EDGE ( 'NONE', *, *, #57282, .F. ) ;
#5500 = CARTESIAN_POINT ( 'NONE',  ( 0.3401186441510237191, 12.03768714635924830, 2.382124782498401316 ) ) ;
#5501 = EDGE_LOOP ( 'NONE', ( #50690, #58761, #38136, #1680 ) ) ;
#5502 = CIRCLE ( 'NONE', #22466, 5.000000000000000000 ) ;
#5503 = ADVANCED_FACE ( 'NONE', ( #8879 ), #54103, .F. ) ;
#5504 = ORIENTED_EDGE ( 'NONE', *, *, #14327, .T. ) ;
#5505 = VECTOR ( 'NONE', #56715, 1000.000000000000000 ) ;
#5506 = CARTESIAN_POINT ( 'NONE',  ( 5.516018279890452902, 0.006629829924290471695, -0.001397286410094441449 ) ) ;
#5507 = CARTESIAN_POINT ( 'NONE',  ( 1.459561108993335354, -10.62073135189157291, 6.861308540877669060 ) ) ;
#5508 = CARTESIAN_POINT ( 'NONE',  ( -37.00000000000000711, 12.63095688309031495, -1.738225594539862584 ) ) ;
#5509 = CARTESIAN_POINT ( 'NONE',  ( 1.372161826076379043, -12.30755118281447658, 2.769012792636629250 ) ) ;
#5510 = FACE_OUTER_BOUND ( 'NONE', #15434, .T. ) ;
#5511 = CYLINDRICAL_SURFACE ( 'NONE', #33097, 4.999999999999999112 ) ;
#5512 = CIRCLE ( 'NONE', #13978, 5.000000000000000888 ) ;
#5513 = ORIENTED_EDGE ( 'NONE', *, *, #48908, .F. ) ;
#5514 = VERTEX_POINT ( 'NONE', #29171 ) ;
#5515 = AXIS2_PLACEMENT_3D ( 'NONE', #64260, #39644, #9363 ) ;
#5516 = AXIS2_PLACEMENT_3D ( 'NONE', #5800, #6116, #46345 ) ;
#5517 = DIRECTION ( 'NONE',  ( 1.000000000000000000, 0.000000000000000000, 0.000000000000000000 ) ) ;
#5518 = CARTESIAN_POINT ( 'NONE',  ( -2.729227863478770111, -12.79029713166804250, 4.331329641846414447 ) ) ;
#5519 = EDGE_CURVE ( 'NONE', #62845, #15867, #39125, .T. ) ;
#5520 = AXIS2_PLACEMENT_3D ( 'NONE', #56752, #15810, #56391 ) ;
#5521 = AXIS2_PLACEMENT_3D ( 'NONE', #53514, #12265, #1661 ) ;
#5522 = CYLINDRICAL_SURFACE ( 'NONE', #33408, 4.999999999999999112 ) ;
#5523 = VECTOR ( 'NONE', #25385, 1000.000000000000000 ) ;
#5524 = CARTESIAN_POINT ( 'NONE',  ( 35.00000000000000000, 4.705694406421931860E-17, -3.469127814946512892E-15 ) ) ;
#5525 = EDGE_CURVE ( 'NONE', #24280, #25736, #8542, .T. ) ;
#5526 = CARTESIAN_POINT ( 'NONE',  ( 23.56735259781322611, 2.000748643224683487, -13.35387901052309800 ) ) ;
#5527 = CARTESIAN_POINT ( 'NONE',  ( 1.109979610372296310, 2.646302643133297217, -12.24510427445534511 ) ) ;
#5528 = EDGE_CURVE ( 'NONE', #40710, #19771, #60597, .T. ) ;
#5529 = CARTESIAN_POINT ( 'NONE',  ( 35.00000000000000000, 9.196955404009292678, -8.830544224262981245 ) ) ;
#5530 = ORIENTED_EDGE ( 'NONE', *, *, #58041, .F. ) ;
#5531 = CARTESIAN_POINT ( 'NONE',  ( 0.2648978790185584908, 10.53870023327863770, 6.237101853238585569 ) ) ;
#5532 = CARTESIAN_POINT ( 'NONE',  ( 35.00000000000000000, -7.238157050195554554, 10.49626516989278180 ) ) ;
#5533 = CIRCLE ( 'NONE', #48010, 5.000000000000000888 ) ;
#5534 = CIRCLE ( 'NONE', #7655, 4.999999999999999112 ) ;
#5535 = CIRCLE ( 'NONE', #14007, 2.899999999999995026 ) ;
#5536 = CARTESIAN_POINT ( 'NONE',  ( 2.000000000000001776, 3.224464355699842688, 6.771471746881975839 ) ) ;
#5537 = CARTESIAN_POINT ( 'NONE',  ( 35.00000000000000000, -10.54834585426224258, -6.102719229070642903 ) ) ;
#5538 = VERTEX_POINT ( 'NONE', #32813 ) ;
#5539 = CARTESIAN_POINT ( 'NONE',  ( -27.15511094194037511, -2.237231637349085034, -1.124668417986079527 ) ) ;
#5540 = CARTESIAN_POINT ( 'NONE',  ( 2.000000000000001776, 4.409940824963509698, -5.354199675985237050 ) ) ;
#5541 = AXIS2_PLACEMENT_3D ( 'NONE', #56932, #16354, #16992 ) ;
#5542 = CARTESIAN_POINT ( 'NONE',  ( 19.56743653832047869, -28.99999999999999289, -4.999999999999984901 ) ) ;
#5543 = EDGE_LOOP ( 'NONE', ( #63570, #57890, #34012, #51648 ) ) ;
#5544 = CARTESIAN_POINT ( 'NONE',  ( 19.28625800530496903, 6.413918128308424116, 11.87904264843580471 ) ) ;
#5545 = CYLINDRICAL_SURFACE ( 'NONE', #43773, 12.75000000000000178 ) ;
#5546 = DIRECTION ( 'NONE',  ( 0.000000000000000000, -0.07632122047555053856, 0.9970832820307050648 ) ) ;
#5547 = AXIS2_PLACEMENT_3D ( 'NONE', #3305, #42863, #34189 ) ;
#5549 = VERTEX_POINT ( 'NONE', #53122 ) ;
#5548 = DIRECTION ( 'NONE',  ( 1.000000000000000000, 0.000000000000000000, -0.000000000000000000 ) ) ;
#5550 = CARTESIAN_POINT ( 'NONE',  ( -35.00000000000000000, 0.7536123767500182424, -11.72195762423409171 ) ) ;
#5551 = EDGE_CURVE ( 'NONE', #17913, #10194, #42362, .T. ) ;
#5552 = DIRECTION ( 'NONE',  ( -1.000000000000000000, 0.000000000000000000, 0.000000000000000000 ) ) ;
#5553 = ORIENTED_EDGE ( 'NONE', *, *, #54999, .F. ) ;
#5554 = PLANE ( 'NONE',  #38681 ) ;
#5555 = EDGE_CURVE ( 'NONE', #57223, #61328, #13715, .T. ) ;
#5556 = CARTESIAN_POINT ( 'NONE',  ( -27.08429572838383947, 1.338867938658203860, 1.859677275556406384 ) ) ;
#5557 = CARTESIAN_POINT ( 'NONE',  ( 0.2650492433740052611, -7.786978278830034128, 9.451472485870532125 ) ) ;
#5558 = FACE_OUTER_BOUND ( 'NONE', #11866, .T. ) ;
#5559 = DIRECTION ( 'NONE',  ( 0.000000000000000000, -0.01356324068817991481, 0.9999080150203990547 ) ) ;
#5560 = CARTESIAN_POINT ( 'NONE',  ( 2.241536586108912488, 2.605228657247447899, -7.176205604390183623 ) ) ;
#5561 = DIRECTION ( 'NONE',  ( 1.000000000000000000, 0.000000000000000000, 0.000000000000000000 ) ) ;
#5562 = ORIENTED_EDGE ( 'NONE', *, *, #46172, .T. ) ;
#5563 = LINE ( 'NONE', #25832, #54422 ) ;
#5564 = ORIENTED_EDGE ( 'NONE', *, *, #16681, .F. ) ;
#5565 = EDGE_CURVE ( 'NONE', #20378, #32446, #965, .T. ) ;
#5566 = CARTESIAN_POINT ( 'NONE',  ( -35.00000000000000000, -5.927257550915394191, 10.64792938439753378 ) ) ;
#5568 = CARTESIAN_POINT ( 'NONE',  ( 0.3537226245948361103, 11.44347094181051894, 4.442821955543838186 ) ) ;
#5567 = VECTOR ( 'NONE', #17027, 999.9999999999998863 ) ;
#5569 = VECTOR ( 'NONE', #49516, 1000.000000000000114 ) ;
#5570 = DIRECTION ( 'NONE',  ( 0.000000000000000000, 0.01356324068818000848, -0.9999080150203990547 ) ) ;
#5571 = ORIENTED_EDGE ( 'NONE', *, *, #51224, .T. ) ;
#5572 = DIRECTION ( 'NONE',  ( -0.000000000000000000, -1.000000000000000000, -0.000000000000000000 ) ) ;
#5573 = CYLINDRICAL_SURFACE ( 'NONE', #61342, 6.936499999999988120 ) ;
#5574 = CARTESIAN_POINT ( 'NONE',  ( -22.27706485742869091, -0.9832726768967594566, 3.547445275915920071 ) ) ;
#5575 = ORIENTED_EDGE ( 'NONE', *, *, #32647, .F. ) ;
#5576 = EDGE_LOOP ( 'NONE', ( #56015, #24769, #57051, #49544 ) ) ;
#5577 = CARTESIAN_POINT ( 'NONE',  ( 2.244591118396556784, -7.211060161907631105, -2.510215291309289665 ) ) ;
#5578 = EDGE_CURVE ( 'NONE', #46169, #15877, #33500, .T. ) ;
#5579 = EDGE_CURVE ( 'NONE', #34891, #9460, #32784, .T. ) ;
#5580 = ORIENTED_EDGE ( 'NONE', *, *, #59895, .F. ) ;
#5581 = CARTESIAN_POINT ( 'NONE',  ( -36.00000000000000711, 1.113475361586489631, 12.70128625845193326 ) ) ;
#5582 = DIRECTION ( 'NONE',  ( -1.000000000000000000, 0.000000000000000000, -0.000000000000000000 ) ) ;
#5583 = VECTOR ( 'NONE', #2194, 1000.000000000000000 ) ;
#5584 = CARTESIAN_POINT ( 'NONE',  ( -27.10719052120871098, 2.355164825213508450, -0.1538293304135275597 ) ) ;
#5585 = EDGE_CURVE ( 'NONE', #27385, #33979, #64391, .T. ) ;
#5586 = CARTESIAN_POINT ( 'NONE',  ( 2.244591118396559448, 7.137527852925285465, -2.712243649838633530 ) ) ;
#5587 = AXIS2_PLACEMENT_3D ( 'NONE', #4560, #40096, #8878 ) ;
#5588 = DIRECTION ( 'NONE',  ( -1.000000000000000000, 0.000000000000000000, 0.000000000000000000 ) ) ;
#5589 = CARTESIAN_POINT ( 'NONE',  ( 0.2650492594609250019, -10.66007682546621282, 6.027447650185331796 ) ) ;
#5590 = CARTESIAN_POINT ( 'NONE',  ( -4.590058209962335489, 6.612760447609789871, 25.00000000000000000 ) ) ;
#5591 = ORIENTED_EDGE ( 'NONE', *, *, #3804, .T. ) ;
#5592 = AXIS2_PLACEMENT_3D ( 'NONE', #42322, #36709, #52354 ) ;
#5593 = FACE_OUTER_BOUND ( 'NONE', #19161, .T. ) ;
#5594 = AXIS2_PLACEMENT_3D ( 'NONE', #30487, #34801, #9881 ) ;
#5595 = CARTESIAN_POINT ( 'NONE',  ( -37.00000000000000711, 0.000000000000000000, 0.000000000000000000 ) ) ;
#5596 = CARTESIAN_POINT ( 'NONE',  ( -35.00000000000000000, 2.216820770815248309, -11.53507381115581332 ) ) ;
#5597 = FACE_OUTER_BOUND ( 'NONE', #12326, .T. ) ;
#5598 = DIRECTION ( 'NONE',  ( -1.000000000000000000, 0.000000000000000000, 0.000000000000000000 ) ) ;
#5599 = CARTESIAN_POINT ( 'NONE',  ( 0.2958664285830420737, -10.72286791615085022, -5.936220506376345796 ) ) ;
#5600 = LINE ( 'NONE', #42681, #61064 ) ;
#5601 = FACE_OUTER_BOUND ( 'NONE', #23803, .T. ) ;
#5602 = ADVANCED_FACE ( 'NONE', ( #10795 ), #62005, .T. ) ;
#5603 = ORIENTED_EDGE ( 'NONE', *, *, #51532, .T. ) ;
#5604 = DIRECTION ( 'NONE',  ( -1.000000000000000000, 0.000000000000000000, 0.000000000000000000 ) ) ;
#5605 = ADVANCED_FACE ( 'NONE', ( #21095 ), #17095, .T. ) ;
#5606 = AXIS2_PLACEMENT_3D ( 'NONE', #61499, #41214, #56535 ) ;
#5607 = ORIENTED_EDGE ( 'NONE', *, *, #57749, .F. ) ;
#5608 = CARTESIAN_POINT ( 'NONE',  ( -22.28482751661422512, -3.692400780723923415, 0.2989970708918304743 ) ) ;
#5609 = CARTESIAN_POINT ( 'NONE',  ( 0.2646305136544072623, -0.1321451301296985015, -12.24595685781654808 ) ) ;
#5610 = CARTESIAN_POINT ( 'NONE',  ( 0.2653141617320999290, -12.06772699408310423, 2.083144498805234335 ) ) ;
#5611 = CARTESIAN_POINT ( 'NONE',  ( 2.305787727787084407, 2.461236246751170142, -7.249469779319884566 ) ) ;
#5612 = ORIENTED_EDGE ( 'NONE', *, *, #45559, .T. ) ;
#5613 = CIRCLE ( 'NONE', #31229, 12.74999999999999822 ) ;
#5614 = CARTESIAN_POINT ( 'NONE',  ( 26.34661844826604593, 25.00000000000000000, 3.317828791472333005 ) ) ;
#5615 = DIRECTION ( 'NONE',  ( 1.000000000000000000, 0.000000000000000000, 0.000000000000000000 ) ) ;
#5616 = AXIS2_PLACEMENT_3D ( 'NONE', #48575, #49875, #64183 ) ;
#5617 = CARTESIAN_POINT ( 'NONE',  ( 3.092491956585937452, -0.9322768171840393192, 7.863103788722447973 ) ) ;
#5618 = CARTESIAN_POINT ( 'NONE',  ( -37.00000000000000711, 12.21925492305362049, 3.640372113593595582 ) ) ;
#5619 = CIRCLE ( 'NONE', #44898, 12.75000000000000178 ) ;
#5620 = LINE ( 'NONE', #13679, #29884 ) ;
#5621 = DIRECTION ( 'NONE',  ( 0.000000000000000000, -1.000000000000000000, 0.000000000000000000 ) ) ;
#5622 = ORIENTED_EDGE ( 'NONE', *, *, #40016, .F. ) ;
#5623 = CARTESIAN_POINT ( 'NONE',  ( -27.08588607604449194, -0.5840042213184938324, 2.220764381377819952 ) ) ;
#5624 = VERTEX_POINT ( 'NONE', #513 ) ;
#5625 = CARTESIAN_POINT ( 'NONE',  ( -35.00000000000000000, 0.000000000000000000, 0.000000000000000000 ) ) ;
#5626 = FACE_OUTER_BOUND ( 'NONE', #43588, .T. ) ;
#5627 = AXIS2_PLACEMENT_3D ( 'NONE', #12119, #37052, #22099 ) ;
#5628 = DIRECTION ( 'NONE',  ( 1.000000000000000000, 0.000000000000000000, 0.000000000000000000 ) ) ;
#5629 = CARTESIAN_POINT ( 'NONE',  ( -7.756689557399197632, -2.159283824347104641, 11.80546050376997869 ) ) ;
#5630 = VECTOR ( 'NONE', #35538, 1000.000000000000114 ) ;
#5631 = ORIENTED_EDGE ( 'NONE', *, *, #34760, .T. ) ;
#5632 = ORIENTED_EDGE ( 'NONE', *, *, #37503, .F. ) ;
#5633 = DIRECTION ( 'NONE',  ( 0.000000000000000000, 0.000000000000000000, 1.000000000000000000 ) ) ;
#5634 = VERTEX_POINT ( 'NONE', #11138 ) ;
#5635 = EDGE_CURVE ( 'NONE', #31395, #924, #43425, .T. ) ;
#5636 = CARTESIAN_POINT ( 'NONE',  ( 2.251139882113958546, -6.551456272498873190, -3.925854078924290391 ) ) ;
#5637 = DIRECTION ( 'NONE',  ( 0.000000000000000000, -0.9985334138511243740, 0.05413890858540761075 ) ) ;
#5638 = CARTESIAN_POINT ( 'NONE',  ( -22.27720387087364884, -3.430312021254878552, -1.337073746937890828 ) ) ;
#5639 = DIRECTION ( 'NONE',  ( 0.000000000000000000, 0.01356324068817998940, -0.9999080150203989437 ) ) ;
#5640 = DIRECTION ( 'NONE',  ( -1.000000000000000000, 0.000000000000000000, 0.000000000000000000 ) ) ;
#5641 = AXIS2_PLACEMENT_3D ( 'NONE', #30010, #20365, #56260 ) ;
#5642 = CARTESIAN_POINT ( 'NONE',  ( 1.549075743846936026, 11.29795072957594648, -5.743768701986331493 ) ) ;
#5643 = CARTESIAN_POINT ( 'NONE',  ( -9.410738856732004720, -2.781742255745475401, 11.67413128860836302 ) ) ;
#5644 = VERTEX_POINT ( 'NONE', #27081 ) ;
#5645 = CARTESIAN_POINT ( 'NONE',  ( 2.440552418640498988, -2.447453236303777313, -7.301551120181787979 ) ) ;
#5646 = ORIENTED_EDGE ( 'NONE', *, *, #62566, .F. ) ;
#5647 = CARTESIAN_POINT ( 'NONE',  ( -22.27719443589224113, 2.462030382548443974, 2.737335337013082182 ) ) ;
#5648 = CARTESIAN_POINT ( 'NONE',  ( 0.3218525148189825269, 10.49750909897053042, 6.342972338926835540 ) ) ;
#5649 = DIRECTION ( 'NONE',  ( 0.000000000000000000, 0.01356324068817998940, -0.9999080150203990547 ) ) ;
#5650 = EDGE_CURVE ( 'NONE', #63127, #43263, #47047, .T. ) ;
#5651 = VERTEX_POINT ( 'NONE', #31413 ) ;
#5652 = CARTESIAN_POINT ( 'NONE',  ( 2.990245332647884613, -5.049055049623163427, -6.814589384235021363 ) ) ;
#5653 = ORIENTED_EDGE ( 'NONE', *, *, #45519, .T. ) ;
#5654 = LINE ( 'NONE', #40885, #19494 ) ;
#5655 =( BOUNDED_CURVE ( )  B_SPLINE_CURVE ( 3, ( #10028, #59925, #19691, #34936 ),
 .UNSPECIFIED., .F., .F. ) 
 B_SPLINE_CURVE_WITH_KNOTS ( ( 4, 4 ),
 ( 2.276420903748625602, 2.328873244820985899 ),
 .UNSPECIFIED. ) 
 CURVE ( )  GEOMETRIC_REPRESENTATION_ITEM ( )  RATIONAL_B_SPLINE_CURVE ( ( 1.000000000000000000, 0.9997707424672948040, 0.9997707424672948040, 1.000000000000000000 ) ) 
 REPRESENTATION_ITEM ( '' )  );
#5656 = CARTESIAN_POINT ( 'NONE',  ( 6.582987406907342631, -7.685813705153371700, -11.10488467197773232 ) ) ;
#5657 = CARTESIAN_POINT ( 'NONE',  ( -36.00000000000000711, 10.39746860227890757, 7.379373053628905943 ) ) ;
#5658 = CARTESIAN_POINT ( 'NONE',  ( -48.45393016956177235, -0.3105270330721054961, 5.105971556042225856 ) ) ;
#5659 = ORIENTED_EDGE ( 'NONE', *, *, #65673, .T. ) ;
#5660 = ORIENTED_EDGE ( 'NONE', *, *, #57551, .T. ) ;
#5661 = CARTESIAN_POINT ( 'NONE',  ( -35.00000000000000000, -0.8294751490780184477, 12.15823808070322443 ) ) ;
#5662 = ORIENTED_EDGE ( 'NONE', *, *, #34401, .T. ) ;
#5663 = DIRECTION ( 'NONE',  ( 1.000000000000000000, 0.000000000000000000, 0.000000000000000000 ) ) ;
#5664 = ORIENTED_EDGE ( 'NONE', *, *, #32779, .F. ) ;
#5665 = AXIS2_PLACEMENT_3D ( 'NONE', #36266, #25644, #56569 ) ;
#5666 = CIRCLE ( 'NONE', #42790, 4.999999999999999112 ) ;
#5667 = ORIENTED_EDGE ( 'NONE', *, *, #56920, .T. ) ;
#5668 = ORIENTED_EDGE ( 'NONE', *, *, #35610, .F. ) ;
#5669 = LINE ( 'NONE', #35232, #29870 ) ;
#5670 = CARTESIAN_POINT ( 'NONE',  ( 1.462291587748162813, 11.65117843858566893, 4.914320681884643882 ) ) ;
#5671 = AXIS2_PLACEMENT_3D ( 'NONE', #42901, #57226, #7006 ) ;
#5672 = CARTESIAN_POINT ( 'NONE',  ( 5.514970785353741078, -0.001117786416802585238, -0.004588761610585022008 ) ) ;
#5673 = CARTESIAN_POINT ( 'NONE',  ( 2.290907136833252089, 2.768669624188787814, -7.132394668149358630 ) ) ;
#5674 = CARTESIAN_POINT ( 'NONE',  ( -37.00000000000000711, 0.000000000000000000, 0.000000000000000000 ) ) ;
#5675 = VERTEX_POINT ( 'NONE', #56710 ) ;
#5676 = CARTESIAN_POINT ( 'NONE',  ( 2.253265082352140514, -2.491579069691978621, -7.220580418433788061 ) ) ;
#5677 = ORIENTED_EDGE ( 'NONE', *, *, #9156, .T. ) ;
#5678 = LINE ( 'NONE', #27242, #3083 ) ;
#5679 = B_SPLINE_CURVE_WITH_KNOTS ( 'NONE', 3,
 ( #37249, #43220, #52578, #47568, #1375, #36608, #22281, #42548, #62852, #57896, #56912, #12304, #52881, #7313, #22634, #33902 ),
 .UNSPECIFIED., .F., .F.,
 ( 4, 3, 3, 3, 3, 4 ),
 ( 5.963111948670274387E-19, 0.0003017745587525298007, 0.0006035491769808827393, 0.0009053241094668298006, 0.001207275924539980873, 0.001510325902532946895 ),
 .UNSPECIFIED. ) ;
#5681 = DIRECTION ( 'NONE',  ( 0.000000000000000000, 0.000000000000000000, 1.000000000000000000 ) ) ;
#5680 = AXIS2_PLACEMENT_3D ( 'NONE', #51643, #51318, #10388 ) ;
#5682 = CARTESIAN_POINT ( 'NONE',  ( 37.00000000000000711, 4.705694406421931860E-17, -3.469127814946512892E-15 ) ) ;
#5683 = CARTESIAN_POINT ( 'NONE',  ( -27.27811836728105632, 13.23177170242203537, -2.726413120567312109 ) ) ;
#5684 = AXIS2_PLACEMENT_3D ( 'NONE', #33571, #28568, #37578 ) ;
#5685 = CARTESIAN_POINT ( 'NONE',  ( 28.79300809604977474, 9.772829246361629529, 6.977156320580031768 ) ) ;
#5686 = DIRECTION ( 'NONE',  ( 0.000000000000000000, -1.000000000000000000, 0.000000000000000000 ) ) ;
#5687 = EDGE_CURVE ( 'NONE', #48764, #22402, #57267, .T. ) ;
#5688 = AXIS2_PLACEMENT_3D ( 'NONE', #12545, #32823, #53133 ) ;
#5689 = ORIENTED_EDGE ( 'NONE', *, *, #53219, .F. ) ;
#5690 = DIRECTION ( 'NONE',  ( 1.000000000000000000, 0.000000000000000000, 0.000000000000000000 ) ) ;
#5691 = ORIENTED_EDGE ( 'NONE', *, *, #19251, .T. ) ;
#5692 = CARTESIAN_POINT ( 'NONE',  ( -37.25000000000000711, -27.21021009056489248, -4.500000000000000888 ) ) ;
#5693 = AXIS2_PLACEMENT_3D ( 'NONE', #64210, #59227, #24290 ) ;
#5694 = DIRECTION ( 'NONE',  ( 0.9688695217174486674, 5.204170427930422072E-15, -0.2475719085175099865 ) ) ;
#5695 = CARTESIAN_POINT ( 'NONE',  ( 2.255723233588630805, -3.704537245405363777, -6.680843247642031635 ) ) ;
#5696 = DIRECTION ( 'NONE',  ( 0.000000000000000000, -0.01356324068817998940, 0.9999080150203990547 ) ) ;
#5697 = ORIENTED_EDGE ( 'NONE', *, *, #32702, .T. ) ;
#5698 = CARTESIAN_POINT ( 'NONE',  ( 1.719304012341582588, 5.690355757825640737, -11.38834240361563488 ) ) ;
#5699 = DIRECTION ( 'NONE',  ( 1.000000000000000000, 0.000000000000000000, 0.000000000000000000 ) ) ;
#5700 = FACE_BOUND ( 'NONE', #30657, .T. ) ;
#5701 = CARTESIAN_POINT ( 'NONE',  ( 22.11934408877570135, -13.40694460789532449, -1.623494447580545952 ) ) ;
#5702 = EDGE_CURVE ( 'NONE', #40383, #61423, #31743, .T. ) ;
#5703 = AXIS2_PLACEMENT_3D ( 'NONE', #44405, #64687, #45402 ) ;
#5704 = FACE_OUTER_BOUND ( 'NONE', #6821, .T. ) ;
#5705 = CARTESIAN_POINT ( 'NONE',  ( -35.00000000000000000, 8.258652103341553641, -8.352657516904583801 ) ) ;
#5706 = CARTESIAN_POINT ( 'NONE',  ( -37.00000000000000711, -11.81949347079749302, 2.968224442958360410 ) ) ;
#5707 = CARTESIAN_POINT ( 'NONE',  ( 1.452237505248555660, 12.55261342181975515, 1.611965288198772717 ) ) ;
#5708 = CARTESIAN_POINT ( 'NONE',  ( 2.241311220309554209, 0.09281826062106607322, -7.633829235838274663 ) ) ;
#5709 = CIRCLE ( 'NONE', #21649, 6.936499999999990784 ) ;
#5710 = VECTOR ( 'NONE', #3422, 1000.000000000000000 ) ;
#5711 = ORIENTED_EDGE ( 'NONE', *, *, #5734, .T. ) ;
#5713 = ORIENTED_EDGE ( 'NONE', *, *, #49684, .F. ) ;
#5712 = EDGE_CURVE ( 'NONE', #29524, #18956, #26442, .T. ) ;
#5714 = CARTESIAN_POINT ( 'NONE',  ( 5.514970785353741078, -0.001897634820904983786, -0.004324946436530298539 ) ) ;
#5715 = CARTESIAN_POINT ( 'NONE',  ( 46.51586683006346590, -0.6857498399870713968, -10.66240463596387400 ) ) ;
#5716 = CYLINDRICAL_SURFACE ( 'NONE', #34302, 4.999999999999999112 ) ;
#5717 = CIRCLE ( 'NONE', #16335, 12.18649999999999878 ) ;
#5718 = CARTESIAN_POINT ( 'NONE',  ( 0.2648978790185619880, -1.996248716311710414, 12.08224454301447892 ) ) ;
#5719 = ADVANCED_FACE ( 'NONE', ( #36047 ), #36725, .T. ) ;
#5720 = ORIENTED_EDGE ( 'NONE', *, *, #15803, .F. ) ;
#5721 = CIRCLE ( 'NONE', #24831, 12.75000000000000178 ) ;
#5722 = VERTEX_POINT ( 'NONE', #31718 ) ;
#5723 = ORIENTED_EDGE ( 'NONE', *, *, #35881, .F. ) ;
#5724 = DIRECTION ( 'NONE',  ( 0.000000000000000000, -0.7790879021242441693, 0.6269146997508066033 ) ) ;
#5725 = AXIS2_PLACEMENT_3D ( 'NONE', #488, #41681, #35694 ) ;
#5726 = DIRECTION ( 'NONE',  ( 1.000000000000000000, 0.000000000000000000, 0.000000000000000000 ) ) ;
#5727 = EDGE_CURVE ( 'NONE', #62996, #52558, #51712, .T. ) ;
#5728 = VERTEX_POINT ( 'NONE', #825 ) ;
#5729 = CARTESIAN_POINT ( 'NONE',  ( -16.98800322446194855, 2.922502605998049674, -11.63868456991314027 ) ) ;
#5730 = CARTESIAN_POINT ( 'NONE',  ( 2.000000000000001776, -0.4129979343797593461, 6.800241778083677247 ) ) ;
#5731 = ORIENTED_EDGE ( 'NONE', *, *, #3226, .F. ) ;
#5732 = AXIS2_PLACEMENT_3D ( 'NONE', #34325, #49633, #29646 ) ;
#5733 = CARTESIAN_POINT ( 'NONE',  ( 2.247112776671929879, 4.818685025479959805, -5.923998863713823226 ) ) ;
#5734 = EDGE_CURVE ( 'NONE', #56025, #64706, #61332, .T. ) ;
#5735 = CARTESIAN_POINT ( 'NONE',  ( 7.125164966884262263, -31.43290117443645926, -14.16047883281914110 ) ) ;
#5736 = CARTESIAN_POINT ( 'NONE',  ( 5.514970785353741078, 0.004713149585127261558, 0.0003039746380524470729 ) ) ;
#5737 = ORIENTED_EDGE ( 'NONE', *, *, #7429, .T. ) ;
#5738 = LINE ( 'NONE', #55614, #16151 ) ;
#5739 = EDGE_LOOP ( 'NONE', ( #4009, #36151, #35383, #49915 ) ) ;
#5740 = EDGE_CURVE ( 'NONE', #60025, #9428, #48772, .T. ) ;
#5741 = CARTESIAN_POINT ( 'NONE',  ( -14.29135464769095520, 7.782112657557433977, 11.03126115115966499 ) ) ;
#5742 = ORIENTED_EDGE ( 'NONE', *, *, #47744, .T. ) ;
#5743 = CARTESIAN_POINT ( 'NONE',  ( -17.64665465971367553, -7.710886870156880235, 11.08500766144072891 ) ) ;
#5744 = DIRECTION ( 'NONE',  ( 1.000000000000000000, -0.000000000000000000, 0.000000000000000000 ) ) ;
#5745 = CARTESIAN_POINT ( 'NONE',  ( 2.251152103363644574, 3.926807817126193090, 6.550893877460167047 ) ) ;
#5746 = DIRECTION ( 'NONE',  ( 0.000000000000000000, -0.01356324068817992175, 0.9999080150203990547 ) ) ;
#5747 = AXIS2_PLACEMENT_3D ( 'NONE', #36547, #7252, #62785 ) ;
#5748 = CARTESIAN_POINT ( 'NONE',  ( 0.2872850955227750913, -12.25172867346922878, 0.2089153415334442931 ) ) ;
#5749 = CARTESIAN_POINT ( 'NONE',  ( 8.459648224137296779, 3.953564174085363092, 11.33341040866371863 ) ) ;
#5750 = CARTESIAN_POINT ( 'NONE',  ( -27.08429572838383947, 2.279961732801592422, -0.2296550094122856711 ) ) ;
#5751 = LINE ( 'NONE', #26656, #64956 ) ;
#5753 = ORIENTED_EDGE ( 'NONE', *, *, #32219, .F. ) ;
#5752 = CARTESIAN_POINT ( 'NONE',  ( -18.45105770001609713, 4.180413819594255287, -12.83901097965013349 ) ) ;
#5754 = EDGE_CURVE ( 'NONE', #25736, #49400, #58252, .T. ) ;
#5755 = DIRECTION ( 'NONE',  ( 0.000000000000000000, 0.000000000000000000, 1.000000000000000000 ) ) ;
#5756 = ORIENTED_EDGE ( 'NONE', *, *, #3921, .T. ) ;
#5757 = DIRECTION ( 'NONE',  ( 0.000000000000000000, 0.000000000000000000, 1.000000000000000000 ) ) ;
#5758 = CARTESIAN_POINT ( 'NONE',  ( 2.770579946183337583, -5.784075095088754281, -5.249166435139423825 ) ) ;
#5759 = AXIS2_PLACEMENT_3D ( 'NONE', #27581, #62831, #2339 ) ;
#5760 = ORIENTED_EDGE ( 'NONE', *, *, #865, .F. ) ;
#5762 = AXIS2_PLACEMENT_3D ( 'NONE', #10250, #25896, #30530 ) ;
#5761 = CARTESIAN_POINT ( 'NONE',  ( 0.3341166715381256869, 8.078283863465498982, 9.234320413907830982 ) ) ;
#5763 = CARTESIAN_POINT ( 'NONE',  ( 0.4626703367448859461, 11.66326339726757766, -3.943760108616669591 ) ) ;
#5764 = CARTESIAN_POINT ( 'NONE',  ( 0.2653141617321022605, -9.352766656400001821, -7.905395731875590748 ) ) ;
#5765 = CARTESIAN_POINT ( 'NONE',  ( 2.000000000000001776, 2.469490258309423591, 6.482025155313315246 ) ) ;
#5766 = CIRCLE ( 'NONE', #39573, 7.938172270156617749 ) ;
#5767 = CARTESIAN_POINT ( 'NONE',  ( 3.291290029914074378, 8.250315036047103590, -10.68561190601526079 ) ) ;
#5768 = ORIENTED_EDGE ( 'NONE', *, *, #23033, .F. ) ;
#5769 = CARTESIAN_POINT ( 'NONE',  ( -17.83419946441818027, -9.720786832536937538, -7.036071585506806336 ) ) ;
#5770 = CIRCLE ( 'NONE', #16332, 5.000000000000000888 ) ;
#5771 = ORIENTED_EDGE ( 'NONE', *, *, #54520, .T. ) ;
#5772 = CARTESIAN_POINT ( 'NONE',  ( 2.653899356899243944, 0.2611590963044465585, 7.767552767343915754 ) ) ;
#5773 = DIRECTION ( 'NONE',  ( 0.000000000000000000, 0.01356324068817998940, -0.9999080150203990547 ) ) ;
#5774 = CARTESIAN_POINT ( 'NONE',  ( 1.000000000000000888, 1.530946385938475762, -7.342084388195351252 ) ) ;
#5775 = ORIENTED_EDGE ( 'NONE', *, *, #15696, .F. ) ;
#5776 = CIRCLE ( 'NONE', #21715, 5.000000000000001776 ) ;
#5777 = CARTESIAN_POINT ( 'NONE',  ( -27.10719052120871098, -1.044362304621479165, 2.116547233941197703 ) ) ;
#5778 = ADVANCED_FACE ( 'NONE', ( #16764 ), #32051, .T. ) ;
#5779 = CARTESIAN_POINT ( 'NONE',  ( -22.70624764888619751, -4.891815784104535325, 1.907540768355092231 ) ) ;
#5780 = CARTESIAN_POINT ( 'NONE',  ( 49.13724917365554745, -0.1745483773780858450, -6.524050439336988028 ) ) ;
#5781 = VECTOR ( 'NONE', #34944, 1000.000000000000114 ) ;
#5782 = DIRECTION ( 'NONE',  ( -1.000000000000000000, 0.000000000000000000, 0.000000000000000000 ) ) ;
#5783 = CARTESIAN_POINT ( 'NONE',  ( 8.437200413559441614, 4.476360154859203355, 25.00000000000000000 ) ) ;
#5784 = CARTESIAN_POINT ( 'NONE',  ( 0.2652384529303124516, 2.061422456317187457, -12.07141085622970955 ) ) ;
#5785 = DIRECTION ( 'NONE',  ( -1.000000000000000000, 0.000000000000000000, 0.000000000000000000 ) ) ;
#5786 = DIRECTION ( 'NONE',  ( 0.000000000000000000, -6.883382752675980017E-15, 1.000000000000000000 ) ) ;
#5787 = B_SPLINE_CURVE_WITH_KNOTS ( 'NONE', 3,
 ( #60018, #55346, #14113, #54710, #64331, #9131, #55011, #24420, #64983, #14436 ),
 .UNSPECIFIED., .F., .F.,
 ( 4, 3, 3, 4 ),
 ( 9.351243737687475743E-19, 6.607638129004469909E-05, 9.911389841680516837E-05, 0.0001667630577588622570 ),
 .UNSPECIFIED. ) ;
#5788 = AXIS2_PLACEMENT_3D ( 'NONE', #13988, #29295, #54587 ) ;
#5789 = EDGE_CURVE ( 'NONE', #44959, #12280, #2897, .T. ) ;
#5790 = ORIENTED_EDGE ( 'NONE', *, *, #44875, .F. ) ;
#5791 = DIRECTION ( 'NONE',  ( -1.000000000000000000, 0.000000000000000000, 0.000000000000000000 ) ) ;
#5792 = CARTESIAN_POINT ( 'NONE',  ( 17.48646793688874013, -11.52800716181782370, 7.061530710347139639 ) ) ;
#5793 = ORIENTED_EDGE ( 'NONE', *, *, #39680, .F. ) ;
#5794 = ADVANCED_FACE ( 'NONE', ( #53989 ), #18087, .T. ) ;
#5795 = CARTESIAN_POINT ( 'NONE',  ( 0.6511581176954559513, 10.54760823437294803, 6.471755598256069497 ) ) ;
#5796 = CARTESIAN_POINT ( 'NONE',  ( -22.27722019094931483, 3.463038365117174333, 1.249795790945178897 ) ) ;
#5797 = CARTESIAN_POINT ( 'NONE',  ( 35.00000000000000000, 8.551552972817191289, 8.052525312709789773 ) ) ;
#5798 = VERTEX_POINT ( 'NONE', #58328 ) ;
#5799 = CARTESIAN_POINT ( 'NONE',  ( 0.3040950598368144520, 10.49113473328030821, 6.347045025870802881 ) ) ;
#5800 = CARTESIAN_POINT ( 'NONE',  ( 2.000000000000001776, 1.779948802829910193, -6.576141558201243242 ) ) ;
#5801 = ADVANCED_FACE ( 'NONE', ( #33033 ), #22404, .T. ) ;
#5802 = VERTEX_POINT ( 'NONE', #52689 ) ;
#5803 = CIRCLE ( 'NONE', #45082, 4.999999999999999112 ) ;
#5804 = AXIS2_PLACEMENT_3D ( 'NONE', #15159, #60726, #49768 ) ;
#5805 = VERTEX_POINT ( 'NONE', #17438 ) ;
#5806 = ORIENTED_EDGE ( 'NONE', *, *, #50812, .T. ) ;
#5807 = B_SPLINE_CURVE_WITH_KNOTS ( 'NONE', 3,
 ( #59902, #49288, #45565, #35255, #14632, #54257, #39926, #14965, #55562, #54898, #29608, #9021, #19668, #60210, #24642, #9322 ),
 .UNSPECIFIED., .F., .F.,
 ( 4, 3, 3, 3, 3, 4 ),
 ( 1.463672932855430986E-18, 0.0003017745587525266565, 0.0006035491769808764510, 0.0009053241094668187418, 0.001207275924539138231, 0.001510325902531263996 ),
 .UNSPECIFIED. ) ;
#5808 = CARTESIAN_POINT ( 'NONE',  ( 36.00000000000000711, 2.865935305911623487, -12.42372387097883646 ) ) ;
#5809 = EDGE_CURVE ( 'NONE', #5144, #42603, #28071, .T. ) ;
#5810 = ORIENTED_EDGE ( 'NONE', *, *, #55574, .F. ) ;
#5811 = CARTESIAN_POINT ( 'NONE',  ( -37.00000000000000711, 0.000000000000000000, 0.000000000000000000 ) ) ;
#5812 = CYLINDRICAL_SURFACE ( 'NONE', #16617, 6.936499999999988120 ) ;
#5813 = CARTESIAN_POINT ( 'NONE',  ( -47.00000000000000711, 0.000000000000000000, 0.000000000000000000 ) ) ;
#5814 = CARTESIAN_POINT ( 'NONE',  ( 3.152665057736049103, -0.4801242025610908959, -7.923639299008895520 ) ) ;
#5815 = VERTEX_POINT ( 'NONE', #7117 ) ;
#5816 = AXIS2_PLACEMENT_3D ( 'NONE', #58769, #3569, #64048 ) ;
#5817 = FACE_OUTER_BOUND ( 'NONE', #29716, .T. ) ;
#5818 = EDGE_CURVE ( 'NONE', #31374, #47315, #64586, .T. ) ;
#5819 = CARTESIAN_POINT ( 'NONE',  ( 9.461050110694847248, -32.74574823825055603, 12.19700847635464669 ) ) ;
#5820 = CARTESIAN_POINT ( 'NONE',  ( 24.44290582448688554, -2.844751314854803592, -13.19810646351145067 ) ) ;
#5822 = EDGE_LOOP ( 'NONE', ( #12261, #43013, #13208, #15289 ) ) ;
#5821 = CARTESIAN_POINT ( 'NONE',  ( 37.00000000000000711, 4.705694406421931860E-17, -3.469127814946512892E-15 ) ) ;
#5823 = CARTESIAN_POINT ( 'NONE',  ( 2.241451721903216399, -2.668222118333498205, 7.153019588493063630 ) ) ;
#5824 = ORIENTED_EDGE ( 'NONE', *, *, #31609, .F. ) ;
#5825 = LINE ( 'NONE', #44697, #23181 ) ;
#5826 = ORIENTED_EDGE ( 'NONE', *, *, #60895, .F. ) ;
#5827 = ORIENTED_EDGE ( 'NONE', *, *, #30102, .F. ) ;
#5828 = CARTESIAN_POINT ( 'NONE',  ( 35.00000000000000000, -0.7008968033239626472, -12.16632754454236576 ) ) ;
#5829 = EDGE_CURVE ( 'NONE', #64384, #57499, #24917, .T. ) ;
#5830 = CARTESIAN_POINT ( 'NONE',  ( 7.085269882676145770, -28.78331678330111387, 12.46778293907355994 ) ) ;
#5831 = AXIS2_PLACEMENT_3D ( 'NONE', #46120, #63026, #41762 ) ;
#5832 = CARTESIAN_POINT ( 'NONE',  ( 2.261269890822070749, -7.639767381742377239, -0.1394916642590645905 ) ) ;
#5833 = ORIENTED_EDGE ( 'NONE', *, *, #10070, .T. ) ;
#5834 = CARTESIAN_POINT ( 'NONE',  ( 2.639814597422740938, 7.689608172406201092, -1.095525832903406327 ) ) ;
#5835 = CARTESIAN_POINT ( 'NONE',  ( 1.719304012338836563, -2.961219984258077087, 12.38166659046417095 ) ) ;
#5836 = CARTESIAN_POINT ( 'NONE',  ( 0.2958664285830415741, -12.02992237133199893, 2.345117904768581063 ) ) ;
#5838 = EDGE_LOOP ( 'NONE', ( #24220, #27829, #21430, #12977 ) ) ;
#5837 = ADVANCED_FACE ( 'NONE', ( #48681 ), #410, .F. ) ;
#5839 = ORIENTED_EDGE ( 'NONE', *, *, #45220, .F. ) ;
#5840 = DIRECTION ( 'NONE',  ( 1.000000000000000000, -0.000000000000000000, 0.000000000000000000 ) ) ;
#5841 = ORIENTED_EDGE ( 'NONE', *, *, #15074, .T. ) ;
#5842 = EDGE_CURVE ( 'NONE', #5634, #63998, #39987, .T. ) ;
#5843 = ORIENTED_EDGE ( 'NONE', *, *, #64538, .F. ) ;
#5844 = DIRECTION ( 'NONE',  ( 1.000000000000000000, 0.000000000000000000, -0.000000000000000000 ) ) ;
#5845 = DIRECTION ( 'NONE',  ( 0.000000000000000000, 0.3218879778915972878, -0.9467777615094571386 ) ) ;
#5846 = DIRECTION ( 'NONE',  ( 1.000000000000000000, -0.000000000000000000, -0.000000000000000000 ) ) ;
#5847 = CARTESIAN_POINT ( 'NONE',  ( 18.75685862065280674, 1.097595231443926567, 11.95276324670687629 ) ) ;
#5848 = CARTESIAN_POINT ( 'NONE',  ( 0.3665391374699472626, -6.368473106897056368, -10.50279796150443268 ) ) ;
#5849 = LINE ( 'NONE', #46384, #5505 ) ;
#5850 = AXIS2_PLACEMENT_3D ( 'NONE', #58017, #50802, #62636 ) ;
#5851 = CARTESIAN_POINT ( 'NONE',  ( -22.27719443589224113, -0.7635131876694993824, -3.601617131804410565 ) ) ;
#5852 =( BOUNDED_SURFACE ( )  B_SPLINE_SURFACE ( 3, 1, ( 
 ( #10771, #21069 ),
 ( #16088, #31391 ),
 ( #22382, #57987 ),
 ( #46680, #32667 ) ),
 .UNSPECIFIED., .F., .F., .F. ) 
 B_SPLINE_SURFACE_WITH_KNOTS ( ( 4, 4 ),
 ( 2, 2 ),
 ( 0.000000000000000000, 1.000000000000000000 ),
 ( 0.000000000000000000, 1.000000000000000000 ),
 .UNSPECIFIED. ) 
 GEOMETRIC_REPRESENTATION_ITEM ( )  RATIONAL_B_SPLINE_SURFACE ( (
 ( 1.000000000000000000, 1.000000000000000000),
 ( 0.6933888150995267674, 0.9895912004443193632),
 ( 0.6933888150995267674, 0.9895912004443193632),
 ( 1.000000000000000000, 1.000000000000000000) ) ) 
 REPRESENTATION_ITEM ( '' )  SURFACE ( )  );
#5853 = ORIENTED_EDGE ( 'NONE', *, *, #34976, .F. ) ;
#5854 = CARTESIAN_POINT ( 'NONE',  ( 35.00000000000000000, -7.561043153948031836, -9.557269938331533154 ) ) ;
#5855 =( GEOMETRIC_REPRESENTATION_CONTEXT ( 3 ) GLOBAL_UNCERTAINTY_ASSIGNED_CONTEXT ( ( #58286 ) ) GLOBAL_UNIT_ASSIGNED_CONTEXT ( ( #42479, #52816, #43471 ) ) REPRESENTATION_CONTEXT ( 'NONE', 'WORKASPACE' ) );
#5856 = CARTESIAN_POINT ( 'NONE',  ( 35.00000000000000000, 10.07641281632177588, -6.036400161834603928 ) ) ;
#5857 = CARTESIAN_POINT ( 'NONE',  ( 2.990245332647840204, 8.426135047918846155, -0.9653152459622572623 ) ) ;
#5858 = EDGE_CURVE ( 'NONE', #29920, #18553, #11364, .T. ) ;
#5859 = CARTESIAN_POINT ( 'NONE',  ( 6.750737678534439290, -5.599118668687368405, 10.61556038268959767 ) ) ;
#5860 = EDGE_CURVE ( 'NONE', #39632, #33098, #15043, .T. ) ;
#5861 = CARTESIAN_POINT ( 'NONE',  ( -22.46225619532222950, 2.255146441673809843, 3.586917175123511381 ) ) ;
#5862 = AXIS2_PLACEMENT_3D ( 'NONE', #25292, #33711, #24982 ) ;
#5863 = CARTESIAN_POINT ( 'NONE',  ( 35.00000000000000000, 4.041347439436019151, 11.02904044024204211 ) ) ;
#5864 = CARTESIAN_POINT ( 'NONE',  ( 0.9296196016850440946, 2.573053270831450856, -12.19921892950026532 ) ) ;
#5865 = FACE_BOUND ( 'NONE', #14078, .T. ) ;
#5866 = ORIENTED_EDGE ( 'NONE', *, *, #15454, .F. ) ;
#5867 = VECTOR ( 'NONE', #14614, 1000.000000000000000 ) ;
#5868 = FACE_OUTER_BOUND ( 'NONE', #3097, .T. ) ;
#5869 = CARTESIAN_POINT ( 'NONE',  ( 35.00000000000000000, 4.705694406421931860E-17, -3.469127814946512892E-15 ) ) ;
#5870 = EDGE_CURVE ( 'NONE', #26580, #41890, #53862, .T. ) ;
#5871 = DIRECTION ( 'NONE',  ( -1.000000000000000000, 0.000000000000000000, 0.000000000000000000 ) ) ;
#5872 = EDGE_CURVE ( 'NONE', #29441, #22391, #43206, .T. ) ;
#5873 = CARTESIAN_POINT ( 'NONE',  ( -25.57027579282264185, 10.04421752534342893, 6.567951868637986301 ) ) ;
#5874 = CARTESIAN_POINT ( 'NONE',  ( 35.00000000000000000, -4.237620530777882699, -11.42599468261427909 ) ) ;
#5875 = EDGE_LOOP ( 'NONE', ( #52296, #29112, #39950, #36395 ) ) ;
#5876 = CARTESIAN_POINT ( 'NONE',  ( -17.57070937885803374, -9.283194252049366213, -9.806837742160563920 ) ) ;
#5877 = DIRECTION ( 'NONE',  ( 1.000000000000000000, 0.000000000000000000, 0.000000000000000000 ) ) ;
#5878 = CARTESIAN_POINT ( 'NONE',  ( 11.77510182854060439, -29.30972061338851375, -6.669332763618045057 ) ) ;
#5879 = ORIENTED_EDGE ( 'NONE', *, *, #33733, .T. ) ;
#5880 = CARTESIAN_POINT ( 'NONE',  ( -9.044148139924335084, -12.95551142774388254, -3.795959767731165169 ) ) ;
#5881 = CARTESIAN_POINT ( 'NONE',  ( -47.00000000000000711, 0.000000000000000000, 0.000000000000000000 ) ) ;
#5882 = CARTESIAN_POINT ( 'NONE',  ( -47.00000000000000711, 0.000000000000000000, 0.000000000000000000 ) ) ;
#5883 = EDGE_CURVE ( 'NONE', #45297, #20405, #61290, .T. ) ;
#5885 = ORIENTED_EDGE ( 'NONE', *, *, #55911, .F. ) ;
#5884 = DIRECTION ( 'NONE',  ( 0.000000000000000000, 0.6745969609292610247, 0.7381862504171999850 ) ) ;
#5886 = CARTESIAN_POINT ( 'NONE',  ( -27.10719052120871098, 2.295785794152562787, 0.5475695427849293084 ) ) ;
#5887 = AXIS2_PLACEMENT_3D ( 'NONE', #33389, #3148, #53687 ) ;
#5888 = CARTESIAN_POINT ( 'NONE',  ( -35.00000000000000000, 11.44858830469740241, -2.627174906296955381 ) ) ;
#5889 = EDGE_LOOP ( 'NONE', ( #41201, #38113, #38078, #52769 ) ) ;
#5890 = CARTESIAN_POINT ( 'NONE',  ( -37.00000000000000711, -7.718225330433741149, -9.430788938294133672 ) ) ;
#5891 = CARTESIAN_POINT ( 'NONE',  ( 32.00000000000000000, 15.00000000000000000, 1.836970198721028406E-15 ) ) ;
#5892 = FACE_OUTER_BOUND ( 'NONE', #16686, .T. ) ;
#5893 = CARTESIAN_POINT ( 'NONE',  ( 0.4626703367448379844, -1.858541096401079340, -12.17089897506941831 ) ) ;
#5894 = CARTESIAN_POINT ( 'NONE',  ( -9.684784117213519394, 9.450766871535190461, -7.397823669409496539 ) ) ;
#5895 = EDGE_CURVE ( 'NONE', #7261, #5463, #65502, .T. ) ;
#5896 = CYLINDRICAL_SURFACE ( 'NONE', #7955, 3.477897737712717152 ) ;
#5898 = VERTEX_POINT ( 'NONE', #9086 ) ;
#5897 = CARTESIAN_POINT ( 'NONE',  ( -35.00000000000000000, 10.42955799785328708, -6.303578524886837009 ) ) ;
#5899 = LINE ( 'NONE', #45545, #50424 ) ;
#5900 = VERTEX_POINT ( 'NONE', #29366 ) ;
#5901 = CARTESIAN_POINT ( 'NONE',  ( 2.261269890822072082, -5.017604628138437661, 5.762737836065097596 ) ) ;
#5902 = ORIENTED_EDGE ( 'NONE', *, *, #6159, .T. ) ;
#5903 = DIRECTION ( 'NONE',  ( 0.000000000000000000, 0.7107927964194478143, -0.7034014504948233881 ) ) ;
#5904 = DIRECTION ( 'NONE',  ( 0.000000000000000000, 0.000000000000000000, 1.000000000000000000 ) ) ;
#5905 = EDGE_CURVE ( 'NONE', #1113, #53238, #3973, .T. ) ;
#5906 = LINE ( 'NONE', #30159, #3533 ) ;
#5907 = ADVANCED_FACE ( 'NONE', ( #4101 ), #13731, .T. ) ;
#5908 = FACE_OUTER_BOUND ( 'NONE', #22678, .T. ) ;
#5909 = EDGE_LOOP ( 'NONE', ( #48183, #29484, #48736, #19623 ) ) ;
#5910 = CARTESIAN_POINT ( 'NONE',  ( -37.00000000000000711, 0.000000000000000000, 0.000000000000000000 ) ) ;
#5911 = AXIS2_PLACEMENT_3D ( 'NONE', #53543, #28251, #48546 ) ;
#5912 = CARTESIAN_POINT ( 'NONE',  ( -24.43643092833920960, -9.282280370820542359, 7.608281883034075932 ) ) ;
#5913 = CARTESIAN_POINT ( 'NONE',  ( -22.27721701579900682, -1.205877546543695278, 3.478642907697079956 ) ) ;
#5914 = ORIENTED_EDGE ( 'NONE', *, *, #39843, .T. ) ;
#5915 = ORIENTED_EDGE ( 'NONE', *, *, #11984, .F. ) ;
#5916 = ADVANCED_FACE ( 'NONE', ( #44993 ), #48552, .T. ) ;
#5917 = DIRECTION ( 'NONE',  ( 0.000000000000000000, 0.000000000000000000, 1.000000000000000000 ) ) ;
#5918 = VERTEX_POINT ( 'NONE', #39334 ) ;
#5919 = DIRECTION ( 'NONE',  ( -1.000000000000000000, 0.000000000000000000, -0.000000000000000000 ) ) ;
#5920 = CARTESIAN_POINT ( 'NONE',  ( -27.09229696323320979, 0.5586335684093801657, -2.247106967994374482 ) ) ;
#5921 = CARTESIAN_POINT ( 'NONE',  ( 0.2646305136544065406, -7.972778379581612285, 9.296005949277198255 ) ) ;
#5922 = VECTOR ( 'NONE', #58220, 1000.000000000000000 ) ;
#5923 = CARTESIAN_POINT ( 'NONE',  ( -27.09364415740165910, 1.009938549038103206, -2.088137158971423268 ) ) ;
#5924 = CYLINDRICAL_SURFACE ( 'NONE', #7566, 20.00000000000000000 ) ;
#5925 = DIRECTION ( 'NONE',  ( 0.000000000000000000, 0.000000000000000000, 1.000000000000000000 ) ) ;
#5926 = CARTESIAN_POINT ( 'NONE',  ( 2.258463476536645587, 7.499249607179738319, 1.460294809170969099 ) ) ;
#5927 = ORIENTED_EDGE ( 'NONE', *, *, #4458, .F. ) ;
#5928 = CARTESIAN_POINT ( 'NONE',  ( 35.00000000000000000, 10.14408668126221613, 5.921969905510239940 ) ) ;
#5929 = CARTESIAN_POINT ( 'NONE',  ( -35.00000000000000000, -9.240395740215685549, 7.251710744571544964 ) ) ;
#5930 = CYLINDRICAL_SURFACE ( 'NONE', #59322, 12.18650000000000055 ) ;
#5931 = DIRECTION ( 'NONE',  ( -1.000000000000000000, 0.000000000000000000, -0.000000000000000000 ) ) ;
#5932 = CARTESIAN_POINT ( 'NONE',  ( -2.676156797222403849, 7.839276155712927796, 10.99183054655308389 ) ) ;
#5933 = CARTESIAN_POINT ( 'NONE',  ( 35.00000000000000000, -4.041347439435937439, -11.02904044024207764 ) ) ;
#5934 = CARTESIAN_POINT ( 'NONE',  ( 37.00000000000000711, -3.511814412392203266, -11.66953048682398730 ) ) ;
#5935 = FACE_OUTER_BOUND ( 'NONE', #35780, .T. ) ;
#5936 = VERTEX_POINT ( 'NONE', #44636 ) ;
#5937 = AXIS2_PLACEMENT_3D ( 'NONE', #24555, #60133, #44834 ) ;
#5938 = EDGE_CURVE ( 'NONE', #30257, #21056, #64926, .T. ) ;
#5939 = ORIENTED_EDGE ( 'NONE', *, *, #25589, .F. ) ;
#5940 = DIRECTION ( 'NONE',  ( -1.000000000000000000, -0.000000000000000000, 0.000000000000000000 ) ) ;
#5941 = EDGE_CURVE ( 'NONE', #19644, #57557, #8193, .T. ) ;
#5942 = ORIENTED_EDGE ( 'NONE', *, *, #49382, .T. ) ;
#5943 = CARTESIAN_POINT ( 'NONE',  ( -22.31328051695926007, -3.781397440874596061, 0.2528478350593901802 ) ) ;
#5944 = DIRECTION ( 'NONE',  ( -1.000000000000000000, -0.000000000000000000, -0.000000000000000000 ) ) ;
#5945 = CARTESIAN_POINT ( 'NONE',  ( 1.104777566491146557, -9.895624035730012480, -7.679758239385240159 ) ) ;
#5946 = CARTESIAN_POINT ( 'NONE',  ( 2.241352910868908310, 2.532612177304540246, -7.202080440908716241 ) ) ;
#5947 = VERTEX_POINT ( 'NONE', #54962 ) ;
#5948 = CYLINDRICAL_SURFACE ( 'NONE', #47331, 12.74999999999999822 ) ;
#5949 = CARTESIAN_POINT ( 'NONE',  ( 36.00000000000000711, 2.080187960898561172, -12.57916205664482412 ) ) ;
#5950 = EDGE_CURVE ( 'NONE', #17535, #4846, #14519, .T. ) ;
#5951 = DIRECTION ( 'NONE',  ( -0.3865475372811022492, -0.7187975063895643002, -0.5778504531711118331 ) ) ;
#5952 = CARTESIAN_POINT ( 'NONE',  ( -14.47334165536099881, 3.872983346207417021, -1.000000000000000000 ) ) ;
#5953 = CARTESIAN_POINT ( 'NONE',  ( 9.268278201553693307, 6.103558304117178146, -12.04593591654801799 ) ) ;
#5954 = CARTESIAN_POINT ( 'NONE',  ( 2.259025283528086181, 2.741148848567763086, 7.131631878998401675 ) ) ;
#5955 = ORIENTED_EDGE ( 'NONE', *, *, #2660, .F. ) ;
#5956 = FACE_OUTER_BOUND ( 'NONE', #52267, .T. ) ;
#5957 = ORIENTED_EDGE ( 'NONE', *, *, #38142, .T. ) ;
#5958 = LINE ( 'NONE', #15883, #8963 ) ;
#5959 = DIRECTION ( 'NONE',  ( 0.000000000000000000, 0.01356324068817998940, -0.9999080150203990547 ) ) ;
#5960 = CARTESIAN_POINT ( 'NONE',  ( 35.00000000000000000, -10.01317267707881165, 6.946017217730044990 ) ) ;
#5961 = EDGE_CURVE ( 'NONE', #53475, #46122, #51725, .T. ) ;
#5962 = CARTESIAN_POINT ( 'NONE',  ( -30.18541646480309026, -1.416020129149132334, -13.42553116244734746 ) ) ;
#5963 = EDGE_CURVE ( 'NONE', #11560, #6736, #88, .T. ) ;
#5964 = DIRECTION ( 'NONE',  ( 0.000000000000000000, -0.8827602140260367714, 0.4698238015817268187 ) ) ;
#5965 = AXIS2_PLACEMENT_3D ( 'NONE', #25034, #60934, #60593 ) ;
#5966 = ORIENTED_EDGE ( 'NONE', *, *, #45821, .T. ) ;
#5967 = ORIENTED_EDGE ( 'NONE', *, *, #36957, .F. ) ;
#5968 = CARTESIAN_POINT ( 'NONE',  ( 5.515539859299206427, 0.005336559634876942085, 0.002856745161749560304 ) ) ;
#5969 = ORIENTED_EDGE ( 'NONE', *, *, #28704, .F. ) ;
#5970 = CARTESIAN_POINT ( 'NONE',  ( -18.04458733766117362, 25.00000000000000000, 3.916728392552376370 ) ) ;
#5971 = CARTESIAN_POINT ( 'NONE',  ( 3.115331810559627712, 4.248790708446858133, -12.82013328618461223 ) ) ;
#5972 = CARTESIAN_POINT ( 'NONE',  ( -18.04458733766117362, -11.34280559204704097, 3.916728392552376370 ) ) ;
#5973 = CARTESIAN_POINT ( 'NONE',  ( 1.198791140417294843, 9.279671759317841051, 8.460175745277314974 ) ) ;
#5974 = CARTESIAN_POINT ( 'NONE',  ( 0.000000000000000000, 6.441884263200815752, 2.217201541069855786 ) ) ;
#5975 = DIRECTION ( 'NONE',  ( -1.000000000000000000, -1.836970198721029688E-16, -0.000000000000000000 ) ) ;
#5976 = CARTESIAN_POINT ( 'NONE',  ( 0.8375941296829887417, 12.30893872205359152, -1.780036797757713174 ) ) ;
#5977 = ORIENTED_EDGE ( 'NONE', *, *, #6654, .F. ) ;
#5978 = B_SPLINE_CURVE_WITH_KNOTS ( 'NONE', 3,
 ( #47311, #5518, #12679, #1752, #37961, #62904, #27016, #58257, #22690, #27649, #526, #20793, #37304, #36059, #51063, #53271 ),
 .UNSPECIFIED., .F., .F.,
 ( 4, 2, 2, 2, 2, 2, 2, 4 ),
 ( 0.000000000000000000, 0.001108109431372354420, 0.002216218862744708841, 0.003324328294117063261, 0.004432437725489417682, 0.006648656588234126523, 0.007756766019606478775, 0.008864875450978831894 ),
 .UNSPECIFIED. ) ;
#5979 = CARTESIAN_POINT ( 'NONE',  ( 1.462291587749844135, -11.25382118863310765, 5.766456054323949587 ) ) ;
#5980 = ORIENTED_EDGE ( 'NONE', *, *, #27999, .T. ) ;
#5981 = ADVANCED_FACE ( 'NONE', ( #3807 ), #50117, .F. ) ;
#5982 = CARTESIAN_POINT ( 'NONE',  ( 22.58646936605650168, -11.74531380756754828, -6.665220879160888678 ) ) ;
#5983 = CARTESIAN_POINT ( 'NONE',  ( -27.08430418657510685, 1.863523114788013801, -1.333569526609269085 ) ) ;
#5984 = ORIENTED_EDGE ( 'NONE', *, *, #3722, .T. ) ;
#5985 = ADVANCED_FACE ( 'NONE', ( #26340 ), #21012, .T. ) ;
#5986 = CARTESIAN_POINT ( 'NONE',  ( -27.09229696323388836, 1.666734935102336612, 1.607344345646377404 ) ) ;
#5987 = CARTESIAN_POINT ( 'NONE',  ( -22.27709082389155171, 3.569727173833830758, -0.8996430462092170899 ) ) ;
#5988 = ORIENTED_EDGE ( 'NONE', *, *, #64580, .T. ) ;
#5989 = LINE ( 'NONE', #20262, #24806 ) ;
#5990 = CARTESIAN_POINT ( 'NONE',  ( -15.30016555129098599, -29.00876116002302396, -11.22753712089058808 ) ) ;
#5991 = DIRECTION ( 'NONE',  ( 1.000000000000000000, 0.000000000000000000, -0.000000000000000000 ) ) ;
#5992 = ORIENTED_EDGE ( 'NONE', *, *, #21176, .F. ) ;
#5993 = ORIENTED_EDGE ( 'NONE', *, *, #8939, .F. ) ;
#5994 = EDGE_CURVE ( 'NONE', #15359, #63312, #45983, .T. ) ;
#5995 = CARTESIAN_POINT ( 'NONE',  ( 36.00000000000000711, 11.24036214326529048, 6.018036132182036368 ) ) ;
#5996 = ORIENTED_EDGE ( 'NONE', *, *, #60786, .T. ) ;
#5997 = DIRECTION ( 'NONE',  ( 1.000000000000000000, -0.000000000000000000, 0.000000000000000000 ) ) ;
#5998 = ORIENTED_EDGE ( 'NONE', *, *, #44285, .T. ) ;
#5999 = EDGE_LOOP ( 'NONE', ( #14846, #57002, #40623, #39808 ) ) ;
#6000 = ORIENTED_EDGE ( 'NONE', *, *, #62112, .F. ) ;
#6001 = CARTESIAN_POINT ( 'NONE',  ( 2.000000000000001776, 6.796153407501467569, -1.388283512725773772 ) ) ;
#6002 = DIRECTION ( 'NONE',  ( 1.000000000000000000, 0.000000000000000000, -0.000000000000000000 ) ) ;
#6003 = CARTESIAN_POINT ( 'NONE',  ( 2.770579946183334030, -1.056759439485520424, -7.739026583264751125 ) ) ;
#6004 = CARTESIAN_POINT ( 'NONE',  ( 9.575800908719084958, 11.95193887484099093, -1.072919909436247154 ) ) ;
#6005 = FACE_OUTER_BOUND ( 'NONE', #23698, .T. ) ;
#6006 = ORIENTED_EDGE ( 'NONE', *, *, #61029, .T. ) ;
#6007 = AXIS2_PLACEMENT_3D ( 'NONE', #63284, #53332, #44003 ) ;
#6008 = LINE ( 'NONE', #57186, #36470 ) ;
#6009 = CIRCLE ( 'NONE', #29320, 17.59807621135332312 ) ;
#6010 = EDGE_LOOP ( 'NONE', ( #61169, #33056, #53639, #57174 ) ) ;
#6011 = CARTESIAN_POINT ( 'NONE',  ( 0.000000000000000000, 0.000000000000000000, 0.000000000000000000 ) ) ;
#6012 = B_SPLINE_CURVE_WITH_KNOTS ( 'NONE', 3,
 ( #24171, #44437, #14188, #65055, #10503, #44772, #15497, #45768, #30149, #60737, #20826, #230, #30779, #40789, #5213, #25158 ),
 .UNSPECIFIED., .F., .F.,
 ( 4, 2, 2, 2, 2, 2, 2, 4 ),
 ( 0.000000000000000000, 0.002138034596868667800, 0.003207051895303000832, 0.004276069193737333865, 0.005345086492171666898, 0.006414103790605999930, 0.007483121089040332963, 0.008552138387474665995 ),
 .UNSPECIFIED. ) ;
#6013 = CARTESIAN_POINT ( 'NONE',  ( -27.08935880048752409, 0.6272370006475171955, 2.219773948423720444 ) ) ;
#6014 = CYLINDRICAL_SURFACE ( 'NONE', #19414, 6.842778212674966554 ) ;
#6015 = CARTESIAN_POINT ( 'NONE',  ( 0.2767916011545391020, -8.018602152763797619, -9.260929738915313791 ) ) ;
#6016 = CARTESIAN_POINT ( 'NONE',  ( 29.08103898107091112, 5.276197063807976484, 10.78770863057103568 ) ) ;
#6017 = CARTESIAN_POINT ( 'NONE',  ( 3.152665057734129306, -7.923639299008720549, -0.4801242025592799556 ) ) ;
#6018 = ORIENTED_EDGE ( 'NONE', *, *, #38040, .F. ) ;
#6019 = CARTESIAN_POINT ( 'NONE',  ( -36.00000000000000711, -12.73293890771483028, -0.6593684648221820321 ) ) ;
#6020 = EDGE_CURVE ( 'NONE', #61618, #55634, #34023, .T. ) ;
#6021 = EDGE_LOOP ( 'NONE', ( #41764, #48451, #50400, #44731 ) ) ;
#6022 = CARTESIAN_POINT ( 'NONE',  ( 0.2646305136544065406, -4.312539723326210606, 11.46223899740598640 ) ) ;
#6023 =( NAMED_UNIT ( * ) SI_UNIT ( $, .STERADIAN. ) SOLID_ANGLE_UNIT ( ) );
#6024 = CARTESIAN_POINT ( 'NONE',  ( 2.899286259009683953, 6.239228647238633130, -4.769992516330172627 ) ) ;
#6025 = DIRECTION ( 'NONE',  ( 0.000000000000000000, 0.01356324068817992175, -0.9999080150203990547 ) ) ;
#6026 = CARTESIAN_POINT ( 'NONE',  ( 0.000000000000000000, 0.000000000000000000, 0.000000000000000000 ) ) ;
#6027 = VERTEX_POINT ( 'NONE', #55950 ) ;
#6028 = PLANE ( 'NONE',  #60048 ) ;
#6029 = DIRECTION ( 'NONE',  ( 1.000000000000000000, 0.000000000000000000, 0.000000000000000000 ) ) ;
#6030 = CARTESIAN_POINT ( 'NONE',  ( -35.00000000000000000, 12.74921544981111055, -0.1414404973752581562 ) ) ;
#6031 = CARTESIAN_POINT ( 'NONE',  ( 2.440552418640495880, 3.678171968408328940, 6.765628357760791189 ) ) ;
#6032 = CARTESIAN_POINT ( 'NONE',  ( 0.3654063281920718054, 12.27672420655579089, -0.2633658439603773216 ) ) ;
#6034 = EDGE_CURVE ( 'NONE', #3889, #38752, #30659, .T. ) ;
#6033 = DIRECTION ( 'NONE',  ( 1.000000000000000000, 0.000000000000000000, 0.000000000000000000 ) ) ;
#6035 = APPLICATION_CONTEXT ( 'automotive_design' ) ;
#6036 = CARTESIAN_POINT ( 'NONE',  ( 0.3665391374699465965, 12.13918562134718826, 1.872534962004841708 ) ) ;
#6037 = CARTESIAN_POINT ( 'NONE',  ( -37.00000000000000711, 0.000000000000000000, 0.000000000000000000 ) ) ;
#6038 = VECTOR ( 'NONE', #51297, 1000.000000000000000 ) ;
#6039 = EDGE_CURVE ( 'NONE', #6851, #58393, #19166, .T. ) ;
#6040 = ORIENTED_EDGE ( 'NONE', *, *, #9124, .F. ) ;
#6041 = ORIENTED_EDGE ( 'NONE', *, *, #34661, .F. ) ;
#6043 = CARTESIAN_POINT ( 'NONE',  ( 2.000000000000001776, 0.000000000000000000, 0.000000000000000000 ) ) ;
#6042 =( BOUNDED_SURFACE ( )  B_SPLINE_SURFACE ( 3, 1, ( 
 ( #21892, #629 ),
 ( #31840, #20890 ),
 ( #30856, #46822 ),
 ( #41833, #1288 ) ),
 .UNSPECIFIED., .F., .F., .F. ) 
 B_SPLINE_SURFACE_WITH_KNOTS ( ( 4, 4 ),
 ( 2, 2 ),
 ( 0.000000000000000000, 1.000000000000000000 ),
 ( 0.000000000000000000, 1.000000000000000000 ),
 .UNSPECIFIED. ) 
 GEOMETRIC_REPRESENTATION_ITEM ( )  RATIONAL_B_SPLINE_SURFACE ( (
 ( 1.000000000000000000, 1.000000000000000000),
 ( 0.9942764183789327692, 0.8450855930916585379),
 ( 0.9942764183789327692, 0.8450855930916585379),
 ( 1.000000000000000000, 1.000000000000000000) ) ) 
 REPRESENTATION_ITEM ( '' )  SURFACE ( )  );
#6044 = CARTESIAN_POINT ( 'NONE',  ( 48.17199526896421702, -0.3660652840184965284, -6.262213226250246123 ) ) ;
#6045 = DIRECTION ( 'NONE',  ( 0.000000000000000000, -0.5767582926624852391, -0.8169148498130358593 ) ) ;
#6046 = DIRECTION ( 'NONE',  ( -1.000000000000000000, 0.000000000000000000, 0.000000000000000000 ) ) ;
#6047 = ORIENTED_EDGE ( 'NONE', *, *, #9426, .T. ) ;
#6048 = ORIENTED_EDGE ( 'NONE', *, *, #37551, .F. ) ;
#6049 = ORIENTED_EDGE ( 'NONE', *, *, #11391, .F. ) ;
#6050 = CARTESIAN_POINT ( 'NONE',  ( 36.00000000000000711, -11.80185301892977279, 4.824807283154243898 ) ) ;
#6051 = EDGE_CURVE ( 'NONE', #17370, #11727, #51902, .T. ) ;
#6052 = LINE ( 'NONE', #52588, #40612 ) ;
#6053 = VERTEX_POINT ( 'NONE', #41293 ) ;
#6054 = FACE_OUTER_BOUND ( 'NONE', #2548, .T. ) ;
#6055 = CARTESIAN_POINT ( 'NONE',  ( 1.719304012339844867, -12.64775761152577971, 1.452142814149586902 ) ) ;
#6056 = EDGE_LOOP ( 'NONE', ( #36359, #53154, #14270, #22903 ) ) ;
#6057 = DIRECTION ( 'NONE',  ( 1.000000000000000000, 0.000000000000000000, 0.000000000000000000 ) ) ;
#6058 = CARTESIAN_POINT ( 'NONE',  ( 16.03117610287102579, -29.21144266226587760, -10.60889071582655241 ) ) ;
#6059 = CARTESIAN_POINT ( 'NONE',  ( 2.247206125383335085, 7.135412558555234597, 2.720255231379262728 ) ) ;
#6060 = VERTEX_POINT ( 'NONE', #51637 ) ;
#6061 = CARTESIAN_POINT ( 'NONE',  ( 0.3401186441510234415, 12.12646044229293274, -1.878666403202209567 ) ) ;
#6062 = VERTEX_POINT ( 'NONE', #61918 ) ;
#6063 = CARTESIAN_POINT ( 'NONE',  ( 35.00000000000000000, -0.6593684648219556577, 12.73293890771483383 ) ) ;
#6064 = ORIENTED_EDGE ( 'NONE', *, *, #17607, .T. ) ;
#6065 = CARTESIAN_POINT ( 'NONE',  ( 35.00000000000000000, -12.46157735505187247, 2.696588552979187536 ) ) ;
#6066 = CARTESIAN_POINT ( 'NONE',  ( -0.4370662499787615340, -31.03649492335484439, 14.44372008463347079 ) ) ;
#6067 = DIRECTION ( 'NONE',  ( 0.000000000000000000, 0.4198891015602592147, 0.9075754196709596711 ) ) ;
#6068 = EDGE_CURVE ( 'NONE', #20284, #7532, #61262, .T. ) ;
#6069 = CARTESIAN_POINT ( 'NONE',  ( -24.98829009532795808, 4.047772734466310141, 0.3426763744735841777 ) ) ;
#6070 = LINE ( 'NONE', #56939, #13365 ) ;
#6071 = CARTESIAN_POINT ( 'NONE',  ( -35.00000000000000000, -8.496612874013223404, 9.506317355798342916 ) ) ;
#6072 = LINE ( 'NONE', #55277, #55880 ) ;
#6073 = CARTESIAN_POINT ( 'NONE',  ( 0.2653519991613826345, 4.167757449530418157, 11.51519138201631876 ) ) ;
#6075 = VERTEX_POINT ( 'NONE', #52291 ) ;
#6074 = CARTESIAN_POINT ( 'NONE',  ( 35.00000000000000000, 4.705694406421931860E-17, -3.469127814946512892E-15 ) ) ;
#6076 = DIRECTION ( 'NONE',  ( -1.000000000000000000, -0.000000000000000000, 0.000000000000000000 ) ) ;
#6077 = ORIENTED_EDGE ( 'NONE', *, *, #28984, .F. ) ;
#6078 = CARTESIAN_POINT ( 'NONE',  ( 0.2676618633000457659, -4.339362305359514949, 11.45242956837285853 ) ) ;
#6079 = CARTESIAN_POINT ( 'NONE',  ( 2.573738926104378599, -5.779258037546978422, -5.156412073069344792 ) ) ;
#6080 = EDGE_LOOP ( 'NONE', ( #13156, #15115, #17283, #21192, #48982, #9686 ) ) ;
#6081 = CARTESIAN_POINT ( 'NONE',  ( 2.907497136250910774, 7.497839665536955245, 2.346692756478168995 ) ) ;
#6082 = CARTESIAN_POINT ( 'NONE',  ( 0.2638984909335720941, 10.70468911391664157, 5.950360275955092426 ) ) ;
#6083 = CARTESIAN_POINT ( 'NONE',  ( 0.2651627923886325511, -9.324231535593057174, -7.938954356958184633 ) ) ;
#6084 = VECTOR ( 'NONE', #6002, 1000.000000000000000 ) ;
#6085 = DIRECTION ( 'NONE',  ( 1.000000000000000000, -0.000000000000000000, 0.000000000000000000 ) ) ;
#6086 = CARTESIAN_POINT ( 'NONE',  ( 0.2646305136544072623, 10.53923716745255490, -6.237419468586968385 ) ) ;
#6087 = ORIENTED_EDGE ( 'NONE', *, *, #29389, .T. ) ;
#6088 = VECTOR ( 'NONE', #11025, 1000.000000000000000 ) ;
#6089 = CARTESIAN_POINT ( 'NONE',  ( -17.73204436170163234, -5.329256642071285910, -10.75287752448376644 ) ) ;
#6090 = ADVANCED_FACE ( 'NONE', ( #36649 ), #11370, .T. ) ;
#6091 = ORIENTED_EDGE ( 'NONE', *, *, #43589, .F. ) ;
#6092 = CARTESIAN_POINT ( 'NONE',  ( 0.2648978790185593790, 12.08224454301448958, 1.996248716311670446 ) ) ;
#6093 = DIRECTION ( 'NONE',  ( -1.000000000000000000, 0.000000000000000000, 0.000000000000000000 ) ) ;
#6094 = ADVANCED_FACE ( 'NONE', ( #57264 ), #25061, .F. ) ;
#6095 = DIRECTION ( 'NONE',  ( 0.9364047569793457759, -0.3509218304786018705, 0.000000000000000000 ) ) ;
#6096 = ORIENTED_EDGE ( 'NONE', *, *, #38405, .F. ) ;
#6097 = DIRECTION ( 'NONE',  ( -1.000000000000000000, 0.000000000000000000, 0.000000000000000000 ) ) ;
#6098 = EDGE_CURVE ( 'NONE', #59129, #60647, #17733, .T. ) ;
#6099 = CARTESIAN_POINT ( 'NONE',  ( 29.15566506771730104, 8.541154756424255368, 10.48791489529884480 ) ) ;
#6100 = DIRECTION ( 'NONE',  ( -1.000000000000000000, 0.000000000000000000, 0.000000000000000000 ) ) ;
#6101 = FACE_OUTER_BOUND ( 'NONE', #35367, .T. ) ;
#6102 = CARTESIAN_POINT ( 'NONE',  ( 0.2653519890538384995, 1.477274386607676477E-15, 12.24619734961521189 ) ) ;
#6103 = FACE_OUTER_BOUND ( 'NONE', #44197, .T. ) ;
#6104 = ADVANCED_FACE ( 'NONE', ( #63222 ), #63535, .F. ) ;
#6105 = CARTESIAN_POINT ( 'NONE',  ( 1.547277799337858584, 4.961646058323314179, 11.66196709685579158 ) ) ;
#6106 = DIRECTION ( 'NONE',  ( 0.000000000000000000, -0.9105187689795911643, 0.4134677391718609707 ) ) ;
#6107 = VERTEX_POINT ( 'NONE', #62550 ) ;
#6108 = CARTESIAN_POINT ( 'NONE',  ( -17.96034788017830053, 6.012426159432092909, 12.08945883540747346 ) ) ;
#6109 = CARTESIAN_POINT ( 'NONE',  ( 6.742624838446524826, -7.056336534564969121, 11.51515283083395857 ) ) ;
#6110 = ORIENTED_EDGE ( 'NONE', *, *, #64067, .F. ) ;
#6111 = CARTESIAN_POINT ( 'NONE',  ( 1.634816307074488995, 10.62369813896843418, 6.964001572434787235 ) ) ;
#6112 = CARTESIAN_POINT ( 'NONE',  ( -37.00000000000000711, 0.000000000000000000, 0.000000000000000000 ) ) ;
#6113 = CARTESIAN_POINT ( 'NONE',  ( -9.824501563233303258, 11.81955781327371291, -6.534828226117857852 ) ) ;
#6114 = EDGE_LOOP ( 'NONE', ( #65729, #58789, #2302, #64270 ) ) ;
#6115 = CARTESIAN_POINT ( 'NONE',  ( 2.273267844204867494, -6.543821324256909655, 3.952852893982274907 ) ) ;
#6116 = DIRECTION ( 'NONE',  ( -1.000000000000000000, 0.000000000000000000, 0.000000000000000000 ) ) ;
#6117 = VERTEX_POINT ( 'NONE', #7706 ) ;
#6118 = CARTESIAN_POINT ( 'NONE',  ( 0.2834382757448042356, -5.949714385480707080, 10.71064820518740213 ) ) ;
#6119 = ORIENTED_EDGE ( 'NONE', *, *, #33503, .F. ) ;
#6120 = VERTEX_POINT ( 'NONE', #47611 ) ;
#6121 = DIRECTION ( 'NONE',  ( 0.000000000000000000, 0.01356324068817998940, -0.9999080150203990547 ) ) ;
#6122 = CIRCLE ( 'NONE', #15638, 2.899999999999995914 ) ;
#6123 = VERTEX_POINT ( 'NONE', #57934 ) ;
#6124 = DIRECTION ( 'NONE',  ( 0.000000000000000000, -0.01356324068817998940, 0.9999080150203990547 ) ) ;
#6125 = CARTESIAN_POINT ( 'NONE',  ( -22.28415773361650309, -3.565377603762382108, 0.9981933716384869815 ) ) ;
#6126 = DIRECTION ( 'NONE',  ( -1.000000000000000000, 0.000000000000000000, -0.000000000000000000 ) ) ;
#6127 = DIRECTION ( 'NONE',  ( 0.000000000000000000, 0.01356324068817998940, -0.9999080150203990547 ) ) ;
#6128 = VERTEX_POINT ( 'NONE', #17692 ) ;
#6129 = CARTESIAN_POINT ( 'NONE',  ( 0.000000000000000000, 0.000000000000000000, 0.000000000000000000 ) ) ;
#6130 = CARTESIAN_POINT ( 'NONE',  ( 1.074417311476293158, -25.72614907888524982, 15.66246854766675156 ) ) ;
#6131 = DIRECTION ( 'NONE',  ( 1.000000000000000000, 0.000000000000000000, -0.000000000000000000 ) ) ;
#6133 = VERTEX_POINT ( 'NONE', #27639 ) ;
#6132 = CARTESIAN_POINT ( 'NONE',  ( 5.515539859299206427, 0.001241880655086591853, -0.005924322247674741922 ) ) ;
#6134 = CARTESIAN_POINT ( 'NONE',  ( 2.241509619876139059, -2.647089031563618633, 7.160887714159610340 ) ) ;
#6135 = ORIENTED_EDGE ( 'NONE', *, *, #323, .T. ) ;
#6136 = CARTESIAN_POINT ( 'NONE',  ( 0.2646305136544072623, 6.008537389229419823, 10.67138229758231738 ) ) ;
#6137 = ORIENTED_EDGE ( 'NONE', *, *, #9124, .T. ) ;
#6138 = ORIENTED_EDGE ( 'NONE', *, *, #35252, .T. ) ;
#6139 = DIRECTION ( 'NONE',  ( 0.000000000000000000, -0.7196168960969719919, -0.6943713148249717193 ) ) ;
#6140 = CARTESIAN_POINT ( 'NONE',  ( 18.00005080000000035, 1.836970198721027222E-16, -1.499999999999997780 ) ) ;
#6141 = DIRECTION ( 'NONE',  ( 0.000000000000000000, -0.01356324068817997726, 0.9999080150203990547 ) ) ;
#6142 = ADVANCED_FACE ( 'NONE', ( #48299 ), #12023, .T. ) ;
#6143 = ORIENTED_EDGE ( 'NONE', *, *, #51371, .T. ) ;
#6144 = CARTESIAN_POINT ( 'NONE',  ( 47.00000000000000711, 4.705694406421931860E-17, -3.469127814946512892E-15 ) ) ;
#6145 = CARTESIAN_POINT ( 'NONE',  ( 0.3675815128205912052, -2.391755495700685241, 12.04510820461658582 ) ) ;
#6146 = CARTESIAN_POINT ( 'NONE',  ( 36.00000000000000711, 12.70128625845192794, -1.113475361586537593 ) ) ;
#6147 = ORIENTED_EDGE ( 'NONE', *, *, #42387, .F. ) ;
#6148 = ORIENTED_EDGE ( 'NONE', *, *, #64302, .F. ) ;
#6149 = DIRECTION ( 'NONE',  ( -1.000000000000000000, 0.000000000000000000, 0.000000000000000000 ) ) ;
#6150 = ORIENTED_EDGE ( 'NONE', *, *, #47830, .T. ) ;
#6151 = ORIENTED_EDGE ( 'NONE', *, *, #55702, .T. ) ;
#6152 = DIRECTION ( 'NONE',  ( -0.5244426074294280538, 0.000000000000000000, 0.8514458006899926490 ) ) ;
#6153 = CARTESIAN_POINT ( 'NONE',  ( -37.00000000000000711, 0.000000000000000000, 0.000000000000000000 ) ) ;
#6154 = CARTESIAN_POINT ( 'NONE',  ( -37.00000000000000711, 0.000000000000000000, 0.000000000000000000 ) ) ;
#6155 = CARTESIAN_POINT ( 'NONE',  ( 0.3665391374699465965, 6.368473106897129199, 10.50279796150439005 ) ) ;
#6156 = DIRECTION ( 'NONE',  ( 0.000000000000000000, 0.9796553971857736576, 0.2006870767258926158 ) ) ;
#6157 = VECTOR ( 'NONE', #55859, 1000.000000000000000 ) ;
#6158 = DIRECTION ( 'NONE',  ( 0.000000000000000000, 0.000000000000000000, 1.000000000000000000 ) ) ;
#6159 = EDGE_CURVE ( 'NONE', #47988, #9409, #45703, .T. ) ;
#6160 = DIRECTION ( 'NONE',  ( 0.000000000000000000, -0.01356324068817999114, 0.9999080150203989437 ) ) ;
#6161 = CIRCLE ( 'NONE', #45430, 12.74999999999999822 ) ;
#6162 = EDGE_CURVE ( 'NONE', #64295, #10376, #56609, .T. ) ;
#6163 = ORIENTED_EDGE ( 'NONE', *, *, #39496, .F. ) ;
#6164 = ADVANCED_FACE ( 'NONE', ( #58931 ), #15340, .F. ) ;
#6165 = CARTESIAN_POINT ( 'NONE',  ( -22.28629837673887693, -3.055064048018810929, 2.102970853432575282 ) ) ;
#6166 = CARTESIAN_POINT ( 'NONE',  ( 35.00000000000000000, -0.7214809346829402781, -11.72397916322012179 ) ) ;
#6167 = CIRCLE ( 'NONE', #31625, 5.000000000000002665 ) ;
#6168 = CARTESIAN_POINT ( 'NONE',  ( 2.000000000000001776, 0.000000000000000000, 0.000000000000000000 ) ) ;
#6169 = CARTESIAN_POINT ( 'NONE',  ( 2.305787727787083519, 3.682701754025512919, 6.711944854845837583 ) ) ;
#6170 = AXIS2_PLACEMENT_3D ( 'NONE', #40457, #14841, #60757 ) ;
#6171 = EDGE_CURVE ( 'NONE', #40578, #37945, #5366, .T. ) ;
#6172 = CARTESIAN_POINT ( 'NONE',  ( 24.17999985073118197, -2.133694974929364552, -13.33140535122455717 ) ) ;
#6173 = ADVANCED_FACE ( 'NONE', ( #44908 ), #4028, .T. ) ;
#6174 = CARTESIAN_POINT ( 'NONE',  ( 3.334832302356885769, 3.396901620706510361, -11.51108694095134766 ) ) ;
#6175 = CARTESIAN_POINT ( 'NONE',  ( 8.553052268354708332, 3.426888109790365622, -11.50363822801515568 ) ) ;
#6176 = ORIENTED_EDGE ( 'NONE', *, *, #55728, .F. ) ;
#6177 = CARTESIAN_POINT ( 'NONE',  ( -37.00000000000000711, 0.000000000000000000, 0.000000000000000000 ) ) ;
#6178 = CARTESIAN_POINT ( 'NONE',  ( 2.000000000000001776, -6.750946897830688798, -1.593658756657146292 ) ) ;
#6179 = CARTESIAN_POINT ( 'NONE',  ( -35.00000000000000000, 9.913596905230113165, 8.017674001891819557 ) ) ;
#6180 = CARTESIAN_POINT ( 'NONE',  ( 15.63877597542616016, -34.91516792956262805, 5.826750174075395527 ) ) ;
#6181 = EDGE_CURVE ( 'NONE', #31335, #25218, #42503, .T. ) ;
#6182 = LINE ( 'NONE', #61685, #53265 ) ;
#6183 = CARTESIAN_POINT ( 'NONE',  ( 2.524535260912731616, -7.184101064217925270, 2.850096701925854514 ) ) ;
#6184 = ORIENTED_EDGE ( 'NONE', *, *, #25800, .T. ) ;
#6185 = CARTESIAN_POINT ( 'NONE',  ( 2.241352910868908310, -3.744764251556946366, -6.652881166698550786 ) ) ;
#6186 = CARTESIAN_POINT ( 'NONE',  ( 37.00000000000000711, 9.196955404009292678, -8.830544224262981245 ) ) ;
#6188 = EDGE_CURVE ( 'NONE', #59781, #37175, #59520, .T. ) ;
#6187 = CARTESIAN_POINT ( 'NONE',  ( -22.66110217412718342, -0.6585288088159785280, 4.900671186447912220 ) ) ;
#6189 = ORIENTED_EDGE ( 'NONE', *, *, #64778, .T. ) ;
#6190 = CARTESIAN_POINT ( 'NONE',  ( 2.969415267404726499, 7.007431655063608211, 3.597837242549700942 ) ) ;
#6191 = DIRECTION ( 'NONE',  ( 0.000000000000000000, -0.01356324068817998940, 0.9999080150203990547 ) ) ;
#6192 = CARTESIAN_POINT ( 'NONE',  ( 0.9232058338315048962, 11.84276737136206137, -3.908895078357403019 ) ) ;
#6194 = EDGE_LOOP ( 'NONE', ( #60636, #17466, #7603, #31172 ) ) ;
#6193 = CYLINDRICAL_SURFACE ( 'NONE', #40253, 12.18649999999999878 ) ;
#6195 = CARTESIAN_POINT ( 'NONE',  ( -27.08776759928964850, 2.229418711698783806, 0.5731512436791836862 ) ) ;
#6196 = DIRECTION ( 'NONE',  ( 1.000000000000000000, 0.000000000000000000, -0.000000000000000000 ) ) ;
#6197 = ORIENTED_EDGE ( 'NONE', *, *, #39819, .T. ) ;
#6198 = CARTESIAN_POINT ( 'NONE',  ( -22.66110217412718697, 4.366928509133841452, -2.319520136975649294 ) ) ;
#6199 = CARTESIAN_POINT ( 'NONE',  ( 37.00000000000000711, 4.705694406421931860E-17, -3.469127814946512892E-15 ) ) ;
#6200 = CIRCLE ( 'NONE', #40153, 5.000000000000002665 ) ;
#6201 = CARTESIAN_POINT ( 'NONE',  ( 23.57323689665027544, 1.992445679240424150, -11.83683888636838333 ) ) ;
#6202 = CARTESIAN_POINT ( 'NONE',  ( -3.992345480360331766, -11.80960273735984600, 6.553217067094195158 ) ) ;
#6203 = CARTESIAN_POINT ( 'NONE',  ( 26.25882823526612597, 13.04980996862090947, 3.460358416528618086 ) ) ;
#6204 = CARTESIAN_POINT ( 'NONE',  ( 2.000000000000001776, -2.473437528934089524, -7.080403010455012414 ) ) ;
#6206 = ORIENTED_EDGE ( 'NONE', *, *, #65639, .T. ) ;
#6205 = CARTESIAN_POINT ( 'NONE',  ( 0.2872850955227771452, 11.44140577127598668, -4.386654201695032285 ) ) ;
#6207 = CIRCLE ( 'NONE', #9347, 5.000000000000002665 ) ;
#6208 = VERTEX_POINT ( 'NONE', #24296 ) ;
#6209 = CARTESIAN_POINT ( 'NONE',  ( -29.76531599071173062, -3.714239038275569449, 12.97905452356682865 ) ) ;
#6210 = ORIENTED_EDGE ( 'NONE', *, *, #60031, .F. ) ;
#6211 = DIRECTION ( 'NONE',  ( 0.000000000000000000, -0.01356324068817998940, 0.9999080150203990547 ) ) ;
#6212 = CARTESIAN_POINT ( 'NONE',  ( -18.08686583997218733, 4.947294784127231893, 10.93504697000629911 ) ) ;
#6213 = EDGE_CURVE ( 'NONE', #64826, #22962, #34274, .T. ) ;
#6214 = DIRECTION ( 'NONE',  ( 0.000000000000000000, -0.1740410799127470320, -0.9847383929261643853 ) ) ;
#6215 = VERTEX_POINT ( 'NONE', #33940 ) ;
#6216 = CARTESIAN_POINT ( 'NONE',  ( 0.000000000000000000, 0.000000000000000000, 0.000000000000000000 ) ) ;
#6217 =( BOUNDED_CURVE ( )  B_SPLINE_CURVE ( 3, ( #56940, #42248, #37624, #46300 ),
 .UNSPECIFIED., .F., .F. ) 
 B_SPLINE_CURVE_WITH_KNOTS ( ( 4, 4 ),
 ( 0.8821975705743981822, 0.9242421917074130633 ),
 .UNSPECIFIED. ) 
 CURVE ( )  GEOMETRIC_REPRESENTATION_ITEM ( )  RATIONAL_B_SPLINE_CURVE ( ( 1.000000000000000000, 0.9998526929113126238, 0.9998526929113126238, 1.000000000000000000 ) ) 
 REPRESENTATION_ITEM ( '' )  );
#6218 = CARTESIAN_POINT ( 'NONE',  ( 0.2646305136544065406, 1.996350543473153216, -12.08286001766533602 ) ) ;
#6219 = DIRECTION ( 'NONE',  ( 0.000000000000000000, -1.000000000000000000, 0.000000000000000000 ) ) ;
#6220 = ORIENTED_EDGE ( 'NONE', *, *, #181, .T. ) ;
#6221 = VERTEX_POINT ( 'NONE', #64521 ) ;
#6222 = CARTESIAN_POINT ( 'NONE',  ( 2.256373768223412846, -7.223078030710452069, -2.487510024221244009 ) ) ;
#6223 = EDGE_CURVE ( 'NONE', #60104, #28065, #2690, .T. ) ;
#6224 = ORIENTED_EDGE ( 'NONE', *, *, #37212, .F. ) ;
#6225 = LINE ( 'NONE', #5581, #33781 ) ;
#6226 = CARTESIAN_POINT ( 'NONE',  ( 0.3040950598368144520, 5.912066680610613467, 10.74226959800793679 ) ) ;
#6227 = DIRECTION ( 'NONE',  ( 1.000000000000000000, 0.000000000000000000, 0.000000000000000000 ) ) ;
#6228 = DIRECTION ( 'NONE',  ( -1.000000000000000000, 0.000000000000000000, -0.000000000000000000 ) ) ;
#6229 = DIRECTION ( 'NONE',  ( 0.000000000000000000, -0.01356324068817999114, 0.9999080150203989437 ) ) ;
#6230 = DIRECTION ( 'NONE',  ( 0.000000000000000000, 0.6478160128811893959, -0.7617968321374923857 ) ) ;
#6231 = ADVANCED_FACE ( 'NONE', ( #39258 ), #18992, .T. ) ;
#6232 = FACE_OUTER_BOUND ( 'NONE', #38088, .T. ) ;
#6233 = ORIENTED_EDGE ( 'NONE', *, *, #40531, .F. ) ;
#6234 = CARTESIAN_POINT ( 'NONE',  ( 35.00000000000000000, 4.705694406421931860E-17, -3.469127814946512892E-15 ) ) ;
#6235 = CIRCLE ( 'NONE', #23219, 12.18650000000000411 ) ;
#6236 = DIRECTION ( 'NONE',  ( -1.000000000000000000, 0.000000000000000000, 0.000000000000000000 ) ) ;
#6237 = EDGE_CURVE ( 'NONE', #24509, #33400, #58371, .T. ) ;
#6238 = CARTESIAN_POINT ( 'NONE',  ( 35.00000000000000000, -11.37311665002365579, -2.936739658819832677 ) ) ;
#6239 = DIRECTION ( 'NONE',  ( -1.000000000000000000, 0.000000000000000000, 0.000000000000000000 ) ) ;
#6240 = CARTESIAN_POINT ( 'NONE',  ( -35.00000000000000000, 8.551552972817082932, 8.052525312709914118 ) ) ;
#6241 = DIRECTION ( 'NONE',  ( -1.000000000000000000, -0.000000000000000000, -0.000000000000000000 ) ) ;
#6242 = VECTOR ( 'NONE', #26711, 1000.000000000000000 ) ;
#6243 = ORIENTED_EDGE ( 'NONE', *, *, #62896, .F. ) ;
#6244 = ORIENTED_EDGE ( 'NONE', *, *, #25082, .T. ) ;
#6245 = CARTESIAN_POINT ( 'NONE',  ( 2.000000000000001776, 0.000000000000000000, 0.000000000000000000 ) ) ;
#6246 = VECTOR ( 'NONE', #53938, 1000.000000000000000 ) ;
#6247 = AXIS2_PLACEMENT_3D ( 'NONE', #50702, #25755, #56326 ) ;
#6248 = ORIENTED_EDGE ( 'NONE', *, *, #52920, .T. ) ;
#6249 = CARTESIAN_POINT ( 'NONE',  ( -22.30078715814471835, -3.743307663037635180, 0.2606204736986815207 ) ) ;
#6250 = ADVANCED_FACE ( 'NONE', ( #14315 ), #54890, .T. ) ;
#6251 = CARTESIAN_POINT ( 'NONE',  ( -15.93470253878248322, 7.893290767330796598, -10.95207400281732113 ) ) ;
#6252 = AXIS2_PLACEMENT_3D ( 'NONE', #12661, #53255, #54580 ) ;
#6253 = CARTESIAN_POINT ( 'NONE',  ( 5.516018279890452902, 0.006629829924290974764, 0.001397286410094337149 ) ) ;
#6254 = DIRECTION ( 'NONE',  ( 1.000000000000000000, 0.000000000000000000, 0.000000000000000000 ) ) ;
#6255 = EDGE_CURVE ( 'NONE', #60004, #1502, #43154, .T. ) ;
#6256 = ORIENTED_EDGE ( 'NONE', *, *, #54436, .T. ) ;
#6257 = CARTESIAN_POINT ( 'NONE',  ( 2.889800649504073782, -5.774917447013012683, 2.030191121417117106 ) ) ;
#6258 = DIRECTION ( 'NONE',  ( 0.000000000000000000, 0.01356324068817998940, -0.9999080150203990547 ) ) ;
#6259 = CARTESIAN_POINT ( 'NONE',  ( 1.020182472822701358, -12.37761526492762876, 1.729367949134579918 ) ) ;
#6260 = CIRCLE ( 'NONE', #42284, 5.000000000000001776 ) ;
#6261 = CARTESIAN_POINT ( 'NONE',  ( -41.46388549984529703, -1.589384660823694562, 18.83126657550987559 ) ) ;
#6262 = EDGE_CURVE ( 'NONE', #20337, #25571, #47734, .T. ) ;
#6263 = EDGE_CURVE ( 'NONE', #53784, #4915, #40571, .T. ) ;
#6264 = ADVANCED_FACE ( 'NONE', ( #683 ), #2141, .F. ) ;
#6265 = DIRECTION ( 'NONE',  ( 0.000000000000000000, 0.000000000000000000, 1.000000000000000000 ) ) ;
#6266 = CARTESIAN_POINT ( 'NONE',  ( 2.251152103363646351, 2.729599998984407083, 7.133254101175193540 ) ) ;
#6267 = EDGE_LOOP ( 'NONE', ( #60858, #4504, #29415, #39487 ) ) ;
#6269 = EDGE_CURVE ( 'NONE', #35192, #12635, #20940, .T. ) ;
#6268 = CARTESIAN_POINT ( 'NONE',  ( -37.00000000000000711, 0.000000000000000000, 0.000000000000000000 ) ) ;
#6270 = VERTEX_POINT ( 'NONE', #45555 ) ;
#6271 = CARTESIAN_POINT ( 'NONE',  ( -2.532614230583026593, -7.965877694534051479, 10.89930238848911337 ) ) ;
#6272 = CYLINDRICAL_SURFACE ( 'NONE', #41579, 5.000000000000000888 ) ;
#6273 = CARTESIAN_POINT ( 'NONE',  ( 0.3675815128205894289, -9.574637318042015011, 7.689697408877242957 ) ) ;
#6274 = CARTESIAN_POINT ( 'NONE',  ( 28.91057078075369802, -9.499749482217620056, 7.335151099638228978 ) ) ;
#6275 = CARTESIAN_POINT ( 'NONE',  ( -4.975205859172452172, -1.416020129149132778, 11.91616074890920451 ) ) ;
#6276 = CIRCLE ( 'NONE', #43416, 12.75000000000000178 ) ;
#6277 = ORIENTED_EDGE ( 'NONE', *, *, #4876, .T. ) ;
#6278 = ORIENTED_EDGE ( 'NONE', *, *, #50608, .T. ) ;
#6279 = CARTESIAN_POINT ( 'NONE',  ( 35.00000000000000000, 11.37311665002363270, 2.936739658819908616 ) ) ;
#6280 = ORIENTED_EDGE ( 'NONE', *, *, #60352, .T. ) ;
#6281 = CARTESIAN_POINT ( 'NONE',  ( -27.08416781016246588, -2.253489850813972240, 0.4141677382007513675 ) ) ;
#6282 = FACE_OUTER_BOUND ( 'NONE', #29358, .T. ) ;
#6283 = CARTESIAN_POINT ( 'NONE',  ( 1.000000000000000888, -1.693411908627245221, 7.306323022404576761 ) ) ;
#6284 = CARTESIAN_POINT ( 'NONE',  ( 1.719304012339844867, -11.67935079956417610, 5.066286238786176455 ) ) ;
#6285 = CARTESIAN_POINT ( 'NONE',  ( 0.9296196016843308874, -7.691217109781701033, -9.812579935705461054 ) ) ;
#6286 = CARTESIAN_POINT ( 'NONE',  ( 1.020182472824531450, 11.03967505355455714, -5.858468047365605003 ) ) ;
#6287 = DIRECTION ( 'NONE',  ( -1.000000000000000000, -0.000000000000000000, -0.000000000000000000 ) ) ;
#6288 = VERTEX_POINT ( 'NONE', #26271 ) ;
#6289 = CARTESIAN_POINT ( 'NONE',  ( 5.514970785353741078, 0.002093325033903813397, -0.004233694591582959355 ) ) ;
#6290 = ORIENTED_EDGE ( 'NONE', *, *, #592, .F. ) ;
#6291 = DIRECTION ( 'NONE',  ( -1.000000000000000000, 0.000000000000000000, -0.000000000000000000 ) ) ;
#6292 = CARTESIAN_POINT ( 'NONE',  ( 17.31227647733753017, 10.56962781760056380, 8.406781232797083447 ) ) ;
#6293 = EDGE_CURVE ( 'NONE', #52168, #28250, #17478, .T. ) ;
#6294 = ORIENTED_EDGE ( 'NONE', *, *, #12088, .T. ) ;
#6295 = CYLINDRICAL_SURFACE ( 'NONE', #42554, 12.75000000000000178 ) ;
#6297 = ORIENTED_EDGE ( 'NONE', *, *, #49771, .F. ) ;
#6296 = AXIS2_PLACEMENT_3D ( 'NONE', #54839, #4296, #31516 ) ;
#6298 = CARTESIAN_POINT ( 'NONE',  ( 2.000000000000001776, -0.3246585432986597852, 6.805031400696099020 ) ) ;
#6299 = CARTESIAN_POINT ( 'NONE',  ( -16.47895549814540317, -34.42947327577542893, -6.127516784536645389 ) ) ;
#6300 = DIRECTION ( 'NONE',  ( -1.000000000000000000, 0.000000000000000000, 0.000000000000000000 ) ) ;
#6301 = EDGE_LOOP ( 'NONE', ( #17092, #1236, #14500, #25660 ) ) ;
#6302 = ORIENTED_EDGE ( 'NONE', *, *, #8939, .T. ) ;
#6303 = CARTESIAN_POINT ( 'NONE',  ( 0.2646305136544065406, -2.256625640822235379, -12.03696649559616993 ) ) ;
#6304 = VERTEX_POINT ( 'NONE', #26589 ) ;
#6305 = CARTESIAN_POINT ( 'NONE',  ( 12.52750123246316072, 0.4973700281276248192, 25.00000000000000000 ) ) ;
#6306 = VERTEX_POINT ( 'NONE', #30917 ) ;
#6307 = EDGE_CURVE ( 'NONE', #28230, #52982, #40912, .T. ) ;
#6308 = ORIENTED_EDGE ( 'NONE', *, *, #59465, .F. ) ;
#6309 = AXIS2_PLACEMENT_3D ( 'NONE', #17448, #37722, #7445 ) ;
#6310 = ORIENTED_EDGE ( 'NONE', *, *, #26584, .F. ) ;
#6311 = CARTESIAN_POINT ( 'NONE',  ( 2.907497136250123848, -5.781215374755555025, 5.319973245618085045 ) ) ;
#6312 = CARTESIAN_POINT ( 'NONE',  ( 2.255723233588638355, 5.010912740807773602, -5.766109278028810792 ) ) ;
#6313 = DIRECTION ( 'NONE',  ( -1.000000000000000000, 0.000000000000000000, 0.000000000000000000 ) ) ;
#6314 = CARTESIAN_POINT ( 'NONE',  ( 0.000000000000000000, -6.883677378339468689, 0.8544109087185604023 ) ) ;
#6315 = CARTESIAN_POINT ( 'NONE',  ( -37.00000000000000711, 11.47758908105694786, 2.497432891016883261 ) ) ;
#6316 = ORIENTED_EDGE ( 'NONE', *, *, #49829, .T. ) ;
#6317 = CARTESIAN_POINT ( 'NONE',  ( -35.00000000000000000, -4.400442035671030538, 11.96656215839367299 ) ) ;
#6318 = EDGE_LOOP ( 'NONE', ( #58486, #15188, #7829, #17643 ) ) ;
#6319 = CARTESIAN_POINT ( 'NONE',  ( -29.43980975494970309, -3.641506875706034041, -12.99959336572439561 ) ) ;
#6320 = CARTESIAN_POINT ( 'NONE',  ( -22.27709082389155171, 2.641652894015124708, -2.563977319272113586 ) ) ;
#6321 = DIRECTION ( 'NONE',  ( 1.000000000000000000, -0.000000000000000000, 0.000000000000000000 ) ) ;
#6322 = EDGE_CURVE ( 'NONE', #62732, #63634, #42960, .T. ) ;
#6323 = CARTESIAN_POINT ( 'NONE',  ( 0.3053067050349149714, -2.355726819985503262, 12.03105545708856106 ) ) ;
#6324 = FACE_OUTER_BOUND ( 'NONE', #62203, .T. ) ;
#6325 = CARTESIAN_POINT ( 'NONE',  ( 0.6511581176972880414, -10.54760823437317008, -6.471755598256867081 ) ) ;
#6326 = EDGE_CURVE ( 'NONE', #54096, #44256, #34319, .T. ) ;
#6327 = AXIS2_PLACEMENT_3D ( 'NONE', #44494, #34531, #18925 ) ;
#6328 = VERTEX_POINT ( 'NONE', #21271 ) ;
#6329 = AXIS2_PLACEMENT_3D ( 'NONE', #35655, #26028, #437 ) ;
#6330 = ORIENTED_EDGE ( 'NONE', *, *, #53074, .F. ) ;
#6331 = CARTESIAN_POINT ( 'NONE',  ( 0.3341166715381310159, 10.74942732659231837, 5.914486946113945542 ) ) ;
#6332 = CARTESIAN_POINT ( 'NONE',  ( -12.41459945261391162, -27.32694502519497348, -12.80960016232523202 ) ) ;
#6333 = CARTESIAN_POINT ( 'NONE',  ( 2.770579946183330478, 6.173813901927609926, -4.784693811915826878 ) ) ;
#6334 = CYLINDRICAL_SURFACE ( 'NONE', #47913, 2.899999999999994582 ) ;
#6335 = DIRECTION ( 'NONE',  ( -1.000000000000000000, 0.000000000000000000, -0.000000000000000000 ) ) ;
#6336 = VERTEX_POINT ( 'NONE', #41546 ) ;
#6337 = CARTESIAN_POINT ( 'NONE',  ( 41.00000000000000711, 5.493969937218003549E-16, -4.500000000000000888 ) ) ;
#6338 = DIRECTION ( 'NONE',  ( 1.000000000000000000, -0.000000000000000000, -0.000000000000000000 ) ) ;
#6339 = CARTESIAN_POINT ( 'NONE',  ( 3.152665057735980714, 1.848755561853925533, 7.719888720907654545 ) ) ;
#6340 = CARTESIAN_POINT ( 'NONE',  ( 21.94561096463932870, -13.06103434740021108, -3.434726814316783727 ) ) ;
#6341 = B_SPLINE_CURVE_WITH_KNOTS ( 'NONE', 3,
 ( #2279, #47187, #42151, #7930, #23206, #43465, #17574, #2940, #18224, #6618, #32182, #52506, #37514, #58463, #38495, #57819, #37843, #63745, #62438 ),
 .UNSPECIFIED., .F., .F.,
 ( 4, 3, 3, 3, 3, 3, 4 ),
 ( 6.508826038821074665E-18, 2.825908398831552076E-05, 4.208813692484427327E-05, 5.591713746944529178E-05, 6.279584083232600446E-05, 9.105792820297518039E-05, 0.0001153131102488865703 ),
 .UNSPECIFIED. ) ;
#6342 = EDGE_CURVE ( 'NONE', #62669, #50699, #16298, .T. ) ;
#6343 = VECTOR ( 'NONE', #42, 1000.000000000000000 ) ;
#6344 = ADVANCED_FACE ( 'NONE', ( #6324 ), #58684, .F. ) ;
#6345 = CARTESIAN_POINT ( 'NONE',  ( -37.00000000000000711, 0.000000000000000000, 0.000000000000000000 ) ) ;
#6347 = EDGE_CURVE ( 'NONE', #58400, #9014, #27909, .T. ) ;
#6346 = CYLINDRICAL_SURFACE ( 'NONE', #42366, 5.000000000000000888 ) ;
#6348 = DIRECTION ( 'NONE',  ( 1.000000000000000000, 0.000000000000000000, 0.000000000000000000 ) ) ;
#6349 = CARTESIAN_POINT ( 'NONE',  ( -27.08429572838383947, 1.632445743623435197, -1.608131779585709076 ) ) ;
#6350 = DIRECTION ( 'NONE',  ( 1.000000000000000000, 0.000000000000000000, 0.000000000000000000 ) ) ;
#6351 = AXIS2_PLACEMENT_3D ( 'NONE', #57578, #11997, #32279 ) ;
#6352 = ADVANCED_FACE ( 'NONE', ( #22597 ), #27248, .T. ) ;
#6353 = ORIENTED_EDGE ( 'NONE', *, *, #19207, .T. ) ;
#6354 = ORIENTED_EDGE ( 'NONE', *, *, #52931, .T. ) ;
#6355 = CARTESIAN_POINT ( 'NONE',  ( 2.430348790457504293, -6.566563360302382080, 4.016278121583770400 ) ) ;
#6356 = CARTESIAN_POINT ( 'NONE',  ( 43.04762206662383761, -1.319502909267364243, -15.89732852394791784 ) ) ;
#6357 = FACE_OUTER_BOUND ( 'NONE', #10917, .T. ) ;
#6358 = CARTESIAN_POINT ( 'NONE',  ( 36.00000000000000711, 12.54989509947654192, 2.250029553613614564 ) ) ;
#6359 = ORIENTED_EDGE ( 'NONE', *, *, #37005, .F. ) ;
#6360 = EDGE_LOOP ( 'NONE', ( #35528, #26225, #10770, #8747 ) ) ;
#6361 = ORIENTED_EDGE ( 'NONE', *, *, #15168, .F. ) ;
#6362 = FACE_OUTER_BOUND ( 'NONE', #16068, .T. ) ;
#6364 = DIRECTION ( 'NONE',  ( -1.000000000000000000, 0.000000000000000000, 0.000000000000000000 ) ) ;
#6363 = AXIS2_PLACEMENT_3D ( 'NONE', #59574, #39936, #34293 ) ;
#6365 = VECTOR ( 'NONE', #45157, 1000.000000000000000 ) ;
#6366 = EDGE_LOOP ( 'NONE', ( #54406, #33944, #1785, #34109 ) ) ;
#6367 = CARTESIAN_POINT ( 'NONE',  ( -37.00000000000000711, -12.74921544981111055, 0.1414404973751688388 ) ) ;
#6368 = CYLINDRICAL_SURFACE ( 'NONE', #41684, 2.899999999999994582 ) ;
#6369 = ADVANCED_FACE ( 'NONE', ( #32538 ), #32868, .T. ) ;
#6370 = EDGE_LOOP ( 'NONE', ( #16511, #54228, #48420, #61154 ) ) ;
#6371 = CARTESIAN_POINT ( 'NONE',  ( 19.67311005600952711, -0.7004819783312107306, 25.00000000000000000 ) ) ;
#6372 = CIRCLE ( 'NONE', #42406, 6.936499999999987232 ) ;
#6373 = CARTESIAN_POINT ( 'NONE',  ( 14.42557999471933705, -30.05477271089583269, -4.241434648442556465 ) ) ;
#6374 = CARTESIAN_POINT ( 'NONE',  ( 24.17672931252117152, -3.380230056746429401, 11.51978025207018241 ) ) ;
#6375 = ORIENTED_EDGE ( 'NONE', *, *, #29339, .T. ) ;
#6376 = CARTESIAN_POINT ( 'NONE',  ( 0.2706063244538051693, 12.09107863371559866, -1.954041462022295450 ) ) ;
#6377 = EDGE_LOOP ( 'NONE', ( #60681, #56289, #4877, #8261 ) ) ;
#6378 = DIRECTION ( 'NONE',  ( 1.000000000000000000, 0.000000000000000000, -0.000000000000000000 ) ) ;
#6379 = ADVANCED_FACE ( 'NONE', ( #47227 ), #21942, .T. ) ;
#6380 = FACE_OUTER_BOUND ( 'NONE', #38848, .T. ) ;
#6381 = CARTESIAN_POINT ( 'NONE',  ( -6.008663266758395238, -31.76136623419596106, 13.60005156548239036 ) ) ;
#6382 = CARTESIAN_POINT ( 'NONE',  ( -37.00000000000000711, 0.000000000000000000, 0.000000000000000000 ) ) ;
#6383 = FACE_OUTER_BOUND ( 'NONE', #16647, .T. ) ;
#6384 = LINE ( 'NONE', #31956, #3271 ) ;
#6385 = CARTESIAN_POINT ( 'NONE',  ( 0.3675815128205912052, 6.367184624550311867, -10.50067073900645198 ) ) ;
#6386 = CARTESIAN_POINT ( 'NONE',  ( 0.000000000000000000, 5.585096664091945939, 4.113602740025928739 ) ) ;
#6387 = ORIENTED_EDGE ( 'NONE', *, *, #36887, .F. ) ;
#6388 = CARTESIAN_POINT ( 'NONE',  ( -22.70624764888619751, -4.097886656202274658, -3.282666355490689192 ) ) ;
#6389 = ORIENTED_EDGE ( 'NONE', *, *, #65123, .T. ) ;
#6390 = CARTESIAN_POINT ( 'NONE',  ( -35.00000000000000000, 0.000000000000000000, 0.000000000000000000 ) ) ;
#6391 = CARTESIAN_POINT ( 'NONE',  ( 2.899286259009692390, -5.780956296532483663, -5.316140236670832131 ) ) ;
#6392 = EDGE_CURVE ( 'NONE', #46044, #57324, #23579, .T. ) ;
#6393 = ADVANCED_FACE ( 'NONE', ( #37210 ), #7969, .T. ) ;
#6394 = VERTEX_POINT ( 'NONE', #57525 ) ;
#6395 = CARTESIAN_POINT ( 'NONE',  ( 3.152665057736252940, 7.609997527622067715, 2.258875078500286016 ) ) ;
#6396 = CARTESIAN_POINT ( 'NONE',  ( 5.536195898058073439, 0.007485416011287806572, -0.004027525919832459014 ) ) ;
#6397 = VECTOR ( 'NONE', #35220, 1000.000000000000000 ) ;
#6398 = CARTESIAN_POINT ( 'NONE',  ( -27.10512513516275845, -2.256292013315179812, 0.6711200423626850764 ) ) ;
#6399 = CARTESIAN_POINT ( 'NONE',  ( -22.27384469013076185, -3.548341908721032389, -0.9835229356382479970 ) ) ;
#6400 = EDGE_CURVE ( 'NONE', #38220, #46560, #19126, .T. ) ;
#6401 = CARTESIAN_POINT ( 'NONE',  ( 2.241317068080788122, 7.204761327831662676, 2.524952427347059825 ) ) ;
#6402 = ORIENTED_EDGE ( 'NONE', *, *, #46576, .T. ) ;
#6403 = CARTESIAN_POINT ( 'NONE',  ( -37.00000000000000711, -6.475373545682229448, -10.32377448871674908 ) ) ;
#6404 = ORIENTED_EDGE ( 'NONE', *, *, #44870, .F. ) ;
#6405 = DIRECTION ( 'NONE',  ( 0.000000000000000000, -1.000000000000000000, 0.000000000000000000 ) ) ;
#6406 = FACE_OUTER_BOUND ( 'NONE', #18161, .T. ) ;
#6407 = CARTESIAN_POINT ( 'NONE',  ( 35.00000000000000000, 5.865551165831078606, -11.32068061209297483 ) ) ;
#6408 = EDGE_LOOP ( 'NONE', ( #48471, #63028, #59772, #24919 ) ) ;
#6409 = CARTESIAN_POINT ( 'NONE',  ( -27.09729107899804390, -1.021938248125916271, 2.094470452260984494 ) ) ;
#6410 = ADVANCED_FACE ( 'NONE', ( #6974 ), #37558, .T. ) ;
#6411 = B_SPLINE_CURVE_WITH_KNOTS ( 'NONE', 3,
 ( #15175, #20165, #30148, #35107, #55419, #45766, #25479, #46115, #10502, #25157, #56062, #35455, #11180, #26461, #10185, #25822, #30465, #61067, #45428 ),
 .UNSPECIFIED., .F., .F.,
 ( 4, 3, 3, 3, 3, 3, 4 ),
 ( 1.099757308482672315E-17, 4.457896483014753801E-05, 6.639290541542144030E-05, 8.820687556479127171E-05, 0.0001100173248778949181, 0.0001545671401658163307, 0.0001830328308068594713 ),
 .UNSPECIFIED. ) ;
#6412 = CIRCLE ( 'NONE', #52068, 12.18650000000000055 ) ;
#6413 = AXIS2_PLACEMENT_3D ( 'NONE', #48306, #3404, #23013 ) ;
#6414 = AXIS2_PLACEMENT_3D ( 'NONE', #58363, #7827, #63647 ) ;
#6415 = DIRECTION ( 'NONE',  ( 0.000000000000000000, 0.000000000000000000, 1.000000000000000000 ) ) ;
#6416 =( BOUNDED_SURFACE ( )  B_SPLINE_SURFACE ( 3, 1, ( 
 ( #28535, #24526 ),
 ( #39823, #23228 ),
 ( #53827, #49178 ),
 ( #59147, #2966 ) ),
 .UNSPECIFIED., .F., .F., .F. ) 
 B_SPLINE_SURFACE_WITH_KNOTS ( ( 4, 4 ),
 ( 2, 2 ),
 ( 0.000000000000000000, 1.000000000000000000 ),
 ( 0.000000000000000000, 1.000000000000000000 ),
 .UNSPECIFIED. ) 
 GEOMETRIC_REPRESENTATION_ITEM ( )  RATIONAL_B_SPLINE_SURFACE ( (
 ( 1.000000000000000000, 1.000000000000000000),
 ( 0.9856612449720755231, 0.9999558406602322425),
 ( 0.9856612449720755231, 0.9999558406602322425),
 ( 1.000000000000000000, 1.000000000000000000) ) ) 
 REPRESENTATION_ITEM ( '' )  SURFACE ( )  );
#6417 = CARTESIAN_POINT ( 'NONE',  ( 2.177405672432018324, 0.6747479782259074854, 11.17876532285389146 ) ) ;
#6418 = DIRECTION ( 'NONE',  ( 0.000000000000000000, -0.7790879021242573810, 0.6269146997507903940 ) ) ;
#6419 = DIRECTION ( 'NONE',  ( 1.000000000000000000, 0.000000000000000000, 0.000000000000000000 ) ) ;
#6420 = CARTESIAN_POINT ( 'NONE',  ( 35.00000000000000000, -11.98254675519226531, 2.220215194442026974 ) ) ;
#6421 = CARTESIAN_POINT ( 'NONE',  ( 1.719304012338833676, 5.066286238785588480, 11.67935079956406597 ) ) ;
#6422 = DIRECTION ( 'NONE',  ( 0.000000000000000000, -0.7621620551276288014, -0.6473862847818365740 ) ) ;
#6423 = CIRCLE ( 'NONE', #10673, 12.74999999999999822 ) ;
#6424 = ORIENTED_EDGE ( 'NONE', *, *, #28011, .T. ) ;
#6425 = CARTESIAN_POINT ( 'NONE',  ( -17.29810829516095794, 7.115115252187681705, 11.47444202231375598 ) ) ;
#6426 = DIRECTION ( 'NONE',  ( -1.000000000000000000, -0.000000000000000000, -0.000000000000000000 ) ) ;
#6427 = AXIS2_PLACEMENT_3D ( 'NONE', #51328, #452, #16392 ) ;
#6428 = EDGE_LOOP ( 'NONE', ( #29084, #32774, #65446, #4452 ) ) ;
#6429 = CARTESIAN_POINT ( 'NONE',  ( 35.00000000000000000, 4.705694406421931860E-17, -3.469127814946512892E-15 ) ) ;
#6430 = CARTESIAN_POINT ( 'NONE',  ( -37.00000000000000711, 10.84030624090606665, 6.711949091238182064 ) ) ;
#6431 = VERTEX_POINT ( 'NONE', #32229 ) ;
#6432 = CARTESIAN_POINT ( 'NONE',  ( -35.04709527796842394, -0.005292201869334239861, -0.01117341439756461274 ) ) ;
#6433 = ORIENTED_EDGE ( 'NONE', *, *, #57835, .F. ) ;
#6434 = AXIS2_PLACEMENT_3D ( 'NONE', #62228, #31324, #51625 ) ;
#6435 = CARTESIAN_POINT ( 'NONE',  ( 0.2767916011545419885, -5.959903879715655606, 10.70244578860293139 ) ) ;
#6436 = ORIENTED_EDGE ( 'NONE', *, *, #27493, .T. ) ;
#6437 = ORIENTED_EDGE ( 'NONE', *, *, #38872, .F. ) ;
#6438 = CARTESIAN_POINT ( 'NONE',  ( 35.00000000000000000, 4.705694406421931860E-17, -3.469127814946512892E-15 ) ) ;
#6439 = ORIENTED_EDGE ( 'NONE', *, *, #1389, .T. ) ;
#6440 = CARTESIAN_POINT ( 'NONE',  ( -24.90381799016406461, -9.122167393312837547, 7.798732004451876421 ) ) ;
#6441 = CARTESIAN_POINT ( 'NONE',  ( -37.25000000000000711, -27.21021009056489248, -4.500000000000000888 ) ) ;
#6442 = CARTESIAN_POINT ( 'NONE',  ( -35.00000000000000000, -6.303578524886872536, -10.42955799785326576 ) ) ;
#6443 = CARTESIAN_POINT ( 'NONE',  ( 35.00000000000000000, 4.705694406421931860E-17, -3.469127814946512892E-15 ) ) ;
#6444 = EDGE_CURVE ( 'NONE', #29772, #43237, #17616, .T. ) ;
#6445 = ORIENTED_EDGE ( 'NONE', *, *, #57163, .F. ) ;
#6446 = CARTESIAN_POINT ( 'NONE',  ( 35.00000000000000000, -2.021542716731485001, -12.01765980939841327 ) ) ;
#6447 = CARTESIAN_POINT ( 'NONE',  ( -2.167161191928854258, -27.87656208324061069, 12.44306432472098756 ) ) ;
#6448 = CARTESIAN_POINT ( 'NONE',  ( 5.516018279890452902, -0.003191189039764880282, -0.005976902763919027944 ) ) ;
#6450 = ORIENTED_EDGE ( 'NONE', *, *, #32469, .T. ) ;
#6449 = DIRECTION ( 'NONE',  ( 0.000000000000000000, 0.3193015301359743985, 0.9476531711828043436 ) ) ;
#6452 = AXIS2_PLACEMENT_3D ( 'NONE', #65057, #4898, #15178 ) ;
#6451 = CARTESIAN_POINT ( 'NONE',  ( -18.04458733766117362, -12.91933584589293282, 3.916728392552376370 ) ) ;
#6453 = ORIENTED_EDGE ( 'NONE', *, *, #8010, .T. ) ;
#6454 = CARTESIAN_POINT ( 'NONE',  ( 2.990245332647846421, 3.789007530133591484, 7.587819667496370712 ) ) ;
#6455 = ORIENTED_EDGE ( 'NONE', *, *, #33540, .T. ) ;
#6456 = LINE ( 'NONE', #27067, #46454 ) ;
#6457 = DIRECTION ( 'NONE',  ( 1.000000000000000000, 0.000000000000000000, 0.000000000000000000 ) ) ;
#6458 = CARTESIAN_POINT ( 'NONE',  ( 2.247206125382827047, -7.635476611656036638, -0.1157489416152311518 ) ) ;
#6459 = CIRCLE ( 'NONE', #42500, 12.75000000000000178 ) ;
#6460 = ORIENTED_EDGE ( 'NONE', *, *, #30627, .T. ) ;
#6461 = EDGE_CURVE ( 'NONE', #24932, #63728, #12695, .T. ) ;
#6463 = CIRCLE ( 'NONE', #10717, 12.74999999999999822 ) ;
#6462 = CARTESIAN_POINT ( 'NONE',  ( 1.194176325881339595, 8.457794872459121649, 9.279760592562121602 ) ) ;
#6464 = CARTESIAN_POINT ( 'NONE',  ( 0.2638984909335720941, 12.02508546958700109, -2.322601104020543872 ) ) ;
#6465 = CARTESIAN_POINT ( 'NONE',  ( 0.2671309869109492752, -12.03155065772886623, 2.286013846429986618 ) ) ;
#6466 = EDGE_LOOP ( 'NONE', ( #4599, #38624, #19733, #38902 ) ) ;
#6467 = ORIENTED_EDGE ( 'NONE', *, *, #45658, .T. ) ;
#6468 = CYLINDRICAL_SURFACE ( 'NONE', #47589, 5.000000000000000888 ) ;
#6469 = ORIENTED_EDGE ( 'NONE', *, *, #43077, .T. ) ;
#6470 = EDGE_CURVE ( 'NONE', #22718, #19643, #49895, .T. ) ;
#6471 = ORIENTED_EDGE ( 'NONE', *, *, #50608, .F. ) ;
#6472 = CARTESIAN_POINT ( 'NONE',  ( 37.00000000000000711, 4.705694406421931860E-17, -3.469127814946512892E-15 ) ) ;
#6473 = DIRECTION ( 'NONE',  ( -1.000000000000000000, 0.000000000000000000, -0.000000000000000000 ) ) ;
#6474 = CARTESIAN_POINT ( 'NONE',  ( 35.00000000000000000, 7.817610399097634222, 8.766823244861901898 ) ) ;
#6475 = DIRECTION ( 'NONE',  ( 0.000000000000000000, 0.000000000000000000, 1.000000000000000000 ) ) ;
#6477 = AXIS2_PLACEMENT_3D ( 'NONE', #52821, #63122, #28520 ) ;
#6476 = CARTESIAN_POINT ( 'NONE',  ( -37.00000000000000711, 10.49591321039680736, 5.273331777780375873 ) ) ;
#6478 = VECTOR ( 'NONE', #65290, 1000.000000000000000 ) ;
#6479 = DIRECTION ( 'NONE',  ( -1.000000000000000000, 0.000000000000000000, 0.000000000000000000 ) ) ;
#6480 = CARTESIAN_POINT ( 'NONE',  ( 29.51976981715666781, 25.00000000000000000, 11.09513982864076276 ) ) ;
#6481 = CIRCLE ( 'NONE', #40436, 12.75000000000000178 ) ;
#6482 = CIRCLE ( 'NONE', #26637, 12.75000000000000178 ) ;
#6483 = ORIENTED_EDGE ( 'NONE', *, *, #29079, .T. ) ;
#6484 = CARTESIAN_POINT ( 'NONE',  ( -22.27945548916780183, -3.016427163003897238, 2.122548946923907387 ) ) ;
#6485 = CARTESIAN_POINT ( 'NONE',  ( -3.161163348754353120, -5.207994443204945867, 10.84706555580636511 ) ) ;
#6486 = AXIS2_PLACEMENT_3D ( 'NONE', #31253, #16284, #16614 ) ;
#6487 = B_SPLINE_CURVE_WITH_KNOTS ( 'NONE', 3,
 ( #15062, #15708, #10733, #36333 ),
 .UNSPECIFIED., .F., .F.,
 ( 4, 4 ),
 ( 5.898697549827394244E-18, 0.002289549871878519133 ),
 .UNSPECIFIED. ) ;
#6488 = CARTESIAN_POINT ( 'NONE',  ( 0.3160775863651120177, 4.419114254410051679, -11.43919651388221226 ) ) ;
#6489 = CARTESIAN_POINT ( 'NONE',  ( 2.241449424704145876, 3.763973574060632377, -6.642105568284066841 ) ) ;
#6490 = AXIS2_PLACEMENT_3D ( 'NONE', #420, #26011, #50632 ) ;
#6491 = CARTESIAN_POINT ( 'NONE',  ( 0.2648978790185619880, 12.03635331166815270, -2.256510822326019738 ) ) ;
#6492 = CARTESIAN_POINT ( 'NONE',  ( 37.00000000000000711, 5.644643009979216863, 10.30098186818242922 ) ) ;
#6493 = CIRCLE ( 'NONE', #58532, 12.75000000000000178 ) ;
#6494 = ORIENTED_EDGE ( 'NONE', *, *, #20060, .F. ) ;
#6495 = CARTESIAN_POINT ( 'NONE',  ( -40.99999999999999289, -25.49182303066451993, -1.512869109757708941 ) ) ;
#6496 = ADVANCED_FACE ( 'NONE', ( #38533 ), #58168, .T. ) ;
#6497 = CARTESIAN_POINT ( 'NONE',  ( 35.00000000000000000, 2.250029553613756228, -12.54989509947652060 ) ) ;
#6498 = CARTESIAN_POINT ( 'NONE',  ( 2.653899356900514039, 1.091629880170411848, -7.694895988366599937 ) ) ;
#6499 = CARTESIAN_POINT ( 'NONE',  ( -18.24403761432370175, -13.49999999999999822, 0.6264592723685493691 ) ) ;
#6500 = EDGE_CURVE ( 'NONE', #2095, #52731, #42513, .T. ) ;
#6501 = AXIS2_PLACEMENT_3D ( 'NONE', #7131, #17454, #23091 ) ;
#6502 = AXIS2_PLACEMENT_3D ( 'NONE', #42448, #26524, #56820 ) ;
#6503 = DIRECTION ( 'NONE',  ( -1.000000000000000000, 0.000000000000000000, 0.000000000000000000 ) ) ;
#6504 = CARTESIAN_POINT ( 'NONE',  ( -25.10029369095171248, -9.207521581778740583, 9.878167689217567826 ) ) ;
#6505 = ORIENTED_EDGE ( 'NONE', *, *, #2299, .T. ) ;
#6506 = DIRECTION ( 'NONE',  ( 0.000000000000000000, 0.000000000000000000, 1.000000000000000000 ) ) ;
#6507 = CARTESIAN_POINT ( 'NONE',  ( 35.00000000000000000, 4.705694406421931860E-17, -3.469127814946512892E-15 ) ) ;
#6508 = CARTESIAN_POINT ( 'NONE',  ( -35.04643116707788408, -0.009511118309140503824, 0.007621814750495559121 ) ) ;
#6509 = ORIENTED_EDGE ( 'NONE', *, *, #40319, .F. ) ;
#6510 = DIRECTION ( 'NONE',  ( -1.000000000000000000, 0.000000000000000000, -0.000000000000000000 ) ) ;
#6511 = DIRECTION ( 'NONE',  ( 0.000000000000000000, 0.01356324068817998940, -0.9999080150203990547 ) ) ;
#6512 = CARTESIAN_POINT ( 'NONE',  ( 0.2655924914740778187, -10.58356227062105148, -6.161287456391793427 ) ) ;
#6514 = ORIENTED_EDGE ( 'NONE', *, *, #20659, .T. ) ;
#6513 = CARTESIAN_POINT ( 'NONE',  ( 0.2648978790185584908, -12.24533305150758089, -0.1321385342563691223 ) ) ;
#6515 = DIRECTION ( 'NONE',  ( 0.000000000000000000, -0.01356324068817998940, 0.9999080150203990547 ) ) ;
#6516 = EDGE_CURVE ( 'NONE', #44564, #32447, #33217, .T. ) ;
#6517 = CARTESIAN_POINT ( 'NONE',  ( 32.00000000000000000, 15.00000000000000000, 0.000000000000000000 ) ) ;
#6518 = ORIENTED_EDGE ( 'NONE', *, *, #31940, .T. ) ;
#6519 = CIRCLE ( 'NONE', #19243, 5.000000000000000888 ) ;
#6520 = CYLINDRICAL_SURFACE ( 'NONE', #12082, 4.999999999999999112 ) ;
#6521 = DIRECTION ( 'NONE',  ( -1.000000000000000000, 0.000000000000000000, -0.000000000000000000 ) ) ;
#6522 = DIRECTION ( 'NONE',  ( 1.000000000000000000, -0.000000000000000000, 0.000000000000000000 ) ) ;
#6523 = CARTESIAN_POINT ( 'NONE',  ( -35.00000000000000000, 0.000000000000000000, 0.000000000000000000 ) ) ;
#6524 = EDGE_CURVE ( 'NONE', #43331, #60300, #40683, .T. ) ;
#6525 = DIRECTION ( 'NONE',  ( 0.8386510381079236298, 0.5446691071471760903, -0.000000000000000000 ) ) ;
#6526 = EDGE_CURVE ( 'NONE', #7525, #65358, #49822, .T. ) ;
#6527 = CIRCLE ( 'NONE', #35166, 7.938172270156617749 ) ;
#6528 = CARTESIAN_POINT ( 'NONE',  ( -10.95212338237647920, -9.902220863987562183, 9.175839033069923545 ) ) ;
#6530 = VERTEX_POINT ( 'NONE', #44175 ) ;
#6529 = CARTESIAN_POINT ( 'NONE',  ( 0.2647959493198570047, 11.45640103018464195, -4.326188315749620372 ) ) ;
#6531 = EDGE_CURVE ( 'NONE', #52659, #48378, #31960, .T. ) ;
#6532 = ORIENTED_EDGE ( 'NONE', *, *, #28608, .T. ) ;
#6533 = CARTESIAN_POINT ( 'NONE',  ( -29.92777678363736626, -3.750539801530011985, 12.96855624952674724 ) ) ;
#6534 = AXIS2_PLACEMENT_3D ( 'NONE', #34176, #65407, #49504 ) ;
#6535 = VERTEX_POINT ( 'NONE', #13894 ) ;
#6536 = CARTESIAN_POINT ( 'NONE',  ( 0.6473888112830247232, -11.51036712212683355, 4.540486098228939227 ) ) ;
#6537 = FACE_OUTER_BOUND ( 'NONE', #7933, .T. ) ;
#6538 = EDGE_CURVE ( 'NONE', #47492, #49777, #16141, .T. ) ;
#6539 = B_SPLINE_CURVE_WITH_KNOTS ( 'NONE', 3,
 ( #13492, #54420, #60051, #38450, #33776, #64678, #49111, #58767, #53762, #13188, #55048, #33471, #23835, #43423, #44098, #59387 ),
 .UNSPECIFIED., .F., .F.,
 ( 4, 3, 3, 3, 3, 4 ),
 ( 3.104202383059129028E-15, 0.0002126834539179675815, 0.0004253519300366209862, 0.0006380165497224082579, 0.0007442707582428152160, 0.0009453531351418435844 ),
 .UNSPECIFIED. ) ;
#6540 = FACE_OUTER_BOUND ( 'NONE', #63246, .T. ) ;
#6541 = ORIENTED_EDGE ( 'NONE', *, *, #51723, .T. ) ;
#6543 = CARTESIAN_POINT ( 'NONE',  ( 5.520433897694421610, 0.01006947824912450551, 0.01120198501134887781 ) ) ;
#6542 = AXIS2_PLACEMENT_3D ( 'NONE', #3636, #38854, #48841 ) ;
#6544 = LINE ( 'NONE', #11834, #34666 ) ;
#6546 = EDGE_CURVE ( 'NONE', #3310, #56510, #10517, .T. ) ;
#6545 = FACE_BOUND ( 'NONE', #27766, .T. ) ;
#6547 = VERTEX_POINT ( 'NONE', #23581 ) ;
#6548 = ORIENTED_EDGE ( 'NONE', *, *, #64067, .T. ) ;
#6549 = DIRECTION ( 'NONE',  ( 0.000000000000000000, 1.000000000000000000, 0.000000000000000000 ) ) ;
#6550 = CIRCLE ( 'NONE', #5515, 4.999999999999998224 ) ;
#6551 = AXIS2_PLACEMENT_3D ( 'NONE', #15084, #55669, #10752 ) ;
#6552 = EDGE_LOOP ( 'NONE', ( #14356, #18879, #14618, #36187 ) ) ;
#6553 = CARTESIAN_POINT ( 'NONE',  ( 35.00000000000000000, 4.705694406421931860E-17, -3.469127814946512892E-15 ) ) ;
#6554 = CARTESIAN_POINT ( 'NONE',  ( 29.03457606387295087, -4.854210015632035358, 10.97436308512422265 ) ) ;
#6555 = B_SPLINE_CURVE_WITH_KNOTS ( 'NONE', 3,
 ( #60285, #25367, #4792, #50980, #14711, #34990, #25054, #45325, #20057, #40321, #42598, #36658, #51964, #47953, #27323, #57275 ),
 .UNSPECIFIED., .F., .F.,
 ( 4, 3, 3, 3, 3, 4 ),
 ( 0.000000000000000000, 0.0002176109881720194434, 0.0004352086762394498788, 0.0006528017811446724375, 0.0007615147961451543875, 0.0009453342004946168253 ),
 .UNSPECIFIED. ) ;
#6556 = DIRECTION ( 'NONE',  ( 1.000000000000000000, 0.000000000000000000, 0.000000000000000000 ) ) ;
#6557 = CARTESIAN_POINT ( 'NONE',  ( 1.194176325881336043, 12.44396189284385024, 1.672143286119605055 ) ) ;
#6558 = AXIS2_PLACEMENT_3D ( 'NONE', #34546, #20236, #59500 ) ;
#6559 = CIRCLE ( 'NONE', #19328, 12.18649999999999878 ) ;
#6560 = CARTESIAN_POINT ( 'NONE',  ( -35.00000000000000000, 0.000000000000000000, 0.000000000000000000 ) ) ;
#6561 = CARTESIAN_POINT ( 'NONE',  ( 2.994568964204214812, -7.825096839971885210, 0.9739368093814469995 ) ) ;
#6562 = AXIS2_PLACEMENT_3D ( 'NONE', #63639, #33065, #3504 ) ;
#6563 = ADVANCED_FACE ( 'NONE', ( #38867 ), #13573, .T. ) ;
#6564 = CARTESIAN_POINT ( 'NONE',  ( -36.00000000000000711, 7.094637218249359556, 10.59380114696472752 ) ) ;
#6565 = ORIENTED_EDGE ( 'NONE', *, *, #26283, .F. ) ;
#6566 = CARTESIAN_POINT ( 'NONE',  ( 1.372161826075799507, 12.60140585080784703, -0.5897614319401539573 ) ) ;
#6567 = ORIENTED_EDGE ( 'NONE', *, *, #48177, .F. ) ;
#6568 = CARTESIAN_POINT ( 'NONE',  ( 0.2648978790185584908, 2.256510822326303956, -12.03635331166809941 ) ) ;
#6569 = DIRECTION ( 'NONE',  ( 0.000000000000000000, -0.4380125133593849029, 0.8989688749565220016 ) ) ;
#6570 = CARTESIAN_POINT ( 'NONE',  ( -9.146844076892975295, 9.365293060442926532, -7.512015364276853013 ) ) ;
#6571 = CARTESIAN_POINT ( 'NONE',  ( 37.00000000000000711, -11.50504120060945823, -4.018060380616357286 ) ) ;
#6572 = CARTESIAN_POINT ( 'NONE',  ( 0.3665391374699467075, 7.691255657244293609, 9.576575648339046509 ) ) ;
#6573 = CARTESIAN_POINT ( 'NONE',  ( -27.45775109278351067, -11.83395752356219255, -1.989333891161980894 ) ) ;
#6574 = AXIS2_PLACEMENT_3D ( 'NONE', #12817, #59062, #33753 ) ;
#6575 = EDGE_LOOP ( 'NONE', ( #34657, #51216 ) ) ;
#6576 = CIRCLE ( 'NONE', #64972, 12.75000000000000178 ) ;
#6577 = ORIENTED_EDGE ( 'NONE', *, *, #63735, .T. ) ;
#6578 = CARTESIAN_POINT ( 'NONE',  ( 2.000000000000001776, -3.859771122243078167, 5.613913289150019637 ) ) ;
#6579 = AXIS2_PLACEMENT_3D ( 'NONE', #22861, #18192, #63711 ) ;
#6580 = VERTEX_POINT ( 'NONE', #20204 ) ;
#6581 = DIRECTION ( 'NONE',  ( 0.000000000000000000, 0.9903235168508545128, 0.1387779952735854194 ) ) ;
#6582 = DIRECTION ( 'NONE',  ( -1.000000000000000000, -0.000000000000000000, 0.000000000000000000 ) ) ;
#6583 = VECTOR ( 'NONE', #17415, 1000.000000000000000 ) ;
#6584 = CARTESIAN_POINT ( 'NONE',  ( -37.00000000000000711, 11.16627499335650242, 3.645068577060221582 ) ) ;
#6585 = CARTESIAN_POINT ( 'NONE',  ( 2.249013661412228693, 1.444210756221647518, -7.499157010299421167 ) ) ;
#6586 = VERTEX_POINT ( 'NONE', #15852 ) ;
#6587 = CARTESIAN_POINT ( 'NONE',  ( 0.2650492433740075926, -6.218175523534217319, -10.54996000109281340 ) ) ;
#6589 = CIRCLE ( 'NONE', #43733, 5.000000000000000000 ) ;
#6588 = DIRECTION ( 'NONE',  ( 0.000000000000000000, 0.9903235168508555120, 0.1387779952735781475 ) ) ;
#6590 = CARTESIAN_POINT ( 'NONE',  ( 0.4626703367445803017, -12.17089897506931528, 1.858541096401158832 ) ) ;
#6591 = CARTESIAN_POINT ( 'NONE',  ( -48.66712064925836501, -0.2684213679329330304, 8.095633725969744177 ) ) ;
#6592 = EDGE_CURVE ( 'NONE', #20113, #21123, #34996, .T. ) ;
#6593 = CARTESIAN_POINT ( 'NONE',  ( 0.3675815128205912052, 6.367184624550311867, -10.50067073900645198 ) ) ;
#6594 = AXIS2_PLACEMENT_3D ( 'NONE', #33765, #48758, #8501 ) ;
#6595 = CARTESIAN_POINT ( 'NONE',  ( -17.29244623348158783, 2.525873743887551814, -11.73115347397429176 ) ) ;
#6596 = ORIENTED_EDGE ( 'NONE', *, *, #14140, .F. ) ;
#6597 = CARTESIAN_POINT ( 'NONE',  ( -12.58062741647496274, -29.25281707778071549, -4.759732266940785550 ) ) ;
#6598 = ORIENTED_EDGE ( 'NONE', *, *, #56982, .T. ) ;
#6599 = DIRECTION ( 'NONE',  ( 0.000000000000000000, 0.5987040770935622147, -0.8009703041134208501 ) ) ;
#6600 = CARTESIAN_POINT ( 'NONE',  ( -37.00000000000000711, 0.000000000000000000, 0.000000000000000000 ) ) ;
#6601 = DIRECTION ( 'NONE',  ( 0.000000000000000000, 0.01356324068817998940, -0.9999080150203990547 ) ) ;
#6602 = VECTOR ( 'NONE', #62682, 1000.000000000000000 ) ;
#6603 = CARTESIAN_POINT ( 'NONE',  ( -6.606501376987225171, -1.681841871581811088, 11.88175788702164404 ) ) ;
#6604 = AXIS2_PLACEMENT_3D ( 'NONE', #17140, #63015, #37082 ) ;
#6605 = CIRCLE ( 'NONE', #245, 12.18650000000000055 ) ;
#6606 = AXIS2_PLACEMENT_3D ( 'NONE', #40147, #29522, #9907 ) ;
#6607 = EDGE_CURVE ( 'NONE', #11283, #22582, #28658, .T. ) ;
#6608 = ORIENTED_EDGE ( 'NONE', *, *, #22629, .T. ) ;
#6609 = ORIENTED_EDGE ( 'NONE', *, *, #20480, .T. ) ;
#6610 = LINE ( 'NONE', #60816, #12717 ) ;
#6611 = VERTEX_POINT ( 'NONE', #35804 ) ;
#6612 = LINE ( 'NONE', #16583, #3295 ) ;
#6613 =( BOUNDED_SURFACE ( )  B_SPLINE_SURFACE ( 3, 1, ( 
 ( #8118, #48684 ),
 ( #3142, #63961 ),
 ( #18440, #13415 ),
 ( #53992, #8436 ) ),
 .UNSPECIFIED., .F., .F., .F. ) 
 B_SPLINE_SURFACE_WITH_KNOTS ( ( 4, 4 ),
 ( 2, 2 ),
 ( 0.000000000000000000, 1.000000000000000000 ),
 ( 0.000000000000000000, 1.000000000000000000 ),
 .UNSPECIFIED. ) 
 GEOMETRIC_REPRESENTATION_ITEM ( )  RATIONAL_B_SPLINE_SURFACE ( (
 ( 1.000000000000000000, 1.000000000000000000),
 ( 0.6933888150995267674, 0.9895912004443193632),
 ( 0.6933888150995267674, 0.9895912004443193632),
 ( 1.000000000000000000, 1.000000000000000000) ) ) 
 REPRESENTATION_ITEM ( '' )  SURFACE ( )  );
#6614 = LINE ( 'NONE', #6283, #53257 ) ;
#6615 = DIRECTION ( 'NONE',  ( 1.000000000000000000, -0.000000000000000000, -0.000000000000000000 ) ) ;
#6616 = CARTESIAN_POINT ( 'NONE',  ( 2.368238019614553824, 7.674602282635826001, -0.1797502808084445181 ) ) ;
#6617 = EDGE_CURVE ( 'NONE', #53922, #59346, #62633, .T. ) ;
#6618 = CARTESIAN_POINT ( 'NONE',  ( 2.260457164927183626, -1.190240296002724740, 7.547495527593548914 ) ) ;
#6619 = CARTESIAN_POINT ( 'NONE',  ( -7.173176924626749162, -1.348899530466227015, 11.92417379687110568 ) ) ;
#6620 = VERTEX_POINT ( 'NONE', #36488 ) ;
#6621 = EDGE_CURVE ( 'NONE', #56717, #37109, #17868, .T. ) ;
#6622 = CARTESIAN_POINT ( 'NONE',  ( -27.28573687977897677, 1.043905432732902927, 2.702109387930228479 ) ) ;
#6623 = ORIENTED_EDGE ( 'NONE', *, *, #16533, .F. ) ;
#6624 = CARTESIAN_POINT ( 'NONE',  ( 37.00000000000000711, 12.68495603654573500, 1.286231064351171627 ) ) ;
#6625 = AXIS2_PLACEMENT_3D ( 'NONE', #50320, #25036, #49352 ) ;
#6626 = CARTESIAN_POINT ( 'NONE',  ( -8.891032880924177206, 11.36194426013951997, -3.860857758255646921 ) ) ;
#6627 = CARTESIAN_POINT ( 'NONE',  ( 1.937114397841932290, 0.9020203649533465873, -12.80345148322678384 ) ) ;
#6628 = CARTESIAN_POINT ( 'NONE',  ( 3.152665057733930798, -5.761241965769118067, -5.461013642405381674 ) ) ;
#6629 = EDGE_LOOP ( 'NONE', ( #46684, #804, #3527, #63415 ) ) ;
#6630 = CARTESIAN_POINT ( 'NONE',  ( 37.00000000000000711, 4.705694406421931860E-17, -3.469127814946512892E-15 ) ) ;
#6631 = CARTESIAN_POINT ( 'NONE',  ( -13.98431177871173858, -30.12623156650373701, -5.679219063900182718 ) ) ;
#6633 = EDGE_CURVE ( 'NONE', #11368, #11657, #43509, .T. ) ;
#6632 = CARTESIAN_POINT ( 'NONE',  ( 35.00000000000000000, 4.705694406421931860E-17, -3.469127814946512892E-15 ) ) ;
#6634 = ORIENTED_EDGE ( 'NONE', *, *, #40017, .T. ) ;
#6635 = ORIENTED_EDGE ( 'NONE', *, *, #11639, .T. ) ;
#6636 = CARTESIAN_POINT ( 'NONE',  ( 5.515539859299206427, -0.004037661319610856558, 0.004509673239148324041 ) ) ;
#6638 = ORIENTED_EDGE ( 'NONE', *, *, #63479, .T. ) ;
#6637 = EDGE_CURVE ( 'NONE', #42088, #45883, #273, .T. ) ;
#6639 = EDGE_LOOP ( 'NONE', ( #47844, #3854, #42478, #21067 ) ) ;
#6640 = ORIENTED_EDGE ( 'NONE', *, *, #16948, .T. ) ;
#6642 = EDGE_CURVE ( 'NONE', #57337, #62155, #51795, .T. ) ;
#6641 = ORIENTED_EDGE ( 'NONE', *, *, #19755, .T. ) ;
#6643 = CARTESIAN_POINT ( 'NONE',  ( 2.241528039335007438, -7.179411278563573973, 2.596349773934855332 ) ) ;
#6644 = CYLINDRICAL_SURFACE ( 'NONE', #17784, 4.999999999999999112 ) ;
#6645 = DIRECTION ( 'NONE',  ( -1.000000000000000000, 0.000000000000000000, 0.000000000000000000 ) ) ;
#6646 = DIRECTION ( 'NONE',  ( 0.000000000000000000, 0.000000000000000000, -1.000000000000000000 ) ) ;
#6647 = CARTESIAN_POINT ( 'NONE',  ( 37.00000000000000711, 4.705694406421931860E-17, -3.469127814946512892E-15 ) ) ;
#6648 = ORIENTED_EDGE ( 'NONE', *, *, #28327, .F. ) ;
#6649 = ADVANCED_FACE ( 'NONE', ( #50800 ), #60778, .T. ) ;
#6650 = CARTESIAN_POINT ( 'NONE',  ( 2.000000000000001776, -6.441884263200823746, -2.217201541069834914 ) ) ;
#6651 = ORIENTED_EDGE ( 'NONE', *, *, #63970, .F. ) ;
#6652 = CARTESIAN_POINT ( 'NONE',  ( 35.00000000000000000, -1.456211999474423369, -11.65554240571057143 ) ) ;
#6653 = DIRECTION ( 'NONE',  ( -1.000000000000000000, 0.000000000000000000, 0.000000000000000000 ) ) ;
#6654 = EDGE_CURVE ( 'NONE', #6851, #797, #5253, .T. ) ;
#6655 = CARTESIAN_POINT ( 'NONE',  ( 2.305787727787083519, 4.792270232040894307, 5.970480882365237996 ) ) ;
#6656 = CARTESIAN_POINT ( 'NONE',  ( 0.2872850955227730929, -8.035297825011307182, -9.251080475901439115 ) ) ;
#6657 = DIRECTION ( 'NONE',  ( 0.000000000000000000, 0.7196168960969817618, 0.6943713148249615053 ) ) ;
#6658 = CARTESIAN_POINT ( 'NONE',  ( 0.3675815128205912052, -10.50067073900647330, -6.367184624550275451 ) ) ;
#6659 = CIRCLE ( 'NONE', #38480, 5.000000000000000888 ) ;
#6660 = CIRCLE ( 'NONE', #52318, 12.18650000000000055 ) ;
#6661 = VECTOR ( 'NONE', #65739, 1000.000000000000114 ) ;
#6662 = ORIENTED_EDGE ( 'NONE', *, *, #19181, .F. ) ;
#6663 = CARTESIAN_POINT ( 'NONE',  ( 0.000000000000000000, -1.058508696394911963, -6.730038252034928448 ) ) ;
#6664 = ORIENTED_EDGE ( 'NONE', *, *, #33756, .T. ) ;
#6665 = DIRECTION ( 'NONE',  ( 0.000000000000000000, -0.01356324068817991828, 0.9999080150203990547 ) ) ;
#6666 = CARTESIAN_POINT ( 'NONE',  ( 3.152665057736253829, 5.761241965767907480, -5.461013642407265500 ) ) ;
#6667 = CARTESIAN_POINT ( 'NONE',  ( 19.56743653832046803, -33.00000000000000000, -5.000000000000012434 ) ) ;
#6668 = CARTESIAN_POINT ( 'NONE',  ( 35.00000000000000000, -4.309077947445731027, -10.92721691015454510 ) ) ;
#6669 = CARTESIAN_POINT ( 'NONE',  ( 2.969415267403817005, 7.815364626283781924, 0.9841783286033500833 ) ) ;
#6670 = ORIENTED_EDGE ( 'NONE', *, *, #9633, .F. ) ;
#6671 = CARTESIAN_POINT ( 'NONE',  ( 37.00000000000000711, -11.74226168163341555, -0.3025107581130825896 ) ) ;
#6672 = CARTESIAN_POINT ( 'NONE',  ( 36.00000000000000711, 7.745827850123149005, 10.12742074351888100 ) ) ;
#6673 = CARTESIAN_POINT ( 'NONE',  ( 35.00000000000000000, -12.26766708251988724, 3.473736367725380969 ) ) ;
#6674 = DIRECTION ( 'NONE',  ( -1.000000000000000000, 0.000000000000000000, 0.000000000000000000 ) ) ;
#6675 = AXIS2_PLACEMENT_3D ( 'NONE', #10585, #55503, #30230 ) ;
#6676 = EDGE_CURVE ( 'NONE', #9320, #24124, #46238, .T. ) ;
#6677 = CARTESIAN_POINT ( 'NONE',  ( -37.00000000000000711, 0.000000000000000000, 0.000000000000000000 ) ) ;
#6678 = AXIS2_PLACEMENT_3D ( 'NONE', #14287, #55519, #15274 ) ;
#6679 = EDGE_LOOP ( 'NONE', ( #8469, #60130, #2270, #45789 ) ) ;
#6680 = AXIS2_PLACEMENT_3D ( 'NONE', #31242, #46524, #41523 ) ;
#6681 = CARTESIAN_POINT ( 'NONE',  ( 0.2646305136544072623, 7.972778379581551889, 9.296005949277251545 ) ) ;
#6682 = CARTESIAN_POINT ( 'NONE',  ( 0.000000000000000000, 0.000000000000000000, 0.000000000000000000 ) ) ;
#6683 = ADVANCED_FACE ( 'NONE', ( #35499 ), #16207, .T. ) ;
#6684 = EDGE_CURVE ( 'NONE', #17893, #21858, #9903, .T. ) ;
#6685 = ORIENTED_EDGE ( 'NONE', *, *, #5740, .T. ) ;
#6686 = ORIENTED_EDGE ( 'NONE', *, *, #38646, .F. ) ;
#6687 = CARTESIAN_POINT ( 'NONE',  ( 0.2653519890518162283, 2.126538543978078177, 12.06014856238021693 ) ) ;
#6688 = CARTESIAN_POINT ( 'NONE',  ( 47.45484198363494954, -0.5059748548177207539, -8.508429091481751527 ) ) ;
#6689 = CARTESIAN_POINT ( 'NONE',  ( 47.00000000000000711, 4.705694406421931860E-17, -3.469127814946512892E-15 ) ) ;
#6690 = CARTESIAN_POINT ( 'NONE',  ( 0.3109076770649050747, -1.896437056876546512, 12.11383728282219074 ) ) ;
#6691 = ORIENTED_EDGE ( 'NONE', *, *, #39924, .F. ) ;
#6692 = EDGE_CURVE ( 'NONE', #47761, #64752, #21203, .T. ) ;
#6693 = CIRCLE ( 'NONE', #9850, 5.000000000000000888 ) ;
#6694 = ORIENTED_EDGE ( 'NONE', *, *, #23821, .T. ) ;
#6695 = VERTEX_POINT ( 'NONE', #20863 ) ;
#6696 = CARTESIAN_POINT ( 'NONE',  ( 2.889800649504073782, -5.334644486274173758, -3.002151847318972777 ) ) ;
#6697 = CIRCLE ( 'NONE', #19422, 4.999999999999999112 ) ;
#6699 = VECTOR ( 'NONE', #55247, 1000.000000000000000 ) ;
#6698 = CARTESIAN_POINT ( 'NONE',  ( -4.975205859172452172, -1.416020129149132778, 25.00000000000000000 ) ) ;
#6700 = ORIENTED_EDGE ( 'NONE', *, *, #11894, .T. ) ;
#6701 = CARTESIAN_POINT ( 'NONE',  ( 35.00000000000000000, 11.86701198550355940, -2.772148766916162188 ) ) ;
#6702 = FACE_OUTER_BOUND ( 'NONE', #27162, .T. ) ;
#6703 = ORIENTED_EDGE ( 'NONE', *, *, #25038, .T. ) ;
#6704 = DIRECTION ( 'NONE',  ( -1.000000000000000000, 0.000000000000000000, 0.000000000000000000 ) ) ;
#6705 = DIRECTION ( 'NONE',  ( 0.000000000000000000, -0.01356324068817999114, 0.9999080150203989437 ) ) ;
#6706 = CYLINDRICAL_SURFACE ( 'NONE', #56897, 4.999999999999999112 ) ;
#6707 = ORIENTED_EDGE ( 'NONE', *, *, #11273, .T. ) ;
#6708 = AXIS2_PLACEMENT_3D ( 'NONE', #40916, #1347, #11625 ) ;
#6709 = CARTESIAN_POINT ( 'NONE',  ( -37.00000000000000711, -11.80185301892984384, 4.824807283154077808 ) ) ;
#6710 = ORIENTED_EDGE ( 'NONE', *, *, #47652, .F. ) ;
#6711 = CARTESIAN_POINT ( 'NONE',  ( -10.95212338237647920, -9.902220863987562183, 25.00000000000000000 ) ) ;
#6712 = AXIS2_PLACEMENT_3D ( 'NONE', #65208, #35598, #49923 ) ;
#6713 = CARTESIAN_POINT ( 'NONE',  ( -17.64392624464051806, -7.224638894555154955, 11.40788166233496170 ) ) ;
#6714 = EDGE_CURVE ( 'NONE', #26131, #41694, #22940, .T. ) ;
#6715 = B_SPLINE_CURVE_WITH_KNOTS ( 'NONE', 3,
 ( #224, #35756, #25472, #26455, #36439, #35450, #46109, #31122, #10838, #51749, #16494, #57059, #15490, #30771, #20495, #11174 ),
 .UNSPECIFIED., .F., .F.,
 ( 4, 3, 3, 3, 3, 4 ),
 ( 0.000000000000000000, 0.0002176109881720219370, 0.0004352086762394582272, 0.0006528017811446855563, 0.0007615147961451689158, 0.0009453342004945030925 ),
 .UNSPECIFIED. ) ;
#6716 = CARTESIAN_POINT ( 'NONE',  ( 14.33157020395877268, -34.50275931095526261, -8.076358832434346269 ) ) ;
#6717 = AXIS2_PLACEMENT_3D ( 'NONE', #59122, #28840, #37838 ) ;
#6718 = DIRECTION ( 'NONE',  ( 0.000000000000000000, -1.000000000000000000, 0.000000000000000000 ) ) ;
#6719 = FACE_OUTER_BOUND ( 'NONE', #48296, .T. ) ;
#6720 = DIRECTION ( 'NONE',  ( 0.000000000000000000, 0.8989688749565142301, 0.4380125133594005016 ) ) ;
#6721 = CYLINDRICAL_SURFACE ( 'NONE', #6895, 25.00000000000000000 ) ;
#6722 = LINE ( 'NONE', #427, #40517 ) ;
#6723 = ORIENTED_EDGE ( 'NONE', *, *, #15643, .T. ) ;
#6724 = EDGE_CURVE ( 'NONE', #14872, #20098, #26188, .T. ) ;
#6725 = DIRECTION ( 'NONE',  ( -1.000000000000000000, 0.000000000000000000, 0.000000000000000000 ) ) ;
#6726 = VERTEX_POINT ( 'NONE', #11222 ) ;
#6727 = CYLINDRICAL_SURFACE ( 'NONE', #5165, 12.75000000000000178 ) ;
#6728 = CARTESIAN_POINT ( 'NONE',  ( -28.41827485489077532, 3.509237424706437292, -13.03592162821790801 ) ) ;
#6729 = EDGE_CURVE ( 'NONE', #48474, #58225, #54927, .T. ) ;
#6730 = ORIENTED_EDGE ( 'NONE', *, *, #14613, .T. ) ;
#6731 = CARTESIAN_POINT ( 'NONE',  ( 2.589278595513614611, 7.361833592938543447, 2.423168677231871460 ) ) ;
#6732 = CARTESIAN_POINT ( 'NONE',  ( 0.3665391374699465965, 9.576575648339021640, 7.691255657244325583 ) ) ;
#6733 = DIRECTION ( 'NONE',  ( -1.000000000000000000, -0.000000000000000000, -0.000000000000000000 ) ) ;
#6734 = ORIENTED_EDGE ( 'NONE', *, *, #27332, .T. ) ;
#6735 = VECTOR ( 'NONE', #30967, 1000.000000000000114 ) ;
#6736 = VERTEX_POINT ( 'NONE', #58091 ) ;
#6737 = CARTESIAN_POINT ( 'NONE',  ( 36.00000000000000711, 12.49688848680884234, -2.527899948230686089 ) ) ;
#6738 = VERTEX_POINT ( 'NONE', #6571 ) ;
#6739 = CARTESIAN_POINT ( 'NONE',  ( 1.719304012340733934, -12.20344780066092305, -3.626341562669774365 ) ) ;
#6740 = CARTESIAN_POINT ( 'NONE',  ( 36.00000000000000711, -5.710938531231790627, -11.39945968423469580 ) ) ;
#6741 = CARTESIAN_POINT ( 'NONE',  ( 1.937114397841935398, 0.9020203649531696177, 12.80345148322679627 ) ) ;
#6742 = ORIENTED_EDGE ( 'NONE', *, *, #19074, .T. ) ;
#6743 = AXIS2_PLACEMENT_3D ( 'NONE', #42687, #43032, #38713 ) ;
#6744 = DIRECTION ( 'NONE',  ( -1.000000000000000000, -0.000000000000000000, -0.000000000000000000 ) ) ;
#6745 = CIRCLE ( 'NONE', #30079, 12.18650000000000055 ) ;
#6746 = ADVANCED_FACE ( 'NONE', ( #22170 ), #63378, .F. ) ;
#6747 = EDGE_CURVE ( 'NONE', #53954, #29924, #29691, .T. ) ;
#6748 = DIRECTION ( 'NONE',  ( 1.000000000000000000, 0.000000000000000000, 0.000000000000000000 ) ) ;
#6749 = CARTESIAN_POINT ( 'NONE',  ( -37.00000000000000711, -10.30098186818253758, 5.644643009979033899 ) ) ;
#6750 = AXIS2_PLACEMENT_3D ( 'NONE', #50894, #5690, #45910 ) ;
#6751 = DIRECTION ( 'NONE',  ( 0.000000000000000000, 0.4134677391718510897, 0.9105187689795954942 ) ) ;
#6752 = LINE ( 'NONE', #35673, #16862 ) ;
#6753 = DIRECTION ( 'NONE',  ( 1.000000000000000000, 0.000000000000000000, 0.000000000000000000 ) ) ;
#6754 = DIRECTION ( 'NONE',  ( 0.000000000000000000, 0.01356324068817998940, -0.9999080150203990547 ) ) ;
#6755 = CARTESIAN_POINT ( 'NONE',  ( 37.00000000000000711, 4.705694406421931860E-17, -3.469127814946512892E-15 ) ) ;
#6756 = CIRCLE ( 'NONE', #8839, 5.000000000000001776 ) ;
#6757 = EDGE_CURVE ( 'NONE', #16846, #44289, #21627, .T. ) ;
#6758 = VECTOR ( 'NONE', #49704, 1000.000000000000000 ) ;
#6759 = B_SPLINE_CURVE_WITH_KNOTS ( 'NONE', 3,
 ( #47750, #2198, #57078, #6536, #26810, #32111, #63035, #17498, #12477, #47110, #36459, #52431, #27141, #37770, #47436, #57747 ),
 .UNSPECIFIED., .F., .F.,
 ( 4, 3, 3, 3, 3, 4 ),
 ( 2.710505431213761085E-19, 0.0003017745587525258975, 0.0006035491769808751499, 0.0009053241094668185249, 0.001207275924539989763, 0.001510325902532974216 ),
 .UNSPECIFIED. ) ;
#6760 = ORIENTED_EDGE ( 'NONE', *, *, #15444, .F. ) ;
#6761 = CARTESIAN_POINT ( 'NONE',  ( 5.514970785353741078, -0.001326349372336609999, -0.004532877335078314314 ) ) ;
#6762 = CARTESIAN_POINT ( 'NONE',  ( 0.2657645697724698719, -12.24540328300721548, -0.1513403555226850161 ) ) ;
#6763 = VERTEX_POINT ( 'NONE', #36814 ) ;
#6764 = CARTESIAN_POINT ( 'NONE',  ( 36.00000000000000711, -1.908798535168467536, -12.60630747491662618 ) ) ;
#6765 = CARTESIAN_POINT ( 'NONE',  ( 2.655192694323065705, -5.293797899977148447, -8.010337395401304406 ) ) ;
#6766 = ORIENTED_EDGE ( 'NONE', *, *, #17173, .F. ) ;
#6767 = DIRECTION ( 'NONE',  ( 1.000000000000000000, 0.000000000000000000, 0.000000000000000000 ) ) ;
#6768 = ORIENTED_EDGE ( 'NONE', *, *, #39716, .F. ) ;
#6769 = EDGE_CURVE ( 'NONE', #53550, #47123, #38196, .T. ) ;
#6770 = CARTESIAN_POINT ( 'NONE',  ( 0.000000000000000000, 6.812627895098307462, 0.04423456934733380197 ) ) ;
#6771 = ORIENTED_EDGE ( 'NONE', *, *, #4380, .F. ) ;
#6772 = ORIENTED_EDGE ( 'NONE', *, *, #10043, .F. ) ;
#6773 = EDGE_CURVE ( 'NONE', #5329, #24551, #27821, .T. ) ;
#6774 = LINE ( 'NONE', #21746, #1921 ) ;
#6775 = AXIS2_PLACEMENT_3D ( 'NONE', #39148, #34162, #28857 ) ;
#6776 = VERTEX_POINT ( 'NONE', #17531 ) ;
#6777 = CARTESIAN_POINT ( 'NONE',  ( -24.81264729437695848, -8.085877654816028937, 8.874484760932165983 ) ) ;
#6778 = CARTESIAN_POINT ( 'NONE',  ( 1.462291587750749633, -11.65117843858596558, -4.914320681886166220 ) ) ;
#6779 = CARTESIAN_POINT ( 'NONE',  ( 22.78406729994189561, -4.691424615418254618, -12.65938842238563744 ) ) ;
#6780 = DIRECTION ( 'NONE',  ( 0.000000000000000000, 0.9903235168508555120, 0.1387779952735782862 ) ) ;
#6781 = VERTEX_POINT ( 'NONE', #37798 ) ;
#6782 = FACE_OUTER_BOUND ( 'NONE', #56016, .T. ) ;
#6783 = CARTESIAN_POINT ( 'NONE',  ( 1.717027338329501829, -31.08339181399450979, 14.39386062070807171 ) ) ;
#6784 = CARTESIAN_POINT ( 'NONE',  ( 2.907497136251154579, -7.848280798453004081, 0.3592423305256113863 ) ) ;
#6786 = ORIENTED_EDGE ( 'NONE', *, *, #44938, .F. ) ;
#6785 = DIRECTION ( 'NONE',  ( -1.000000000000000000, -0.000000000000000000, 0.000000000000000000 ) ) ;
#6787 = CARTESIAN_POINT ( 'NONE',  ( -28.19916972693312829, 11.19825076026768151, -4.324271721581003369 ) ) ;
#6788 = ORIENTED_EDGE ( 'NONE', *, *, #55545, .F. ) ;
#6789 = VECTOR ( 'NONE', #16501, 1000.000000000000000 ) ;
#6790 = CARTESIAN_POINT ( 'NONE',  ( 0.2653519991613815243, 9.395283368383282152, -7.854838327448875113 ) ) ;
#6791 = ORIENTED_EDGE ( 'NONE', *, *, #42958, .F. ) ;
#6792 = CARTESIAN_POINT ( 'NONE',  ( 21.53315970858584549, -11.27100376921459635, -4.123804204784697447 ) ) ;
#6793 = DIRECTION ( 'NONE',  ( 0.000000000000000000, 0.6478160128811948359, -0.7617968321374878338 ) ) ;
#6794 = EDGE_CURVE ( 'NONE', #27971, #19813, #53091, .T. ) ;
#6796 = CARTESIAN_POINT ( 'NONE',  ( 1.020182472821632214, -4.691131056022166845, 11.58401323226448909 ) ) ;
#6795 = CIRCLE ( 'NONE', #60950, 2.899999999999994582 ) ;
#6797 = ORIENTED_EDGE ( 'NONE', *, *, #54934, .T. ) ;
#6798 = CARTESIAN_POINT ( 'NONE',  ( -37.00000000000000711, -9.557269938331609538, 7.561043153947932360 ) ) ;
#6799 = CARTESIAN_POINT ( 'NONE',  ( 3.152665057734040488, 0.000000000000000000, 0.000000000000000000 ) ) ;
#6800 = CARTESIAN_POINT ( 'NONE',  ( 0.000000000000000000, -33.00000000000000000, 0.000000000000000000 ) ) ;
#6801 = ORIENTED_EDGE ( 'NONE', *, *, #34589, .T. ) ;
#6802 = EDGE_CURVE ( 'NONE', #12068, #28265, #33967, .T. ) ;
#6803 =( BOUNDED_CURVE ( )  B_SPLINE_CURVE ( 3, ( #5212, #40437, #21138, #20502 ),
 .UNSPECIFIED., .F., .F. ) 
 B_SPLINE_CURVE_WITH_KNOTS ( ( 4, 4 ),
 ( 1.570796326794897446, 1.605031943246829185 ),
 .UNSPECIFIED. ) 
 CURVE ( )  GEOMETRIC_REPRESENTATION_ITEM ( )  RATIONAL_B_SPLINE_CURVE ( ( 1.000000000000000000, 0.9999023292654991568, 0.9999023292654991568, 1.000000000000000000 ) ) 
 REPRESENTATION_ITEM ( '' )  );
#6804 = AXIS2_PLACEMENT_3D ( 'NONE', #58357, #26780, #42368 ) ;
#6805 = EDGE_LOOP ( 'NONE', ( #6256, #23946, #65084, #4554 ) ) ;
#6806 = CARTESIAN_POINT ( 'NONE',  ( 2.305787727787084407, 7.508843116234155346, 1.493241775258449255 ) ) ;
#6807 = ORIENTED_EDGE ( 'NONE', *, *, #53978, .F. ) ;
#6808 = VECTOR ( 'NONE', #63072, 1000.000000000000000 ) ;
#6809 = ORIENTED_EDGE ( 'NONE', *, *, #59482, .T. ) ;
#6810 = AXIS2_PLACEMENT_3D ( 'NONE', #60942, #5416, #36956 ) ;
#6811 = DIRECTION ( 'NONE',  ( -1.000000000000000000, 0.000000000000000000, 0.000000000000000000 ) ) ;
#6812 = DIRECTION ( 'NONE',  ( 1.000000000000000000, 0.000000000000000000, -0.000000000000000000 ) ) ;
#6813 = DIRECTION ( 'NONE',  ( 0.000000000000000000, 0.9105187689795967154, -0.4134677391718482586 ) ) ;
#6814 = DIRECTION ( 'NONE',  ( 1.000000000000000000, 0.000000000000000000, 0.000000000000000000 ) ) ;
#6815 = DIRECTION ( 'NONE',  ( -1.000000000000000000, 0.000000000000000000, 0.000000000000000000 ) ) ;
#6816 = AXIS2_PLACEMENT_3D ( 'NONE', #47656, #27053, #22727 ) ;
#6817 = DIRECTION ( 'NONE',  ( 0.000000000000000000, 0.9985334138511237079, 0.05413890858542116241 ) ) ;
#6818 = ADVANCED_FACE ( 'NONE', ( #7882 ), #28158, .T. ) ;
#6819 = DIRECTION ( 'NONE',  ( 1.000000000000000000, 0.000000000000000000, 0.000000000000000000 ) ) ;
#6820 =( BOUNDED_SURFACE ( )  B_SPLINE_SURFACE ( 3, 1, ( 
 ( #16866, #5609 ),
 ( #35812, #37139 ),
 ( #26849, #10554 ),
 ( #40840, #30834 ) ),
 .UNSPECIFIED., .F., .F., .F. ) 
 B_SPLINE_SURFACE_WITH_KNOTS ( ( 4, 4 ),
 ( 2, 2 ),
 ( 0.000000000000000000, 1.000000000000000000 ),
 ( 0.000000000000000000, 1.000000000000000000 ),
 .UNSPECIFIED. ) 
 GEOMETRIC_REPRESENTATION_ITEM ( )  RATIONAL_B_SPLINE_SURFACE ( (
 ( 1.000000000000000000, 1.000000000000000000),
 ( 0.9856612449720755231, 0.9999558406602322425),
 ( 0.9856612449720755231, 0.9999558406602322425),
 ( 1.000000000000000000, 1.000000000000000000) ) ) 
 REPRESENTATION_ITEM ( '' )  SURFACE ( )  );
#6821 = EDGE_LOOP ( 'NONE', ( #18142, #20252, #30407, #1699 ) ) ;
#6822 = CIRCLE ( 'NONE', #22715, 12.18650000000000055 ) ;
#6823 = CARTESIAN_POINT ( 'NONE',  ( -22.30078715814471479, -3.111489293522209820, 2.097357782488221023 ) ) ;
#6824 = CARTESIAN_POINT ( 'NONE',  ( 12.51043786959929527, 0.3316631525046815909, -11.99656223984053760 ) ) ;
#6825 = CYLINDRICAL_SURFACE ( 'NONE', #61982, 5.000000000000000888 ) ;
#6826 = AXIS2_PLACEMENT_3D ( 'NONE', #44637, #25693, #10384 ) ;
#6827 = CARTESIAN_POINT ( 'NONE',  ( 5.536195898058073439, 0.002666509901869610743, 0.008071068258923192601 ) ) ;
#6828 = EDGE_CURVE ( 'NONE', #2293, #55606, #42447, .T. ) ;
#6829 = CARTESIAN_POINT ( 'NONE',  ( 35.00000000000000000, 4.705694406421931860E-17, -3.469127814946512892E-15 ) ) ;
#6830 = CARTESIAN_POINT ( 'NONE',  ( 47.00000000000000711, 4.705694406421931860E-17, -3.469127814946512892E-15 ) ) ;
#6831 = ORIENTED_EDGE ( 'NONE', *, *, #49622, .F. ) ;
#6832 = DIRECTION ( 'NONE',  ( -1.000000000000000000, 0.000000000000000000, 0.000000000000000000 ) ) ;
#6833 = CIRCLE ( 'NONE', #34441, 6.936499999999990784 ) ;
#6834 = DIRECTION ( 'NONE',  ( -0.3865475372811021937, 0.8082200352954617140, 0.4442537292684412553 ) ) ;
#6835 = FACE_OUTER_BOUND ( 'NONE', #62461, .T. ) ;
#6836 = VECTOR ( 'NONE', #42805, 1000.000000000000000 ) ;
#6837 = DIRECTION ( 'NONE',  ( 0.000000000000000000, 1.000000000000000000, 0.000000000000000000 ) ) ;
#6838 = EDGE_CURVE ( 'NONE', #648, #23034, #63702, .T. ) ;
#6839 = CARTESIAN_POINT ( 'NONE',  ( -24.82456806599946830, 8.749941039790773090, 8.214224094661178199 ) ) ;
#6840 = CARTESIAN_POINT ( 'NONE',  ( -25.50184365408103204, -8.498472128355658128, 10.49391108592481814 ) ) ;
#6841 = ORIENTED_EDGE ( 'NONE', *, *, #54743, .F. ) ;
#6842 = DIRECTION ( 'NONE',  ( 1.000000000000000000, 0.000000000000000000, 0.000000000000000000 ) ) ;
#6843 = DIRECTION ( 'NONE',  ( 0.000000000000000000, -0.3218879778915842427, 0.9467777615094614685 ) ) ;
#6844 = CARTESIAN_POINT ( 'NONE',  ( 2.276198483116796734, -4.795748742147632804, -5.955030244776002846 ) ) ;
#6845 = VERTEX_POINT ( 'NONE', #18182 ) ;
#6846 = CARTESIAN_POINT ( 'NONE',  ( -10.00000000000000178, 0.000000000000000000, 7.499999999999988454 ) ) ;
#6847 = DIRECTION ( 'NONE',  ( -1.000000000000000000, 0.000000000000000000, -0.000000000000000000 ) ) ;
#6848 = EDGE_CURVE ( 'NONE', #12145, #57976, #50985, .T. ) ;
#6849 = AXIS2_PLACEMENT_3D ( 'NONE', #7440, #22412, #48031 ) ;
#6851 = VERTEX_POINT ( 'NONE', #38786 ) ;
#6850 = CARTESIAN_POINT ( 'NONE',  ( 22.57855258442565116, 3.026812727784649493, -13.15630665159948975 ) ) ;
#6852 = CARTESIAN_POINT ( 'NONE',  ( -35.00000000000000000, 0.000000000000000000, 0.000000000000000000 ) ) ;
#6853 = ADVANCED_FACE ( 'NONE', ( #44734 ), #14470, .T. ) ;
#6854 = VECTOR ( 'NONE', #16508, 1000.000000000000000 ) ;
#6855 = CARTESIAN_POINT ( 'NONE',  ( 0.2717059086739065932, -4.354191483751194802, -11.44824199474646420 ) ) ;
#6856 = EDGE_LOOP ( 'NONE', ( #46673, #17653, #40172, #45748 ) ) ;
#6857 = FACE_OUTER_BOUND ( 'NONE', #64406, .T. ) ;
#6858 = DIRECTION ( 'NONE',  ( -1.000000000000000000, -0.000000000000000000, 0.000000000000000000 ) ) ;
#6859 = CARTESIAN_POINT ( 'NONE',  ( 0.2648978790185602672, -7.769924372105269761, 9.465406350830582127 ) ) ;
#6860 = DIRECTION ( 'NONE',  ( 0.000000000000000000, 0.000000000000000000, 1.000000000000000000 ) ) ;
#6861 = CARTESIAN_POINT ( 'NONE',  ( -9.514445118316093186, 11.30297198722328567, -4.050438551049715841 ) ) ;
#6862 = CARTESIAN_POINT ( 'NONE',  ( -35.00000000000000000, 4.725891942574755866, 10.75351884295729477 ) ) ;
#6864 = VERTEX_POINT ( 'NONE', #49441 ) ;
#6863 = CARTESIAN_POINT ( 'NONE',  ( 35.00000000000000000, -10.62137734850271364, -5.015831474386272859 ) ) ;
#6865 = CARTESIAN_POINT ( 'NONE',  ( 10.47226376122552516, 7.645066471088986404, 11.12901864558550180 ) ) ;
#6866 = EDGE_LOOP ( 'NONE', ( #62178, #13749, #23359, #1119 ) ) ;
#6867 = CARTESIAN_POINT ( 'NONE',  ( 23.46994683125024750, -4.312020184895027697, -11.20298071244178573 ) ) ;
#6868 = VERTEX_POINT ( 'NONE', #3881 ) ;
#6869 = CYLINDRICAL_SURFACE ( 'NONE', #65517, 7.499999999999988454 ) ;
#6870 = ADVANCED_FACE ( 'NONE', ( #34743 ), #59083, .T. ) ;
#6871 = CARTESIAN_POINT ( 'NONE',  ( -3.191470641060126567, 11.27526359945950496, 4.125568914908559925 ) ) ;
#6872 = VECTOR ( 'NONE', #64443, 1000.000000000000000 ) ;
#6873 = CARTESIAN_POINT ( 'NONE',  ( -32.70177428389710883, -2.904144763113407191, 22.74422317523286807 ) ) ;
#6874 = CARTESIAN_POINT ( 'NONE',  ( 5.514624014163232779, -0.002216125254993232471, 0.003498325728817954818 ) ) ;
#6875 = ORIENTED_EDGE ( 'NONE', *, *, #33853, .F. ) ;
#6876 = CARTESIAN_POINT ( 'NONE',  ( 35.00000000000000000, 11.60979404548634619, -3.704519465651352483 ) ) ;
#6877 = CARTESIAN_POINT ( 'NONE',  ( 2.276905613633652070, 5.757134111949752331, -5.031956778294075505 ) ) ;
#6878 = ORIENTED_EDGE ( 'NONE', *, *, #64874, .F. ) ;
#6879 = ORIENTED_EDGE ( 'NONE', *, *, #34457, .T. ) ;
#6880 = CARTESIAN_POINT ( 'NONE',  ( 29.03457606387295087, -7.862146963512102182, 10.97436308512422265 ) ) ;
#6881 = ORIENTED_EDGE ( 'NONE', *, *, #42480, .F. ) ;
#6882 = FACE_OUTER_BOUND ( 'NONE', #17739, .T. ) ;
#6883 = CARTESIAN_POINT ( 'NONE',  ( -10.95212338237647920, -9.902220863987562183, -6.778349501228825069 ) ) ;
#6884 = CARTESIAN_POINT ( 'NONE',  ( 35.00000000000000000, 4.705694406421931860E-17, -3.469127814946512892E-15 ) ) ;
#6885 = CARTESIAN_POINT ( 'NONE',  ( 1.547277799337430038, 12.58038279313686481, 1.534072017333138360 ) ) ;
#6886 = EDGE_CURVE ( 'NONE', #46786, #9459, #6539, .T. ) ;
#6887 = DIRECTION ( 'NONE',  ( 1.000000000000000000, -0.000000000000000000, -0.000000000000000000 ) ) ;
#6888 = DIRECTION ( 'NONE',  ( -1.000000000000000000, 0.000000000000000000, 0.000000000000000000 ) ) ;
#6889 = CARTESIAN_POINT ( 'NONE',  ( -37.00000000000000711, -5.130401251914653571, -11.05394794832835359 ) ) ;
#6890 = ORIENTED_EDGE ( 'NONE', *, *, #61859, .F. ) ;
#6891 = CARTESIAN_POINT ( 'NONE',  ( 1.014383007554949589, 12.48801387563329257, -0.4441500209063513616 ) ) ;
#6892 = ORIENTED_EDGE ( 'NONE', *, *, #22856, .F. ) ;
#6893 = DIRECTION ( 'NONE',  ( -1.000000000000000000, 0.000000000000000000, 0.000000000000000000 ) ) ;
#6894 = DIRECTION ( 'NONE',  ( 1.000000000000000000, 0.000000000000000000, -0.000000000000000000 ) ) ;
#6895 = AXIS2_PLACEMENT_3D ( 'NONE', #21337, #36950, #32603 ) ;
#6896 = DIRECTION ( 'NONE',  ( 1.000000000000000000, 0.000000000000000000, 0.000000000000000000 ) ) ;
#6897 = CARTESIAN_POINT ( 'NONE',  ( 0.000000000000000000, -0.4129979343796691404, -6.800241778083718991 ) ) ;
#6898 = CARTESIAN_POINT ( 'NONE',  ( 0.000000000000000000, 244.9489742783177917, 156.8996349149244054 ) ) ;
#6899 = VECTOR ( 'NONE', #37014, 1000.000000000000000 ) ;
#6900 = VERTEX_POINT ( 'NONE', #9475 ) ;
#6901 = VERTEX_POINT ( 'NONE', #64366 ) ;
#6902 = CARTESIAN_POINT ( 'NONE',  ( -27.08704841010922593, 0.1930432016059930034, 2.291653842312383116 ) ) ;
#6903 = EDGE_CURVE ( 'NONE', #65435, #53879, #27607, .T. ) ;
#6904 = ORIENTED_EDGE ( 'NONE', *, *, #22612, .F. ) ;
#6905 = CARTESIAN_POINT ( 'NONE',  ( -16.00005080000000035, 0.000000000000000000, 0.000000000000000000 ) ) ;
#6906 = CARTESIAN_POINT ( 'NONE',  ( -37.00000000000000711, 10.39746860227890757, 7.379373053628906831 ) ) ;
#6907 = DIRECTION ( 'NONE',  ( -1.000000000000000000, 0.000000000000000000, 0.000000000000000000 ) ) ;
#6908 = ADVANCED_FACE ( 'NONE', ( #8197 ), #13810, .T. ) ;
#6909 = ORIENTED_EDGE ( 'NONE', *, *, #10450, .F. ) ;
#6910 = CARTESIAN_POINT ( 'NONE',  ( 35.00000000000000000, 9.240395740215630482, -7.251710744571611578 ) ) ;
#6911 = CARTESIAN_POINT ( 'NONE',  ( 3.152665057734040488, 0.000000000000000000, 0.000000000000000000 ) ) ;
#6912 = CARTESIAN_POINT ( 'NONE',  ( 2.844750968616352793, -1.031816958530431316, 7.767336242081023912 ) ) ;
#6913 = DIRECTION ( 'NONE',  ( -1.000000000000000000, 0.000000000000000000, 0.000000000000000000 ) ) ;
#6914 = B_SPLINE_CURVE_WITH_KNOTS ( 'NONE', 3,
 ( #52597, #41606, #15996, #12325, #6059, #57911, #31311, #21324, #37611, #61550, #32589, #26642, #52266, #62529, #1719, #27615, #22653, #2378, #11669 ),
 .UNSPECIFIED., .F., .F.,
 ( 4, 3, 3, 3, 3, 3, 4 ),
 ( 4.336808689942017255E-19, 2.831840207625097852E-05, 4.217266860012006086E-05, 5.602024318565493148E-05, 6.290810168137762047E-05, 9.120440631110077504E-05, 0.0001153103026478315791 ),
 .UNSPECIFIED. ) ;
#6915 = CIRCLE ( 'NONE', #49421, 12.18649999999999878 ) ;
#6916 = EDGE_CURVE ( 'NONE', #46888, #47458, #28466, .T. ) ;
#6917 = DIRECTION ( 'NONE',  ( 1.000000000000000000, -0.000000000000000000, -0.000000000000000000 ) ) ;
#6918 = CARTESIAN_POINT ( 'NONE',  ( -35.00000000000000000, 0.000000000000000000, 0.000000000000000000 ) ) ;
#6919 = EDGE_LOOP ( 'NONE', ( #20085, #57270, #25579, #17902 ) ) ;
#6920 = CARTESIAN_POINT ( 'NONE',  ( -13.50035326695106797, -34.20038524408859359, -9.091202907900893138 ) ) ;
#6921 = EDGE_LOOP ( 'NONE', ( #11908, #28823, #2653, #2652 ) ) ;
#6922 = DIRECTION ( 'NONE',  ( 1.000000000000000000, 0.000000000000000000, 0.000000000000000000 ) ) ;
#6923 = CARTESIAN_POINT ( 'NONE',  ( 2.241526690369556984, 7.179945570618761153, 2.594870554108865246 ) ) ;
#6924 = FACE_OUTER_BOUND ( 'NONE', #22998, .T. ) ;
#6925 = AXIS2_PLACEMENT_3D ( 'NONE', #51, #4409, #49949 ) ;
#6926 = CARTESIAN_POINT ( 'NONE',  ( 1.634816307074478114, 12.68239325670150386, 0.7191532042390553769 ) ) ;
#6927 = DIRECTION ( 'NONE',  ( 1.000000000000000000, 0.000000000000000000, 0.000000000000000000 ) ) ;
#6928 = ORIENTED_EDGE ( 'NONE', *, *, #55416, .F. ) ;
#6929 = ORIENTED_EDGE ( 'NONE', *, *, #8809, .F. ) ;
#6931 = ADVANCED_FACE ( 'NONE', ( #48770 ), #44398, .T. ) ;
#6930 = CARTESIAN_POINT ( 'NONE',  ( 5.530133899448235191, -0.001124651387255098814, 0.01594518557925581753 ) ) ;
#6932 = ORIENTED_EDGE ( 'NONE', *, *, #17856, .T. ) ;
#6933 = CARTESIAN_POINT ( 'NONE',  ( -27.08419642509982950, -2.239682169453945715, 0.4837273216074967075 ) ) ;
#6935 = VECTOR ( 'NONE', #30933, 1000.000000000000000 ) ;
#6934 = CARTESIAN_POINT ( 'NONE',  ( 37.00000000000000711, 4.545979934229410269, -11.30684963584391234 ) ) ;
#6936 = DIRECTION ( 'NONE',  ( 0.000000000000000000, 0.01356324068817992175, -0.9999080150203990547 ) ) ;
#6937 = CARTESIAN_POINT ( 'NONE',  ( 0.2648978790185619880, 12.03635331166815270, -2.256510822326019738 ) ) ;
#6938 = CARTESIAN_POINT ( 'NONE',  ( -37.00000000000000711, 3.640372113593720815, -12.21925492305358318 ) ) ;
#6939 = CARTESIAN_POINT ( 'NONE',  ( 2.241352910868909643, 5.794346703933845433, 4.970878533273779709 ) ) ;
#6940 = DIRECTION ( 'NONE',  ( 0.000000000000000000, -0.01356324068818000328, 0.9999080150203990547 ) ) ;
#6941 = VERTEX_POINT ( 'NONE', #39759 ) ;
#6942 = ORIENTED_EDGE ( 'NONE', *, *, #32611, .T. ) ;
#6943 = CARTESIAN_POINT ( 'NONE',  ( 2.080613030138688480, 0.000000000000000000, 0.000000000000000000 ) ) ;
#6944 = EDGE_LOOP ( 'NONE', ( #53725, #35649, #47603, #61882 ) ) ;
#6945 = MANIFOLD_SOLID_BREP ( 'Join1', #59965 ) ;
#6946 = DIRECTION ( 'NONE',  ( 0.000000000000000000, 0.01356324068817998940, -0.9999080150203990547 ) ) ;
#6947 = CARTESIAN_POINT ( 'NONE',  ( -35.00000000000000000, -1.463443770872689509, -12.09831040184925577 ) ) ;
#6948 = DIRECTION ( 'NONE',  ( 0.000000000000000000, -0.9985334138511243740, 0.05413890858540768708 ) ) ;
#6949 = EDGE_LOOP ( 'NONE', ( #33492, #34577, #43633, #38608 ) ) ;
#6950 = CARTESIAN_POINT ( 'NONE',  ( 5.530133899448235191, -0.01594518557925581406, -0.001124651387255154325 ) ) ;
#6951 = CARTESIAN_POINT ( 'NONE',  ( -14.30187556442842656, -30.10361765235625597, -4.782130246577440680 ) ) ;
#6952 = CARTESIAN_POINT ( 'NONE',  ( 2.440552418640497656, -1.531218882877344534, 7.547055375260057097 ) ) ;
#6953 = ORIENTED_EDGE ( 'NONE', *, *, #12025, .T. ) ;
#6954 = ORIENTED_EDGE ( 'NONE', *, *, #29375, .F. ) ;
#6955 = CARTESIAN_POINT ( 'NONE',  ( 0.2638984909335720941, -2.322601104020586060, -12.02508546958699398 ) ) ;
#6956 = ORIENTED_EDGE ( 'NONE', *, *, #38287, .F. ) ;
#6957 = ORIENTED_EDGE ( 'NONE', *, *, #45243, .F. ) ;
#6958 = EDGE_LOOP ( 'NONE', ( #29863, #59050, #46446, #41986 ) ) ;
#6959 = VERTEX_POINT ( 'NONE', #3221 ) ;
#6960 = CARTESIAN_POINT ( 'NONE',  ( 2.241451721903216843, -7.194631024842657929, 2.553895636571910988 ) ) ;
#6961 = CARTESIAN_POINT ( 'NONE',  ( 2.249013661412018195, 5.000301708455996419, -5.772355099776886433 ) ) ;
#6962 = EDGE_CURVE ( 'NONE', #23964, #55391, #14867, .T. ) ;
#6963 = AXIS2_PLACEMENT_3D ( 'NONE', #12600, #43863, #57868 ) ;
#6964 = CARTESIAN_POINT ( 'NONE',  ( -35.00000000000000000, 10.49591321039680736, 5.273331777780375873 ) ) ;
#6965 = CARTESIAN_POINT ( 'NONE',  ( 2.259830038564998311, 2.742210045659281725, -7.131511317046831167 ) ) ;
#6966 = CARTESIAN_POINT ( 'NONE',  ( -35.00000000000000000, 0.000000000000000000, 0.000000000000000000 ) ) ;
#6967 = CARTESIAN_POINT ( 'NONE',  ( 37.00000000000000711, 9.430788938294046631, -7.718225330433843290 ) ) ;
#6968 = ORIENTED_EDGE ( 'NONE', *, *, #7271, .F. ) ;
#6969 = CARTESIAN_POINT ( 'NONE',  ( -35.00000000000000000, 10.91072401419410554, 5.428340790341743549 ) ) ;
#6970 = CYLINDRICAL_SURFACE ( 'NONE', #2333, 12.18650000000000055 ) ;
#6971 = CARTESIAN_POINT ( 'NONE',  ( 2.247112776671923662, 3.716786765231635759, -6.670755883246408224 ) ) ;
#6972 = COLOUR_RGB ( '', 0.40784314, 0.44705882, 0.49803922) ;
#6973 = DIRECTION ( 'NONE',  ( -1.000000000000000000, 0.000000000000000000, 0.000000000000000000 ) ) ;
#6974 = FACE_OUTER_BOUND ( 'NONE', #34658, .T. ) ;
#6975 = CARTESIAN_POINT ( 'NONE',  ( 0.3057689695767539795, -11.59726335252430829, -3.975296631252078772 ) ) ;
#6976 = EDGE_CURVE ( 'NONE', #33925, #17893, #4325, .T. ) ;
#6977 = ORIENTED_EDGE ( 'NONE', *, *, #46484, .F. ) ;
#6978 = CARTESIAN_POINT ( 'NONE',  ( 5.514970785353741078, -0.003415090918276162540, 0.003262412238248699973 ) ) ;
#6979 = VECTOR ( 'NONE', #40760, 1000.000000000000000 ) ;
#6980 = ORIENTED_EDGE ( 'NONE', *, *, #34398, .F. ) ;
#6981 = EDGE_CURVE ( 'NONE', #56228, #61588, #10805, .T. ) ;
#6982 = DIRECTION ( 'NONE',  ( -1.000000000000000000, 0.000000000000000000, 0.000000000000000000 ) ) ;
#6983 = DIRECTION ( 'NONE',  ( -1.000000000000000000, 0.000000000000000000, 0.000000000000000000 ) ) ;
#6984 = CYLINDRICAL_SURFACE ( 'NONE', #52634, 12.75000000000000178 ) ;
#6985 = DIRECTION ( 'NONE',  ( -1.000000000000000000, 0.000000000000000000, 0.000000000000000000 ) ) ;
#6986 = EDGE_CURVE ( 'NONE', #21944, #45661, #40072, .T. ) ;
#6987 = CARTESIAN_POINT ( 'NONE',  ( 3.047904605210434603, -4.747272783555597009, -6.318654123925961485 ) ) ;
#6988 = ORIENTED_EDGE ( 'NONE', *, *, #2965, .F. ) ;
#6989 = CARTESIAN_POINT ( 'NONE',  ( 1.633930747253265814, 10.62371422070961557, -6.963441708414618070 ) ) ;
#6990 = DIRECTION ( 'NONE',  ( 1.000000000000000000, 0.000000000000000000, -0.000000000000000000 ) ) ;
#6991 = DIRECTION ( 'NONE',  ( 1.000000000000000000, 0.000000000000000000, 0.000000000000000000 ) ) ;
#6992 = CARTESIAN_POINT ( 'NONE',  ( -21.17861794710831091, 25.00000000000000000, -3.604945070120774808 ) ) ;
#6993 = AXIS2_PLACEMENT_3D ( 'NONE', #43328, #17084, #62962 ) ;
#6994 = EDGE_CURVE ( 'NONE', #41167, #665, #62672, .T. ) ;
#6995 = DIRECTION ( 'NONE',  ( 0.000000000000000000, 0.000000000000000000, 1.000000000000000000 ) ) ;
#6996 =( BOUNDED_CURVE ( )  B_SPLINE_CURVE ( 3, ( #28277, #16659, #37258, #36931 ),
 .UNSPECIFIED., .F., .T. ) 
 B_SPLINE_CURVE_WITH_KNOTS ( ( 4, 4 ),
 ( 4.635356053521499931, 4.651107231023391186 ),
 .UNSPECIFIED. ) 
 CURVE ( )  GEOMETRIC_REPRESENTATION_ITEM ( )  RATIONAL_B_SPLINE_CURVE ( ( 1.000000000000000000, 0.9999793251408052308, 0.9999793251408052308, 1.000000000000000000 ) ) 
 REPRESENTATION_ITEM ( '' )  );
#6997 = ORIENTED_EDGE ( 'NONE', *, *, #24242, .T. ) ;
#6998 = ADVANCED_FACE ( 'NONE', ( #60359 ), #56028, .T. ) ;
#6999 = CARTESIAN_POINT ( 'NONE',  ( 0.2646305136544072623, 7.770320294339177813, 9.465888453932986835 ) ) ;
#7000 = CARTESIAN_POINT ( 'NONE',  ( 1.375507693219674588, -5.789143338281887985, -11.20969178069651484 ) ) ;
#7001 = ORIENTED_EDGE ( 'NONE', *, *, #28993, .F. ) ;
#7002 = EDGE_CURVE ( 'NONE', #20463, #29440, #26431, .T. ) ;
#7003 = ORIENTED_EDGE ( 'NONE', *, *, #51131, .T. ) ;
#7004 = DIRECTION ( 'NONE',  ( -1.000000000000000000, 0.000000000000000000, 0.000000000000000000 ) ) ;
#7005 = CARTESIAN_POINT ( 'NONE',  ( -27.08588607604433918, -1.631236259432285784, -1.616144682268734423 ) ) ;
#7006 = DIRECTION ( 'NONE',  ( 0.000000000000000000, -0.4935949184179322380, 0.8696919319575150409 ) ) ;
#7007 = EDGE_CURVE ( 'NONE', #4699, #63989, #524, .T. ) ;
#7008 = CARTESIAN_POINT ( 'NONE',  ( 0.2872850955227743142, -1.921748909352239298, 12.10187515377843503 ) ) ;
#7009 = VERTEX_POINT ( 'NONE', #5179 ) ;
#7010 = ORIENTED_EDGE ( 'NONE', *, *, #56543, .T. ) ;
#7011 = ORIENTED_EDGE ( 'NONE', *, *, #27856, .T. ) ;
#7012 = CARTESIAN_POINT ( 'NONE',  ( 35.00000000000000000, -12.73293890771483383, -0.6593684648220086153 ) ) ;
#7013 = DIRECTION ( 'NONE',  ( -1.000000000000000000, 0.000000000000000000, 0.000000000000000000 ) ) ;
#7014 = EDGE_LOOP ( 'NONE', ( #14218, #20819, #42010, #19956 ) ) ;
#7015 = CIRCLE ( 'NONE', #37815, 2.899999999999994582 ) ;
#7016 = CYLINDRICAL_SURFACE ( 'NONE', #37904, 5.000000000000000888 ) ;
#7017 = LINE ( 'NONE', #11994, #26832 ) ;
#7018 = EDGE_LOOP ( 'NONE', ( #62340, #1978, #40542, #16762 ) ) ;
#7019 = AXIS2_PLACEMENT_3D ( 'NONE', #61284, #15714, #56291 ) ;
#7020 = CARTESIAN_POINT ( 'NONE',  ( -27.08418322526031119, -0.3452258100746897207, -2.265123059255418347 ) ) ;
#7021 = CARTESIAN_POINT ( 'NONE',  ( 8.240410296153493519, -29.00819526741761578, -11.87861853819113733 ) ) ;
#7022 = DIRECTION ( 'NONE',  ( 0.000000000000000000, -0.01356324068817998940, 0.9999080150203990547 ) ) ;
#7023 = ORIENTED_EDGE ( 'NONE', *, *, #6724, .F. ) ;
#7024 = DIRECTION ( 'NONE',  ( -1.000000000000000000, -0.000000000000000000, 0.000000000000000000 ) ) ;
#7025 = EDGE_LOOP ( 'NONE', ( #7508, #3286, #19631, #43735 ) ) ;
#7026 = CARTESIAN_POINT ( 'NONE',  ( 1.547277799339723758, 7.618736734813467137, -10.12789507952378898 ) ) ;
#7027 = CARTESIAN_POINT ( 'NONE',  ( 0.2648978790185602672, 7.769924372105329269, -9.465406350830530613 ) ) ;
#7028 = CARTESIAN_POINT ( 'NONE',  ( 6.824632601691471123, -31.95616727126968115, -13.35541573562854722 ) ) ;
#7029 = FACE_OUTER_BOUND ( 'NONE', #65297, .T. ) ;
#7030 = EDGE_CURVE ( 'NONE', #38363, #33343, #41061, .T. ) ;
#7031 = CARTESIAN_POINT ( 'NONE',  ( -37.00000000000000711, 11.90598845858533750, 4.561791185930457182 ) ) ;
#7032 = DIRECTION ( 'NONE',  ( -1.000000000000000000, -0.000000000000000000, 0.000000000000000000 ) ) ;
#7033 = DIRECTION ( 'NONE',  ( 1.000000000000000000, -0.000000000000000000, 0.000000000000000000 ) ) ;
#7034 = DIRECTION ( 'NONE',  ( -0.3865475372811021937, 0.8730852074079739067, 0.2971585806051880718 ) ) ;
#7035 = ORIENTED_EDGE ( 'NONE', *, *, #28329, .T. ) ;
#7036 = LINE ( 'NONE', #46954, #16251 ) ;
#7037 = ORIENTED_EDGE ( 'NONE', *, *, #63896, .F. ) ;
#7038 = CARTESIAN_POINT ( 'NONE',  ( 0.2833330754217368019, -4.379886056890972768, 11.44258640049859821 ) ) ;
#7039 = CARTESIAN_POINT ( 'NONE',  ( 2.297017764049617661, 6.708511771223625964, 3.682881532880238673 ) ) ;
#7040 = ORIENTED_EDGE ( 'NONE', *, *, #40363, .F. ) ;
#7041 = EDGE_CURVE ( 'NONE', #20378, #22014, #26576, .T. ) ;
#7042 = FACE_OUTER_BOUND ( 'NONE', #49879, .T. ) ;
#7043 = CARTESIAN_POINT ( 'NONE',  ( 0.2717059086739041507, 12.03041489115254414, -2.300075171420108422 ) ) ;
#7044 = CARTESIAN_POINT ( 'NONE',  ( 0.2652384770603665731, -9.338499095996370514, -7.922175044417074652 ) ) ;
#7045 = MANIFOLD_SOLID_BREP ( 'Boss-Extrude1', #36549 ) ;
#7046 = EDGE_LOOP ( 'NONE', ( #33677, #6703, #10179, #8429 ) ) ;
#7047 = ADVANCED_FACE ( 'NONE', ( #27093 ), #31094, .T. ) ;
#7048 = ORIENTED_EDGE ( 'NONE', *, *, #39665, .F. ) ;
#7049 = DIRECTION ( 'NONE',  ( -0.3865475372811021937, -0.01937500237527774866, -0.9220659470476463282 ) ) ;
#7050 = EDGE_LOOP ( 'NONE', ( #48091, #28303, #64506, #65702, #6700, #24057, #47370, #28776, #13834, #53088, #46274, #4688, #27306, #41436, #45053, #8465, #39325, #23622, #35158, #42018, #21127, #51776, #59081, #50513, #15980, #45943, #52284, #7865, #961, #4341, #64179, #28023, #36455, #26891 ) ) ;
#7051 = CYLINDRICAL_SURFACE ( 'NONE', #55205, 12.75000000000000178 ) ;
#7052 = CARTESIAN_POINT ( 'NONE',  ( -27.08426571771018487, 2.098821047392067207, 0.9198084705429259156 ) ) ;
#7053 = CARTESIAN_POINT ( 'NONE',  ( -35.04643116707788408, -0.01204777744936991191, 0.001845126042312322800 ) ) ;
#7054 = EDGE_CURVE ( 'NONE', #54831, #39860, #8189, .T. ) ;
#7055 = CARTESIAN_POINT ( 'NONE',  ( -35.00000000000000000, -9.348667969174350389, -7.817492529713957694 ) ) ;
#7056 = ORIENTED_EDGE ( 'NONE', *, *, #6263, .T. ) ;
#7057 = CARTESIAN_POINT ( 'NONE',  ( 0.3040950598368144520, 12.02925914197705204, 2.376091969481256783 ) ) ;
#7058 = AXIS2_PLACEMENT_3D ( 'NONE', #28995, #19350, #49307 ) ;
#7059 = CARTESIAN_POINT ( 'NONE',  ( 18.57729641407469501, -29.86520738451960355, -7.358162954095295305 ) ) ;
#7060 = DIRECTION ( 'NONE',  ( 0.000000000000000000, 0.01356324068817998940, -0.9999080150203990547 ) ) ;
#7061 = EDGE_CURVE ( 'NONE', #82, #27703, #37198, .T. ) ;
#7062 = CARTESIAN_POINT ( 'NONE',  ( -35.00000000000000000, 12.16632754454237819, -0.7008968033237440443 ) ) ;
#7063 = CARTESIAN_POINT ( 'NONE',  ( 0.3675815128205894289, 10.50067073900651771, 6.367184624550202621 ) ) ;
#7064 = EDGE_CURVE ( 'NONE', #7826, #45182, #34022, .T. ) ;
#7065 = CARTESIAN_POINT ( 'NONE',  ( 37.00000000000000711, -0.8294751490778421443, 12.15823808070322976 ) ) ;
#7066 = DIRECTION ( 'NONE',  ( 1.000000000000000000, -0.000000000000000000, 0.000000000000000000 ) ) ;
#7067 = CARTESIAN_POINT ( 'NONE',  ( -22.28546858134833286, -2.654201075783114927, -2.587024666338680667 ) ) ;
#7068 = EDGE_CURVE ( 'NONE', #65184, #19802, #37048, .T. ) ;
#7069 = ORIENTED_EDGE ( 'NONE', *, *, #49496, .T. ) ;
#7070 = ADVANCED_FACE ( 'NONE', ( #43946 ), #18018, .T. ) ;
#7071 = CARTESIAN_POINT ( 'NONE',  ( -14.73932195233055609, 7.919210176484706487, 10.93330280096819074 ) ) ;
#7072 = CARTESIAN_POINT ( 'NONE',  ( 1.000000000000000888, -7.387287142779332960, -1.295372019972250710 ) ) ;
#7073 = ORIENTED_EDGE ( 'NONE', *, *, #62336, .F. ) ;
#7074 = CARTESIAN_POINT ( 'NONE',  ( -22.27718150314433387, -3.596602356343906681, 0.7862703917636705286 ) ) ;
#7075 = LINE ( 'NONE', #2088, #58740 ) ;
#7076 = EDGE_LOOP ( 'NONE', ( #27806, #58221, #50069, #63938, #7193 ) ) ;
#7077 = EDGE_CURVE ( 'NONE', #47218, #3051, #13027, .T. ) ;
#7078 = CARTESIAN_POINT ( 'NONE',  ( 47.00000000000000711, 4.705694406421931860E-17, -3.469127814946512892E-15 ) ) ;
#7079 = ORIENTED_EDGE ( 'NONE', *, *, #28541, .F. ) ;
#7080 = FACE_OUTER_BOUND ( 'NONE', #53658, .T. ) ;
#7081 = ORIENTED_EDGE ( 'NONE', *, *, #43223, .T. ) ;
#7082 = ORIENTED_EDGE ( 'NONE', *, *, #53860, .F. ) ;
#7083 = FACE_OUTER_BOUND ( 'NONE', #31474, .T. ) ;
#7084 = ORIENTED_EDGE ( 'NONE', *, *, #47893, .T. ) ;
#7085 = DIRECTION ( 'NONE',  ( -1.000000000000000000, 0.000000000000000000, 0.000000000000000000 ) ) ;
#7086 = B_SPLINE_CURVE_WITH_KNOTS ( 'NONE', 3,
 ( #58380, #12160, #37763, #53053, #25917, #42730, #22137, #7847, #27781, #22471, #43069, #48085, #63029, #15907, #43388, #28122 ),
 .UNSPECIFIED., .F., .F.,
 ( 4, 3, 3, 3, 3, 4 ),
 ( 0.000000000000000000, 0.0002999043160757463937, 0.0005998071753051251783, 0.0008997092107374914235, 0.001204458948196565800, 0.001510329163478326504 ),
 .UNSPECIFIED. ) ;
#7087 = CARTESIAN_POINT ( 'NONE',  ( 35.00000000000000000, -0.06441628369827803735, 12.18632975068352309 ) ) ;
#7088 = CARTESIAN_POINT ( 'NONE',  ( 22.57855258442564761, -4.427776684447072952, -12.75322679295976691 ) ) ;
#7089 = DIRECTION ( 'NONE',  ( 1.000000000000000000, -0.000000000000000000, -0.000000000000000000 ) ) ;
#7090 = VERTEX_POINT ( 'NONE', #48616 ) ;
#7091 = FACE_OUTER_BOUND ( 'NONE', #3777, .T. ) ;
#7092 = CARTESIAN_POINT ( 'NONE',  ( 4.225235259830817824, -25.92188032005471143, 15.36840686706593928 ) ) ;
#7093 = DIRECTION ( 'NONE',  ( 0.000000000000000000, 0.9467777615094560284, 0.3218879778916007295 ) ) ;
#7095 = VERTEX_POINT ( 'NONE', #3069 ) ;
#7094 = CARTESIAN_POINT ( 'NONE',  ( -26.14647939271262800, 10.67107426152631788, 5.490406654534011999 ) ) ;
#7096 = LINE ( 'NONE', #32029, #41587 ) ;
#7097 = ORIENTED_EDGE ( 'NONE', *, *, #31480, .F. ) ;
#7098 = CARTESIAN_POINT ( 'NONE',  ( 2.350038591458107451, 4.746773736939504218, 9.502240128958677090 ) ) ;
#7099 = ORIENTED_EDGE ( 'NONE', *, *, #6223, .F. ) ;
#7100 = CIRCLE ( 'NONE', #51697, 4.999999999999999112 ) ;
#7101 = CARTESIAN_POINT ( 'NONE',  ( 21.61122408824027374, -11.12492833342144216, -4.503027499503673425 ) ) ;
#7102 = CARTESIAN_POINT ( 'NONE',  ( -18.25006854224444908, -9.443202773001939221, 25.00000000000000000 ) ) ;
#7103 = CYLINDRICAL_SURFACE ( 'NONE', #13134, 4.999999999999999112 ) ;
#7105 = EDGE_CURVE ( 'NONE', #41254, #47877, #49933, .T. ) ;
#7104 = EDGE_LOOP ( 'NONE', ( #58177, #45034, #28856, #23703 ) ) ;
#7106 = DIRECTION ( 'NONE',  ( 1.000000000000000000, 0.000000000000000000, 0.000000000000000000 ) ) ;
#7107 = CARTESIAN_POINT ( 'NONE',  ( 5.515539859299206427, -0.004509673239148311030, -0.004037661319610873038 ) ) ;
#7108 = CARTESIAN_POINT ( 'NONE',  ( 2.241536586108912044, -5.844297002038577382, 4.912162027558472310 ) ) ;
#7109 = EDGE_LOOP ( 'NONE', ( #39986, #54631, #53564, #3543 ) ) ;
#7110 = EDGE_CURVE ( 'NONE', #39817, #9384, #5365, .T. ) ;
#7111 = EDGE_LOOP ( 'NONE', ( #42813, #1695, #4466, #14105 ) ) ;
#7112 = DIRECTION ( 'NONE',  ( 0.000000000000000000, -0.6943713148249534006, 0.7196168960969896444 ) ) ;
#7113 = ORIENTED_EDGE ( 'NONE', *, *, #29459, .T. ) ;
#7114 = ORIENTED_EDGE ( 'NONE', *, *, #24960, .T. ) ;
#7115 = EDGE_CURVE ( 'NONE', #12300, #8992, #29740, .T. ) ;
#7116 = DIRECTION ( 'NONE',  ( -1.000000000000000000, 0.000000000000000000, 0.000000000000000000 ) ) ;
#7117 = CARTESIAN_POINT ( 'NONE',  ( 37.00000000000000711, 10.42955799785319826, -6.303578524886986223 ) ) ;
#7118 = DIRECTION ( 'NONE',  ( 0.000000000000000000, -0.01356324068817998940, 0.9999080150203990547 ) ) ;
#7119 = CARTESIAN_POINT ( 'NONE',  ( -22.30398854582848145, 1.062335901716063624, 3.608860109585115605 ) ) ;
#7120 = CARTESIAN_POINT ( 'NONE',  ( -35.00000000000000000, 0.000000000000000000, 0.000000000000000000 ) ) ;
#7121 = DIRECTION ( 'NONE',  ( 0.000000000000000000, 0.01356324068817991828, -0.9999080150203990547 ) ) ;
#7122 = DIRECTION ( 'NONE',  ( -1.000000000000000000, 0.000000000000000000, 0.000000000000000000 ) ) ;
#7123 = VERTEX_POINT ( 'NONE', #54597 ) ;
#7124 = CARTESIAN_POINT ( 'NONE',  ( 1.719304012338199295, 11.67935079956398958, 5.066286238785226992 ) ) ;
#7125 = CARTESIAN_POINT ( 'NONE',  ( -22.31213670151049300, -3.145266995071682725, 2.108126385153798132 ) ) ;
#7126 = EDGE_CURVE ( 'NONE', #40853, #18660, #42502, .T. ) ;
#7127 = EDGE_CURVE ( 'NONE', #35179, #3105, #5807, .T. ) ;
#7128 = CARTESIAN_POINT ( 'NONE',  ( 0.2911222467163570027, 4.392242282525022468, -11.44063169461051288 ) ) ;
#7129 = DIRECTION ( 'NONE',  ( -1.000000000000000000, 0.000000000000000000, 0.000000000000000000 ) ) ;
#7130 = DIRECTION ( 'NONE',  ( 1.000000000000000000, 0.000000000000000000, -0.000000000000000000 ) ) ;
#7131 = CARTESIAN_POINT ( 'NONE',  ( -47.00000000000000711, 0.000000000000000000, 0.000000000000000000 ) ) ;
#7132 = CARTESIAN_POINT ( 'NONE',  ( 0.9232058338315058954, 12.21058493388777144, -2.536181247095240288 ) ) ;
#7133 = ORIENTED_EDGE ( 'NONE', *, *, #59433, .F. ) ;
#7134 = DIRECTION ( 'NONE',  ( 1.000000000000000000, 0.000000000000000000, 0.000000000000000000 ) ) ;
#7135 = CARTESIAN_POINT ( 'NONE',  ( 0.3106921474978482922, -1.896868624982982920, -12.11369598333778796 ) ) ;
#7136 = DIRECTION ( 'NONE',  ( 0.000000000000000000, 0.01356324068817998940, -0.9999080150203990547 ) ) ;
#7137 = DIRECTION ( 'NONE',  ( 0.3865475372811021382, 0.9220659470476459951, 0.01937500237529380179 ) ) ;
#7138 = B_SPLINE_CURVE_WITH_KNOTS ( 'NONE', 3,
 ( #33118, #38778, #22837, #18170, #59075, #23480, #44088, #39085, #59379, #53429, #43092, #43757, #54735, #64038, #18522, #33766, #8502, #54411, #27810, #63368, #23827, #8843 ),
 .UNSPECIFIED., .F., .F.,
 ( 4, 3, 3, 3, 3, 3, 3, 4 ),
 ( 9.813077866771631884E-18, 4.447697177976269703E-05, 6.624143997791186948E-05, 8.800576886944293459E-05, 0.0001097699864780885595, 0.0001315341395364375715, 0.0001760120188223282935, 0.0001867971373174741171 ),
 .UNSPECIFIED. ) ;
#7139 = AXIS2_PLACEMENT_3D ( 'NONE', #2308, #22584, #36882 ) ;
#7140 = ADVANCED_FACE ( 'NONE', ( #49596 ), #19001, .T. ) ;
#7141 = AXIS2_PLACEMENT_3D ( 'NONE', #29736, #24427, #60334 ) ;
#7142 = ADVANCED_FACE ( 'NONE', ( #3743 ), #34911, .T. ) ;
#7143 = CYLINDRICAL_SURFACE ( 'NONE', #30940, 4.500030059823568074 ) ;
#7144 = DIRECTION ( 'NONE',  ( 1.000000000000000000, -0.000000000000000000, 0.000000000000000000 ) ) ;
#7145 = ORIENTED_EDGE ( 'NONE', *, *, #39752, .T. ) ;
#7146 = CARTESIAN_POINT ( 'NONE',  ( 2.406456491625610372, 7.573451137023644364, -7.176027849161648930 ) ) ;
#7147 = CARTESIAN_POINT ( 'NONE',  ( -27.64986549192623499, -12.88105143700861888, -4.050455452492842667 ) ) ;
#7148 = FACE_OUTER_BOUND ( 'NONE', #19959, .T. ) ;
#7149 = FACE_OUTER_BOUND ( 'NONE', #8938, .T. ) ;
#7150 = VERTEX_POINT ( 'NONE', #24305 ) ;
#7151 = EDGE_CURVE ( 'NONE', #47299, #27224, #53167, .T. ) ;
#7152 = DIRECTION ( 'NONE',  ( -1.000000000000000000, 0.000000000000000000, -0.000000000000000000 ) ) ;
#7153 = LINE ( 'NONE', #27428, #59613 ) ;
#7154 = ORIENTED_EDGE ( 'NONE', *, *, #50173, .T. ) ;
#7155 = CARTESIAN_POINT ( 'NONE',  ( -36.00000000000000711, -12.60630747491664572, 1.908798535168333643 ) ) ;
#7156 = CARTESIAN_POINT ( 'NONE',  ( 2.000000000000001776, -5.997115278587605403, -3.485633455389573587 ) ) ;
#7157 = ORIENTED_EDGE ( 'NONE', *, *, #48450, .F. ) ;
#7158 = DIRECTION ( 'NONE',  ( -1.000000000000000000, 0.000000000000000000, 0.000000000000000000 ) ) ;
#7159 = DIRECTION ( 'NONE',  ( 0.9688695217174486674, 0.000000000000000000, 0.2475719085175097645 ) ) ;
#7160 = CARTESIAN_POINT ( 'NONE',  ( 0.3675815128205894289, 4.447030445008180344, 11.44679196252410946 ) ) ;
#7161 = DIRECTION ( 'NONE',  ( -1.000000000000000000, 0.000000000000000000, 0.000000000000000000 ) ) ;
#7162 = CARTESIAN_POINT ( 'NONE',  ( 0.2657645697724702050, -11.45515365350258818, -4.330388001246531893 ) ) ;
#7163 = CARTESIAN_POINT ( 'NONE',  ( 1.014383007554950478, 11.88680274101312406, 3.853787798429443079 ) ) ;
#7165 = EDGE_LOOP ( 'NONE', ( #45416, #32914, #15881, #61110 ) ) ;
#7164 = CARTESIAN_POINT ( 'NONE',  ( -2.952869152607107139, 12.96714474214482138, 3.755417052241487585 ) ) ;
#7166 = FACE_OUTER_BOUND ( 'NONE', #42777, .T. ) ;
#7167 = ORIENTED_EDGE ( 'NONE', *, *, #37051, .T. ) ;
#7168 = CARTESIAN_POINT ( 'NONE',  ( 22.88594695219327235, -4.822122601967141264, -10.98850006195556261 ) ) ;
#7169 = VERTEX_POINT ( 'NONE', #44570 ) ;
#7170 = FACE_OUTER_BOUND ( 'NONE', #23356, .T. ) ;
#7171 = CARTESIAN_POINT ( 'NONE',  ( -14.43403921783542287, -30.05772736395422484, 4.235651140255900060 ) ) ;
#7172 = AXIS2_PLACEMENT_3D ( 'NONE', #35635, #34962, #25023 ) ;
#7173 = CARTESIAN_POINT ( 'NONE',  ( 1.719304012338820131, 1.452142814150020556, 12.64775761152757561 ) ) ;
#7174 = CARTESIAN_POINT ( 'NONE',  ( -31.24126863879125438, -3.096129103239070091, -23.22707964006411530 ) ) ;
#7175 = DIRECTION ( 'NONE',  ( 0.000000000000000000, 0.2006870767258889243, -0.9796553971857742127 ) ) ;
#7176 = ORIENTED_EDGE ( 'NONE', *, *, #13778, .T. ) ;
#7177 = EDGE_CURVE ( 'NONE', #27528, #476, #39267, .T. ) ;
#7178 = CARTESIAN_POINT ( 'NONE',  ( -24.42312813602775634, -7.374403702826844764, 9.469279496625576442 ) ) ;
#7179 = CARTESIAN_POINT ( 'NONE',  ( 3.991229212642302127, 6.917749631459077619, -11.62716796859311863 ) ) ;
#7180 = ORIENTED_EDGE ( 'NONE', *, *, #60559, .T. ) ;
#7181 = ORIENTED_EDGE ( 'NONE', *, *, #25198, .T. ) ;
#7182 = CARTESIAN_POINT ( 'NONE',  ( 35.00000000000000000, -2.080187960898473243, 12.57916205664482945 ) ) ;
#7183 = ORIENTED_EDGE ( 'NONE', *, *, #29771, .F. ) ;
#7184 = DIRECTION ( 'NONE',  ( -1.000000000000000000, 0.000000000000000000, 0.000000000000000000 ) ) ;
#7185 = VECTOR ( 'NONE', #62977, 1000.000000000000000 ) ;
#7186 = CARTESIAN_POINT ( 'NONE',  ( -35.00000000000000000, -4.824807283154036952, -11.80185301892985805 ) ) ;
#7187 = DIRECTION ( 'NONE',  ( 0.000000000000000000, -0.04924826701375289995, -0.9987865678893274035 ) ) ;
#7188 = CARTESIAN_POINT ( 'NONE',  ( 0.5547464869798257592, 12.20441397277155993, 1.842327806480188235 ) ) ;
#7189 = CARTESIAN_POINT ( 'NONE',  ( -37.00000000000000711, 11.01837265713082203, -6.415447294506590126 ) ) ;
#7190 = CARTESIAN_POINT ( 'NONE',  ( 2.507146904658099196, -7.640248566386908635, 1.127530020444472703 ) ) ;
#7191 = AXIS2_PLACEMENT_3D ( 'NONE', #29658, #65254, #24694 ) ;
#7192 = CARTESIAN_POINT ( 'NONE',  ( 2.247206125382830155, 7.499376972323892332, 1.439877054338129847 ) ) ;
#7193 = ORIENTED_EDGE ( 'NONE', *, *, #33691, .T. ) ;
#7194 = DIRECTION ( 'NONE',  ( 1.000000000000000000, 0.000000000000000000, 0.000000000000000000 ) ) ;
#7195 = ORIENTED_EDGE ( 'NONE', *, *, #47009, .T. ) ;
#7196 = DIRECTION ( 'NONE',  ( 0.000000000000000000, 0.01356324068817992175, -0.9999080150203990547 ) ) ;
#7197 = EDGE_CURVE ( 'NONE', #27863, #14116, #13997, .T. ) ;
#7198 = FACE_OUTER_BOUND ( 'NONE', #38929, .T. ) ;
#7199 = CARTESIAN_POINT ( 'NONE',  ( 2.298277635560275645, -3.968740875991601413, 6.543949079923926604 ) ) ;
#7200 = DIRECTION ( 'NONE',  ( 0.000000000000000000, -0.9987865678893272925, 0.04924826701375684818 ) ) ;
#7201 = EDGE_CURVE ( 'NONE', #39829, #46242, #24474, .T. ) ;
#7202 = VERTEX_POINT ( 'NONE', #19335 ) ;
#7203 = ORIENTED_EDGE ( 'NONE', *, *, #12685, .F. ) ;
#7204 = CARTESIAN_POINT ( 'NONE',  ( -35.00000000000000000, 2.346765782874606465, -11.95840593935198903 ) ) ;
#7205 = EDGE_LOOP ( 'NONE', ( #28347, #58719, #31948, #35863 ) ) ;
#7206 = CARTESIAN_POINT ( 'NONE',  ( 0.2671309869109482760, 7.747281147400671308, -9.484919892054740842 ) ) ;
#7207 = DIRECTION ( 'NONE',  ( 0.000000000000000000, -0.01356324068817992175, 0.9999080150203990547 ) ) ;
#7208 = CARTESIAN_POINT ( 'NONE',  ( 0.3040950598368144520, -3.956873563689455420, -11.60568999039898941 ) ) ;
#7209 = CARTESIAN_POINT ( 'NONE',  ( 3.092491956585914359, -5.424230976134662541, -5.768471164322597211 ) ) ;
#7210 = EDGE_LOOP ( 'NONE', ( #38580, #44876 ) ) ;
#7211 = CARTESIAN_POINT ( 'NONE',  ( 0.2915757698887290750, 12.10419100255479385, 1.916267336493217233 ) ) ;
#7212 = CARTESIAN_POINT ( 'NONE',  ( 37.00000000000000711, -11.66664283989683426, -5.143145423404238414 ) ) ;
#7213 = CARTESIAN_POINT ( 'NONE',  ( -27.35552965826137140, 0.2619431035392177365, -3.094132632038957276 ) ) ;
#7214 = CARTESIAN_POINT ( 'NONE',  ( -22.23402523511428086, 1.734723475976807094E-15, -8.673617379884035472E-15 ) ) ;
#7215 = EDGE_CURVE ( 'NONE', #27631, #49629, #17694, .T. ) ;
#7216 = AXIS2_PLACEMENT_3D ( 'NONE', #47923, #19945, #29277 ) ;
#7217 = CARTESIAN_POINT ( 'NONE',  ( 0.3160775863651085205, 6.338373607799337783, -10.49803827792115740 ) ) ;
#7218 = LINE ( 'NONE', #53459, #10657 ) ;
#7219 = AXIS2_PLACEMENT_3D ( 'NONE', #53087, #33127, #17186 ) ;
#7220 = ORIENTED_EDGE ( 'NONE', *, *, #41243, .T. ) ;
#7221 = CARTESIAN_POINT ( 'NONE',  ( -16.02805653289875920, -28.24868299250882941, -10.29995797863329621 ) ) ;
#7222 = ORIENTED_EDGE ( 'NONE', *, *, #41135, .T. ) ;
#7223 = AXIS2_PLACEMENT_3D ( 'NONE', #34011, #44317, #58668 ) ;
#7224 = DIRECTION ( 'NONE',  ( 0.000000000000000000, 0.01356324068817991828, -0.9999080150203990547 ) ) ;
#7225 = CARTESIAN_POINT ( 'NONE',  ( 1.719304012339819332, -8.755325027794356174, 9.242227816401850760 ) ) ;
#7226 = CARTESIAN_POINT ( 'NONE',  ( 37.00000000000000711, 7.146664589317909488, -9.321877890560465119 ) ) ;
#7227 = AXIS2_PLACEMENT_3D ( 'NONE', #32054, #6815, #27084 ) ;
#7228 = PLANE ( 'NONE',  #58312 ) ;
#7229 = DIRECTION ( 'NONE',  ( 0.000000000000000000, 0.01356324068817992522, -0.9999080150203990547 ) ) ;
#7230 = EDGE_CURVE ( 'NONE', #33155, #19644, #61645, .T. ) ;
#7231 = VERTEX_POINT ( 'NONE', #50254 ) ;
#7232 = EDGE_LOOP ( 'NONE', ( #14773, #39236, #11311, #55159 ) ) ;
#7233 = CYLINDRICAL_SURFACE ( 'NONE', #35009, 6.936499999999988120 ) ;
#7234 = EDGE_LOOP ( 'NONE', ( #16277, #61881, #32297, #5411 ) ) ;
#7235 = CARTESIAN_POINT ( 'NONE',  ( -37.00000000000000711, 12.16893194857550142, 3.805206332242515366 ) ) ;
#7236 = DIRECTION ( 'NONE',  ( 0.000000000000000000, -0.6943713148249690548, 0.7196168960969744344 ) ) ;
#7237 = CARTESIAN_POINT ( 'NONE',  ( 0.3675815128205894289, -1.872154644482166397, 12.13672785388549613 ) ) ;
#7238 = FACE_OUTER_BOUND ( 'NONE', #32430, .T. ) ;
#7239 = CARTESIAN_POINT ( 'NONE',  ( 1.109979610371589320, -7.679283534372219222, -9.898186741522541965 ) ) ;
#7240 = CARTESIAN_POINT ( 'NONE',  ( -4.806344283790351390, -7.508992741355383416, 25.00000000000000000 ) ) ;
#7241 = CARTESIAN_POINT ( 'NONE',  ( -18.04458733766117362, 12.91933584589294703, 3.916728392552376370 ) ) ;
#7242 = EDGE_LOOP ( 'NONE', ( #3994, #8994, #8240, #1706 ) ) ;
#7243 = ORIENTED_EDGE ( 'NONE', *, *, #37172, .T. ) ;
#7244 = CARTESIAN_POINT ( 'NONE',  ( 35.00000000000000000, 1.039216533672905785, -11.70009620280412221 ) ) ;
#7245 = ORIENTED_EDGE ( 'NONE', *, *, #29515, .F. ) ;
#7246 = MANIFOLD_SOLID_BREP ( 'Move Face1', #25976 ) ;
#7247 = SURFACE_SIDE_STYLE ('',( #33521 ) ) ;
#7248 = DIRECTION ( 'NONE',  ( -1.000000000000000000, 0.000000000000000000, 0.000000000000000000 ) ) ;
#7249 = DIRECTION ( 'NONE',  ( -0.000000000000000000, -1.000000000000000000, -0.000000000000000000 ) ) ;
#7250 = CARTESIAN_POINT ( 'NONE',  ( 1.000000000000000888, -5.097042323172408906, -5.501832381651512449 ) ) ;
#7251 = ORIENTED_EDGE ( 'NONE', *, *, #5418, .T. ) ;
#7252 = DIRECTION ( 'NONE',  ( 1.000000000000000000, -0.000000000000000000, 0.000000000000000000 ) ) ;
#7253 = EDGE_CURVE ( 'NONE', #18329, #12876, #3292, .T. ) ;
#7254 = CARTESIAN_POINT ( 'NONE',  ( -19.56743653832047158, -30.00000000000000355, -5.000000000000000888 ) ) ;
#7255 = CIRCLE ( 'NONE', #47617, 2.899999999999995026 ) ;
#7256 = CARTESIAN_POINT ( 'NONE',  ( -22.27218376572352554, -3.670373711461420108, 0.3046453028544536812 ) ) ;
#7257 = VERTEX_POINT ( 'NONE', #61509 ) ;
#7258 = ORIENTED_EDGE ( 'NONE', *, *, #44253, .T. ) ;
#7259 = CARTESIAN_POINT ( 'NONE',  ( -16.98800322446194855, 2.922502605998049674, -11.63868456991314027 ) ) ;
#7260 = EDGE_CURVE ( 'NONE', #49200, #27489, #26278, .T. ) ;
#7261 = VERTEX_POINT ( 'NONE', #6666 ) ;
#7262 = ORIENTED_EDGE ( 'NONE', *, *, #5829, .T. ) ;
#7263 = CARTESIAN_POINT ( 'NONE',  ( 2.269879328256730222, 3.949706986712200329, 6.544400685875841894 ) ) ;
#7264 = ORIENTED_EDGE ( 'NONE', *, *, #31188, .F. ) ;
#7265 = EDGE_LOOP ( 'NONE', ( #1805, #60073, #40210, #40713 ) ) ;
#7266 = CARTESIAN_POINT ( 'NONE',  ( 35.00000000000000000, 4.705694406421931860E-17, -3.469127814946512892E-15 ) ) ;
#7268 = CIRCLE ( 'NONE', #51863, 5.000000000000000000 ) ;
#7267 = CARTESIAN_POINT ( 'NONE',  ( 0.000000000000000000, 4.472310526050767621, 6.020667617347370104 ) ) ;
#7269 = CARTESIAN_POINT ( 'NONE',  ( 36.00000000000000711, 10.12742074351896449, -7.745827850123049529 ) ) ;
#7271 = EDGE_CURVE ( 'NONE', #39378, #9622, #52123, .T. ) ;
#7270 = FACE_OUTER_BOUND ( 'NONE', #63258, .T. ) ;
#7272 = CARTESIAN_POINT ( 'NONE',  ( -37.00000000000000711, -10.93004082984014147, -6.564808257521884904 ) ) ;
#7273 = LINE ( 'NONE', #1975, #43934 ) ;
#7274 = AXIS2_PLACEMENT_3D ( 'NONE', #26, #16317, #40251 ) ;
#7275 = AXIS2_PLACEMENT_3D ( 'NONE', #16090, #31698, #36378 ) ;
#7276 = ORIENTED_EDGE ( 'NONE', *, *, #22198, .T. ) ;
#7277 = CARTESIAN_POINT ( 'NONE',  ( -35.00000000000000000, 10.25474254703952859, 6.584150480049587806 ) ) ;
#7278 = CARTESIAN_POINT ( 'NONE',  ( -22.27715239060371744, 2.689999469426704426, -2.513478159995845562 ) ) ;
#7279 = AXIS2_PLACEMENT_3D ( 'NONE', #54886, #5332, #19653 ) ;
#7280 = DIRECTION ( 'NONE',  ( 0.000000000000000000, 0.000000000000000000, 1.000000000000000000 ) ) ;
#7281 = EDGE_CURVE ( 'NONE', #49136, #5918, #64863, .T. ) ;
#7282 = CARTESIAN_POINT ( 'NONE',  ( 0.3218525148189819718, -2.370084734146296501, 12.03385614540603221 ) ) ;
#7283 = DIRECTION ( 'NONE',  ( -1.000000000000000000, 0.000000000000000000, 0.000000000000000000 ) ) ;
#7284 = CARTESIAN_POINT ( 'NONE',  ( 19.56743653832047158, -30.00000000000000000, -5.000000000000000888 ) ) ;
#7285 = CIRCLE ( 'NONE', #15769, 12.75000000000000178 ) ;
#7286 = ORIENTED_EDGE ( 'NONE', *, *, #7526, .F. ) ;
#7287 = DIRECTION ( 'NONE',  ( 1.000000000000000000, 0.000000000000000000, 0.000000000000000000 ) ) ;
#7288 = ORIENTED_EDGE ( 'NONE', *, *, #5145, .F. ) ;
#7289 = DIRECTION ( 'NONE',  ( -1.000000000000000000, 0.000000000000000000, 0.000000000000000000 ) ) ;
#7290 = DIRECTION ( 'NONE',  ( 0.000000000000000000, -0.01356324068817991828, 0.9999080150203990547 ) ) ;
#7291 = CARTESIAN_POINT ( 'NONE',  ( 12.52916646628448127, -13.04480612694435671, -3.481077218509882165 ) ) ;
#7292 = CARTESIAN_POINT ( 'NONE',  ( 2.903928887688274063, 5.221047506681124162, -7.046356840275977973 ) ) ;
#7293 = DIRECTION ( 'NONE',  ( -1.000000000000000000, 0.000000000000000000, 0.000000000000000000 ) ) ;
#7294 = ORIENTED_EDGE ( 'NONE', *, *, #15988, .T. ) ;
#7295 = DIRECTION ( 'NONE',  ( 1.000000000000000000, 0.000000000000000000, 0.000000000000000000 ) ) ;
#7296 = CARTESIAN_POINT ( 'NONE',  ( 0.2833330754217374681, 2.326361469893388545, -12.02930703389097467 ) ) ;
#7297 = DIRECTION ( 'NONE',  ( 0.000000000000000000, -0.9999080150203992767, -0.01356324068816951341 ) ) ;
#7298 = CARTESIAN_POINT ( 'NONE',  ( -3.936294612518189684, 11.99894110015778814, 6.199062502346824211 ) ) ;
#7299 = AXIS2_PLACEMENT_3D ( 'NONE', #36236, #45564, #35590 ) ;
#7300 = DIRECTION ( 'NONE',  ( 0.000000000000000000, -0.2960891610144378849, -0.9551603052523520709 ) ) ;
#7301 = ORIENTED_EDGE ( 'NONE', *, *, #6444, .T. ) ;
#7302 = CIRCLE ( 'NONE', #44457, 4.999999999999999112 ) ;
#7303 = DIRECTION ( 'NONE',  ( -1.000000000000000000, 0.000000000000000000, 0.000000000000000000 ) ) ;
#7304 = CARTESIAN_POINT ( 'NONE',  ( -1.846890694235063357, -30.59587057577333624, 15.23951446459229864 ) ) ;
#7305 = EDGE_CURVE ( 'NONE', #18880, #939, #45455, .T. ) ;
#7306 = AXIS2_PLACEMENT_3D ( 'NONE', #3990, #48332, #24254 ) ;
#7307 = EDGE_CURVE ( 'NONE', #18956, #48492, #48954, .T. ) ;
#7308 = ORIENTED_EDGE ( 'NONE', *, *, #47313, .F. ) ;
#7309 = CARTESIAN_POINT ( 'NONE',  ( -9.730999143771754234, 11.41738891610202344, -7.214510183280433253 ) ) ;
#7310 = ORIENTED_EDGE ( 'NONE', *, *, #63153, .F. ) ;
#7311 = DIRECTION ( 'NONE',  ( 0.000000000000000000, 0.01356324068817991828, -0.9999080150203990547 ) ) ;
#7312 = CARTESIAN_POINT ( 'NONE',  ( -27.10719052120871098, -1.714424047991075506, -1.622102031466694072 ) ) ;
#7313 = CARTESIAN_POINT ( 'NONE',  ( 1.547277799338532933, -7.618736734813612799, 10.12789507952316725 ) ) ;
#7314 = CONICAL_SURFACE ( 'NONE', #44335, 7.938172270156617749, 1.280189991382167047 ) ;
#7315 = CARTESIAN_POINT ( 'NONE',  ( -22.29290468048228036, -2.097193667172395859, -3.083035815361915510 ) ) ;
#7316 = VERTEX_POINT ( 'NONE', #32547 ) ;
#7317 = VERTEX_POINT ( 'NONE', #33228 ) ;
#7318 = CIRCLE ( 'NONE', #43440, 4.999999999999999112 ) ;
#7319 = ORIENTED_EDGE ( 'NONE', *, *, #4712, .F. ) ;
#7320 = CARTESIAN_POINT ( 'NONE',  ( 36.00000000000000711, 0.4871980014161481631, -12.74068829017554272 ) ) ;
#7321 = CARTESIAN_POINT ( 'NONE',  ( -36.00000000000000711, -11.24036214326516436, -6.018036132182281506 ) ) ;
#7322 = EDGE_CURVE ( 'NONE', #21537, #27004, #23592, .T. ) ;
#7323 = ORIENTED_EDGE ( 'NONE', *, *, #62677, .F. ) ;
#7324 = DIRECTION ( 'NONE',  ( -1.000000000000000000, 0.000000000000000000, 0.000000000000000000 ) ) ;
#7325 = CARTESIAN_POINT ( 'NONE',  ( 2.276198483117262139, -7.555081843354695792, 1.175725118478829545 ) ) ;
#7326 = ORIENTED_EDGE ( 'NONE', *, *, #17485, .F. ) ;
#7327 = CARTESIAN_POINT ( 'NONE',  ( 2.000000000000001776, -7.484036900328561615, -0.4890722589970097345 ) ) ;
#7328 = EDGE_CURVE ( 'NONE', #4893, #58346, #26618, .T. ) ;
#7329 = EDGE_CURVE ( 'NONE', #36221, #31314, #2636, .T. ) ;
#7330 = CARTESIAN_POINT ( 'NONE',  ( 22.21055375121777686, -11.96926186085320154, -0.8606626411553354172 ) ) ;
#7331 = DIRECTION ( 'NONE',  ( 1.000000000000000000, 0.000000000000000000, 0.000000000000000000 ) ) ;
#7332 = ORIENTED_EDGE ( 'NONE', *, *, #41595, .F. ) ;
#7333 = VERTEX_POINT ( 'NONE', #22943 ) ;
#7334 = CARTESIAN_POINT ( 'NONE',  ( -35.00000000000000000, -12.08216339958899788, -1.591260454995368390 ) ) ;
#7335 = ADVANCED_FACE ( 'NONE', ( #43516 ), #43193, .T. ) ;
#7336 = ORIENTED_EDGE ( 'NONE', *, *, #20445, .T. ) ;
#7337 = CARTESIAN_POINT ( 'NONE',  ( -19.30822655423815348, 11.87722838305601591, -1.744063228020214185 ) ) ;
#7338 = VERTEX_POINT ( 'NONE', #38203 ) ;
#7339 = CARTESIAN_POINT ( 'NONE',  ( 2.241311220309555097, 3.736531646286262998, 6.657499176698799204 ) ) ;
#7340 = CARTESIAN_POINT ( 'NONE',  ( 10.63582125256380806, -33.14335888457106449, -11.52436878476450133 ) ) ;
#7341 = CARTESIAN_POINT ( 'NONE',  ( 37.00000000000000711, -10.92721691015452912, 4.309077947445766554 ) ) ;
#7343 = CARTESIAN_POINT ( 'NONE',  ( -35.00000000000000000, 0.000000000000000000, 0.000000000000000000 ) ) ;
#7342 = VECTOR ( 'NONE', #61202, 1000.000000000000000 ) ;
#7345 = EDGE_CURVE ( 'NONE', #43267, #56626, #31919, .T. ) ;
#7344 = DIRECTION ( 'NONE',  ( -1.000000000000000000, 0.000000000000000000, 0.000000000000000000 ) ) ;
#7346 = CARTESIAN_POINT ( 'NONE',  ( 1.549075743846935138, 6.912427991524520365, -10.62322497417011569 ) ) ;
#7347 = CARTESIAN_POINT ( 'NONE',  ( 37.00000000000000711, 4.705694406421931860E-17, -3.469127814946512892E-15 ) ) ;
#7348 = ORIENTED_EDGE ( 'NONE', *, *, #63306, .F. ) ;
#7349 = DIRECTION ( 'NONE',  ( 0.000000000000000000, -1.000000000000000000, 0.000000000000000000 ) ) ;
#7350 = ORIENTED_EDGE ( 'NONE', *, *, #10696, .F. ) ;
#7351 = CARTESIAN_POINT ( 'NONE',  ( 35.00000000000000000, -1.171570255487531131, -11.68758509253248157 ) ) ;
#7352 = EDGE_CURVE ( 'NONE', #49132, #36604, #42261, .T. ) ;
#7353 = CARTESIAN_POINT ( 'NONE',  ( 35.00000000000000000, 3.645068577060024850, -11.16627499335656815 ) ) ;
#7354 = ORIENTED_EDGE ( 'NONE', *, *, #63549, .F. ) ;
#7355 = DIRECTION ( 'NONE',  ( -1.000000000000000000, 0.000000000000000000, 0.000000000000000000 ) ) ;
#7356 = CARTESIAN_POINT ( 'NONE',  ( 0.3474126878361767923, 6.359473273659701498, 10.49748369253934044 ) ) ;
#7357 = CARTESIAN_POINT ( 'NONE',  ( 2.000000000000001776, -6.796153407501448029, 1.388283512725787761 ) ) ;
#7358 = CIRCLE ( 'NONE', #29660, 12.18650000000000055 ) ;
#7359 = VERTEX_POINT ( 'NONE', #19582 ) ;
#7360 = ORIENTED_EDGE ( 'NONE', *, *, #1058, .T. ) ;
#7361 = CARTESIAN_POINT ( 'NONE',  ( 35.00000000000000000, 4.309077947445811851, 10.92721691015450780 ) ) ;
#7362 = EDGE_CURVE ( 'NONE', #58571, #61612, #62727, .T. ) ;
#7363 = AXIS2_PLACEMENT_3D ( 'NONE', #39531, #14261, #34541 ) ;
#7364 =( BOUNDED_CURVE ( )  B_SPLINE_CURVE ( 3, ( #56966, #770, #11708, #62257 ),
 .UNSPECIFIED., .F., .F. ) 
 B_SPLINE_CURVE_WITH_KNOTS ( ( 4, 4 ),
 ( 4.028742991341328405, 4.061025088278432449 ),
 .UNSPECIFIED. ) 
 CURVE ( )  GEOMETRIC_REPRESENTATION_ITEM ( )  RATIONAL_B_SPLINE_CURVE ( ( 1.000000000000000000, 0.9999131574035865500, 0.9999131574035865500, 1.000000000000000000 ) ) 
 REPRESENTATION_ITEM ( '' )  );
#7365 = ORIENTED_EDGE ( 'NONE', *, *, #52132, .T. ) ;
#7366 = CARTESIAN_POINT ( 'NONE',  ( 2.655192694323943670, -9.204230091442310524, -2.733486750964531087 ) ) ;
#7367 = CYLINDRICAL_SURFACE ( 'NONE', #11177, 12.75000000000000178 ) ;
#7368 = DIRECTION ( 'NONE',  ( 0.000000000000000000, -0.01356324068817998940, 0.9999080150203990547 ) ) ;
#7369 = CARTESIAN_POINT ( 'NONE',  ( -18.41858249652232615, -5.215518226302011229, 10.80810004108996125 ) ) ;
#7370 = VERTEX_POINT ( 'NONE', #9246 ) ;
#7371 = CONICAL_SURFACE ( 'NONE', #24371, 7.938172270156617749, 1.280189991382167047 ) ;
#7372 = CARTESIAN_POINT ( 'NONE',  ( -35.00000000000000000, -7.717887834988307105, 8.854740511458828678 ) ) ;
#7373 = LINE ( 'NONE', #38637, #54163 ) ;
#7374 = DIRECTION ( 'NONE',  ( 0.000000000000000000, -0.01356324068817991828, 0.9999080150203990547 ) ) ;
#7375 = DIRECTION ( 'NONE',  ( -0.3939253465568944290, 0.9068155327749432004, 0.1500280335741505655 ) ) ;
#7376 = DIRECTION ( 'NONE',  ( 0.000000000000000000, -0.9847383929261599445, 0.1740410799127720953 ) ) ;
#7377 = CYLINDRICAL_SURFACE ( 'NONE', #25639, 4.999999999999999112 ) ;
#7378 = CARTESIAN_POINT ( 'NONE',  ( 2.280717697723834370, -5.756537207046726223, 5.034569468898537181 ) ) ;
#7379 = CARTESIAN_POINT ( 'NONE',  ( 0.3675815128205912052, -3.951233083390393030, -11.62724744438069635 ) ) ;
#7380 = B_SPLINE_CURVE_WITH_KNOTS ( 'NONE', 3,
 ( #32759, #60264, #58071, #58745, #53067, #48431, #17506, #25031, #37777, #43082, #63358, #13167, #28137 ),
 .UNSPECIFIED., .F., .F.,
 ( 4, 3, 3, 3, 4 ),
 ( 0.0002792983885906313336, 0.0002796382307041357217, 0.0003495477861619808576, 0.0004194573423310284663, 0.0005586102576333146046 ),
 .UNSPECIFIED. ) ;
#7381 = EDGE_CURVE ( 'NONE', #58319, #21005, #19248, .T. ) ;
#7382 = AXIS2_PLACEMENT_3D ( 'NONE', #62313, #52690, #2134 ) ;
#7383 = VERTEX_POINT ( 'NONE', #35164 ) ;
#7384 = CARTESIAN_POINT ( 'NONE',  ( 2.255723233588950549, -0.1321982600347777204, 7.638048593862504454 ) ) ;
#7385 = CARTESIAN_POINT ( 'NONE',  ( 5.632405787856444412, -9.296918358879166178, 9.794213099898851027 ) ) ;
#7386 = VERTEX_POINT ( 'NONE', #24891 ) ;
#7387 = AXIS2_PLACEMENT_3D ( 'NONE', #51485, #10541, #16206 ) ;
#7388 = DIRECTION ( 'NONE',  ( -1.000000000000000000, -0.000000000000000000, 0.000000000000000000 ) ) ;
#7389 = CARTESIAN_POINT ( 'NONE',  ( 2.406456491625053928, -5.751891873093266661, -8.704497555695612121 ) ) ;
#7390 = EDGE_LOOP ( 'NONE', ( #27137, #43168, #47001, #57148 ) ) ;
#7391 = DIRECTION ( 'NONE',  ( -1.000000000000000000, 0.000000000000000000, 0.000000000000000000 ) ) ;
#7392 = EDGE_LOOP ( 'NONE', ( #45874, #47356, #65473, #6330 ) ) ;
#7393 = CARTESIAN_POINT ( 'NONE',  ( -35.00000000000000000, -4.545979934229492869, 11.30684963584387681 ) ) ;
#7394 = VERTEX_POINT ( 'NONE', #34198 ) ;
#7395 = EDGE_LOOP ( 'NONE', ( #2775, #14574, #1258, #15762 ) ) ;
#7396 = CARTESIAN_POINT ( 'NONE',  ( 37.00000000000000711, -7.718225330433870823, -9.430788938294027091 ) ) ;
#7397 = EDGE_CURVE ( 'NONE', #26297, #7370, #26380, .T. ) ;
#7398 = ORIENTED_EDGE ( 'NONE', *, *, #44516, .T. ) ;
#7399 = FACE_OUTER_BOUND ( 'NONE', #20885, .T. ) ;
#7400 = CARTESIAN_POINT ( 'NONE',  ( 35.00000000000000000, 5.710938531231874116, 11.39945968423464784 ) ) ;
#7401 = CIRCLE ( 'NONE', #53085, 5.000000000000000000 ) ;
#7402 = CARTESIAN_POINT ( 'NONE',  ( 0.000000000000000000, 7.387287142779349836, 1.295372019972174549 ) ) ;
#7403 = FACE_OUTER_BOUND ( 'NONE', #63574, .T. ) ;
#7404 = ORIENTED_EDGE ( 'NONE', *, *, #8010, .F. ) ;
#7405 = FACE_OUTER_BOUND ( 'NONE', #39946, .T. ) ;
#7406 = ADVANCED_FACE ( 'NONE', ( #18622 ), #28895, .T. ) ;
#7408 = B_SPLINE_CURVE_WITH_KNOTS ( 'NONE', 3,
 ( #19689, #14650, #60230, #4055 ),
 .UNSPECIFIED., .F., .F.,
 ( 4, 4 ),
 ( 1.734723475976807094E-18, 0.002404377236383827953 ),
 .UNSPECIFIED. ) ;
#7407 = DIRECTION ( 'NONE',  ( 1.000000000000000000, 0.000000000000000000, 0.000000000000000000 ) ) ;
#7409 = CARTESIAN_POINT ( 'NONE',  ( -22.31328051695926007, -3.685074213229319717, -0.8849444482788241251 ) ) ;
#7411 = ORIENTED_EDGE ( 'NONE', *, *, #57736, .T. ) ;
#7410 = CARTESIAN_POINT ( 'NONE',  ( 35.00000000000000000, -11.95840593935202811, -2.346765782874394635 ) ) ;
#7412 = CARTESIAN_POINT ( 'NONE',  ( -10.00000000000000178, 0.000000000000000000, 0.000000000000000000 ) ) ;
#7413 = EDGE_CURVE ( 'NONE', #56567, #41081, #45744, .T. ) ;
#7414 = ORIENTED_EDGE ( 'NONE', *, *, #64284, .T. ) ;
#7415 = CARTESIAN_POINT ( 'NONE',  ( 35.00000000000000000, -1.039216533672818299, 11.70009620280412399 ) ) ;
#7416 = ORIENTED_EDGE ( 'NONE', *, *, #58570, .T. ) ;
#7417 = CARTESIAN_POINT ( 'NONE',  ( 2.665405856346780400, 2.723742051529458585, 9.171500569027783101 ) ) ;
#7418 = CARTESIAN_POINT ( 'NONE',  ( 0.000000000000000000, -4.472310526050724100, -6.020667617347421618 ) ) ;
#7419 = CARTESIAN_POINT ( 'NONE',  ( 2.000000000000001776, 0.000000000000000000, 0.000000000000000000 ) ) ;
#7420 = VERTEX_POINT ( 'NONE', #33873 ) ;
#7421 = CARTESIAN_POINT ( 'NONE',  ( 1.014383007554947369, 8.367379244277135086, 9.280879504740973118 ) ) ;
#7422 = CARTESIAN_POINT ( 'NONE',  ( 1.719304012339826659, -12.64775761152879596, -1.452142814149639305 ) ) ;
#7423 = CARTESIAN_POINT ( 'NONE',  ( 2.241506898688417682, -5.822995664778295222, 4.937416071751822066 ) ) ;
#7424 = ORIENTED_EDGE ( 'NONE', *, *, #43826, .T. ) ;
#7425 = ORIENTED_EDGE ( 'NONE', *, *, #35653, .T. ) ;
#7426 = DIRECTION ( 'NONE',  ( 0.000000000000000000, -0.7621620551276423461, 0.6473862847818205868 ) ) ;
#7427 = EDGE_LOOP ( 'NONE', ( #59635, #58194, #50398, #41105 ) ) ;
#7428 = ADVANCED_FACE ( 'NONE', ( #49205 ), #29227, .T. ) ;
#7429 = EDGE_CURVE ( 'NONE', #56470, #53254, #17081, .T. ) ;
#7430 = VERTEX_POINT ( 'NONE', #9564 ) ;
#7431 = CARTESIAN_POINT ( 'NONE',  ( -3.740102306720532788, 25.00000000000000000, -6.044082642436763742 ) ) ;
#7432 = CARTESIAN_POINT ( 'NONE',  ( -35.00000000000000000, -6.584150480049623333, 10.25474254703950905 ) ) ;
#7433 = CARTESIAN_POINT ( 'NONE',  ( 36.00000000000000711, -4.400442035670862673, 11.96656215839372983 ) ) ;
#7434 = CARTESIAN_POINT ( 'NONE',  ( 0.9232058338315058954, 6.559496812049661507, 10.60677148422246674 ) ) ;
#7435 = ADVANCED_FACE ( 'NONE', ( #44185 ), #64453, .T. ) ;
#7436 = DIRECTION ( 'NONE',  ( 1.000000000000000000, -0.000000000000000000, -0.000000000000000000 ) ) ;
#7437 = CARTESIAN_POINT ( 'NONE',  ( 0.9232058338315058954, 11.84276737136200452, 3.908895078357559782 ) ) ;
#7438 = VECTOR ( 'NONE', #50087, 1000.000000000000000 ) ;
#7439 = AXIS2_PLACEMENT_3D ( 'NONE', #2900, #21865, #42109 ) ;
#7440 = CARTESIAN_POINT ( 'NONE',  ( -10.00000000000000178, 0.000000000000000000, 0.000000000000000000 ) ) ;
#7441 = EDGE_CURVE ( 'NONE', #22102, #49356, #43819, .T. ) ;
#7442 = ORIENTED_EDGE ( 'NONE', *, *, #59189, .T. ) ;
#7443 = EDGE_CURVE ( 'NONE', #39229, #52589, #56454, .T. ) ;
#7444 = CARTESIAN_POINT ( 'NONE',  ( 35.00000000000000000, 5.273331777780336793, -10.49591321039682690 ) ) ;
#7445 = DIRECTION ( 'NONE',  ( 0.000000000000000000, 0.01356324068817998940, -0.9999080150203990547 ) ) ;
#7446 = CIRCLE ( 'NONE', #44599, 12.00000000000000000 ) ;
#7447 = DIRECTION ( 'NONE',  ( -1.000000000000000000, 0.000000000000000000, 0.000000000000000000 ) ) ;
#7448 = CARTESIAN_POINT ( 'NONE',  ( -35.00000000000000000, -11.05394794832833583, 5.130401251914692651 ) ) ;
#7449 = B_SPLINE_CURVE_WITH_KNOTS ( 'NONE', 3,
 ( #28569, #13594, #33882, #48871, #43871, #18630, #64155, #38889, #59179, #28905, #23933, #18932, #59489, #13915, #10909, #50178, #55481, #61770, #35819, #56818, #9926, #5272 ),
 .UNSPECIFIED., .F., .F.,
 ( 4, 3, 3, 3, 3, 3, 3, 4 ),
 ( 0.000000000000000000, 4.455945684386631000E-05, 6.636307477203665399E-05, 8.816671873158535159E-05, 0.0001099660380492586736, 0.0001317545563165287723, 0.0001762613022895051528, 0.0001867992666138375594 ),
 .UNSPECIFIED. ) ;
#7450 = CIRCLE ( 'NONE', #60528, 12.18649999999999878 ) ;
#7451 = CYLINDRICAL_SURFACE ( 'NONE', #44737, 4.999999999999999112 ) ;
#7452 = CARTESIAN_POINT ( 'NONE',  ( 2.305787727787083519, -3.682701754025559993, 6.711944854845811825 ) ) ;
#7453 = ORIENTED_EDGE ( 'NONE', *, *, #36672, .T. ) ;
#7454 = CARTESIAN_POINT ( 'NONE',  ( -27.01437459610461644, 25.00000000000000000, -2.220455681983952267 ) ) ;
#7455 = DIRECTION ( 'NONE',  ( -1.000000000000000000, 0.000000000000000000, 0.000000000000000000 ) ) ;
#7456 = LINE ( 'NONE', #18465, #19466 ) ;
#7457 = DIRECTION ( 'NONE',  ( 0.000000000000000000, 0.000000000000000000, 1.000000000000000000 ) ) ;
#7458 = CIRCLE ( 'NONE', #30803, 12.74999999999999822 ) ;
#7459 = B_SPLINE_CURVE_WITH_KNOTS ( 'NONE', 3,
 ( #9842, #4556, #29783, #15155, #14490, #56047, #55070, #24824, #14173, #45106, #24481, #65040, #30452, #5198, #40770, #25466 ),
 .UNSPECIFIED., .F., .F.,
 ( 4, 3, 3, 3, 3, 4 ),
 ( 0.000000000000000000, 0.0002176109881719783250, 0.0004352086762393702441, 0.0006528017811445535005, 0.0007615147961450135497, 0.0009453342004945436416 ),
 .UNSPECIFIED. ) ;
#7460 = EDGE_CURVE ( 'NONE', #33098, #55547, #39096, .T. ) ;
#7461 = DIRECTION ( 'NONE',  ( 0.000000000000000000, -0.9551603052523510717, 0.2960891610144409936 ) ) ;
#7462 = CARTESIAN_POINT ( 'NONE',  ( -35.00000000000000000, 11.73808581813437968, -0.4353888892048790038 ) ) ;
#7463 = AXIS2_PLACEMENT_3D ( 'NONE', #6216, #36464, #2467 ) ;
#7464 = EDGE_LOOP ( 'NONE', ( #32008, #40340, #2382, #5885 ) ) ;
#7465 = CARTESIAN_POINT ( 'NONE',  ( 18.12964925673133010, -7.571604912534921183, 9.321062701759899483 ) ) ;
#7466 = CARTESIAN_POINT ( 'NONE',  ( 0.3665391374699464300, -10.76665847464317061, 5.911453292029563933 ) ) ;
#7467 = DIRECTION ( 'NONE',  ( 0.000000000000000000, 0.000000000000000000, -1.000000000000000000 ) ) ;
#7468 = CARTESIAN_POINT ( 'NONE',  ( 2.000000000000001776, 0.000000000000000000, 0.000000000000000000 ) ) ;
#7469 = ORIENTED_EDGE ( 'NONE', *, *, #7755, .T. ) ;
#7470 = CYLINDRICAL_SURFACE ( 'NONE', #38236, 13.50000000000000178 ) ;
#7471 = AXIS2_PLACEMENT_3D ( 'NONE', #16165, #22464, #41760 ) ;
#7472 = CARTESIAN_POINT ( 'NONE',  ( -10.00000000000000178, 0.000000000000000000, 0.000000000000000000 ) ) ;
#7473 = EDGE_LOOP ( 'NONE', ( #23438, #4162, #49592, #38059 ) ) ;
#7474 = ADVANCED_FACE ( 'NONE', ( #56810 ), #31831, .F. ) ;
#7475 = EDGE_LOOP ( 'NONE', ( #50570, #31479, #6509, #40691 ) ) ;
#7476 = CYLINDRICAL_SURFACE ( 'NONE', #6604, 7.499999999999988454 ) ;
#7477 = AXIS2_PLACEMENT_3D ( 'NONE', #47481, #53114, #27187 ) ;
#7478 = CIRCLE ( 'NONE', #16027, 12.75000000000000178 ) ;
#7479 = CARTESIAN_POINT ( 'NONE',  ( 0.2648978790185593790, -4.312320170909161199, -11.46165506714232762 ) ) ;
#7480 = ORIENTED_EDGE ( 'NONE', *, *, #28389, .F. ) ;
#7481 = CYLINDRICAL_SURFACE ( 'NONE', #13232, 12.18650000000000055 ) ;
#7482 = LINE ( 'NONE', #8153, #52729 ) ;
#7483 = DIRECTION ( 'NONE',  ( 0.000000000000000000, -0.6051742151937555825, -0.7960930657056509707 ) ) ;
#7484 = FACE_OUTER_BOUND ( 'NONE', #1323, .T. ) ;
#7485 = CARTESIAN_POINT ( 'NONE',  ( 37.00000000000000711, -12.57916205664482767, -2.080187960898521649 ) ) ;
#7486 = CARTESIAN_POINT ( 'NONE',  ( 0.2759803524722231893, 5.960075719898836333, 10.70204612651777865 ) ) ;
#7488 = EDGE_LOOP ( 'NONE', ( #1491, #17728, #50811, #42667 ) ) ;
#7487 = CARTESIAN_POINT ( 'NONE',  ( 1.000000000000000888, 0.7281529553923131726, -7.464569195442812166 ) ) ;
#7489 = CARTESIAN_POINT ( 'NONE',  ( 2.000000000000001776, 0.000000000000000000, 0.000000000000000000 ) ) ;
#7490 = ADVANCED_FACE ( 'NONE', ( #31190 ), #10899, .F. ) ;
#7491 = VERTEX_POINT ( 'NONE', #283 ) ;
#7492 = DIRECTION ( 'NONE',  ( 0.000000000000000000, 0.000000000000000000, -1.000000000000000000 ) ) ;
#7493 = ORIENTED_EDGE ( 'NONE', *, *, #5054, .F. ) ;
#7494 = EDGE_LOOP ( 'NONE', ( #50657, #58047, #20022, #41351 ) ) ;
#7495 = PRODUCT_CONTEXT ( 'NONE', #57885, 'mechanical' ) ;
#7496 = CARTESIAN_POINT ( 'NONE',  ( -2.952869152607107139, -12.96714474214480717, 3.755417052241487585 ) ) ;
#7497 = VECTOR ( 'NONE', #42389, 1000.000000000000000 ) ;
#7498 = CARTESIAN_POINT ( 'NONE',  ( -22.27718150314433387, 3.596602356343910234, -0.7862703917636566509 ) ) ;
#7499 = CARTESIAN_POINT ( 'NONE',  ( 2.589278595513750503, 1.582391164331769406, 7.587119248534422766 ) ) ;
#7500 = CARTESIAN_POINT ( 'NONE',  ( -30.43939922888039007, -3.192189569316896236, 23.38849890424057065 ) ) ;
#7501 = DIRECTION ( 'NONE',  ( -1.000000000000000000, 0.000000000000000000, 0.000000000000000000 ) ) ;
#7503 = ORIENTED_EDGE ( 'NONE', *, *, #1480, .T. ) ;
#7502 = VECTOR ( 'NONE', #13494, 1000.000000000000000 ) ;
#7504 = VECTOR ( 'NONE', #31319, 1000.000000000000000 ) ;
#7505 = FACE_OUTER_BOUND ( 'NONE', #43251, .T. ) ;
#7506 = DIRECTION ( 'NONE',  ( 0.000000000000000000, 0.01356324068818000328, -0.9999080150203990547 ) ) ;
#7508 = ORIENTED_EDGE ( 'NONE', *, *, #59154, .F. ) ;
#7507 = CARTESIAN_POINT ( 'NONE',  ( 1.194176325881334710, -11.96454551582841042, -3.807610977967044175 ) ) ;
#7509 = ORIENTED_EDGE ( 'NONE', *, *, #14104, .F. ) ;
#7510 = AXIS2_PLACEMENT_3D ( 'NONE', #20713, #56954, #65581 ) ;
#7511 = DIRECTION ( 'NONE',  ( -1.000000000000000000, 0.000000000000000000, 0.000000000000000000 ) ) ;
#7512 = VERTEX_POINT ( 'NONE', #46165 ) ;
#7513 = DIRECTION ( 'NONE',  ( 0.000000000000000000, -0.9651210252299821102, -0.2618041379715529970 ) ) ;
#7514 = DIRECTION ( 'NONE',  ( -1.000000000000000000, 0.000000000000000000, 0.000000000000000000 ) ) ;
#7515 = DIRECTION ( 'NONE',  ( 1.000000000000000000, 0.000000000000000000, 0.000000000000000000 ) ) ;
#7516 = EDGE_CURVE ( 'NONE', #14900, #23975, #57435, .T. ) ;
#7517 = DIRECTION ( 'NONE',  ( 0.000000000000000000, -0.01356324068817998940, 0.9999080150203990547 ) ) ;
#7518 = DIRECTION ( 'NONE',  ( 0.000000000000000000, -0.01356324068817998940, 0.9999080150203990547 ) ) ;
#7519 = CARTESIAN_POINT ( 'NONE',  ( -27.09364415740217780, -1.918701019215943493, 1.303410551736210898 ) ) ;
#7520 = EDGE_CURVE ( 'NONE', #27787, #16234, #15226, .T. ) ;
#7521 = DIRECTION ( 'NONE',  ( 0.000000000000000000, 0.01356324068817992001, -0.9999080150203990547 ) ) ;
#7522 = CIRCLE ( 'NONE', #6490, 7.499999999999988454 ) ;
#7523 = ORIENTED_EDGE ( 'NONE', *, *, #56226, .F. ) ;
#7524 = CYLINDRICAL_SURFACE ( 'NONE', #22090, 7.499999999999988454 ) ;
#7525 = VERTEX_POINT ( 'NONE', #11232 ) ;
#7526 = EDGE_CURVE ( 'NONE', #725, #53268, #2237, .T. ) ;
#7527 = CIRCLE ( 'NONE', #62775, 12.74999999999999822 ) ;
#7528 = DIRECTION ( 'NONE',  ( 0.000000000000000000, -1.000000000000000000, 0.000000000000000000 ) ) ;
#7529 = CYLINDRICAL_SURFACE ( 'NONE', #18978, 4.999999999999999112 ) ;
#7530 = CARTESIAN_POINT ( 'NONE',  ( 36.00000000000000711, -7.882940143791699050, 10.02106554660717030 ) ) ;
#7531 = CARTESIAN_POINT ( 'NONE',  ( -35.00000000000000000, -11.73808581813438323, 0.4353888892047964587 ) ) ;
#7532 = VERTEX_POINT ( 'NONE', #20217 ) ;
#7533 = AXIS2_PLACEMENT_3D ( 'NONE', #64959, #23100, #64312 ) ;
#7534 = ORIENTED_EDGE ( 'NONE', *, *, #57543, .T. ) ;
#7535 = AXIS2_PLACEMENT_3D ( 'NONE', #61705, #62053, #36772 ) ;
#7536 = CARTESIAN_POINT ( 'NONE',  ( 2.889800649504073782, 3.986129653162709285, -4.645655809191325147 ) ) ;
#7537 = ORIENTED_EDGE ( 'NONE', *, *, #16997, .F. ) ;
#7538 = CIRCLE ( 'NONE', #15874, 5.000000000000001776 ) ;
#7539 = CYLINDRICAL_SURFACE ( 'NONE', #33021, 2.999999999999995559 ) ;
#7540 = CARTESIAN_POINT ( 'NONE',  ( -28.56473390530002021, 3.589939350442142185, -11.45074047018220753 ) ) ;
#7541 = DIRECTION ( 'NONE',  ( 0.000000000000000000, -0.9847383929261636082, 0.1740410799127514174 ) ) ;
#7542 = CARTESIAN_POINT ( 'NONE',  ( -37.00000000000000711, -8.389074212634351824, 8.839356091080015076 ) ) ;
#7543 = VERTEX_POINT ( 'NONE', #51804 ) ;
#7544 = CARTESIAN_POINT ( 'NONE',  ( 0.2653519890518161728, -6.123106317427082779, -10.60551359205156707 ) ) ;
#7545 = CARTESIAN_POINT ( 'NONE',  ( -22.29018399051993882, -2.585196332786384055, 2.675685774027739328 ) ) ;
#7546 = CARTESIAN_POINT ( 'NONE',  ( 2.798553295784531159, 25.00000000000000000, 7.462808788758677814 ) ) ;
#7547 = CYLINDRICAL_SURFACE ( 'NONE', #64638, 13.50000000000000178 ) ;
#7548 = AXIS2_PLACEMENT_3D ( 'NONE', #20839, #1226, #6214 ) ;
#7549 = CIRCLE ( 'NONE', #32976, 12.75000000000000178 ) ;
#7550 = PRODUCT_DEFINITION ( 'UNKNOWN', '', #27136, #32561 ) ;
#7551 = EDGE_CURVE ( 'NONE', #27477, #29748, #20558, .T. ) ;
#7552 = CIRCLE ( 'NONE', #35160, 2.899999999999994582 ) ;
#7553 = DIRECTION ( 'NONE',  ( 0.000000000000000000, 0.000000000000000000, -1.000000000000000000 ) ) ;
#7554 = ADVANCED_FACE ( 'NONE', ( #62103 ), #25531, .T. ) ;
#7555 = DIRECTION ( 'NONE',  ( -1.000000000000000000, 0.000000000000000000, 0.000000000000000000 ) ) ;
#7556 =( BOUNDED_SURFACE ( )  B_SPLINE_SURFACE ( 3, 1, ( 
 ( #4405, #64889 ),
 ( #40615, #60908 ),
 ( #30623, #15348 ),
 ( #30318, #5378 ) ),
 .UNSPECIFIED., .F., .F., .F. ) 
 B_SPLINE_SURFACE_WITH_KNOTS ( ( 4, 4 ),
 ( 2, 2 ),
 ( 0.000000000000000000, 1.000000000000000000 ),
 ( 0.000000000000000000, 1.000000000000000000 ),
 .UNSPECIFIED. ) 
 GEOMETRIC_REPRESENTATION_ITEM ( )  RATIONAL_B_SPLINE_SURFACE ( (
 ( 1.000000000000000000, 1.000000000000000000),
 ( 0.9942764183789327692, 0.8450855930916580938),
 ( 0.9942764183789327692, 0.8450855930916580938),
 ( 1.000000000000000000, 1.000000000000000000) ) ) 
 REPRESENTATION_ITEM ( '' )  SURFACE ( )  );
#7557 = VERTEX_POINT ( 'NONE', #45479 ) ;
#7558 = CARTESIAN_POINT ( 'NONE',  ( -35.04643116707788408, 0.01156612771643569793, 0.003844232202706091006 ) ) ;
#7559 = CARTESIAN_POINT ( 'NONE',  ( 29.51976981715666781, 7.690765383426390045, 11.09513982864076276 ) ) ;
#7560 = CIRCLE ( 'NONE', #11775, 12.74999999999999822 ) ;
#7561 = CARTESIAN_POINT ( 'NONE',  ( -36.00000000000000711, -12.46157735505191333, 2.696588552979013009 ) ) ;
#7562 = ORIENTED_EDGE ( 'NONE', *, *, #21431, .T. ) ;
#7563 = FACE_OUTER_BOUND ( 'NONE', #18649, .T. ) ;
#7564 = CARTESIAN_POINT ( 'NONE',  ( -35.00000000000000000, 0.000000000000000000, 0.000000000000000000 ) ) ;
#7565 = DIRECTION ( 'NONE',  ( 0.000000000000000000, 0.000000000000000000, 1.000000000000000000 ) ) ;
#7566 = AXIS2_PLACEMENT_3D ( 'NONE', #32129, #62383, #51476 ) ;
#7567 = EDGE_CURVE ( 'NONE', #33417, #59719, #35508, .T. ) ;
#7568 = CARTESIAN_POINT ( 'NONE',  ( -29.95711186975066198, 0.8286516086034492190, -13.48164454051215877 ) ) ;
#7569 = CARTESIAN_POINT ( 'NONE',  ( 0.2657645697724703715, -11.55867655367624280, 4.045961170622970116 ) ) ;
#7570 = VERTEX_POINT ( 'NONE', #58100 ) ;
#7571 = ORIENTED_EDGE ( 'NONE', *, *, #44421, .F. ) ;
#7572 = CARTESIAN_POINT ( 'NONE',  ( 3.152665057734040488, 0.000000000000000000, 0.000000000000000000 ) ) ;
#7573 = ORIENTED_EDGE ( 'NONE', *, *, #36863, .F. ) ;
#7574 = CIRCLE ( 'NONE', #51228, 2.899999999999995914 ) ;
#7575 = DIRECTION ( 'NONE',  ( -1.000000000000000000, 0.000000000000000000, 0.000000000000000000 ) ) ;
#7576 = CARTESIAN_POINT ( 'NONE',  ( -35.00000000000000000, 0.000000000000000000, 0.000000000000000000 ) ) ;
#7577 = DIRECTION ( 'NONE',  ( 1.000000000000000000, 0.000000000000000000, 0.000000000000000000 ) ) ;
#7578 =( BOUNDED_CURVE ( )  B_SPLINE_CURVE ( 3, ( #62018, #21452, #6824, #26765 ),
 .UNSPECIFIED., .F., .F. ) 
 B_SPLINE_CURVE_WITH_KNOTS ( ( 4, 4 ),
 ( 1.570796326794895892, 1.612255705401422601 ),
 .UNSPECIFIED. ) 
 CURVE ( )  GEOMETRIC_REPRESENTATION_ITEM ( )  RATIONAL_B_SPLINE_CURVE ( ( 1.000000000000000000, 0.9998567651231480280, 0.9998567651231480280, 1.000000000000000000 ) ) 
 REPRESENTATION_ITEM ( '' )  );
#7579 = CARTESIAN_POINT ( 'NONE',  ( -16.00005080000000035, 0.000000000000000000, 0.000000000000000000 ) ) ;
#7580 = CARTESIAN_POINT ( 'NONE',  ( 0.6511581176968144202, -7.698038847496639470, -9.688955459274998461 ) ) ;
#7581 = CARTESIAN_POINT ( 'NONE',  ( 2.298277635560815657, 5.755367168478065842, 5.044791616847147608 ) ) ;
#7582 = DIRECTION ( 'NONE',  ( 0.000000000000000000, 0.7381862504171974315, -0.6745969609292639113 ) ) ;
#7583 = ORIENTED_EDGE ( 'NONE', *, *, #8335, .F. ) ;
#7584 = CIRCLE ( 'NONE', #52226, 12.73084802173761787 ) ;
#7585 = EDGE_CURVE ( 'NONE', #20717, #40151, #37241, .T. ) ;
#7586 = EDGE_CURVE ( 'NONE', #9622, #21959, #12513, .T. ) ;
#7587 = ORIENTED_EDGE ( 'NONE', *, *, #40675, .T. ) ;
#7588 = DIRECTION ( 'NONE',  ( 1.000000000000000000, 0.000000000000000000, 0.000000000000000000 ) ) ;
#7589 = ORIENTED_EDGE ( 'NONE', *, *, #39255, .T. ) ;
#7590 = ADVANCED_FACE ( 'NONE', ( #32792 ), #58773, .T. ) ;
#7591 = DIRECTION ( 'NONE',  ( -1.000000000000000000, -0.000000000000000000, -0.000000000000000000 ) ) ;
#7593 = CARTESIAN_POINT ( 'NONE',  ( 1.462291587751940014, 8.602888600422827992, -9.267729738231986758 ) ) ;
#7592 = CIRCLE ( 'NONE', #41567, 5.000000000000000888 ) ;
#7594 = AXIS2_PLACEMENT_3D ( 'NONE', #59090, #54427, #44404 ) ;
#7595 = CARTESIAN_POINT ( 'NONE',  ( 37.00000000000000711, -1.591260454995155671, 12.08216339958901742 ) ) ;
#7596 = ORIENTED_EDGE ( 'NONE', *, *, #31727, .F. ) ;
#7597 = CARTESIAN_POINT ( 'NONE',  ( -37.00000000000000711, 0.000000000000000000, 0.000000000000000000 ) ) ;
#7598 = CARTESIAN_POINT ( 'NONE',  ( 1.937114397841935398, -12.33981801388255306, -3.531416430611418633 ) ) ;
#7599 = DIRECTION ( 'NONE',  ( 0.000000000000000000, 0.07632122047555796318, -0.9970832820307042876 ) ) ;
#7600 = ORIENTED_EDGE ( 'NONE', *, *, #43212, .T. ) ;
#7601 = ORIENTED_EDGE ( 'NONE', *, *, #20965, .T. ) ;
#7602 = DIRECTION ( 'NONE',  ( 0.000000000000000000, 0.01356324068817998940, -0.9999080150203990547 ) ) ;
#7603 = ORIENTED_EDGE ( 'NONE', *, *, #35830, .F. ) ;
#7604 = CARTESIAN_POINT ( 'NONE',  ( 2.266490820343224577, 3.946561086901473558, 6.544980046121041006 ) ) ;
#7605 = ORIENTED_EDGE ( 'NONE', *, *, #44065, .F. ) ;
#7606 = ORIENTED_EDGE ( 'NONE', *, *, #13868, .T. ) ;
#7607 = VECTOR ( 'NONE', #26814, 1000.000000000000000 ) ;
#7608 = CARTESIAN_POINT ( 'NONE',  ( -22.27722019094931127, -2.813874087060002527, 2.374181302998998877 ) ) ;
#7609 = EDGE_CURVE ( 'NONE', #5162, #6270, #27214, .T. ) ;
#7610 = CARTESIAN_POINT ( 'NONE',  ( 2.305787727787083519, 5.047606869483132641, -5.756228004061408221 ) ) ;
#7611 = CIRCLE ( 'NONE', #13946, 12.18650000000000055 ) ;
#7612 = B_SPLINE_CURVE_WITH_KNOTS ( 'NONE', 3,
 ( #3581, #63392, #22529, #7898, #13822, #23172, #48141, #18847, #7545, #12519, #8212, #63716, #64377, #38466, #33486, #17860, #54090, #8523, #53452, #53775, #2599, #2912 ),
 .UNSPECIFIED., .F., .F.,
 ( 4, 3, 3, 3, 3, 3, 3, 4 ),
 ( 0.000000000000000000, 4.455945684386370791E-05, 6.636307477203548847E-05, 8.816671873158297989E-05, 0.0001099660380492561800, 0.0001317545563165253299, 0.0001762613022894969942, 0.0001867992666138382099 ),
 .UNSPECIFIED. ) ;
#7613 = CARTESIAN_POINT ( 'NONE',  ( 12.93723047338301058, 4.476360154859203355, 25.00000000000000000 ) ) ;
#7614 = CARTESIAN_POINT ( 'NONE',  ( 0.3537226245948361103, 8.088784578751420540, -9.233810598191700691 ) ) ;
#7615 = CARTESIAN_POINT ( 'NONE',  ( 0.2646305136544072623, -1.996350543472915184, -12.08286001766537687 ) ) ;
#7616 = CIRCLE ( 'NONE', #38403, 5.000000000000000888 ) ;
#7617 = ADVANCED_FACE ( 'NONE', ( #42436 ), #17538, .T. ) ;
#7618 = DIRECTION ( 'NONE',  ( 0.000000000000000000, 0.000000000000000000, 1.000000000000000000 ) ) ;
#7619 = ORIENTED_EDGE ( 'NONE', *, *, #55231, .T. ) ;
#7620 = DIRECTION ( 'NONE',  ( -1.000000000000000000, -0.000000000000000000, 0.000000000000000000 ) ) ;
#7621 = CARTESIAN_POINT ( 'NONE',  ( 2.000000000000001776, -1.956810415765137368, -6.654767106875568494 ) ) ;
#7622 = VECTOR ( 'NONE', #28432, 1000.000000000000000 ) ;
#7623 = DIRECTION ( 'NONE',  ( 0.000000000000000000, -0.01356324068817992175, 0.9999080150203990547 ) ) ;
#7624 = DIRECTION ( 'NONE',  ( 0.000000000000000000, 0.6478160128811893959, -0.7617968321374923857 ) ) ;
#7625 = CARTESIAN_POINT ( 'NONE',  ( -35.00000000000000000, -9.390600770287930388, -8.624332853796161658 ) ) ;
#7626 = CARTESIAN_POINT ( 'NONE',  ( 35.00000000000000000, -11.02904044024205987, 4.041347439435972966 ) ) ;
#7627 = CIRCLE ( 'NONE', #51161, 12.18649999999999878 ) ;
#7628 = CARTESIAN_POINT ( 'NONE',  ( 2.589278595513451631, -4.081908913131900185, -6.588350318048493470 ) ) ;
#7629 = DIRECTION ( 'NONE',  ( 0.000000000000000000, -0.01356324068817991828, 0.9999080150203990547 ) ) ;
#7630 = CARTESIAN_POINT ( 'NONE',  ( 0.9296196016818686347, 5.870433615767222335, 10.99907063288793729 ) ) ;
#7631 = ORIENTED_EDGE ( 'NONE', *, *, #65309, .T. ) ;
#7632 = LINE ( 'NONE', #27917, #39684 ) ;
#7633 = CIRCLE ( 'NONE', #6594, 1.500000000000000222 ) ;
#7634 = ORIENTED_EDGE ( 'NONE', *, *, #57033, .T. ) ;
#7635 = CARTESIAN_POINT ( 'NONE',  ( -11.08072612429806014, -9.571970673523852113, 7.260798853501513328 ) ) ;
#7636 = CARTESIAN_POINT ( 'NONE',  ( 2.247206125382827935, 5.923516414428655175, -4.819320926502576263 ) ) ;
#7637 = FACE_OUTER_BOUND ( 'NONE', #55001, .T. ) ;
#7638 = CARTESIAN_POINT ( 'NONE',  ( 0.2653141617321012058, 9.352766656400060441, 7.905395731875527687 ) ) ;
#7639 = CARTESIAN_POINT ( 'NONE',  ( -35.00000000000000000, 7.110831038798278492, 9.896810808925417646 ) ) ;
#7640 = ORIENTED_EDGE ( 'NONE', *, *, #24222, .F. ) ;
#7641 = DIRECTION ( 'NONE',  ( 0.000000000000000000, -0.01356324068817999114, 0.9999080150203989437 ) ) ;
#7642 = CARTESIAN_POINT ( 'NONE',  ( 37.00000000000000711, 12.54989509947654192, 2.250029553613615452 ) ) ;
#7643 = CARTESIAN_POINT ( 'NONE',  ( -27.10128162969832744, 2.102429195189572830, 1.032914450114625016 ) ) ;
#7644 = CARTESIAN_POINT ( 'NONE',  ( 0.2650492594609232255, -2.017987075343877557, -12.07870403910583690 ) ) ;
#7645 = VECTOR ( 'NONE', #42379, 1000.000000000000000 ) ;
#7646 = CIRCLE ( 'NONE', #12956, 12.18649999999999878 ) ;
#7647 = AXIS2_PLACEMENT_3D ( 'NONE', #43966, #22352, #13687 ) ;
#7648 = ADVANCED_FACE ( 'NONE', ( #37138 ), #7539, .T. ) ;
#7649 = DIRECTION ( 'NONE',  ( -1.000000000000000000, 0.000000000000000000, 0.000000000000000000 ) ) ;
#7650 = ORIENTED_EDGE ( 'NONE', *, *, #60671, .T. ) ;
#7651 = CARTESIAN_POINT ( 'NONE',  ( 5.514970785353741078, 0.001326349372336295580, -0.004532877335078716770 ) ) ;
#7652 = CARTESIAN_POINT ( 'NONE',  ( 1.372161826076671254, -8.551811013234788206, -9.274145586376244310 ) ) ;
#7653 = CARTESIAN_POINT ( 'NONE',  ( 4.308196110052892319E-12, -30.53649492335491189, 15.30974548841782656 ) ) ;
#7654 = VECTOR ( 'NONE', #37176, 1000.000000000000000 ) ;
#7655 = AXIS2_PLACEMENT_3D ( 'NONE', #4961, #25223, #45497 ) ;
#7656 = EDGE_CURVE ( 'NONE', #33192, #19282, #59573, .T. ) ;
#7657 = VERTEX_POINT ( 'NONE', #27176 ) ;
#7659 = FACE_OUTER_BOUND ( 'NONE', #29655, .T. ) ;
#7658 = AXIS2_PLACEMENT_3D ( 'NONE', #36980, #15401, #20727 ) ;
#7660 = ORIENTED_EDGE ( 'NONE', *, *, #44038, .F. ) ;
#7661 = CARTESIAN_POINT ( 'NONE',  ( 2.241352910868909643, -6.569501556381469598, 3.889181972941426313 ) ) ;
#7662 = CYLINDRICAL_SURFACE ( 'NONE', #50193, 6.936499999999988120 ) ;
#7663 = CARTESIAN_POINT ( 'NONE',  ( -27.10512513516273359, -1.709353012332570643, -1.618446180705552573 ) ) ;
#7664 = DIRECTION ( 'NONE',  ( -1.000000000000000000, -0.000000000000000000, 0.000000000000000000 ) ) ;
#7665 = CIRCLE ( 'NONE', #17203, 12.74999999999999822 ) ;
#7666 = CARTESIAN_POINT ( 'NONE',  ( 37.00000000000000711, 9.390600770288115129, 8.624332853795948495 ) ) ;
#7667 = EDGE_LOOP ( 'NONE', ( #61627, #2129, #12260, #60180 ) ) ;
#7668 = EDGE_CURVE ( 'NONE', #53854, #22894, #39376, .T. ) ;
#7669 = AXIS2_PLACEMENT_3D ( 'NONE', #43852, #64136, #18614 ) ;
#7670 = EDGE_LOOP ( 'NONE', ( #2380, #10607, #41145, #50326 ) ) ;
#7671 = ORIENTED_EDGE ( 'NONE', *, *, #55042, .T. ) ;
#7672 = CARTESIAN_POINT ( 'NONE',  ( 2.242819959140645913, 7.208832857235912606, -2.514828506624997573 ) ) ;
#7673 = DIRECTION ( 'NONE',  ( 0.000000000000000000, 0.01356324068817998940, -0.9999080150203990547 ) ) ;
#7674 = ORIENTED_EDGE ( 'NONE', *, *, #49298, .T. ) ;
#7675 = B_SPLINE_CURVE_WITH_KNOTS ( 'NONE', 3,
 ( #58496, #12578, #49506, #32860, #34179, #3946, #38524, #8921, #58845, #27901, #48208, #2661, #22921, #63451, #17921, #34510, #34812, #4925, #14856, #65728, #30810, #40820 ),
 .UNSPECIFIED., .F., .F.,
 ( 4, 3, 3, 3, 3, 3, 3, 4 ),
 ( 3.150255712925088731E-18, 4.449119708436434972E-05, 6.626296329539814380E-05, 8.803456484962096553E-05, 0.0001098060367612739010, 0.0001315774408628451900, 0.0001760698110411101100, 0.0001829697163287813692 ),
 .UNSPECIFIED. ) ;
#7676 = CARTESIAN_POINT ( 'NONE',  ( 0.000000000000000000, 0.000000000000000000, 0.000000000000000000 ) ) ;
#7677 = CARTESIAN_POINT ( 'NONE',  ( -22.29115169517546136, -0.2790989024812826069, -3.712980101756741202 ) ) ;
#7678 = ORIENTED_EDGE ( 'NONE', *, *, #12198, .F. ) ;
#7679 = LINE ( 'NONE', #27964, #8854 ) ;
#7680 = CARTESIAN_POINT ( 'NONE',  ( 2.259025283528087513, -2.741148848567716456, -7.131631878998416774 ) ) ;
#7681 = CARTESIAN_POINT ( 'NONE',  ( 36.00000000000000711, 8.830544224263075392, 9.196955404009196755 ) ) ;
#7682 = VERTEX_POINT ( 'NONE', #2590 ) ;
#7683 = ORIENTED_EDGE ( 'NONE', *, *, #55574, .T. ) ;
#7684 = CARTESIAN_POINT ( 'NONE',  ( 37.00000000000000711, 4.426194442447407340, 11.35427606708800852 ) ) ;
#7685 = ORIENTED_EDGE ( 'NONE', *, *, #49636, .T. ) ;
#7686 = DIRECTION ( 'NONE',  ( -1.000000000000000000, 0.000000000000000000, 0.000000000000000000 ) ) ;
#7687 = ORIENTED_EDGE ( 'NONE', *, *, #13163, .T. ) ;
#7688 = AXIS2_PLACEMENT_3D ( 'NONE', #48411, #18137, #2862 ) ;
#7689 = CARTESIAN_POINT ( 'NONE',  ( 0.2638984909335716500, 0.1991813963115696973, -12.24571285024408951 ) ) ;
#7690 = CARTESIAN_POINT ( 'NONE',  ( 4.340384785879546570, -31.41030204081753752, -14.02840248442898208 ) ) ;
#7691 = EDGE_CURVE ( 'NONE', #11726, #49219, #56376, .T. ) ;
#7692 = CARTESIAN_POINT ( 'NONE',  ( 2.000000000000001776, 7.493043167941616289, 0.3229614270519615693 ) ) ;
#7693 = AXIS2_PLACEMENT_3D ( 'NONE', #25885, #64775, #9252 ) ;
#7695 = AXIS2_PLACEMENT_3D ( 'NONE', #2846, #2521, #22792 ) ;
#7694 = CARTESIAN_POINT ( 'NONE',  ( 37.00000000000000711, -12.42372387097884001, -2.865935305911582631 ) ) ;
#7696 = DIRECTION ( 'NONE',  ( 0.000000000000000000, 0.000000000000000000, 1.000000000000000000 ) ) ;
#7697 = DIRECTION ( 'NONE',  ( 0.000000000000000000, -1.000000000000000000, 0.000000000000000000 ) ) ;
#7698 = CARTESIAN_POINT ( 'NONE',  ( -27.39679304536733540, -9.459809594864578841, -7.405314960163760674 ) ) ;
#7699 = ORIENTED_EDGE ( 'NONE', *, *, #6051, .F. ) ;
#7700 = DIRECTION ( 'NONE',  ( 0.000000000000000000, -0.01356324068817992175, 0.9999080150203990547 ) ) ;
#7701 = VERTEX_POINT ( 'NONE', #38117 ) ;
#7702 = CARTESIAN_POINT ( 'NONE',  ( 2.247206125382826603, -2.720255231377985083, 7.135412558555544571 ) ) ;
#7703 = CARTESIAN_POINT ( 'NONE',  ( 2.280717697722503878, 6.699799459370877841, 3.687451363406097027 ) ) ;
#7704 = ORIENTED_EDGE ( 'NONE', *, *, #16779, .T. ) ;
#7705 = CARTESIAN_POINT ( 'NONE',  ( -16.35697571030837594, 8.282848916715964904, 8.683172938416127806 ) ) ;
#7706 = CARTESIAN_POINT ( 'NONE',  ( -37.00000000000000711, -2.220215194441820916, -11.98254675519230616 ) ) ;
#7707 = CARTESIAN_POINT ( 'NONE',  ( 35.00000000000000000, 0.2661492558803343345, -12.18359334611896649 ) ) ;
#7708 = CIRCLE ( 'NONE', #44855, 5.000000000000000888 ) ;
#7710 = ADVANCED_FACE ( 'NONE', ( #32146 ), #1601, .T. ) ;
#7709 = ORIENTED_EDGE ( 'NONE', *, *, #34292, .F. ) ;
#7711 = CIRCLE ( 'NONE', #31044, 2.899999999999994582 ) ;
#7712 = ORIENTED_EDGE ( 'NONE', *, *, #20674, .T. ) ;
#7713 = CARTESIAN_POINT ( 'NONE',  ( 2.941278708680199916, -0.1348063076486517853, -6.138172921908582325 ) ) ;
#7714 = AXIS2_PLACEMENT_3D ( 'NONE', #20678, #36619, #47274 ) ;
#7715 = VERTEX_POINT ( 'NONE', #17200 ) ;
#7716 = CARTESIAN_POINT ( 'NONE',  ( 145.1370849898475797, 3.309064568108273190E-14, 0.000000000000000000 ) ) ;
#7717 = VECTOR ( 'NONE', #44461, 1000.000000000000000 ) ;
#7718 = DIRECTION ( 'NONE',  ( 0.000000000000000000, 0.01356324068817998940, -0.9999080150203990547 ) ) ;
#7719 = DIRECTION ( 'NONE',  ( -0.3162277663656185012, 0.1673616205762862574, 0.9338040949457712125 ) ) ;
#7720 = CARTESIAN_POINT ( 'NONE',  ( -7.489022030332961322, 5.127957880411581293, -10.84914964302385521 ) ) ;
#7721 = EDGE_LOOP ( 'NONE', ( #42562, #63249, #65247, #14991 ) ) ;
#7722 = CARTESIAN_POINT ( 'NONE',  ( 0.2833330754217379677, -12.02930703389099598, -2.326361469893360567 ) ) ;
#7723 = AXIS2_PLACEMENT_3D ( 'NONE', #31054, #1129, #10430 ) ;
#7724 = ADVANCED_FACE ( 'NONE', ( #57784 ), #3228, .T. ) ;
#7725 = CARTESIAN_POINT ( 'NONE',  ( 5.029029651858271777, -26.84634345473923034, -15.78007771861069486 ) ) ;
#7726 = CARTESIAN_POINT ( 'NONE',  ( 21.97889514767880925, 13.29909890247968285, -2.348602380154369396 ) ) ;
#7727 = CARTESIAN_POINT ( 'NONE',  ( 0.2638984909335720941, -1.930290337334137130, 12.09426044257623722 ) ) ;
#7728 = EDGE_CURVE ( 'NONE', #35757, #23816, #36751, .T. ) ;
#7729 = FACE_OUTER_BOUND ( 'NONE', #21, .T. ) ;
#7730 = FACE_OUTER_BOUND ( 'NONE', #14226, .T. ) ;
#7731 = CARTESIAN_POINT ( 'NONE',  ( 2.899286259009695943, 5.316140236670850783, -5.780956296532465011 ) ) ;
#7732 = VECTOR ( 'NONE', #35998, 1000.000000000000000 ) ;
#7733 = AXIS2_PLACEMENT_3D ( 'NONE', #402, #20331, #25323 ) ;
#7734 = B_SPLINE_CURVE_WITH_KNOTS ( 'NONE', 3,
 ( #58650, #9061, #53320, #4078, #63934, #23723 ),
 .UNSPECIFIED., .F., .F.,
 ( 4, 2, 4 ),
 ( 0.005173693434891112747, 0.006312000079627475523, 0.007450306724363838298 ),
 .UNSPECIFIED. ) ;
#7735 = AXIS2_PLACEMENT_3D ( 'NONE', #5869, #47401, #51073 ) ;
#7736 = AXIS2_PLACEMENT_3D ( 'NONE', #56570, #25001, #65532 ) ;
#7737 = ADVANCED_FACE ( 'NONE', ( #54750 ), #64371, .T. ) ;
#7738 = EDGE_LOOP ( 'NONE', ( #13398, #1922, #21836, #58608 ) ) ;
#7739 = CARTESIAN_POINT ( 'NONE',  ( 2.284126774967660811, -0.1584898568958421905, 7.647017279602163597 ) ) ;
#7740 = VERTEX_POINT ( 'NONE', #23500 ) ;
#7741 = CYLINDRICAL_SURFACE ( 'NONE', #34222, 12.18649999999999878 ) ;
#7742 = CARTESIAN_POINT ( 'NONE',  ( -22.28023996335807411, 3.676538434326163785, -0.3233044107360694697 ) ) ;
#7743 = CARTESIAN_POINT ( 'NONE',  ( 32.00000000000000000, -11.99999999999997513, 0.000000000000000000 ) ) ;
#7744 = VERTEX_POINT ( 'NONE', #8205 ) ;
#7745 = CARTESIAN_POINT ( 'NONE',  ( 2.262775599887391742, 6.546038779271709629, 3.942403752833328223 ) ) ;
#7746 = ORIENTED_EDGE ( 'NONE', *, *, #62517, .F. ) ;
#7747 = CIRCLE ( 'NONE', #19431, 6.936499999999989008 ) ;
#7748 = DIRECTION ( 'NONE',  ( -1.000000000000000000, 0.000000000000000000, 0.000000000000000000 ) ) ;
#7749 = VERTEX_POINT ( 'NONE', #43777 ) ;
#7750 = ORIENTED_EDGE ( 'NONE', *, *, #15493, .T. ) ;
#7751 = CARTESIAN_POINT ( 'NONE',  ( 0.2648978790185584908, -7.769924372105139199, -9.465406350830686932 ) ) ;
#7752 = AXIS2_PLACEMENT_3D ( 'NONE', #6043, #7004, #62510 ) ;
#7753 = CARTESIAN_POINT ( 'NONE',  ( -22.27945548916780183, -3.346394890313974191, -1.551028078364850460 ) ) ;
#7754 = ORIENTED_EDGE ( 'NONE', *, *, #19383, .F. ) ;
#7755 = EDGE_CURVE ( 'NONE', #57555, #54366, #20026, .T. ) ;
#7756 = DIRECTION ( 'NONE',  ( 0.000000000000000000, -0.9635499925192253512, 0.2675283385292119842 ) ) ;
#7757 = CARTESIAN_POINT ( 'NONE',  ( 2.350038591458511128, 10.60256821300654018, 0.6402934222728309255 ) ) ;
#7758 = CYLINDRICAL_SURFACE ( 'NONE', #6816, 13.50000000000000178 ) ;
#7759 = DIRECTION ( 'NONE',  ( 0.000000000000000000, -0.8369827122275287357, -0.5472293298355360713 ) ) ;
#7760 = EDGE_LOOP ( 'NONE', ( #40395, #54620, #17923, #51750 ) ) ;
#7761 = DIRECTION ( 'NONE',  ( 0.000000000000000000, 0.000000000000000000, 1.000000000000000000 ) ) ;
#7762 = AXIS2_PLACEMENT_3D ( 'NONE', #32448, #28783, #3549 ) ;
#7763 = CARTESIAN_POINT ( 'NONE',  ( 12.80904563207495350, -29.07871018746164538, 3.648338481107272546 ) ) ;
#7764 = CARTESIAN_POINT ( 'NONE',  ( 2.241352910868908310, -1.407733736974815963, -7.503490710578247125 ) ) ;
#7766 = VERTEX_POINT ( 'NONE', #14474 ) ;
#7765 = FACE_OUTER_BOUND ( 'NONE', #7760, .T. ) ;
#7767 = CARTESIAN_POINT ( 'NONE',  ( -22.30625920655495165, -3.687109008463848703, -0.8854385781085442053 ) ) ;
#7768 = ORIENTED_EDGE ( 'NONE', *, *, #54154, .F. ) ;
#7769 = CARTESIAN_POINT ( 'NONE',  ( -17.61945576107935452, 13.14228823968358384, 3.170957093146434147 ) ) ;
#7770 = ORIENTED_EDGE ( 'NONE', *, *, #16135, .T. ) ;
#7771 = DIRECTION ( 'NONE',  ( -1.000000000000000000, -0.000000000000000000, -0.000000000000000000 ) ) ;
#7772 = DIRECTION ( 'NONE',  ( 0.000000000000000000, -0.01356324068817999114, 0.9999080150203989437 ) ) ;
#7773 = CYLINDRICAL_SURFACE ( 'NONE', #47835, 12.18650000000000055 ) ;
#7774 = CARTESIAN_POINT ( 'NONE',  ( 0.2647959493198558945, -4.049980114636448469, 11.55693259385004978 ) ) ;
#7775 = CIRCLE ( 'NONE', #5703, 5.000000000000000000 ) ;
#7776 = CARTESIAN_POINT ( 'NONE',  ( 0.2647959493198558945, 9.474789498086993333, 7.758440170207198783 ) ) ;
#7777 = CYLINDRICAL_SURFACE ( 'NONE', #48442, 4.999999999999999112 ) ;
#7778 = CARTESIAN_POINT ( 'NONE',  ( -22.28073302975500880, -3.572053042948119206, -0.9342220484185019824 ) ) ;
#7779 =( BOUNDED_SURFACE ( )  B_SPLINE_SURFACE ( 3, 1, ( 
 ( #48894, #43891 ),
 ( #27948, #53563 ),
 ( #28589, #37913 ),
 ( #33592, #62854 ) ),
 .UNSPECIFIED., .F., .F., .F. ) 
 B_SPLINE_SURFACE_WITH_KNOTS ( ( 4, 4 ),
 ( 2, 2 ),
 ( 0.000000000000000000, 1.000000000000000000 ),
 ( 0.000000000000000000, 1.000000000000000000 ),
 .UNSPECIFIED. ) 
 GEOMETRIC_REPRESENTATION_ITEM ( )  RATIONAL_B_SPLINE_SURFACE ( (
 ( 1.000000000000000000, 1.000000000000000000),
 ( 0.9932032654565553509, 0.8386279382598736953),
 ( 0.9932032654565553509, 0.8386279382598736953),
 ( 1.000000000000000000, 1.000000000000000000) ) ) 
 REPRESENTATION_ITEM ( '' )  SURFACE ( )  );
#7780 = ORIENTED_EDGE ( 'NONE', *, *, #33540, .F. ) ;
#7781 = DIRECTION ( 'NONE',  ( 1.000000000000000000, 0.000000000000000000, 0.000000000000000000 ) ) ;
#7782 = ORIENTED_EDGE ( 'NONE', *, *, #37005, .T. ) ;
#7783 = AXIS2_PLACEMENT_3D ( 'NONE', #27276, #28588, #22633 ) ;
#7784 = VERTEX_POINT ( 'NONE', #28807 ) ;
#7786 = CIRCLE ( 'NONE', #37484, 22.50555349946515449 ) ;
#7785 = CARTESIAN_POINT ( 'NONE',  ( 18.98898312442693737, -6.102278294184944940, 12.04338967756598500 ) ) ;
#7787 = CARTESIAN_POINT ( 'NONE',  ( -22.29479313954897890, 3.360948587163232304, 1.627767898183716921 ) ) ;
#7788 = CARTESIAN_POINT ( 'NONE',  ( 35.00000000000000000, -10.28547182238011715, -5.672855678558653914 ) ) ;
#7789 = DIRECTION ( 'NONE',  ( -1.000000000000000000, 0.000000000000000000, 0.000000000000000000 ) ) ;
#7790 = CARTESIAN_POINT ( 'NONE',  ( 0.2646305136544072623, -7.972778379581489716, -9.296005949277306613 ) ) ;
#7791 = AXIS2_PLACEMENT_3D ( 'NONE', #4804, #24740, #14725 ) ;
#7792 = EDGE_CURVE ( 'NONE', #17827, #41367, #28802, .T. ) ;
#7793 = CYLINDRICAL_SURFACE ( 'NONE', #29923, 5.000000000000000888 ) ;
#7794 = AXIS2_PLACEMENT_3D ( 'NONE', #32179, #52808, #52504 ) ;
#7795 = DIRECTION ( 'NONE',  ( 1.000000000000000000, 0.000000000000000000, -0.000000000000000000 ) ) ;
#7796 = ORIENTED_EDGE ( 'NONE', *, *, #12424, .T. ) ;
#7797 = AXIS2_PLACEMENT_3D ( 'NONE', #56194, #20944, #57199 ) ;
#7798 = CARTESIAN_POINT ( 'NONE',  ( -37.00000000000000711, 9.700295462048664774, 7.376655759824919834 ) ) ;
#7799 = CARTESIAN_POINT ( 'NONE',  ( -37.00000000000000711, -12.60630747491664572, 1.908798535168333643 ) ) ;
#7800 = AXIS2_PLACEMENT_3D ( 'NONE', #21491, #6522, #41759 ) ;
#7801 = CARTESIAN_POINT ( 'NONE',  ( 2.251152103363650792, -4.812779263775054162, 5.930529991878074725 ) ) ;
#7802 = DIRECTION ( 'NONE',  ( 1.000000000000000000, -0.000000000000000000, 0.000000000000000000 ) ) ;
#7803 = EDGE_CURVE ( 'NONE', #12091, #28250, #49119, .T. ) ;
#7804 = B_SPLINE_CURVE_WITH_KNOTS ( 'NONE', 3,
 ( #12329, #28291, #24277, #33610, #18973, #13961, #28607, #44541, #23970, #17670, #37932, #27970, #38596, #4007, #59215, #32926, #58224, #3710, #54222 ),
 .UNSPECIFIED., .F., .F.,
 ( 4, 3, 3, 3, 3, 3, 4 ),
 ( 8.673617379884035472E-19, 2.831840207499595013E-05, 4.217266859840597111E-05, 5.602024318396033026E-05, 6.290810167969150990E-05, 9.120440630944968421E-05, 0.0001153103026479758458 ),
 .UNSPECIFIED. ) ;
#7805 = AXIS2_PLACEMENT_3D ( 'NONE', #6443, #32351, #47016 ) ;
#7806 = FACE_OUTER_BOUND ( 'NONE', #31645, .T. ) ;
#7807 = ADVANCED_FACE ( 'NONE', ( #40405 ), #41065, .T. ) ;
#7808 = CIRCLE ( 'NONE', #50301, 5.000000000000000888 ) ;
#7809 = CARTESIAN_POINT ( 'NONE',  ( 1.937114397841935398, 12.45230409340485878, -3.111612666689950846 ) ) ;
#7810 = ADVANCED_FACE ( 'NONE', ( #60709 ), #197, .T. ) ;
#7811 = ORIENTED_EDGE ( 'NONE', *, *, #21976, .F. ) ;
#7812 = LINE ( 'NONE', #23770, #50000 ) ;
#7813 = CARTESIAN_POINT ( 'NONE',  ( 0.2648978790185593790, -11.55204314799266818, 4.063980959785006952 ) ) ;
#7814 = FACE_OUTER_BOUND ( 'NONE', #19196, .T. ) ;
#7815 = CARTESIAN_POINT ( 'NONE',  ( 0.8745425597690195119, -31.03649492335506110, 14.44372008463322921 ) ) ;
#7816 = CIRCLE ( 'NONE', #13120, 12.75000000000000178 ) ;
#7817 = ADVANCED_FACE ( 'NONE', ( #61344 ), #54401, .F. ) ;
#7818 = CARTESIAN_POINT ( 'NONE',  ( -37.00000000000000711, 0.000000000000000000, 0.000000000000000000 ) ) ;
#7819 = CARTESIAN_POINT ( 'NONE',  ( -24.87682914247800881, -10.97525152144739202, 7.868201376384557300 ) ) ;
#7820 = ORIENTED_EDGE ( 'NONE', *, *, #10086, .F. ) ;
#7821 = FACE_OUTER_BOUND ( 'NONE', #52258, .T. ) ;
#7822 = CARTESIAN_POINT ( 'NONE',  ( 35.00000000000000000, -6.475373545682373333, -10.32377448871666026 ) ) ;
#7823 = EDGE_CURVE ( 'NONE', #11411, #32398, #22436, .T. ) ;
#7824 = CARTESIAN_POINT ( 'NONE',  ( 2.000000000000001776, 0.000000000000000000, 0.000000000000000000 ) ) ;
#7825 = CARTESIAN_POINT ( 'NONE',  ( -18.56158150824929010, 4.674298569737585396, -11.05522311479379205 ) ) ;
#7826 = VERTEX_POINT ( 'NONE', #51413 ) ;
#7827 = DIRECTION ( 'NONE',  ( -1.000000000000000000, 0.000000000000000000, 0.000000000000000000 ) ) ;
#7828 = DIRECTION ( 'NONE',  ( 0.000000000000000000, 0.000000000000000000, 1.000000000000000000 ) ) ;
#7829 = ORIENTED_EDGE ( 'NONE', *, *, #49283, .F. ) ;
#7830 = VECTOR ( 'NONE', #33712, 1000.000000000000000 ) ;
#7831 = ORIENTED_EDGE ( 'NONE', *, *, #65454, .T. ) ;
#7832 = FACE_OUTER_BOUND ( 'NONE', #33175, .T. ) ;
#7833 = EDGE_CURVE ( 'NONE', #28337, #45163, #61040, .T. ) ;
#7834 = EDGE_LOOP ( 'NONE', ( #27011, #2207, #39484, #5504 ) ) ;
#7835 = EDGE_CURVE ( 'NONE', #46122, #57170, #50420, .T. ) ;
#7836 = CARTESIAN_POINT ( 'NONE',  ( -37.25000000000000711, -1.694065894508600678E-18, 1.500000000000000222 ) ) ;
#7837 = LINE ( 'NONE', #18795, #40000 ) ;
#7838 = CARTESIAN_POINT ( 'NONE',  ( 37.00000000000000711, 4.705694406421931860E-17, -3.469127814946512892E-15 ) ) ;
#7839 = CARTESIAN_POINT ( 'NONE',  ( 2.297017764050092392, -7.563558677601590396, -1.166330442180250726 ) ) ;
#7840 = VECTOR ( 'NONE', #16493, 1000.000000000000000 ) ;
#7841 = DIRECTION ( 'NONE',  ( 0.000000000000000000, 1.000000000000000000, 0.000000000000000000 ) ) ;
#7842 = AXIS2_PLACEMENT_3D ( 'NONE', #58175, #57529, #42517 ) ;
#7843 = ADVANCED_FACE ( 'NONE', ( #15473 ), #5184, .T. ) ;
#7844 = CARTESIAN_POINT ( 'NONE',  ( 35.00000000000000000, 10.02106554660720050, 7.882940143791660859 ) ) ;
#7846 = ORIENTED_EDGE ( 'NONE', *, *, #33182, .T. ) ;
#7845 = LINE ( 'NONE', #32742, #44654 ) ;
#7847 = CARTESIAN_POINT ( 'NONE',  ( 1.109979610372329395, 4.732439402375099746, -11.59954799439127449 ) ) ;
#7848 = VERTEX_POINT ( 'NONE', #25132 ) ;
#7849 = CARTESIAN_POINT ( 'NONE',  ( 0.2652384529303136174, 10.57229402027116372, -6.180212112237552624 ) ) ;
#7850 = ORIENTED_EDGE ( 'NONE', *, *, #62771, .F. ) ;
#7851 = VERTEX_POINT ( 'NONE', #16132 ) ;
#7852 = SHAPE_DEFINITION_REPRESENTATION ( #39172, #29683 ) ;
#7853 = CARTESIAN_POINT ( 'NONE',  ( -24.85695914810692386, 10.87191068482259126, 8.004987175091917706 ) ) ;
#7854 = CARTESIAN_POINT ( 'NONE',  ( -11.31614860309221626, -29.68432482266610606, 9.654990830002102342 ) ) ;
#7855 = AXIS2_PLACEMENT_3D ( 'NONE', #12389, #62944, #42989 ) ;
#7856 = CARTESIAN_POINT ( 'NONE',  ( -35.00000000000000000, 7.499679039484183463, -9.040300684349618976 ) ) ;
#7857 = CARTESIAN_POINT ( 'NONE',  ( 22.57855258442564761, -4.427776684447072952, 11.15324139578564910 ) ) ;
#7858 = CARTESIAN_POINT ( 'NONE',  ( -26.58564210842043707, -3.638521970294202657, 24.00000000000000355 ) ) ;
#7859 = DIRECTION ( 'NONE',  ( 0.000000000000000000, 0.01356324068817998940, -0.9999080150203990547 ) ) ;
#7860 = VERTEX_POINT ( 'NONE', #45401 ) ;
#7861 = CARTESIAN_POINT ( 'NONE',  ( -25.77583339569473964, -10.55051720252683722, 5.718653903698916352 ) ) ;
#7862 = CARTESIAN_POINT ( 'NONE',  ( 0.3675815128205894289, -0.2638082659429279997, 12.27743992903066150 ) ) ;
#7863 = CARTESIAN_POINT ( 'NONE',  ( 2.000000000000001776, -7.203928197742102135, 2.086484728383119158 ) ) ;
#7864 = VECTOR ( 'NONE', #55788, 1000.000000000000000 ) ;
#7865 = ORIENTED_EDGE ( 'NONE', *, *, #62645, .T. ) ;
#7866 = CARTESIAN_POINT ( 'NONE',  ( 2.000000000000001776, -6.750946897830710114, 1.593658756657014397 ) ) ;
#7867 = VERTEX_POINT ( 'NONE', #41386 ) ;
#7868 = DIRECTION ( 'NONE',  ( 1.000000000000000000, 0.000000000000000000, 0.000000000000000000 ) ) ;
#7869 = DIRECTION ( 'NONE',  ( 0.000000000000000000, 1.000000000000000000, 0.000000000000000000 ) ) ;
#7870 = FACE_OUTER_BOUND ( 'NONE', #6679, .T. ) ;
#7871 = CARTESIAN_POINT ( 'NONE',  ( 35.00000000000000000, 9.557269938331552694, -7.561043153948004303 ) ) ;
#7872 = EDGE_CURVE ( 'NONE', #10610, #6941, #24578, .T. ) ;
#7873 = CARTESIAN_POINT ( 'NONE',  ( -28.67667724226168602, 1.375746547601641723, 1.299025457479336287 ) ) ;
#7874 = CARTESIAN_POINT ( 'NONE',  ( 0.000000000000000000, -4.604744433234713163, 5.919993978425451608 ) ) ;
#7875 = CIRCLE ( 'NONE', #39754, 12.75000000000000178 ) ;
#7876 = CARTESIAN_POINT ( 'NONE',  ( 2.284126774967660811, 3.960764882115096697, -6.543266298866090125 ) ) ;
#7877 = ORIENTED_EDGE ( 'NONE', *, *, #46322, .F. ) ;
#7878 = CARTESIAN_POINT ( 'NONE',  ( -37.00000000000000711, 9.321877890560440250, 7.146664589317944127 ) ) ;
#7879 = ORIENTED_EDGE ( 'NONE', *, *, #29370, .T. ) ;
#7880 = DIRECTION ( 'NONE',  ( 0.000000000000000000, 0.2355298848897446895, 0.9718671068226476528 ) ) ;
#7881 = CIRCLE ( 'NONE', #47190, 5.000000000000000000 ) ;
#7882 = FACE_OUTER_BOUND ( 'NONE', #48068, .T. ) ;
#7883 = EDGE_CURVE ( 'NONE', #61480, #4911, #35141, .T. ) ;
#7884 = CIRCLE ( 'NONE', #42890, 2.899999999999995026 ) ;
#7885 = CARTESIAN_POINT ( 'NONE',  ( 2.000000000000001776, -0.2704997240204360387, -6.931223712253490987 ) ) ;
#7886 = ORIENTED_EDGE ( 'NONE', *, *, #43030, .T. ) ;
#7887 = EDGE_CURVE ( 'NONE', #10303, #36936, #22367, .T. ) ;
#7888 = CARTESIAN_POINT ( 'NONE',  ( -27.08506889328343803, 0.2104793012480555281, 2.284141197253888311 ) ) ;
#7889 = EDGE_LOOP ( 'NONE', ( #1777, #31982, #52803, #39873 ) ) ;
#7890 = CARTESIAN_POINT ( 'NONE',  ( 2.000000000000001776, -0.4129979343796691404, -6.800241778083718991 ) ) ;
#7891 = CARTESIAN_POINT ( 'NONE',  ( 8.633087204097703804, 5.803048762801607197, 10.50557656966853592 ) ) ;
#7892 = CARTESIAN_POINT ( 'NONE',  ( -27.08871896697732140, -2.082324523416154261, -0.9878677378287702426 ) ) ;
#7893 = CARTESIAN_POINT ( 'NONE',  ( 2.262775599886256650, 1.465770593192990745, -7.499645832851591365 ) ) ;
#7894 = EDGE_CURVE ( 'NONE', #16757, #53403, #37391, .T. ) ;
#7895 = VERTEX_POINT ( 'NONE', #62328 ) ;
#7896 = AXIS2_PLACEMENT_3D ( 'NONE', #31724, #6819, #31091 ) ;
#7897 = CARTESIAN_POINT ( 'NONE',  ( 0.2653141617321031487, -6.084921229689344457, -10.62747662594936671 ) ) ;
#7898 = CARTESIAN_POINT ( 'NONE',  ( -22.29978294495153790, -2.590262069787973243, 2.710748743830185603 ) ) ;
#7899 = DIRECTION ( 'NONE',  ( 0.000000000000000000, 0.000000000000000000, 1.000000000000000000 ) ) ;
#7900 = DIRECTION ( 'NONE',  ( -0.3939253465568943180, -0.8603393047164982210, 0.3234796780324276089 ) ) ;
#7901 = CIRCLE ( 'NONE', #45057, 12.18649999999999878 ) ;
#7902 = CARTESIAN_POINT ( 'NONE',  ( 2.247112776671468914, -0.1165461824817215913, -7.635437439951572536 ) ) ;
#7903 = DIRECTION ( 'NONE',  ( 1.000000000000000000, -0.000000000000000000, -0.000000000000000000 ) ) ;
#7904 = ORIENTED_EDGE ( 'NONE', *, *, #43244, .T. ) ;
#7905 = CARTESIAN_POINT ( 'NONE',  ( -27.08426504710140392, 1.649100202714206986, -1.591094357919260016 ) ) ;
#7907 = VECTOR ( 'NONE', #29755, 1000.000000000000000 ) ;
#7906 = CARTESIAN_POINT ( 'NONE',  ( 29.64698554648902729, 8.428051259464909961, 10.58407887936916758 ) ) ;
#7908 = EDGE_CURVE ( 'NONE', #8359, #64295, #33459, .T. ) ;
#7909 = CARTESIAN_POINT ( 'NONE',  ( 0.3040950598368144520, 6.347045025870913904, -10.49113473328024249 ) ) ;
#7910 = VERTEX_POINT ( 'NONE', #12120 ) ;
#7911 = CARTESIAN_POINT ( 'NONE',  ( -10.66655393549213393, -4.452669714455520733, -12.75039268524656855 ) ) ;
#7912 = CYLINDRICAL_SURFACE ( 'NONE', #12923, 4.999999999999998224 ) ;
#7913 = DIRECTION ( 'NONE',  ( 0.000000000000000000, -0.9868265225415244757, -0.1617819965527746984 ) ) ;
#7914 = ADVANCED_FACE ( 'NONE', ( #33053 ), #7451, .T. ) ;
#7915 = AXIS2_PLACEMENT_3D ( 'NONE', #41141, #61424, #1266 ) ;
#7916 = CYLINDRICAL_SURFACE ( 'NONE', #50910, 12.74999999999999822 ) ;
#7917 = DIRECTION ( 'NONE',  ( 0.000000000000000000, -0.9999080150203992767, -0.01356324068816951341 ) ) ;
#7918 = ADVANCED_FACE ( 'NONE', ( #7806 ), #1833, .T. ) ;
#7919 = AXIS2_PLACEMENT_3D ( 'NONE', #18274, #58507, #38535 ) ;
#7920 = VERTEX_POINT ( 'NONE', #17116 ) ;
#7921 = CARTESIAN_POINT ( 'NONE',  ( 0.3106921474978504016, 1.896868624983064411, 12.11369598333777020 ) ) ;
#7922 = EDGE_CURVE ( 'NONE', #19174, #35378, #38341, .T. ) ;
#7923 = VERTEX_POINT ( 'NONE', #28090 ) ;
#7924 = DIRECTION ( 'NONE',  ( -1.000000000000000000, 0.000000000000000000, -0.000000000000000000 ) ) ;
#7925 = CARTESIAN_POINT ( 'NONE',  ( 0.2834382757448022372, -9.514772331577374231, -7.719209397492075908 ) ) ;
#7926 = DIRECTION ( 'NONE',  ( -1.000000000000000000, -0.000000000000000000, -0.000000000000000000 ) ) ;
#7927 = DIRECTION ( 'NONE',  ( 0.7932577242209934987, -0.6088860180392799970, 0.000000000000000000 ) ) ;
#7928 = DIRECTION ( 'NONE',  ( 1.000000000000000000, 0.000000000000000000, 0.000000000000000000 ) ) ;
#7929 = EDGE_CURVE ( 'NONE', #59672, #20489, #2835, .T. ) ;
#7930 = CARTESIAN_POINT ( 'NONE',  ( 2.280717697723835258, -1.173604464351654331, 7.556934756535380160 ) ) ;
#7931 = DIRECTION ( 'NONE',  ( 0.000000000000000000, 0.01356324068817991828, -0.9999080150203990547 ) ) ;
#7932 = ORIENTED_EDGE ( 'NONE', *, *, #38256, .T. ) ;
#7933 = EDGE_LOOP ( 'NONE', ( #40029, #52833, #44939, #64283 ) ) ;
#7934 = AXIS2_PLACEMENT_3D ( 'NONE', #40095, #44425, #19175 ) ;
#7935 = FILL_AREA_STYLE_COLOUR ( '', #41674 ) ;
#7936 = EDGE_LOOP ( 'NONE', ( #31392, #42646, #11562, #5289 ) ) ;
#7937 =( NAMED_UNIT ( * ) SI_UNIT ( $, .STERADIAN. ) SOLID_ANGLE_UNIT ( ) );
#7938 = CARTESIAN_POINT ( 'NONE',  ( -41.00000000000000711, -25.03188948156373073, -4.500000000000008882 ) ) ;
#7939 = CARTESIAN_POINT ( 'NONE',  ( 0.3675815128205894289, 12.04510820461659293, 2.391755495700645273 ) ) ;
#7940 = CARTESIAN_POINT ( 'NONE',  ( -35.00000000000000000, 0.000000000000000000, 0.000000000000000000 ) ) ;
#7941 = ORIENTED_EDGE ( 'NONE', *, *, #2236, .F. ) ;
#7942 = CARTESIAN_POINT ( 'NONE',  ( -22.27384469013076185, -0.9835229356382323429, 3.548341908721027060 ) ) ;
#7943 = CIRCLE ( 'NONE', #16430, 12.18649999999999878 ) ;
#7944 = CARTESIAN_POINT ( 'NONE',  ( 2.263328370261525446, 6.545781832005237000, -3.943189046766256478 ) ) ;
#7945 = CARTESIAN_POINT ( 'NONE',  ( -35.04709527796842394, 0.007030359780627049027, -0.01016988845958279042 ) ) ;
#7946 = ORIENTED_EDGE ( 'NONE', *, *, #27900, .T. ) ;
#7947 = ORIENTED_EDGE ( 'NONE', *, *, #20310, .T. ) ;
#7948 = DIRECTION ( 'NONE',  ( -1.000000000000000000, -0.000000000000000000, 0.000000000000000000 ) ) ;
#7950 = ORIENTED_EDGE ( 'NONE', *, *, #6322, .F. ) ;
#7949 = AXIS2_PLACEMENT_3D ( 'NONE', #64582, #58664, #63950 ) ;
#7951 = DIRECTION ( 'NONE',  ( 1.000000000000000000, 0.000000000000000000, 0.000000000000000000 ) ) ;
#7952 = EDGE_LOOP ( 'NONE', ( #60061, #32171, #46523, #40520 ) ) ;
#7953 = ORIENTED_EDGE ( 'NONE', *, *, #35915, .F. ) ;
#7954 = CARTESIAN_POINT ( 'NONE',  ( -19.69476066079020171, -4.201994156881551312, -11.24025111398909615 ) ) ;
#7955 = AXIS2_PLACEMENT_3D ( 'NONE', #40795, #36452, #26465 ) ;
#7956 = CARTESIAN_POINT ( 'NONE',  ( -27.09569413923885861, -1.607816962455224985, 1.680421072128823967 ) ) ;
#7957 = EDGE_CURVE ( 'NONE', #24707, #9063, #26768, .T. ) ;
#7958 = DIRECTION ( 'NONE',  ( 0.000000000000000000, 0.2006870767258820687, -0.9796553971857756560 ) ) ;
#7959 = CYLINDRICAL_SURFACE ( 'NONE', #1221, 12.75000000000000178 ) ;
#7960 = CARTESIAN_POINT ( 'NONE',  ( 37.00000000000000711, 2.220215194442072271, 11.98254675519225287 ) ) ;
#7961 = CARTESIAN_POINT ( 'NONE',  ( -35.00000000000000000, -5.273331777780412288, 10.49591321039678959 ) ) ;
#7962 = ADVANCED_FACE ( 'NONE', ( #11784 ), #52706, .T. ) ;
#7963 = ORIENTED_EDGE ( 'NONE', *, *, #34823, .T. ) ;
#7964 = CARTESIAN_POINT ( 'NONE',  ( 2.241311220309555097, -1.417008678104535679, 7.501736494813740386 ) ) ;
#7965 = DIRECTION ( 'NONE',  ( 0.000000000000000000, 0.000000000000000000, 1.000000000000000000 ) ) ;
#7966 = CARTESIAN_POINT ( 'NONE',  ( 2.241317068080780128, 3.737686401539939141, -6.656851426547526707 ) ) ;
#7967 = CARTESIAN_POINT ( 'NONE',  ( -35.05012975565874456, -0.008684292310218014177, -0.01089417657933552247 ) ) ;
#7968 = CARTESIAN_POINT ( 'NONE',  ( -22.59969328935885358, 2.921971394153385138, -3.618004136135298143 ) ) ;
#7969 = CYLINDRICAL_SURFACE ( 'NONE', #3197, 6.936499999999988120 ) ;
#7970 = CARTESIAN_POINT ( 'NONE',  ( 35.00000000000000000, 11.42599468261429152, -4.237620530777845396 ) ) ;
#7971 = CARTESIAN_POINT ( 'NONE',  ( 0.3164563675027701195, -11.60369811966059217, -3.967501530099192930 ) ) ;
#7972 = EDGE_CURVE ( 'NONE', #40710, #46217, #38651, .T. ) ;
#7973 = CARTESIAN_POINT ( 'NONE',  ( -4.975205859172452172, -1.416020129149132778, 11.91616074890920451 ) ) ;
#7974 = AXIS2_PLACEMENT_3D ( 'NONE', #449, #61273, #31013 ) ;
#7975 = ORIENTED_EDGE ( 'NONE', *, *, #60536, .F. ) ;
#7976 = CARTESIAN_POINT ( 'NONE',  ( 2.373367633546869637, -7.151506276328608358, -2.795365972209146399 ) ) ;
#7977 =( BOUNDED_CURVE ( )  B_SPLINE_CURVE ( 3, ( #39791, #9507, #60393, #54105 ),
 .UNSPECIFIED., .F., .F. ) 
 B_SPLINE_CURVE_WITH_KNOTS ( ( 4, 4 ),
 ( 3.954312062358600333, 4.006764403430960186 ),
 .UNSPECIFIED. ) 
 CURVE ( )  GEOMETRIC_REPRESENTATION_ITEM ( )  RATIONAL_B_SPLINE_CURVE ( ( 1.000000000000000000, 0.9997707424672948040, 0.9997707424672948040, 1.000000000000000000 ) ) 
 REPRESENTATION_ITEM ( '' )  );
#7978 = VERTEX_POINT ( 'NONE', #32706 ) ;
#7979 = CARTESIAN_POINT ( 'NONE',  ( 35.00000000000000000, -9.217970097227778936, -7.971186206369441862 ) ) ;
#7980 = CARTESIAN_POINT ( 'NONE',  ( 0.3218525148189836926, -0.2444206315274009833, 12.26259572563018452 ) ) ;
#7981 = DIRECTION ( 'NONE',  ( 1.000000000000000000, 0.000000000000000000, -0.000000000000000000 ) ) ;
#7982 = LINE ( 'NONE', #28248, #49028 ) ;
#7983 = CARTESIAN_POINT ( 'NONE',  ( 2.373367633546870969, -4.795703124519850036, -5.996611082972014728 ) ) ;
#7984 = EDGE_CURVE ( 'NONE', #57723, #7359, #43355, .T. ) ;
#7985 = EDGE_LOOP ( 'NONE', ( #34850, #64535, #17566, #57076 ) ) ;
#7986 =( GEOMETRIC_REPRESENTATION_CONTEXT ( 3 ) GLOBAL_UNCERTAINTY_ASSIGNED_CONTEXT ( ( #27676 ) ) GLOBAL_UNIT_ASSIGNED_CONTEXT ( ( #5383, #15005, #21587 ) ) REPRESENTATION_CONTEXT ( 'NONE', 'WORKASPACE' ) );
#7987 = CARTESIAN_POINT ( 'NONE',  ( 1.104777566491139229, 10.60111489796743278, -6.672212870706091259 ) ) ;
#7988 = CARTESIAN_POINT ( 'NONE',  ( 2.305787727787083519, -3.682701754025559993, 6.711944854845811825 ) ) ;
#7989 = DIRECTION ( 'NONE',  ( 0.000000000000000000, 0.01356324068817991828, -0.9999080150203990547 ) ) ;
#7990 = CARTESIAN_POINT ( 'NONE',  ( 0.2653519890518167279, -2.126538543977996465, -12.06014856238022936 ) ) ;
#7991 = EDGE_CURVE ( 'NONE', #6431, #29014, #8633, .T. ) ;
#7992 = CARTESIAN_POINT ( 'NONE',  ( -10.00000000000000178, 0.000000000000000000, 0.000000000000000000 ) ) ;
#7993 = AXIS2_PLACEMENT_3D ( 'NONE', #43199, #12951, #57539 ) ;
#7994 = ORIENTED_EDGE ( 'NONE', *, *, #13774, .F. ) ;
#7995 = CARTESIAN_POINT ( 'NONE',  ( 3.152665057735843490, -3.546019893114926713, 7.102135024646879735 ) ) ;
#7996 = PRODUCT_DEFINITION_SHAPE ( 'NONE', 'NONE',  #65809 ) ;
#7997 = FACE_OUTER_BOUND ( 'NONE', #13409, .T. ) ;
#7998 = CARTESIAN_POINT ( 'NONE',  ( 2.305787727787084407, -3.971363876083918498, -6.545285700970570275 ) ) ;
#7999 = ADVANCED_FACE ( 'NONE', ( #58344 ), #63310, .T. ) ;
#8000 = CIRCLE ( 'NONE', #45146, 12.18650000000000055 ) ;
#8001 = VERTEX_POINT ( 'NONE', #28400 ) ;
#8002 = ORIENTED_EDGE ( 'NONE', *, *, #39502, .T. ) ;
#8003 = CARTESIAN_POINT ( 'NONE',  ( -27.08588607604433562, 2.215240480751983654, -0.6046196991082997130 ) ) ;
#8004 = EDGE_CURVE ( 'NONE', #22247, #14897, #46186, .T. ) ;
#8005 = ORIENTED_EDGE ( 'NONE', *, *, #222, .F. ) ;
#8006 = CARTESIAN_POINT ( 'NONE',  ( 2.297017764050033772, 5.044319338147331244, 5.755222757172066217 ) ) ;
#8007 = CARTESIAN_POINT ( 'NONE',  ( 35.00000000000000000, 4.705694406421931860E-17, -3.469127814946512892E-15 ) ) ;
#8008 = CARTESIAN_POINT ( 'NONE',  ( -27.08776759928965205, -1.644157618163919699, -1.611072893086249014 ) ) ;
#8009 = CARTESIAN_POINT ( 'NONE',  ( 35.00000000000000000, 10.70999494708492250, -5.814360711498331113 ) ) ;
#8010 = EDGE_CURVE ( 'NONE', #48073, #807, #21569, .T. ) ;
#8011 = DIRECTION ( 'NONE',  ( -0.000000000000000000, -1.000000000000000000, -0.000000000000000000 ) ) ;
#8012 = ORIENTED_EDGE ( 'NONE', *, *, #49946, .F. ) ;
#8013 = VERTEX_POINT ( 'NONE', #34035 ) ;
#8014 = ORIENTED_EDGE ( 'NONE', *, *, #40213, .T. ) ;
#8015 = CARTESIAN_POINT ( 'NONE',  ( 2.298277635560276977, 7.246601281227255775, -2.461898367585308556 ) ) ;
#8016 = DIRECTION ( 'NONE',  ( 0.000000000000000000, 0.000000000000000000, 1.000000000000000000 ) ) ;
#8018 = EDGE_CURVE ( 'NONE', #11746, #52324, #29071, .T. ) ;
#8017 = ORIENTED_EDGE ( 'NONE', *, *, #21381, .T. ) ;
#8019 = CARTESIAN_POINT ( 'NONE',  ( -37.00000000000000711, 0.000000000000000000, 0.000000000000000000 ) ) ;
#8020 = CARTESIAN_POINT ( 'NONE',  ( 2.268878695253354838, -7.551766617932575976, 1.181158368266927106 ) ) ;
#8021 = ORIENTED_EDGE ( 'NONE', *, *, #22340, .F. ) ;
#8022 = CARTESIAN_POINT ( 'NONE',  ( -26.74023318801843985, 1.916028097164423905, -2.752802096869866766 ) ) ;
#8023 = CARTESIAN_POINT ( 'NONE',  ( 37.00000000000000711, 4.705694406421931860E-17, -3.469127814946512892E-15 ) ) ;
#8024 = CARTESIAN_POINT ( 'NONE',  ( 2.000000000000001776, -6.767909380267593811, 0.7805499053120233954 ) ) ;
#8025 = ORIENTED_EDGE ( 'NONE', *, *, #23571, .F. ) ;
#8026 = EDGE_LOOP ( 'NONE', ( #48919, #39897, #52413, #11999 ) ) ;
#8027 = DIRECTION ( 'NONE',  ( 1.000000000000000000, 0.000000000000000000, -0.000000000000000000 ) ) ;
#8028 = VERTEX_POINT ( 'NONE', #29694 ) ;
#8029 = VERTEX_POINT ( 'NONE', #8451 ) ;
#8030 = CARTESIAN_POINT ( 'NONE',  ( 0.2648978790185584908, -4.312320170909314854, 11.46165506714226900 ) ) ;
#8031 = CARTESIAN_POINT ( 'NONE',  ( 8.395146353820784668, -32.40713589851601739, -12.72020452408354529 ) ) ;
#8032 = DIRECTION ( 'NONE',  ( -1.000000000000000000, 0.000000000000000000, 0.000000000000000000 ) ) ;
#8033 = DIRECTION ( 'NONE',  ( 0.000000000000000000, 0.2355298848897447728, 0.9718671068226475418 ) ) ;
#8034 = PLANE ( 'NONE',  #39360 ) ;
#8035 = CARTESIAN_POINT ( 'NONE',  ( 1.020182472822815711, -0.4462553704985123826, 12.48987306958583687 ) ) ;
#8036 = CARTESIAN_POINT ( 'NONE',  ( -27.75684343571922952, -10.82790328082247377, -5.180978323404352714 ) ) ;
#8037 = ORIENTED_EDGE ( 'NONE', *, *, #44065, .T. ) ;
#8038 = CARTESIAN_POINT ( 'NONE',  ( 2.247206125382826158, -7.135412558555532136, -2.720255231378005956 ) ) ;
#8039 = EDGE_CURVE ( 'NONE', #62061, #38335, #34373, .T. ) ;
#8040 = AXIS2_PLACEMENT_3D ( 'NONE', #12605, #42528, #22949 ) ;
#8041 = ORIENTED_EDGE ( 'NONE', *, *, #52887, .T. ) ;
#8042 = CARTESIAN_POINT ( 'NONE',  ( 2.261269890822070749, -2.744033622443662779, 7.131324074141573988 ) ) ;
#8043 = CARTESIAN_POINT ( 'NONE',  ( 37.00000000000000711, 4.705694406421931860E-17, -3.469127814946512892E-15 ) ) ;
#8044 = ORIENTED_EDGE ( 'NONE', *, *, #46405, .T. ) ;
#8045 = CARTESIAN_POINT ( 'NONE',  ( -19.47984447937493613, -3.750539801530005768, 12.96855624952674724 ) ) ;
#8046 = CARTESIAN_POINT ( 'NONE',  ( 0.2872850955227708725, 6.306790329742928414, 10.50585060073182753 ) ) ;
#8047 = CARTESIAN_POINT ( 'NONE',  ( 0.2958664285830446272, -2.345117904768542871, -12.02992237133200426 ) ) ;
#8048 = ORIENTED_EDGE ( 'NONE', *, *, #35872, .T. ) ;
#8049 = ORIENTED_EDGE ( 'NONE', *, *, #31011, .F. ) ;
#8050 = CARTESIAN_POINT ( 'NONE',  ( 2.556980015514201288, -6.815084337351986932, -3.668282146013173151 ) ) ;
#8051 = ORIENTED_EDGE ( 'NONE', *, *, #35056, .F. ) ;
#8052 = DIRECTION ( 'NONE',  ( 1.000000000000000000, -0.000000000000000000, 0.000000000000000000 ) ) ;
#8053 = CARTESIAN_POINT ( 'NONE',  ( -3.761952589723977169, -7.433916943621393436, 9.430559907043596368 ) ) ;
#8054 = LINE ( 'NONE', #28982, #62159 ) ;
#8055 = CARTESIAN_POINT ( 'NONE',  ( -2.747965937637946165, 11.18537856137285580, 4.360398752428172209 ) ) ;
#8056 = CARTESIAN_POINT ( 'NONE',  ( 0.000000000000000000, -6.935703035393428806, -0.1051458740708305362 ) ) ;
#8057 = EDGE_CURVE ( 'NONE', #65704, #44894, #4128, .T. ) ;
#8058 = ORIENTED_EDGE ( 'NONE', *, *, #37923, .T. ) ;
#8059 = CYLINDRICAL_SURFACE ( 'NONE', #18919, 4.999999999999999112 ) ;
#8060 = EDGE_CURVE ( 'NONE', #1336, #7532, #6487, .T. ) ;
#8061 = AXIS2_PLACEMENT_3D ( 'NONE', #28562, #2680, #23593 ) ;
#8062 = CARTESIAN_POINT ( 'NONE',  ( 17.13446681924518700, -29.51054447109571299, -9.416006455614729376 ) ) ;
#8063 = CARTESIAN_POINT ( 'NONE',  ( -27.08426571771018487, -0.9198084705429405705, 2.098821047392059658 ) ) ;
#8064 = CARTESIAN_POINT ( 'NONE',  ( 0.2653519890518174495, 7.871710682401907633, 9.381125756446593300 ) ) ;
#8065 = CARTESIAN_POINT ( 'NONE',  ( 7.313837862481380014, -6.193139553693423949, -10.28892890405838223 ) ) ;
#8066 = CARTESIAN_POINT ( 'NONE',  ( 2.963017218115634677, 5.350609950027751971, -5.778072204777588539 ) ) ;
#8067 = EDGE_CURVE ( 'NONE', #17999, #52684, #64913, .T. ) ;
#8068 = ORIENTED_EDGE ( 'NONE', *, *, #36143, .T. ) ;
#8069 = CARTESIAN_POINT ( 'NONE',  ( 2.251139882113958990, -0.1241612276497191941, 7.636654603229074745 ) ) ;
#8070 = AXIS2_PLACEMENT_3D ( 'NONE', #41818, #25210, #46477 ) ;
#8071 = ORIENTED_EDGE ( 'NONE', *, *, #19961, .T. ) ;
#8072 = DIRECTION ( 'NONE',  ( -1.000000000000000000, 0.000000000000000000, 0.000000000000000000 ) ) ;
#8073 = CARTESIAN_POINT ( 'NONE',  ( 35.00000000000000000, 4.705694406421931860E-17, -3.469127814946512892E-15 ) ) ;
#8074 = CARTESIAN_POINT ( 'NONE',  ( 36.00000000000000711, 6.950793414699941053, 10.68873102412834797 ) ) ;
#8075 = ORIENTED_EDGE ( 'NONE', *, *, #54374, .T. ) ;
#8076 = CARTESIAN_POINT ( 'NONE',  ( 37.25000000000000711, -27.21021009056489248, -4.500000000000000888 ) ) ;
#8077 = CARTESIAN_POINT ( 'NONE',  ( 1.719304012338249921, 10.22720798541395837, 7.581471372740089976 ) ) ;
#8078 = VERTEX_POINT ( 'NONE', #55966 ) ;
#8079 = VERTEX_POINT ( 'NONE', #41311 ) ;
#8080 = VERTEX_POINT ( 'NONE', #61594 ) ;
#8081 = CARTESIAN_POINT ( 'NONE',  ( 0.2706063244538022827, -7.737788863017243557, -9.494160524941774426 ) ) ;
#8082 = CONICAL_SURFACE ( 'NONE', #64359, 7.938172270156617749, 1.280189991382167047 ) ;
#8083 = EDGE_CURVE ( 'NONE', #12489, #62829, #35343, .T. ) ;
#8084 = CARTESIAN_POINT ( 'NONE',  ( -22.28629837673887693, -3.348758206500233925, -1.594277649056540902 ) ) ;
#8085 = VERTEX_POINT ( 'NONE', #55653 ) ;
#8086 = CARTESIAN_POINT ( 'NONE',  ( -47.00000000000000711, 0.000000000000000000, 0.000000000000000000 ) ) ;
#8087 = CARTESIAN_POINT ( 'NONE',  ( 2.034671305880900505, 11.65517003033663102, 0.7032348381690887162 ) ) ;
#8088 = DIRECTION ( 'NONE',  ( -0.000000000000000000, -0.000000000000000000, -1.000000000000000000 ) ) ;
#8089 = CARTESIAN_POINT ( 'NONE',  ( 18.12752167935788705, 7.578978283205488609, 9.315231351494983159 ) ) ;
#8090 = VERTEX_POINT ( 'NONE', #10399 ) ;
#8091 = CARTESIAN_POINT ( 'NONE',  ( 0.3164563675027606271, -7.696930404785105040, 9.546944054903065080 ) ) ;
#8092 = CARTESIAN_POINT ( 'NONE',  ( 13.20768530587737288, -34.09315906254132500, 9.434917751661075158 ) ) ;
#8093 = CARTESIAN_POINT ( 'NONE',  ( 2.288423627607477862, -1.486973602181100640, -7.504187945869075449 ) ) ;
#8095 = ORIENTED_EDGE ( 'NONE', *, *, #47562, .T. ) ;
#8094 = LINE ( 'NONE', #8746, #4343 ) ;
#8096 = FACE_OUTER_BOUND ( 'NONE', #60115, .T. ) ;
#8097 = ORIENTED_EDGE ( 'NONE', *, *, #50130, .F. ) ;
#8098 = CARTESIAN_POINT ( 'NONE',  ( -18.10219876433327357, 13.45940644062556757, 1.101009084313006037 ) ) ;
#8099 = ORIENTED_EDGE ( 'NONE', *, *, #9999, .T. ) ;
#8100 = DIRECTION ( 'NONE',  ( 0.000000000000000000, -0.01356324068817998940, 0.9999080150203990547 ) ) ;
#8101 = CARTESIAN_POINT ( 'NONE',  ( -22.66110217412718697, 2.622110956932579118, -4.192227617777399828 ) ) ;
#8102 = CYLINDRICAL_SURFACE ( 'NONE', #32956, 12.74999999999999822 ) ;
#8103 = CARTESIAN_POINT ( 'NONE',  ( 0.2648978790185602672, -4.063980959785125080, 11.55204314799262555 ) ) ;
#8104 = CARTESIAN_POINT ( 'NONE',  ( 0.2717059086739008755, 9.494961435243697068, 7.737372654246616577 ) ) ;
#8105 = CARTESIAN_POINT ( 'NONE',  ( -4.975205859172449507, -1.416020129149132778, -13.42553116244733680 ) ) ;
#8106 = DIRECTION ( 'NONE',  ( 0.000000000000000000, 0.000000000000000000, 1.000000000000000000 ) ) ;
#8107 = ADVANCED_FACE ( 'NONE', ( #19752 ), #5445, .T. ) ;
#8108 = ORIENTED_EDGE ( 'NONE', *, *, #11374, .T. ) ;
#8109 = CARTESIAN_POINT ( 'NONE',  ( 1.452237505248552996, -12.55261342181976403, 1.611965288198690116 ) ) ;
#8110 = VERTEX_POINT ( 'NONE', #20726 ) ;
#8111 = EDGE_CURVE ( 'NONE', #35473, #17729, #51331, .T. ) ;
#8112 = ORIENTED_EDGE ( 'NONE', *, *, #152, .F. ) ;
#8113 = FACE_OUTER_BOUND ( 'NONE', #13931, .T. ) ;
#8114 = CARTESIAN_POINT ( 'NONE',  ( -22.27945548916780183, 3.346394890313977744, 1.551028078364822704 ) ) ;
#8115 = CARTESIAN_POINT ( 'NONE',  ( 37.00000000000000711, 4.705694406421931860E-17, -3.469127814946512892E-15 ) ) ;
#8116 = CARTESIAN_POINT ( 'NONE',  ( 0.2647959493198559500, -10.53111783886895125, 6.249846955854230224 ) ) ;
#8117 = B_SPLINE_CURVE_WITH_KNOTS ( 'NONE', 3,
 ( #51594, #26300, #32259, #46580, #61873, #22279, #37591, #51914, #21656, #46917, #41583, #36606, #56910, #6355, #41913, #57558 ),
 .UNSPECIFIED., .F., .F.,
 ( 4, 3, 3, 3, 3, 4 ),
 ( 2.646037958931776106E-15, 0.0002126834539179706172, 0.0004253519300366259736, 0.0006380165497224161725, 0.0007442707582428239980, 0.0009453531351418035774 ),
 .UNSPECIFIED. ) ;
#8118 = CARTESIAN_POINT ( 'NONE',  ( 5.536195898058073439, -0.006672323185952749695, 0.005266167600747576234 ) ) ;
#8119 = DIRECTION ( 'NONE',  ( 0.000000000000000000, 0.5767582926624970074, 0.8169148498130275327 ) ) ;
#8120 = EDGE_CURVE ( 'NONE', #13346, #17960, #29833, .T. ) ;
#8121 = AXIS2_PLACEMENT_3D ( 'NONE', #27688, #20334, #15353 ) ;
#8122 = CARTESIAN_POINT ( 'NONE',  ( 0.5547464869798250930, -10.83828453080460719, -5.905377260991333976 ) ) ;
#8123 = AXIS2_PLACEMENT_3D ( 'NONE', #43697, #54355, #8791 ) ;
#8124 = ORIENTED_EDGE ( 'NONE', *, *, #35210, .F. ) ;
#8125 = CARTESIAN_POINT ( 'NONE',  ( -22.23402523511428086, 1.734723475976807094E-15, -8.673617379884035472E-15 ) ) ;
#8126 = LINE ( 'NONE', #45647, #36664 ) ;
#8127 = CARTESIAN_POINT ( 'NONE',  ( 6.661406098020970390, -4.211117136771884262, -11.23710102852283299 ) ) ;
#8128 = ADVANCED_FACE ( 'NONE', ( #52311 ), #62569, .T. ) ;
#8129 = B_SPLINE_CURVE_WITH_KNOTS ( 'NONE', 3,
 ( #20097, #40360, #10122, #50698, #21066, #11114, #5143, #41347, #61631, #16085, #2110, #62287, #23056 ),
 .UNSPECIFIED., .F., .F.,
 ( 4, 3, 3, 3, 4 ),
 ( 3.035766082959412415E-18, 6.607593386745364342E-05, 0.0001321518677373504551, 0.0001982171734706202092, 0.0002642860854759481208 ),
 .UNSPECIFIED. ) ;
#8130 = CARTESIAN_POINT ( 'NONE',  ( 36.00000000000000711, 8.235637554476776145, 9.733281772932070197 ) ) ;
#8131 = CARTESIAN_POINT ( 'NONE',  ( 37.00000000000000711, 1.908798535168559241, 12.60630747491660486 ) ) ;
#8132 = CARTESIAN_POINT ( 'NONE',  ( -10.66677318034315292, -4.454008058369508305, 12.74975837362279485 ) ) ;
#8133 = CARTESIAN_POINT ( 'NONE',  ( 35.00000000000000000, 9.348667969174517367, 7.817492529713752525 ) ) ;
#8134 = ORIENTED_EDGE ( 'NONE', *, *, #18077, .T. ) ;
#8135 = DIRECTION ( 'NONE',  ( 0.000000000000000000, 0.000000000000000000, -1.000000000000000000 ) ) ;
#8136 = CARTESIAN_POINT ( 'NONE',  ( 47.00000000000000711, 4.705694406421931860E-17, -3.469127814946512892E-15 ) ) ;
#8137 = DIRECTION ( 'NONE',  ( -1.000000000000000000, 0.000000000000000000, 0.000000000000000000 ) ) ;
#8138 = DIRECTION ( 'NONE',  ( 1.000000000000000000, 0.000000000000000000, 0.000000000000000000 ) ) ;
#8139 = ORIENTED_EDGE ( 'NONE', *, *, #24854, .F. ) ;
#8140 = CARTESIAN_POINT ( 'NONE',  ( -18.08686583997219088, 4.946258258172888667, 12.56318811865292062 ) ) ;
#8141 = CARTESIAN_POINT ( 'NONE',  ( 2.241352910868908754, -4.843133558968088614, -5.901537464758503937 ) ) ;
#8142 = FACE_OUTER_BOUND ( 'NONE', #13794, .T. ) ;
#8143 = ORIENTED_EDGE ( 'NONE', *, *, #29896, .F. ) ;
#8144 = DIRECTION ( 'NONE',  ( 1.000000000000000000, 0.000000000000000000, 0.000000000000000000 ) ) ;
#8145 = FACE_OUTER_BOUND ( 'NONE', #43577, .T. ) ;
#8146 = EDGE_LOOP ( 'NONE', ( #22031, #35231, #55530, #35135 ) ) ;
#8147 = VERTEX_POINT ( 'NONE', #16705 ) ;
#8148 = DIRECTION ( 'NONE',  ( -1.000000000000000000, -0.000000000000000000, 0.000000000000000000 ) ) ;
#8149 = EDGE_CURVE ( 'NONE', #11008, #34835, #3330, .T. ) ;
#8150 = AXIS2_PLACEMENT_3D ( 'NONE', #59523, #20835, #10857 ) ;
#8151 = ORIENTED_EDGE ( 'NONE', *, *, #54972, .F. ) ;
#8152 = CARTESIAN_POINT ( 'NONE',  ( 1.287602823386723383, -12.28793447239711512, -2.727479899220638604 ) ) ;
#8153 = CARTESIAN_POINT ( 'NONE',  ( 35.00000000000000000, -6.584150480049477672, 10.25474254703959431 ) ) ;
#8154 = CARTESIAN_POINT ( 'NONE',  ( 37.00000000000000711, -11.90598845858536947, -4.561791185930372805 ) ) ;
#8155 = CARTESIAN_POINT ( 'NONE',  ( 2.241352910868908310, 6.652881166698564108, -3.744764251556923274 ) ) ;
#8156 =( BOUNDED_CURVE ( )  B_SPLINE_CURVE ( 3, ( #14675, #48997, #34958, #13709 ),
 .UNSPECIFIED., .F., .F. ) 
 B_SPLINE_CURVE_WITH_KNOTS ( ( 4, 4 ),
 ( 3.922071288503527153, 3.961819178845479517 ),
 .UNSPECIFIED. ) 
 CURVE ( )  GEOMETRIC_REPRESENTATION_ITEM ( )  RATIONAL_B_SPLINE_CURVE ( ( 1.000000000000000000, 0.9998683464345071714, 0.9998683464345071714, 1.000000000000000000 ) ) 
 REPRESENTATION_ITEM ( '' )  );
#8157 = CARTESIAN_POINT ( 'NONE',  ( 2.368238019615318990, 3.681632831800480954, -6.736275681109146873 ) ) ;
#8158 = CARTESIAN_POINT ( 'NONE',  ( 1.547277799337431592, 12.12286970032282873, 3.695326562729380981 ) ) ;
#8160 = ORIENTED_EDGE ( 'NONE', *, *, #29869, .T. ) ;
#8159 = CARTESIAN_POINT ( 'NONE',  ( 41.00000000000000711, -1.694065894508600678E-18, 0.000000000000000000 ) ) ;
#8161 = CARTESIAN_POINT ( 'NONE',  ( 0.3040950598368144520, 9.229598020917689993, 8.072385578287505581 ) ) ;
#8162 = ORIENTED_EDGE ( 'NONE', *, *, #34682, .F. ) ;
#8163 = CARTESIAN_POINT ( 'NONE',  ( -47.00000000000000711, 0.000000000000000000, 0.000000000000000000 ) ) ;
#8164 = EDGE_LOOP ( 'NONE', ( #431, #50830, #25766, #51922 ) ) ;
#8165 = ORIENTED_EDGE ( 'NONE', *, *, #57289, .F. ) ;
#8166 = CARTESIAN_POINT ( 'NONE',  ( -24.85993732546052470, 9.902695843592100644, 9.181557340668950573 ) ) ;
#8167 = CARTESIAN_POINT ( 'NONE',  ( -0.8948477690461620337, -30.54755392045577622, 15.29677453898827721 ) ) ;
#8168 = CARTESIAN_POINT ( 'NONE',  ( -2.952869152607111136, 4.384817011589738911, 11.17020052527586138 ) ) ;
#8169 = EDGE_CURVE ( 'NONE', #47922, #35439, #57951, .T. ) ;
#8170 = CARTESIAN_POINT ( 'NONE',  ( 2.941278708680199916, -3.185832147968409966, -5.248410529370257649 ) ) ;
#8171 = FACE_OUTER_BOUND ( 'NONE', #45008, .T. ) ;
#8172 = DIRECTION ( 'NONE',  ( 1.000000000000000000, 0.000000000000000000, 0.000000000000000000 ) ) ;
#8173 = ORIENTED_EDGE ( 'NONE', *, *, #42942, .T. ) ;
#8174 = DIRECTION ( 'NONE',  ( -1.000000000000000000, 0.000000000000000000, 0.000000000000000000 ) ) ;
#8175 = EDGE_CURVE ( 'NONE', #46293, #56608, #60650, .T. ) ;
#8176 = CARTESIAN_POINT ( 'NONE',  ( -22.46509356695202086, -4.038408495643994733, 1.314379028669602656 ) ) ;
#8177 = DIRECTION ( 'NONE',  ( 1.000000000000000000, 0.000000000000000000, 0.000000000000000000 ) ) ;
#8178 = ORIENTED_EDGE ( 'NONE', *, *, #33995, .T. ) ;
#8179 = DIRECTION ( 'NONE',  ( 0.000000000000000000, 0.9868265225415254749, 0.1617819965527686199 ) ) ;
#8180 = EDGE_CURVE ( 'NONE', #9450, #19224, #22023, .T. ) ;
#8181 = ORIENTED_EDGE ( 'NONE', *, *, #51948, .F. ) ;
#8182 = CARTESIAN_POINT ( 'NONE',  ( 2.241526690369556984, -1.308664175663819762, 7.521460607153596989 ) ) ;
#8183 = CARTESIAN_POINT ( 'NONE',  ( 0.2648321136542702292, -10.53380804838493923, -6.245325033825842809 ) ) ;
#8184 = CARTESIAN_POINT ( 'NONE',  ( 5.515539859299206427, -0.003740028639278315456, -0.004759416711441667551 ) ) ;
#8185 = DIRECTION ( 'NONE',  ( 0.000000000000000000, -0.5767582926624851281, -0.8169148498130358593 ) ) ;
#8186 = CARTESIAN_POINT ( 'NONE',  ( -37.25000000000000711, -27.21021009056489603, 4.499999999999997335 ) ) ;
#8187 = LINE ( 'NONE', #2893, #3076 ) ;
#8188 = ADVANCED_FACE ( 'NONE', ( #1440 ), #47318, .T. ) ;
#8189 = B_SPLINE_CURVE_WITH_KNOTS ( 'NONE', 3,
 ( #36739, #6485, #41721, #33309, #8053, #57353, #48946, #57032, #21793, #58939, #26761, #52040, #59245, #47059, #1516, #42041, #2757, #62325 ),
 .UNSPECIFIED., .F., .F.,
 ( 4, 2, 2, 2, 2, 2, 2, 2, 4 ),
 ( 9.697399036122160616E-19, 0.002700019232399850349, 0.004050028848599774439, 0.005400038464799701565, 0.006075043272899665996, 0.006750048080999626089, 0.008100057697199548878, 0.009450067313399469066, 0.01080007692959938925 ),
 .UNSPECIFIED. ) ;
#8190 = CARTESIAN_POINT ( 'NONE',  ( 36.00000000000000711, 11.96656215839374937, 4.400442035670817376 ) ) ;
#8191 = VERTEX_POINT ( 'NONE', #12363 ) ;
#8192 = FACE_OUTER_BOUND ( 'NONE', #5999, .T. ) ;
#8193 = CIRCLE ( 'NONE', #38987, 5.000000000000000000 ) ;
#8194 = EDGE_CURVE ( 'NONE', #30859, #3157, #39424, .T. ) ;
#8195 = ORIENTED_EDGE ( 'NONE', *, *, #52209, .T. ) ;
#8196 = CARTESIAN_POINT ( 'NONE',  ( 1.198791140417948986, 3.806343609711437370, 11.96656299555031566 ) ) ;
#8197 = FACE_OUTER_BOUND ( 'NONE', #8914, .T. ) ;
#8198 = AXIS2_PLACEMENT_3D ( 'NONE', #29508, #38519, #38855 ) ;
#8199 = CARTESIAN_POINT ( 'NONE',  ( 1.000000000000000888, -0.8935325819929111901, 7.446583077151331942 ) ) ;
#8200 = LINE ( 'NONE', #44401, #23842 ) ;
#8201 = CARTESIAN_POINT ( 'NONE',  ( -27.94768133936596399, 13.15239037730114369, -3.102958909511970731 ) ) ;
#8202 = AXIS2_PLACEMENT_3D ( 'NONE', #11747, #32364, #56329 ) ;
#8203 = ADVANCED_FACE ( 'NONE', ( #42610 ), #62256, .T. ) ;
#8204 = VERTEX_POINT ( 'NONE', #12045 ) ;
#8205 = CARTESIAN_POINT ( 'NONE',  ( 0.3675815128205912052, 11.44679196252415210, -4.447030445008065769 ) ) ;
#8206 = LINE ( 'NONE', #28473, #53586 ) ;
#8207 = ADVANCED_FACE ( 'NONE', ( #62913 ), #41648, .T. ) ;
#8208 = CARTESIAN_POINT ( 'NONE',  ( 2.256373768223414178, 1.457292142211218611, 7.499124080223143807 ) ) ;
#8209 = CARTESIAN_POINT ( 'NONE',  ( 37.00000000000000711, 4.705694406421931860E-17, -3.469127814946512892E-15 ) ) ;
#8210 = ORIENTED_EDGE ( 'NONE', *, *, #43768, .F. ) ;
#8211 = CARTESIAN_POINT ( 'NONE',  ( 2.717984159218836737, -6.148373979318608740, -4.788867404453649002 ) ) ;
#8212 = CARTESIAN_POINT ( 'NONE',  ( -22.28694879868232803, -2.586016167700811330, 2.661377239830749808 ) ) ;
#8213 = CARTESIAN_POINT ( 'NONE',  ( 2.430348790457612207, -1.144258029164365142, 7.611893186157537627 ) ) ;
#8214 = DIRECTION ( 'NONE',  ( 0.000000000000000000, 0.000000000000000000, 1.000000000000000000 ) ) ;
#8215 = CARTESIAN_POINT ( 'NONE',  ( 2.260457164927189400, -0.1384509728648543325, -7.639515169785722648 ) ) ;
#8216 = CARTESIAN_POINT ( 'NONE',  ( -27.95869044047065799, -11.60004630023460948, -3.134771106759090653 ) ) ;
#8217 = EDGE_LOOP ( 'NONE', ( #42229, #3475, #9174, #36310 ) ) ;
#8218 = CARTESIAN_POINT ( 'NONE',  ( -27.08418179957658367, 1.713622993062713373, -1.521007404704320942 ) ) ;
#8219 = FACE_OUTER_BOUND ( 'NONE', #51325, .T. ) ;
#8220 = CARTESIAN_POINT ( 'NONE',  ( -10.55354650058127319, -33.11426855636985778, -11.57717840647777408 ) ) ;
#8221 = EDGE_LOOP ( 'NONE', ( #62924, #23988, #55913, #25592 ) ) ;
#8222 = CARTESIAN_POINT ( 'NONE',  ( 0.2646305136544072623, 12.08286001766535556, 1.996350543473035755 ) ) ;
#8223 = DIRECTION ( 'NONE',  ( 1.000000000000000000, 0.000000000000000000, 0.000000000000000000 ) ) ;
#8224 = CYLINDRICAL_SURFACE ( 'NONE', #5386, 2.809571291727933851 ) ;
#8225 = CYLINDRICAL_SURFACE ( 'NONE', #57268, 5.000000000000000888 ) ;
#8226 = CARTESIAN_POINT ( 'NONE',  ( 0.2671309869109498303, -11.45180222993658070, 4.340541005679486197 ) ) ;
#8227 = B_SPLINE_CURVE_WITH_KNOTS ( 'NONE', 3,
 ( #57154, #36182, #56488, #50532, #316, #16588 ),
 .UNSPECIFIED., .F., .F.,
 ( 4, 2, 4 ),
 ( 1.124229303124644401E-17, 0.001589257412050233947, 0.003178514824100456618 ),
 .UNSPECIFIED. ) ;
#8228 = CIRCLE ( 'NONE', #5056, 4.999999999999999112 ) ;
#8229 = EDGE_CURVE ( 'NONE', #46663, #14288, #49010, .T. ) ;
#8230 = LINE ( 'NONE', #64395, #55218 ) ;
#8231 = ORIENTED_EDGE ( 'NONE', *, *, #62800, .T. ) ;
#8232 = CARTESIAN_POINT ( 'NONE',  ( 2.255723233588949661, -7.222632368701285444, 2.488140745365843287 ) ) ;
#8233 = CARTESIAN_POINT ( 'NONE',  ( 37.00000000000000711, 10.14408668126221613, 5.921969905510239940 ) ) ;
#8234 = CARTESIAN_POINT ( 'NONE',  ( 1.719304012338836563, -7.017415949612288095, 10.62216384465580710 ) ) ;
#8235 = CARTESIAN_POINT ( 'NONE',  ( -27.35552965826137140, 0.2619431035392177365, -3.094132632038957276 ) ) ;
#8236 = LINE ( 'NONE', #3610, #24813 ) ;
#8237 = DIRECTION ( 'NONE',  ( 1.000000000000000000, 0.000000000000000000, 0.000000000000000000 ) ) ;
#8238 = CARTESIAN_POINT ( 'NONE',  ( 2.247112776671466250, 7.539676020705989856, 1.211104213045398614 ) ) ;
#8239 = CARTESIAN_POINT ( 'NONE',  ( 0.2648978790185584908, -1.996248716311547433, -12.08224454301450734 ) ) ;
#8240 = ORIENTED_EDGE ( 'NONE', *, *, #25913, .T. ) ;
#8241 = ORIENTED_EDGE ( 'NONE', *, *, #50522, .F. ) ;
#8242 = EDGE_CURVE ( 'NONE', #7848, #30956, #47948, .T. ) ;
#8243 = CARTESIAN_POINT ( 'NONE',  ( -19.04306142112764633, -4.598438116554168786, -11.08446069010050827 ) ) ;
#8244 = VERTEX_POINT ( 'NONE', #27657 ) ;
#8245 = VECTOR ( 'NONE', #29436, 1000.000000000000000 ) ;
#8246 = DIRECTION ( 'NONE',  ( 0.000000000000000000, 0.01356324068818000328, -0.9999080150203990547 ) ) ;
#8247 = CARTESIAN_POINT ( 'NONE',  ( -36.00000000000000711, 11.24036214326520700, 6.018036132182203346 ) ) ;
#8248 = EDGE_CURVE ( 'NONE', #40729, #41862, #51179, .T. ) ;
#8249 = CARTESIAN_POINT ( 'NONE',  ( -22.28629837673888048, -1.594277649056518475, 3.348758206500239254 ) ) ;
#8250 = EDGE_LOOP ( 'NONE', ( #63592, #15052, #49710, #39008 ) ) ;
#8251 = CARTESIAN_POINT ( 'NONE',  ( -35.04683013664716640, 0.01065093278707341523, -0.006266879427281896002 ) ) ;
#8252 = CARTESIAN_POINT ( 'NONE',  ( 2.244591118396555895, 6.558116599718226247, -3.910457279126638319 ) ) ;
#8253 = DIRECTION ( 'NONE',  ( -1.000000000000000000, -0.000000000000000000, 0.000000000000000000 ) ) ;
#8254 = EDGE_LOOP ( 'NONE', ( #14931, #59705, #39408, #23668 ) ) ;
#8255 = ORIENTED_EDGE ( 'NONE', *, *, #22119, .F. ) ;
#8256 = DIRECTION ( 'NONE',  ( 0.000000000000000000, -0.7617968321374811724, -0.6478160128812026075 ) ) ;
#8257 = EDGE_CURVE ( 'NONE', #46698, #22470, #51973, .T. ) ;
#8258 = EDGE_LOOP ( 'NONE', ( #49847, #494, #17576, #44556 ) ) ;
#8259 = CARTESIAN_POINT ( 'NONE',  ( 5.536195898058073439, -0.002666509901870014500, 0.008071068258923596792 ) ) ;
#8260 = VERTEX_POINT ( 'NONE', #991 ) ;
#8261 = ORIENTED_EDGE ( 'NONE', *, *, #49689, .T. ) ;
#8262 = DIRECTION ( 'NONE',  ( -0.9688695217174486674, 0.000000000000000000, 0.2475719085175094036 ) ) ;
#8263 = CARTESIAN_POINT ( 'NONE',  ( 0.000000000000000000, 0.000000000000000000, 0.000000000000000000 ) ) ;
#8264 = DIRECTION ( 'NONE',  ( 1.000000000000000000, 0.000000000000000000, -0.000000000000000000 ) ) ;
#8265 = DIRECTION ( 'NONE',  ( 0.000000000000000000, -0.01356324068817998940, 0.9999080150203990547 ) ) ;
#8266 = CARTESIAN_POINT ( 'NONE',  ( -28.66013792860432119, 1.306994062650338684, -1.289369452666814020 ) ) ;
#8267 = CARTESIAN_POINT ( 'NONE',  ( 2.889800649504073782, -0.06738247734046161341, -6.121013568931507720 ) ) ;
#8268 = VERTEX_POINT ( 'NONE', #40222 ) ;
#8269 = CARTESIAN_POINT ( 'NONE',  ( -36.00000000000000711, 3.473736367725253960, 12.26766708251992988 ) ) ;
#8270 = EDGE_CURVE ( 'NONE', #34013, #16747, #45892, .T. ) ;
#8271 = CARTESIAN_POINT ( 'NONE',  ( -15.83651567491729395, 7.907244717092745567, 9.026412348056238599 ) ) ;
#8272 = CARTESIAN_POINT ( 'NONE',  ( -37.00000000000000711, -4.074242145635923684, -12.08151691381194581 ) ) ;
#8273 = EDGE_CURVE ( 'NONE', #28113, #11187, #59663, .T. ) ;
#8274 = FACE_OUTER_BOUND ( 'NONE', #3188, .T. ) ;
#8275 = CARTESIAN_POINT ( 'NONE',  ( 2.889800649504073782, 5.334644486274195074, 3.002151847318935030 ) ) ;
#8276 = CARTESIAN_POINT ( 'NONE',  ( -22.65996813707689128, -4.292955455498915995, 2.220979297960717691 ) ) ;
#8277 = CARTESIAN_POINT ( 'NONE',  ( -37.00000000000000711, -7.745827850122939395, -10.12742074351904975 ) ) ;
#8278 = CARTESIAN_POINT ( 'NONE',  ( -36.00000000000000711, 9.621072037177118119, -8.366449238204259231 ) ) ;
#8279 = CARTESIAN_POINT ( 'NONE',  ( -35.00000000000000000, 6.102719229070827645, -10.54834585426213422 ) ) ;
#8280 = EDGE_CURVE ( 'NONE', #2269, #11657, #10809, .T. ) ;
#8281 = AXIS2_PLACEMENT_3D ( 'NONE', #16107, #25429, #55362 ) ;
#8282 = ORIENTED_EDGE ( 'NONE', *, *, #1904, .F. ) ;
#8283 = CARTESIAN_POINT ( 'NONE',  ( 0.2655924914740778187, 12.06787830249868243, -2.083162675473490655 ) ) ;
#8284 = EDGE_CURVE ( 'NONE', #50289, #3042, #47991, .T. ) ;
#8285 = EDGE_CURVE ( 'NONE', #47834, #27353, #20356, .T. ) ;
#8286 = AXIS2_PLACEMENT_3D ( 'NONE', #57771, #12188, #38106 ) ;
#8287 = ORIENTED_EDGE ( 'NONE', *, *, #37699, .T. ) ;
#8288 = CARTESIAN_POINT ( 'NONE',  ( -17.29244623348158783, 2.525873743887551814, 11.73115347397430597 ) ) ;
#8289 = DIRECTION ( 'NONE',  ( 1.000000000000000000, 0.000000000000000000, -0.000000000000000000 ) ) ;
#8290 = CARTESIAN_POINT ( 'NONE',  ( 12.82394711127995812, -12.76747887865895592, -4.390754480898809042 ) ) ;
#8291 = ADVANCED_FACE ( 'NONE', ( #41204 ), #34157, .T. ) ;
#8292 = AXIS2_PLACEMENT_3D ( 'NONE', #12742, #48677, #28702 ) ;
#8293 = CYLINDRICAL_SURFACE ( 'NONE', #8656, 6.936499999999988120 ) ;
#8294 = DIRECTION ( 'NONE',  ( 0.000000000000000000, 0.000000000000000000, -1.000000000000000000 ) ) ;
#8295 = ORIENTED_EDGE ( 'NONE', *, *, #47616, .F. ) ;
#8296 = CARTESIAN_POINT ( 'NONE',  ( 0.7400311444011681283, 10.56075429936776366, -6.506979270898069601 ) ) ;
#8297 = CARTESIAN_POINT ( 'NONE',  ( 2.276905613633648962, -3.688905863353259207, 6.697548486790754652 ) ) ;
#8298 = LINE ( 'NONE', #22951, #36457 ) ;
#8299 = VECTOR ( 'NONE', #53347, 1000.000000000000000 ) ;
#8300 = CARTESIAN_POINT ( 'NONE',  ( 1.104777566491147445, 2.644034362100695645, 12.24382064406180071 ) ) ;
#8301 = FACE_OUTER_BOUND ( 'NONE', #12643, .T. ) ;
#8302 = ORIENTED_EDGE ( 'NONE', *, *, #39948, .T. ) ;
#8303 = CARTESIAN_POINT ( 'NONE',  ( -35.00000000000000000, 9.063649021439076137, -8.146229107149299153 ) ) ;
#8304 = CARTESIAN_POINT ( 'NONE',  ( 1.104777566491144336, -8.411711248089032367, -9.281442536087567419 ) ) ;
#8305 = CARTESIAN_POINT ( 'NONE',  ( -7.613843340936869097, -31.56230424472492757, 13.96789312046862896 ) ) ;
#8306 = ADVANCED_FACE ( 'NONE', ( #46229 ), #51222, .T. ) ;
#8307 = ORIENTED_EDGE ( 'NONE', *, *, #36235, .F. ) ;
#8308 = ORIENTED_EDGE ( 'NONE', *, *, #998, .T. ) ;
#8309 = CARTESIAN_POINT ( 'NONE',  ( -9.656847648909668180, 11.20398564923865514, -7.540956407560663877 ) ) ;
#8310 = ORIENTED_EDGE ( 'NONE', *, *, #52355, .T. ) ;
#8311 = DIRECTION ( 'NONE',  ( 0.000000000000000000, 0.01356324068817991828, -0.9999080150203990547 ) ) ;
#8312 = CARTESIAN_POINT ( 'NONE',  ( 2.963017218115620910, -3.599595431209440477, -7.004145770368809920 ) ) ;
#8313 = CARTESIAN_POINT ( 'NONE',  ( -27.09229696323320624, -1.666734935099465131, -1.607344345646473327 ) ) ;
#8315 = CARTESIAN_POINT ( 'NONE',  ( 0.2739690278137274504, 9.264642836915941260, -8.012873994335592442 ) ) ;
#8314 = VECTOR ( 'NONE', #58752, 1000.000000000000000 ) ;
#8316 = CARTESIAN_POINT ( 'NONE',  ( 2.889800649504073782, 0.9965440656173724099, 6.039722463373542460 ) ) ;
#8317 = EDGE_LOOP ( 'NONE', ( #26160, #54050, #46617, #4666 ) ) ;
#8318 = ADVANCED_FACE ( 'NONE', ( #61489 ), #33605, .F. ) ;
#8319 = ORIENTED_EDGE ( 'NONE', *, *, #39280, .T. ) ;
#8320 = ORIENTED_EDGE ( 'NONE', *, *, #43153, .T. ) ;
#8321 = CARTESIAN_POINT ( 'NONE',  ( 2.261269890822072082, 7.226741992146827442, -2.481875047312865679 ) ) ;
#8322 = FACE_OUTER_BOUND ( 'NONE', #43467, .T. ) ;
#8323 = VERTEX_POINT ( 'NONE', #50879 ) ;
#8324 = DIRECTION ( 'NONE',  ( 1.000000000000000000, 0.000000000000000000, -0.000000000000000000 ) ) ;
#8325 = CARTESIAN_POINT ( 'NONE',  ( -22.27945548916780183, -0.3299677273100632968, -3.673577025288763398 ) ) ;
#8326 = ORIENTED_EDGE ( 'NONE', *, *, #7656, .T. ) ;
#8327 = AXIS2_PLACEMENT_3D ( 'NONE', #18500, #64649, #12807 ) ;
#8328 = CARTESIAN_POINT ( 'NONE',  ( 3.047904605210400408, 7.270585891216620134, 3.098478597269316737 ) ) ;
#8329 = CARTESIAN_POINT ( 'NONE',  ( 2.256373768223415510, -2.737361830682274899, -7.132139410180991845 ) ) ;
#8330 = CARTESIAN_POINT ( 'NONE',  ( -27.08429572838383947, -2.208905845566027537, -0.6096735944848257205 ) ) ;
#8331 = VERTEX_POINT ( 'NONE', #9985 ) ;
#8332 = ORIENTED_EDGE ( 'NONE', *, *, #36311, .F. ) ;
#8333 = AXIS2_PLACEMENT_3D ( 'NONE', #45899, #9991, #9638 ) ;
#8334 = UNCERTAINTY_MEASURE_WITH_UNIT (LENGTH_MEASURE( 1.000000000000000082E-05 ), #22219, 'distance_accuracy_value', 'NONE');
#8335 = EDGE_CURVE ( 'NONE', #311, #59495, #6559, .T. ) ;
#8336 = VERTEX_POINT ( 'NONE', #16283 ) ;
#8337 = CARTESIAN_POINT ( 'NONE',  ( -19.88622662114644513, 11.70525051340494116, -2.725500476031548658 ) ) ;
#8338 = ORIENTED_EDGE ( 'NONE', *, *, #9405, .T. ) ;
#8339 = VECTOR ( 'NONE', #48851, 1000.000000000000000 ) ;
#8340 = CARTESIAN_POINT ( 'NONE',  ( 0.3675815128205894289, -8.093875121226016489, -9.235491948680088825 ) ) ;
#8341 = CARTESIAN_POINT ( 'NONE',  ( 0.2653141617321020385, 11.49253039221382444, 4.229807441322350314 ) ) ;
#8342 = DIRECTION ( 'NONE',  ( 0.3865475372811021382, -0.7888450329201742717, -0.4778122177792066827 ) ) ;
#8343 = LINE ( 'NONE', #49264, #41237 ) ;
#8344 = CARTESIAN_POINT ( 'NONE',  ( -47.00000000000000711, 0.000000000000000000, 0.000000000000000000 ) ) ;
#8345 = CARTESIAN_POINT ( 'NONE',  ( 1.719304012338199517, 0.000000000000000000, 0.000000000000000000 ) ) ;
#8346 = ORIENTED_EDGE ( 'NONE', *, *, #60729, .F. ) ;
#8347 = CARTESIAN_POINT ( 'NONE',  ( 2.245754705088392811, -7.136529175883343790, -2.715960966012167521 ) ) ;
#8348 =( BOUNDED_SURFACE ( )  B_SPLINE_SURFACE ( 3, 1, ( 
 ( #34141, #64398 ),
 ( #8551, #39458 ),
 ( #29178, #59422 ),
 ( #43808, #12888 ) ),
 .UNSPECIFIED., .F., .F., .F. ) 
 B_SPLINE_SURFACE_WITH_KNOTS ( ( 4, 4 ),
 ( 2, 2 ),
 ( 0.000000000000000000, 1.000000000000000000 ),
 ( 0.000000000000000000, 1.000000000000000000 ),
 .UNSPECIFIED. ) 
 GEOMETRIC_REPRESENTATION_ITEM ( )  RATIONAL_B_SPLINE_SURFACE ( (
 ( 1.000000000000000000, 1.000000000000000000),
 ( 0.9942764183789327692, 0.8450855930916580938),
 ( 0.9942764183789327692, 0.8450855930916580938),
 ( 1.000000000000000000, 1.000000000000000000) ) ) 
 REPRESENTATION_ITEM ( '' )  SURFACE ( )  );
#8349 = ORIENTED_EDGE ( 'NONE', *, *, #27664, .T. ) ;
#8350 = DIRECTION ( 'NONE',  ( 0.000000000000000000, 0.000000000000000000, 1.000000000000000000 ) ) ;
#8351 = CARTESIAN_POINT ( 'NONE',  ( -17.85139933901853482, -6.218234000768075198, -11.98572918122005326 ) ) ;
#8352 = ORIENTED_EDGE ( 'NONE', *, *, #51041, .F. ) ;
#8353 = CARTESIAN_POINT ( 'NONE',  ( -35.00000000000000000, -3.916263239775430005, 11.07407352312211302 ) ) ;
#8354 = CARTESIAN_POINT ( 'NONE',  ( 3.152665057735335452, -7.719888720907720270, 1.848755561853250295 ) ) ;
#8355 = EDGE_CURVE ( 'NONE', #13777, #43254, #25942, .T. ) ;
#8356 = EDGE_CURVE ( 'NONE', #14146, #21447, #63576, .T. ) ;
#8357 = VERTEX_POINT ( 'NONE', #20281 ) ;
#8358 = AXIS2_PLACEMENT_3D ( 'NONE', #21630, #7289, #6665 ) ;
#8359 = VERTEX_POINT ( 'NONE', #43172 ) ;
#8360 = CARTESIAN_POINT ( 'NONE',  ( -25.00000000000000355, -9.999999999999998224, 5.000000000000000888 ) ) ;
#8361 = EDGE_CURVE ( 'NONE', #53066, #56700, #16613, .T. ) ;
#8362 = AXIS2_PLACEMENT_3D ( 'NONE', #65649, #50718, #61020 ) ;
#8363 = ORIENTED_EDGE ( 'NONE', *, *, #35824, .T. ) ;
#8364 = CARTESIAN_POINT ( 'NONE',  ( 3.152665057736217413, -7.923639299008909731, 0.4801242025612903475 ) ) ;
#8365 = CARTESIAN_POINT ( 'NONE',  ( -27.08429572838383947, 2.208905845566027537, 0.6096735944847788691 ) ) ;
#8366 = ADVANCED_FACE ( 'NONE', ( #53166, #27555 ), #32528, .F. ) ;
#8367 = FACE_OUTER_BOUND ( 'NONE', #5121, .T. ) ;
#8368 = DIRECTION ( 'NONE',  ( -1.000000000000000000, 0.000000000000000000, 0.000000000000000000 ) ) ;
#8369 = VERTEX_POINT ( 'NONE', #36883 ) ;
#8370 = CARTESIAN_POINT ( 'NONE',  ( 2.903928887688475680, -7.845932231841446836, -3.918141038919469299 ) ) ;
#8371 = VECTOR ( 'NONE', #60159, 1000.000000000000000 ) ;
#8372 = B_SPLINE_CURVE_WITH_KNOTS ( 'NONE', 3,
 ( #9354, #29639, #56229, #24333, #65538, #45595 ),
 .UNSPECIFIED., .F., .F.,
 ( 4, 2, 4 ),
 ( 0.0001654224980408687486, 0.0006219428995476670432, 0.001078463301054465419 ),
 .UNSPECIFIED. ) ;
#8373 = VECTOR ( 'NONE', #41650, 1000.000000000000114 ) ;
#8374 = CIRCLE ( 'NONE', #15655, 12.18650000000000055 ) ;
#8375 = CARTESIAN_POINT ( 'NONE',  ( 2.770579946183332254, -7.633739187313462793, -1.653873933978953215 ) ) ;
#8376 = CARTESIAN_POINT ( 'NONE',  ( 23.64999694718868994, 11.46135651385800180, -7.139647639458894801 ) ) ;
#8378 = AXIS2_PLACEMENT_3D ( 'NONE', #20935, #36571, #10974 ) ;
#8377 = CARTESIAN_POINT ( 'NONE',  ( -27.08418179957658367, -0.7235373421492636847, 2.174042548349516935 ) ) ;
#8379 = CARTESIAN_POINT ( 'NONE',  ( 35.00000000000000000, -2.968224442958486975, -11.81949347079746282 ) ) ;
#8380 = CARTESIAN_POINT ( 'NONE',  ( 4.199947675780304479, -10.87007255795022687, -5.085750118326637370 ) ) ;
#8381 = CARTESIAN_POINT ( 'NONE',  ( -22.28284753389937123, -2.640101649307533549, -2.590196335759745061 ) ) ;
#8382 = CIRCLE ( 'NONE', #16875, 12.75000000000000178 ) ;
#8383 = EDGE_CURVE ( 'NONE', #21953, #40162, #45849, .T. ) ;
#8384 = ORIENTED_EDGE ( 'NONE', *, *, #54436, .F. ) ;
#8385 = CARTESIAN_POINT ( 'NONE',  ( 12.29300949244506924, -11.61203561930438255, -3.031982959488972451 ) ) ;
#8386 = ADVANCED_FACE ( 'NONE', ( #12924 ), #12575, .T. ) ;
#8387 = ORIENTED_EDGE ( 'NONE', *, *, #8556, .F. ) ;
#8388 = CARTESIAN_POINT ( 'NONE',  ( 0.3675815128205894289, 1.872154644482245889, -12.13672785388548547 ) ) ;
#8389 = CARTESIAN_POINT ( 'NONE',  ( -22.27711351828769892, -3.575417021793780403, 0.8770428151440453624 ) ) ;
#8390 = DIRECTION ( 'NONE',  ( -0.000000000000000000, -1.000000000000000000, -0.000000000000000000 ) ) ;
#8391 = ORIENTED_EDGE ( 'NONE', *, *, #44195, .F. ) ;
#8392 = EDGE_CURVE ( 'NONE', #3042, #53140, #30984, .T. ) ;
#8393 = ORIENTED_EDGE ( 'NONE', *, *, #34457, .F. ) ;
#8394 = EDGE_LOOP ( 'NONE', ( #34428, #34153, #46518, #33358 ) ) ;
#8395 = CARTESIAN_POINT ( 'NONE',  ( 35.00000000000000000, 11.10408318471059275, -6.265926637539534383 ) ) ;
#8396 = CARTESIAN_POINT ( 'NONE',  ( -22.71097035706202405, -0.4203397252017116448, 4.965150228107737540 ) ) ;
#8397 = AXIS2_PLACEMENT_3D ( 'NONE', #369, #6335, #5696 ) ;
#8398 = EDGE_LOOP ( 'NONE', ( #237, #42494, #6518, #15555 ) ) ;
#8399 = CARTESIAN_POINT ( 'NONE',  ( 2.000000000000001776, 5.217815162096925086, -5.387430271863535403 ) ) ;
#8400 = DIRECTION ( 'NONE',  ( 0.000000000000000000, -1.000000000000000000, 0.000000000000000000 ) ) ;
#8401 = CARTESIAN_POINT ( 'NONE',  ( 5.515539859299206427, 0.0001942659352250529969, 0.006049968793488821710 ) ) ;
#8402 = CARTESIAN_POINT ( 'NONE',  ( 5.514624014163232779, 0.003498325728817810402, -0.002216125254993677428 ) ) ;
#8403 = ORIENTED_EDGE ( 'NONE', *, *, #9586, .F. ) ;
#8404 = CARTESIAN_POINT ( 'NONE',  ( -22.00000000000000711, -20.00000000000000000, -1.499999999999998002 ) ) ;
#8405 = AXIS2_PLACEMENT_3D ( 'NONE', #57860, #51566, #11945 ) ;
#8406 = CARTESIAN_POINT ( 'NONE',  ( 19.27363075669222425, -28.98570064806743929, 5.846556568011616939 ) ) ;
#8407 = CARTESIAN_POINT ( 'NONE',  ( 2.276905613633650738, -1.479235344773113026, -7.501802783089495108 ) ) ;
#8409 = ORIENTED_EDGE ( 'NONE', *, *, #56311, .T. ) ;
#8408 = CARTESIAN_POINT ( 'NONE',  ( -47.00000000000000711, 0.000000000000000000, 0.000000000000000000 ) ) ;
#8410 = CARTESIAN_POINT ( 'NONE',  ( 0.2638984909335716500, -12.09426044257625321, 1.930290337334017226 ) ) ;
#8411 = ADVANCED_FACE ( 'NONE', ( #11609 ), #47852, .T. ) ;
#8412 = ADVANCED_FACE ( 'NONE', ( #1972 ), #31878, .T. ) ;
#8413 = ORIENTED_EDGE ( 'NONE', *, *, #33263, .F. ) ;
#8414 = CARTESIAN_POINT ( 'NONE',  ( -18.32962124502519075, 13.49796943741737998, 0.4155283434849697533 ) ) ;
#8415 = VERTEX_POINT ( 'NONE', #33203 ) ;
#8416 = CARTESIAN_POINT ( 'NONE',  ( 2.241352910868909643, 7.202080440908774861, -2.532612177304371048 ) ) ;
#8418 = CARTESIAN_POINT ( 'NONE',  ( 0.2648978790185593790, 4.063980959785203240, -11.55204314799259890 ) ) ;
#8417 = VECTOR ( 'NONE', #33803, 1000.000000000000000 ) ;
#8419 = EDGE_CURVE ( 'NONE', #31240, #46276, #7646, .T. ) ;
#8420 = AXIS2_PLACEMENT_3D ( 'NONE', #62045, #25815, #65689 ) ;
#8421 = CARTESIAN_POINT ( 'NONE',  ( -35.00000000000000000, -12.38385022362079724, -3.033604067594711129 ) ) ;
#8422 = CARTESIAN_POINT ( 'NONE',  ( 35.00000000000000000, 11.72195762423409704, 0.7536123767498881243 ) ) ;
#8423 = CARTESIAN_POINT ( 'NONE',  ( 0.2872850955227739256, 9.519656861923731839, 7.715220952083274852 ) ) ;
#8424 = CARTESIAN_POINT ( 'NONE',  ( -8.564638015981364205, -2.705928108065259963, -13.22659762878139489 ) ) ;
#8425 = CARTESIAN_POINT ( 'NONE',  ( -27.20164183316781248, -2.237540722393157377, 1.409601201084047517 ) ) ;
#8426 = AXIS2_PLACEMENT_3D ( 'NONE', #60144, #33578, #54184 ) ;
#8427 = EDGE_LOOP ( 'NONE', ( #19788, #32032, #48692, #42465 ) ) ;
#8428 = CARTESIAN_POINT ( 'NONE',  ( 5.536195898058073439, -0.004468797463753835728, -0.007230647766619673761 ) ) ;
#8429 = ORIENTED_EDGE ( 'NONE', *, *, #36728, .F. ) ;
#8430 = VERTEX_POINT ( 'NONE', #37197 ) ;
#8431 = CARTESIAN_POINT ( 'NONE',  ( 0.4613984246114872789, 1.858723191796632923, -12.17044190070615350 ) ) ;
#8432 = CARTESIAN_POINT ( 'NONE',  ( -22.28121537037577227, 3.345440028056700488, 1.565596675942127147 ) ) ;
#8433 = AXIS2_PLACEMENT_3D ( 'NONE', #28602, #47917, #17332 ) ;
#8434 = CYLINDRICAL_SURFACE ( 'NONE', #44550, 12.18649999999999878 ) ;
#8435 = DIRECTION ( 'NONE',  ( 0.000000000000000000, -0.9985334138511233748, -0.05413890858542835804 ) ) ;
#8436 = CARTESIAN_POINT ( 'NONE',  ( 0.3665391374699465965, -10.76665847464308534, -5.911453292029717588 ) ) ;
#8437 = ADVANCED_FACE ( 'NONE', ( #2310, #22242, #16932 ), #41873, .F. ) ;
#8438 = DIRECTION ( 'NONE',  ( 0.000000000000000000, -0.01356324068817991828, 0.9999080150203990547 ) ) ;
#8439 = DIRECTION ( 'NONE',  ( 0.000000000000000000, -0.01356324068817998940, 0.9999080150203990547 ) ) ;
#8440 = ADVANCED_FACE ( 'NONE', ( #17268 ), #37545, .T. ) ;
#8441 = ORIENTED_EDGE ( 'NONE', *, *, #44678, .T. ) ;
#8442 = CARTESIAN_POINT ( 'NONE',  ( 2.889800649504073782, 6.121013568931506832, -0.06738247734052572879 ) ) ;
#8443 = CARTESIAN_POINT ( 'NONE',  ( 2.262775599886259315, -5.761998514039089692, -5.019217486251096538 ) ) ;
#8444 = CARTESIAN_POINT ( 'NONE',  ( 2.000000000000001776, 6.664893814313781029, -3.439359016433444438 ) ) ;
#8445 = B_SPLINE_CURVE_WITH_KNOTS ( 'NONE', 3,
 ( #40307, #25686, #45978, #39667, #24708, #30351, #50965, #46307, #30995, #54957, #60273, #60602, #29670, #15684, #14387, #15039, #49977, #4779, #44986, #39989, #14695, #9725, #30014, #432, #40978, #50325 ),
 .UNSPECIFIED., .F., .F.,
 ( 4, 2, 2, 2, 2, 2, 2, 2, 2, 2, 2, 2, 4 ),
 ( 0.000000000000000000, 0.001329167301762024245, 0.001993750952643036367, 0.002658334603524048489, 0.003322918254405061913, 0.003987501905286075336, 0.004652085556167088326, 0.005316669207048102183, 0.005981252857929116040, 0.006645836508810130765, 0.007975003810572164550, 0.009304171112334199203, 0.01063333841409623212 ),
 .UNSPECIFIED. ) ;
#8446 = CYLINDRICAL_SURFACE ( 'NONE', #44093, 4.999999999999999112 ) ;
#8447 = DIRECTION ( 'NONE',  ( 0.000000000000000000, 0.01356324068817998940, -0.9999080150203990547 ) ) ;
#8448 = AXIS2_PLACEMENT_3D ( 'NONE', #59484, #19253, #44188 ) ;
#8449 = EDGE_CURVE ( 'NONE', #21988, #62960, #64409, .T. ) ;
#8450 = CIRCLE ( 'NONE', #32714, 12.75000000000000178 ) ;
#8451 = CARTESIAN_POINT ( 'NONE',  ( 37.00000000000000711, 10.84030624090615724, 6.711949091238026632 ) ) ;
#8452 = CARTESIAN_POINT ( 'NONE',  ( 10.87910344070132140, 1.037424946074062992, -11.95562161342227192 ) ) ;
#8453 = ORIENTED_EDGE ( 'NONE', *, *, #59775, .T. ) ;
#8454 = CARTESIAN_POINT ( 'NONE',  ( 2.305787727787084851, -1.493241775258474124, 7.508843116234150905 ) ) ;
#8455 = CARTESIAN_POINT ( 'NONE',  ( 0.000000000000000000, 1.865193240757184290, -6.552473556515182374 ) ) ;
#8456 = CARTESIAN_POINT ( 'NONE',  ( -22.71097035706202760, -2.118550233809395777, -4.510116093748293586 ) ) ;
#8457 = CARTESIAN_POINT ( 'NONE',  ( -37.00000000000000711, 8.235637554476644695, 9.733281772932190989 ) ) ;
#8458 = DIRECTION ( 'NONE',  ( -1.000000000000000000, 0.000000000000000000, -0.000000000000000000 ) ) ;
#8459 = VECTOR ( 'NONE', #18783, 1000.000000000000000 ) ;
#8460 = ADVANCED_FACE ( 'NONE', ( #22918 ), #21928, .F. ) ;
#8461 = VERTEX_POINT ( 'NONE', #38178 ) ;
#8462 = CARTESIAN_POINT ( 'NONE',  ( 5.515539859299206427, 0.0008592514567752934825, -0.005991790098944302714 ) ) ;
#8463 = CARTESIAN_POINT ( 'NONE',  ( 0.3160775863651099638, -12.11619190710940330, 1.892533050396128402 ) ) ;
#8464 = LINE ( 'NONE', #33726, #44567 ) ;
#8465 = ORIENTED_EDGE ( 'NONE', *, *, #6538, .T. ) ;
#8466 = CARTESIAN_POINT ( 'NONE',  ( 0.2834382757447992951, 2.326926314863310363, 12.02923522794682931 ) ) ;
#8467 = CARTESIAN_POINT ( 'NONE',  ( 0.2651627923886316074, -4.105544202112473506, -11.53745192040746836 ) ) ;
#8468 = ORIENTED_EDGE ( 'NONE', *, *, #884, .T. ) ;
#8469 = ORIENTED_EDGE ( 'NONE', *, *, #23736, .T. ) ;
#8470 = CYLINDRICAL_SURFACE ( 'NONE', #50180, 5.000000000000000888 ) ;
#8471 = ADVANCED_FACE ( 'NONE', ( #11933 ), #50719, .T. ) ;
#8472 = ORIENTED_EDGE ( 'NONE', *, *, #48669, .T. ) ;
#8473 = CARTESIAN_POINT ( 'NONE',  ( 0.8375941296801562297, -12.17542732751302204, -2.537217542322243613 ) ) ;
#8474 = DIRECTION ( 'NONE',  ( -1.000000000000000000, 0.000000000000000000, 0.000000000000000000 ) ) ;
#8475 = CYLINDRICAL_SURFACE ( 'NONE', #65177, 12.18649999999999878 ) ;
#8476 = CARTESIAN_POINT ( 'NONE',  ( 2.889800649504073782, 5.774917447013026006, -2.030191121417079358 ) ) ;
#8477 = DIRECTION ( 'NONE',  ( 0.000000000000000000, -0.4698238015817236546, -0.8827602140260383257 ) ) ;
#8479 = ORIENTED_EDGE ( 'NONE', *, *, #17635, .T. ) ;
#8478 = CARTESIAN_POINT ( 'NONE',  ( 1.375507693217270067, 7.647735792765331553, 10.03411718356051807 ) ) ;
#8480 = DIRECTION ( 'NONE',  ( 0.000000000000000000, -0.01356324068817998940, 0.9999080150203990547 ) ) ;
#8481 = ORIENTED_EDGE ( 'NONE', *, *, #25043, .T. ) ;
#8482 = DIRECTION ( 'NONE',  ( -1.000000000000000000, 0.000000000000000000, 0.000000000000000000 ) ) ;
#8483 = ORIENTED_EDGE ( 'NONE', *, *, #64611, .F. ) ;
#8484 = ORIENTED_EDGE ( 'NONE', *, *, #49874, .F. ) ;
#8485 = CARTESIAN_POINT ( 'NONE',  ( -27.10931547487525251, 12.25599567157371439, 5.660530150648361847 ) ) ;
#8486 = CARTESIAN_POINT ( 'NONE',  ( -6.246056400524789609, -31.23659747722503610, 14.42616998329125089 ) ) ;
#8487 = CARTESIAN_POINT ( 'NONE',  ( -4.033318401586639013, 9.047516634271627112, 7.886307366337261371 ) ) ;
#8488 = DIRECTION ( 'NONE',  ( -1.000000000000000000, 0.000000000000000000, 0.000000000000000000 ) ) ;
#8489 = CARTESIAN_POINT ( 'NONE',  ( 3.347841273039249721, -10.61118957148187825, -5.603807266321158664 ) ) ;
#8490 = CARTESIAN_POINT ( 'NONE',  ( -41.00000000000000711, -1.694065894508793271E-18, 4.500000000000001776 ) ) ;
#8491 = VERTEX_POINT ( 'NONE', #8583 ) ;
#8492 = LINE ( 'NONE', #28778, #11327 ) ;
#8493 = VERTEX_POINT ( 'NONE', #13260 ) ;
#8494 = CARTESIAN_POINT ( 'NONE',  ( -25.00000000000000355, -30.00000000000000000, 1.530808498934191521E-15 ) ) ;
#8495 = DIRECTION ( 'NONE',  ( 1.000000000000000000, -0.000000000000000000, 0.000000000000000000 ) ) ;
#8496 = DIRECTION ( 'NONE',  ( 0.000000000000000000, 0.01356324068817998940, -0.9999080150203989437 ) ) ;
#8497 = B_SPLINE_CURVE_WITH_KNOTS ( 'NONE', 3,
 ( #34266, #29285, #18345, #33619, #38607, #64208, #9002, #43249 ),
 .UNSPECIFIED., .F., .F.,
 ( 4, 2, 2, 4 ),
 ( 4.010449034101563893E-18, 0.0003639104015150034324, 0.0007278208030300028532, 0.001455641606060006791 ),
 .UNSPECIFIED. ) ;
#8498 = ORIENTED_EDGE ( 'NONE', *, *, #37915, .T. ) ;
#8499 = CARTESIAN_POINT ( 'NONE',  ( 0.000000000000000000, 5.457833520448658327, 4.281014542496528463 ) ) ;
#8500 = DIRECTION ( 'NONE',  ( 0.000000000000000000, 0.1764146379942750364, 0.9843159429275484262 ) ) ;
#8501 = DIRECTION ( 'NONE',  ( 0.000000000000000000, 0.000000000000000000, 1.000000000000000000 ) ) ;
#8503 = VECTOR ( 'NONE', #41097, 1000.000000000000114 ) ;
#8502 = CARTESIAN_POINT ( 'NONE',  ( -22.30078715814471835, 3.111489293522213373, -2.097357782488221023 ) ) ;
#8504 = CARTESIAN_POINT ( 'NONE',  ( -10.00000000000000178, 0.000000000000000000, 0.000000000000000000 ) ) ;
#8505 = DIRECTION ( 'NONE',  ( 1.000000000000000000, 0.000000000000000000, 0.000000000000000000 ) ) ;
#8506 = FACE_OUTER_BOUND ( 'NONE', #41069, .T. ) ;
#8507 = ORIENTED_EDGE ( 'NONE', *, *, #60621, .T. ) ;
#8508 = ORIENTED_EDGE ( 'NONE', *, *, #2763, .T. ) ;
#8509 = DIRECTION ( 'NONE',  ( 0.000000000000000000, -0.1118654143051476951, -0.9937233664769775654 ) ) ;
#8510 = DIRECTION ( 'NONE',  ( 0.000000000000000000, 0.6943713148249639477, -0.7196168960969794304 ) ) ;
#8511 = CIRCLE ( 'NONE', #12773, 12.74999999999999822 ) ;
#8512 = CARTESIAN_POINT ( 'NONE',  ( 0.2653519991613803586, -11.50013121838206054, -4.209134909048866113 ) ) ;
#8513 = EDGE_CURVE ( 'NONE', #47206, #26332, #21451, .T. ) ;
#8514 = CARTESIAN_POINT ( 'NONE',  ( 35.00000000000000000, -11.61976888909157246, -3.827969819614423841 ) ) ;
#8515 = CARTESIAN_POINT ( 'NONE',  ( 5.516018279890452902, -0.005331956019561682678, 0.004180585980735035401 ) ) ;
#8516 = AXIS2_PLACEMENT_3D ( 'NONE', #27244, #22926, #7965 ) ;
#8517 = CARTESIAN_POINT ( 'NONE',  ( 3.459614771489464946, -11.09853614738469396, -7.685863346768205595 ) ) ;
#8518 = CARTESIAN_POINT ( 'NONE',  ( 37.00000000000000711, -11.10408318471055011, 6.265926637539605437 ) ) ;
#8519 = CARTESIAN_POINT ( 'NONE',  ( 3.152665057736003362, 6.378477742801834438, 4.725420687649379836 ) ) ;
#8520 = CARTESIAN_POINT ( 'NONE',  ( 0.000000000000000000, 0.000000000000000000, -2.999999999999995559 ) ) ;
#8521 = ORIENTED_EDGE ( 'NONE', *, *, #24959, .T. ) ;
#8522 = DIRECTION ( 'NONE',  ( 0.000000000000000000, 0.7381862504171926576, -0.6745969609292691294 ) ) ;
#8523 = CARTESIAN_POINT ( 'NONE',  ( -22.27756824490284160, -2.608445836294056797, 2.599719761044740896 ) ) ;
#8524 = CARTESIAN_POINT ( 'NONE',  ( 35.00000000000000000, -12.09831040184922912, 1.463443770872898453 ) ) ;
#8525 = AXIS2_PLACEMENT_3D ( 'NONE', #65757, #50511, #36835 ) ;
#8526 = EDGE_CURVE ( 'NONE', #6060, #6053, #48550, .T. ) ;
#8527 = AXIS2_PLACEMENT_3D ( 'NONE', #5856, #25446, #35732 ) ;
#8528 = AXIS2_PLACEMENT_3D ( 'NONE', #8804, #64965, #19442 ) ;
#8529 = CARTESIAN_POINT ( 'NONE',  ( -27.08416974970326052, -0.4041872645907051420, -2.255186831366117417 ) ) ;
#8530 = CARTESIAN_POINT ( 'NONE',  ( 2.241352910868908310, -5.901537464758487062, 4.843133558968109043 ) ) ;
#8531 = EDGE_CURVE ( 'NONE', #8602, #1479, #20455, .T. ) ;
#8532 =( BOUNDED_SURFACE ( )  B_SPLINE_SURFACE ( 3, 1, ( 
 ( #257, #15524 ),
 ( #46143, #35791 ),
 ( #40130, #36118 ),
 ( #15202, #14848 ) ),
 .UNSPECIFIED., .F., .F., .T. ) 
 B_SPLINE_SURFACE_WITH_KNOTS ( ( 4, 4 ),
 ( 2, 2 ),
 ( 0.000000000000000000, 1.000000000000000000 ),
 ( 0.000000000000000000, 1.000000000000000000 ),
 .UNSPECIFIED. ) 
 GEOMETRIC_REPRESENTATION_ITEM ( )  RATIONAL_B_SPLINE_SURFACE ( (
 ( 1.000000000000000000, 1.000000000000000000),
 ( 0.6933888150995267674, 0.9895912004443193632),
 ( 0.6933888150995267674, 0.9895912004443193632),
 ( 1.000000000000000000, 1.000000000000000000) ) ) 
 REPRESENTATION_ITEM ( '' )  SURFACE ( )  );
#8533 = ORIENTED_EDGE ( 'NONE', *, *, #8643, .T. ) ;
#8534 = EDGE_CURVE ( 'NONE', #56493, #22570, #8918, .T. ) ;
#8535 = DIRECTION ( 'NONE',  ( 0.000000000000000000, -0.6943713148249534006, 0.7196168960969896444 ) ) ;
#8536 = FACE_OUTER_BOUND ( 'NONE', #30578, .T. ) ;
#8537 = CARTESIAN_POINT ( 'NONE',  ( -6.778443870680312067, -26.22850392868687663, -14.88193859458597856 ) ) ;
#8538 = ORIENTED_EDGE ( 'NONE', *, *, #20735, .F. ) ;
#8539 = EDGE_CURVE ( 'NONE', #47422, #60037, #59598, .T. ) ;
#8540 = CARTESIAN_POINT ( 'NONE',  ( -11.23710731435352983, -5.993765267744247005, -12.10435126123341654 ) ) ;
#8541 = CARTESIAN_POINT ( 'NONE',  ( 36.00000000000000711, -12.66641127287626745, -1.457575200925504300 ) ) ;
#8542 = LINE ( 'NONE', #43452, #45574 ) ;
#8543 = CARTESIAN_POINT ( 'NONE',  ( 0.2956976708475416160, -8.045468685196979663, 9.245952174682525282 ) ) ;
#8544 = B_SPLINE_CURVE_WITH_KNOTS ( 'NONE', 3,
 ( #27442, #12802, #28119, #31768, #42078, #62358, #47429, #48082, #2864, #1864, #42727, #33090, #47102, #7486, #17488, #1557, #21831, #37760, #58053 ),
 .UNSPECIFIED., .F., .F.,
 ( 4, 3, 3, 3, 3, 3, 4 ),
 ( 7.566340834308382272E-18, 4.457896483014924563E-05, 6.639290541542123701E-05, 8.820687556479044501E-05, 0.0001100173248778947826, 0.0001545671401658086329, 0.0001830328308068585768 ),
 .UNSPECIFIED. ) ;
#8545 = CARTESIAN_POINT ( 'NONE',  ( 37.00000000000000711, 4.705694406421931860E-17, -3.469127814946512892E-15 ) ) ;
#8546 = CIRCLE ( 'NONE', #1161, 12.74999999999999822 ) ;
#8547 = EDGE_CURVE ( 'NONE', #45693, #53897, #15121, .T. ) ;
#8548 = CARTESIAN_POINT ( 'NONE',  ( 35.00000000000000000, 4.705694406421931860E-17, -3.469127814946512892E-15 ) ) ;
#8549 = ORIENTED_EDGE ( 'NONE', *, *, #3625, .F. ) ;
#8550 = CARTESIAN_POINT ( 'NONE',  ( -22.71097035706202405, 0.4203397252017515573, -4.965150228107761521 ) ) ;
#8551 = CARTESIAN_POINT ( 'NONE',  ( 5.515188684475870851, -0.001485678338381548735, 0.005140903460551581733 ) ) ;
#8552 = CARTESIAN_POINT ( 'NONE',  ( 1.719304012343089161, 12.64775761152706401, -1.452142814147889816 ) ) ;
#8553 = CARTESIAN_POINT ( 'NONE',  ( 3.092491956585974311, -4.738927301401886893, 6.343509225035307786 ) ) ;
#8554 = CARTESIAN_POINT ( 'NONE',  ( 2.000000000000001776, -1.058508696394911963, -6.730038252034928448 ) ) ;
#8555 = CARTESIAN_POINT ( 'NONE',  ( 37.00000000000000711, -12.26766708251988902, 3.473736367725380969 ) ) ;
#8556 = EDGE_CURVE ( 'NONE', #38380, #57471, #20734, .T. ) ;
#8557 = CARTESIAN_POINT ( 'NONE',  ( -22.94572469358970324, 4.011883207821686170, 2.792384151940626946 ) ) ;
#8558 = CARTESIAN_POINT ( 'NONE',  ( -27.45775109278351067, -8.499184579339635448, -8.471355351200609007 ) ) ;
#8559 = VERTEX_POINT ( 'NONE', #46302 ) ;
#8560 = ORIENTED_EDGE ( 'NONE', *, *, #35880, .F. ) ;
#8561 = CARTESIAN_POINT ( 'NONE',  ( 0.3040950598368144520, 12.11647736519423901, -1.881452845810252628 ) ) ;
#8562 = VECTOR ( 'NONE', #18343, 1000.000000000000000 ) ;
#8563 = ORIENTED_EDGE ( 'NONE', *, *, #53441, .F. ) ;
#8564 = CARTESIAN_POINT ( 'NONE',  ( 0.000000000000000000, -2.664846396702443609, -6.404188155573042884 ) ) ;
#8565 = CARTESIAN_POINT ( 'NONE',  ( 2.665405856346787949, -9.171500569027768890, 2.723742051529419506 ) ) ;
#8566 = EDGE_CURVE ( 'NONE', #63385, #45445, #6722, .T. ) ;
#8567 = CARTESIAN_POINT ( 'NONE',  ( -22.29290468048228036, -1.621390503294478869, 3.357740900108105109 ) ) ;
#8568 = ORIENTED_EDGE ( 'NONE', *, *, #47600, .T. ) ;
#8570 = FACE_OUTER_BOUND ( 'NONE', #36526, .T. ) ;
#8569 = AXIS2_PLACEMENT_3D ( 'NONE', #60100, #20522, #45786 ) ;
#8571 = CARTESIAN_POINT ( 'NONE',  ( 5.520433897694421610, -0.003119431460922320043, 0.01473594271720231851 ) ) ;
#8572 = DIRECTION ( 'NONE',  ( -1.000000000000000000, 0.000000000000000000, 0.000000000000000000 ) ) ;
#8573 = ORIENTED_EDGE ( 'NONE', *, *, #59929, .T. ) ;
#8574 = ORIENTED_EDGE ( 'NONE', *, *, #32100, .T. ) ;
#8575 = FACE_OUTER_BOUND ( 'NONE', #7210, .T. ) ;
#8576 = VECTOR ( 'NONE', #41023, 1000.000000000000000 ) ;
#8577 = CYLINDRICAL_SURFACE ( 'NONE', #17418, 12.18649999999999878 ) ;
#8578 = VERTEX_POINT ( 'NONE', #1410 ) ;
#8579 = ORIENTED_EDGE ( 'NONE', *, *, #45409, .T. ) ;
#8580 = CARTESIAN_POINT ( 'NONE',  ( -22.27706485742869091, -2.985151051101489372, 2.154081322712201096 ) ) ;
#8581 = DIRECTION ( 'NONE',  ( -1.000000000000000000, 0.000000000000000000, 0.000000000000000000 ) ) ;
#8582 = AXIS2_PLACEMENT_3D ( 'NONE', #21121, #20484, #25463 ) ;
#8583 = CARTESIAN_POINT ( 'NONE',  ( -35.00000000000000000, 10.68873102412852560, -6.950793414699680817 ) ) ;
#8584 = DIRECTION ( 'NONE',  ( 1.000000000000000000, 0.000000000000000000, -0.000000000000000000 ) ) ;
#8585 = CARTESIAN_POINT ( 'NONE',  ( 5.514624014163232779, 0.001574979445069367000, 0.003830004412313181561 ) ) ;
#8586 = AXIS2_PLACEMENT_3D ( 'NONE', #2623, #2933, #28503 ) ;
#8587 = CYLINDRICAL_SURFACE ( 'NONE', #30109, 5.000000000000000888 ) ;
#8588 = ORIENTED_EDGE ( 'NONE', *, *, #30900, .F. ) ;
#8589 = CARTESIAN_POINT ( 'NONE',  ( 36.00000000000000711, 9.733281772932160791, -8.235637554476683775 ) ) ;
#8590 = AXIS2_PLACEMENT_3D ( 'NONE', #6474, #27082, #16765 ) ;
#8591 = FACE_OUTER_BOUND ( 'NONE', #13307, .T. ) ;
#8592 = CARTESIAN_POINT ( 'NONE',  ( -19.16411987593509991, -13.50000000000000000, -0.3278540726586408049 ) ) ;
#8593 = DIRECTION ( 'NONE',  ( 0.000000000000000000, -0.9551603052523509607, 0.2960891610144411601 ) ) ;
#8594 = CARTESIAN_POINT ( 'NONE',  ( 37.00000000000000711, 4.705694406421931860E-17, -3.469127814946512892E-15 ) ) ;
#8595 = CARTESIAN_POINT ( 'NONE',  ( -27.08702828306202193, 1.612407531673552219, -1.639744581306265658 ) ) ;
#8596 = CARTESIAN_POINT ( 'NONE',  ( -27.08417568107324058, 1.449568724721390645, 1.774279301226111993 ) ) ;
#8597 = DIRECTION ( 'NONE',  ( -1.000000000000000000, 0.000000000000000000, 0.000000000000000000 ) ) ;
#8598 = LINE ( 'NONE', #53530, #34209 ) ;
#8599 = VECTOR ( 'NONE', #49488, 1000.000000000000000 ) ;
#8600 = EDGE_CURVE ( 'NONE', #31543, #42706, #56942, .T. ) ;
#8601 = AXIS2_PLACEMENT_3D ( 'NONE', #12663, #27990, #62547 ) ;
#8602 = VERTEX_POINT ( 'NONE', #61250 ) ;
#8603 = CARTESIAN_POINT ( 'NONE',  ( 41.00000000000000711, -25.03188948156373428, -4.500000000000011546 ) ) ;
#8604 = CIRCLE ( 'NONE', #38362, 12.75000000000000178 ) ;
#8605 = CIRCLE ( 'NONE', #109, 12.18650000000000411 ) ;
#8606 = ORIENTED_EDGE ( 'NONE', *, *, #31329, .F. ) ;
#8607 = CARTESIAN_POINT ( 'NONE',  ( 35.00000000000000000, 4.603882218679549609, -10.80631716521668828 ) ) ;
#8608 = CARTESIAN_POINT ( 'NONE',  ( 2.305787727787084851, -7.508843116234144688, -1.493241775258500770 ) ) ;
#8609 = CARTESIAN_POINT ( 'NONE',  ( 12.90095149745135039, -12.25278169605762635, -5.681374632462030227 ) ) ;
#8610 = CIRCLE ( 'NONE', #44717, 12.74999999999999822 ) ;
#8611 = CARTESIAN_POINT ( 'NONE',  ( 0.2650492594609242802, 9.309909082761148369, 7.955687020697082446 ) ) ;
#8612 = CARTESIAN_POINT ( 'NONE',  ( 5.516018279890452902, -0.004180585980734566158, 0.005331956019561453694 ) ) ;
#8613 = ORIENTED_EDGE ( 'NONE', *, *, #54370, .F. ) ;
#8614 = CYLINDRICAL_SURFACE ( 'NONE', #41985, 5.000000000000000888 ) ;
#8616 = CIRCLE ( 'NONE', #16051, 5.000000000000001776 ) ;
#8615 = CARTESIAN_POINT ( 'NONE',  ( 22.78406729994189561, -4.691424615418254618, 12.65938842238563744 ) ) ;
#8617 = CARTESIAN_POINT ( 'NONE',  ( -27.09483304420744432, 2.090133548855283241, 1.013994808269825132 ) ) ;
#8618 = CARTESIAN_POINT ( 'NONE',  ( 1.194176325881341594, 2.684784923266289258, 12.26540585042609521 ) ) ;
#8619 = EDGE_CURVE ( 'NONE', #37098, #43663, #40971, .T. ) ;
#8620 = VECTOR ( 'NONE', #9982, 1000.000000000000000 ) ;
#8621 = DIRECTION ( 'NONE',  ( 1.000000000000000000, 0.000000000000000000, 0.000000000000000000 ) ) ;
#8622 = ORIENTED_EDGE ( 'NONE', *, *, #55958, .T. ) ;
#8623 = ADVANCED_FACE ( 'NONE', ( #62541 ), #36514, .F. ) ;
#8624 = CARTESIAN_POINT ( 'NONE',  ( -18.04458733766117362, 11.34280559204706584, 3.916728392552376370 ) ) ;
#8625 = ORIENTED_EDGE ( 'NONE', *, *, #40382, .T. ) ;
#8626 = CIRCLE ( 'NONE', #61676, 12.74999999999999822 ) ;
#8627 = ADVANCED_FACE ( 'NONE', ( #35955 ), #56256, .T. ) ;
#8628 = CARTESIAN_POINT ( 'NONE',  ( 3.031336079628799585, 5.773872239512944482, -5.388626255826449274 ) ) ;
#8629 = CARTESIAN_POINT ( 'NONE',  ( -11.19906371800731471, -32.63487729457052922, 12.17775756912622676 ) ) ;
#8630 = CARTESIAN_POINT ( 'NONE',  ( -35.00000000000000000, -11.90598845858530552, -4.561791185930540671 ) ) ;
#8631 = CARTESIAN_POINT ( 'NONE',  ( -27.10719052120871098, 1.310802520592036391, 1.962717903527646079 ) ) ;
#8632 = CONICAL_SURFACE ( 'NONE', #23492, 5.135612550275435062, 1.249045772030607848 ) ;
#8633 = CIRCLE ( 'NONE', #58598, 12.18650000000000233 ) ;
#8634 = CIRCLE ( 'NONE', #21403, 7.499999999999988454 ) ;
#8635 = ORIENTED_EDGE ( 'NONE', *, *, #12603, .F. ) ;
#8637 = ORIENTED_EDGE ( 'NONE', *, *, #7352, .T. ) ;
#8636 = EDGE_CURVE ( 'NONE', #44356, #20918, #62836, .T. ) ;
#8638 = FACE_OUTER_BOUND ( 'NONE', #24535, .T. ) ;
#8639 = PLANE ( 'NONE',  #26579 ) ;
#8640 = CARTESIAN_POINT ( 'NONE',  ( 37.00000000000000711, 4.705694406421931860E-17, -3.469127814946512892E-15 ) ) ;
#8641 = CARTESIAN_POINT ( 'NONE',  ( 0.2648978790185584908, 12.24533305150758089, 0.1321385342562836074 ) ) ;
#8642 = CARTESIAN_POINT ( 'NONE',  ( 0.3474126878361828430, 9.233692382639482332, -8.085727498271683800 ) ) ;
#8643 = EDGE_CURVE ( 'NONE', #24684, #21602, #11679, .T. ) ;
#8644 = CARTESIAN_POINT ( 'NONE',  ( -22.29677679919927513, -2.096973157017373524, -3.097220482904039063 ) ) ;
#8645 = VERTEX_POINT ( 'NONE', #6386 ) ;
#8646 = EDGE_CURVE ( 'NONE', #5634, #9785, #5751, .T. ) ;
#8647 = ORIENTED_EDGE ( 'NONE', *, *, #41138, .T. ) ;
#8648 = VERTEX_POINT ( 'NONE', #41283 ) ;
#8649 = DIRECTION ( 'NONE',  ( 0.000000000000000000, -0.01356324068817999114, 0.9999080150203989437 ) ) ;
#8650 = EDGE_CURVE ( 'NONE', #28065, #51219, #61126, .T. ) ;
#8651 = CIRCLE ( 'NONE', #29904, 5.000000000000001776 ) ;
#8652 = VECTOR ( 'NONE', #59577, 1000.000000000000000 ) ;
#8653 = CARTESIAN_POINT ( 'NONE',  ( 35.00000000000000000, -9.700295462048712736, -7.376655759824850556 ) ) ;
#8654 = ORIENTED_EDGE ( 'NONE', *, *, #12140, .T. ) ;
#8655 = DIRECTION ( 'NONE',  ( 1.000000000000000000, -0.000000000000000000, -0.000000000000000000 ) ) ;
#8657 = EDGE_CURVE ( 'NONE', #51572, #48935, #52234, .T. ) ;
#8656 = AXIS2_PLACEMENT_3D ( 'NONE', #44493, #28563, #3321 ) ;
#8658 = CARTESIAN_POINT ( 'NONE',  ( -22.66110217412718697, -0.1747008913564180588, 4.941631093908251948 ) ) ;
#8659 = ORIENTED_EDGE ( 'NONE', *, *, #48685, .T. ) ;
#8660 = CARTESIAN_POINT ( 'NONE',  ( -27.04788180060269909, 1.844972430941770103, -2.650714769830301520 ) ) ;
#8661 = DIRECTION ( 'NONE',  ( -1.000000000000000000, 0.000000000000000000, 0.000000000000000000 ) ) ;
#8662 = ORIENTED_EDGE ( 'NONE', *, *, #44969, .T. ) ;
#8664 = EDGE_CURVE ( 'NONE', #40351, #11560, #49051, .T. ) ;
#8663 = VERTEX_POINT ( 'NONE', #50959 ) ;
#8665 = CARTESIAN_POINT ( 'NONE',  ( 2.000000000000001776, 3.341639490130761114, 6.078525953551427996 ) ) ;
#8666 = ORIENTED_EDGE ( 'NONE', *, *, #59345, .F. ) ;
#8667 = CYLINDRICAL_SURFACE ( 'NONE', #23235, 4.999999999999999112 ) ;
#8668 = ORIENTED_EDGE ( 'NONE', *, *, #16873, .F. ) ;
#8669 = CIRCLE ( 'NONE', #42618, 4.999999999999999112 ) ;
#8670 = ORIENTED_EDGE ( 'NONE', *, *, #10421, .T. ) ;
#8671 = VERTEX_POINT ( 'NONE', #14217 ) ;
#8672 = DIRECTION ( 'NONE',  ( 0.000000000000000000, -0.01356324068817998940, 0.9999080150203990547 ) ) ;
#8673 = DIRECTION ( 'NONE',  ( -0.000000000000000000, -1.000000000000000000, -0.000000000000000000 ) ) ;
#8674 = CARTESIAN_POINT ( 'NONE',  ( 37.00000000000000711, -10.49626516989275693, -7.238157050195595410 ) ) ;
#8675 = CARTESIAN_POINT ( 'NONE',  ( 0.6473888112830248343, 11.51036712212685309, -4.540486098228861067 ) ) ;
#8676 = CARTESIAN_POINT ( 'NONE',  ( -22.49803948133827802, -0.1132714802761562861, -4.343047530463637784 ) ) ;
#8677 = VERTEX_POINT ( 'NONE', #44802 ) ;
#8678 = CARTESIAN_POINT ( 'NONE',  ( -37.00000000000000711, -0.3137578094508294280, -12.74613886779085625 ) ) ;
#8679 = CIRCLE ( 'NONE', #45836, 2.899999999999994582 ) ;
#8680 = ORIENTED_EDGE ( 'NONE', *, *, #1142, .T. ) ;
#8681 = DIRECTION ( 'NONE',  ( 0.9582930651793755139, 0.2568015617827278940, 0.1254087680151157735 ) ) ;
#8682 = CARTESIAN_POINT ( 'NONE',  ( 2.000000000000001776, 0.000000000000000000, 0.000000000000000000 ) ) ;
#8683 = AXIS2_PLACEMENT_3D ( 'NONE', #13070, #63587, #32354 ) ;
#8684 = CIRCLE ( 'NONE', #45843, 4.999999999999999112 ) ;
#8685 = VERTEX_POINT ( 'NONE', #52913 ) ;
#8686 = FACE_OUTER_BOUND ( 'NONE', #50411, .T. ) ;
#8687 = CARTESIAN_POINT ( 'NONE',  ( 0.3401186441510237746, 3.955862996551503752, 11.61600526280572332 ) ) ;
#8688 = FACE_OUTER_BOUND ( 'NONE', #760, .T. ) ;
#8689 = B_SPLINE_CURVE_WITH_KNOTS ( 'NONE', 3,
 ( #43639, #18404, #56153, #9360, #29645, #59942, #13701, #3775, #4411, #39641, #46207, #61156, #54930, #29021, #61463, #49632, #38983, #59603, #24034, #20908, #14362, #39302 ),
 .UNSPECIFIED., .F., .F.,
 ( 4, 3, 3, 3, 3, 3, 3, 4 ),
 ( 1.084202172485504434E-19, 4.449119708436757522E-05, 6.626296329540340218E-05, 8.803456484962588510E-05, 0.0001098060367612804469, 0.0001315774408628515326, 0.0001760698110411161002, 0.0001829697163287829413 ),
 .UNSPECIFIED. ) ;
#8690 = ORIENTED_EDGE ( 'NONE', *, *, #19774, .F. ) ;
#8691 = AXIS2_PLACEMENT_3D ( 'NONE', #63410, #43455, #7917 ) ;
#8692 = EDGE_CURVE ( 'NONE', #55868, #12091, #57545, .T. ) ;
#8693 = VECTOR ( 'NONE', #8264, 1000.000000000000000 ) ;
#8694 = AXIS2_PLACEMENT_3D ( 'NONE', #41319, #16408, #27034 ) ;
#8695 = ORIENTED_EDGE ( 'NONE', *, *, #13674, .F. ) ;
#8696 = CARTESIAN_POINT ( 'NONE',  ( -35.04709527796842394, 0.005292201869334239861, 0.01117341439754379606 ) ) ;
#8697 = ORIENTED_EDGE ( 'NONE', *, *, #51478, .T. ) ;
#8698 = DIRECTION ( 'NONE',  ( -1.000000000000000000, 0.000000000000000000, 0.000000000000000000 ) ) ;
#8699 = CARTESIAN_POINT ( 'NONE',  ( -47.00000000000000711, 0.000000000000000000, 0.000000000000000000 ) ) ;
#8700 = CARTESIAN_POINT ( 'NONE',  ( 35.00000000000000000, 1.738225594540169894, 12.63095688309026698 ) ) ;
#8701 = CARTESIAN_POINT ( 'NONE',  ( -36.00000000000000711, 12.31350058095527977, -3.307597835713114609 ) ) ;
#8702 = CARTESIAN_POINT ( 'NONE',  ( 1.104777566491146112, -9.281442536087537221, 8.411711248089069670 ) ) ;
#8703 = EDGE_LOOP ( 'NONE', ( #55703, #24365, #53099, #56780 ) ) ;
#8704 = EDGE_CURVE ( 'NONE', #42070, #19326, #9222, .T. ) ;
#8705 = CARTESIAN_POINT ( 'NONE',  ( 2.241506898688419902, 3.783130304541519440, -6.631235260227124506 ) ) ;
#8706 = DIRECTION ( 'NONE',  ( 0.000000000000000000, 0.000000000000000000, 1.000000000000000000 ) ) ;
#8707 = VECTOR ( 'NONE', #33891, 1000.000000000000000 ) ;
#8708 = TOROIDAL_SURFACE ( 'NONE', #42656, 20.19615242270663558, 3.000000000000000000 ) ;
#8709 = ADVANCED_FACE ( 'NONE', ( #24524 ), #47602, .T. ) ;
#8710 = CARTESIAN_POINT ( 'NONE',  ( 0.3632410797595259644, -12.13515851238022414, -1.872837903657321945 ) ) ;
#8711 = AXIS2_PLACEMENT_3D ( 'NONE', #51288, #60, #16000 ) ;
#8712 = CARTESIAN_POINT ( 'NONE',  ( 2.241352910868908310, 7.633946224498473931, 0.08337961031706864201 ) ) ;
#8713 = LINE ( 'NONE', #65520, #13677 ) ;
#8714 = B_SPLINE_CURVE_WITH_KNOTS ( 'NONE', 3,
 ( #353, #6320, #1338, #37207, #7278, #43180, #52542, #63780, #22593, #23238, #38186, #17612, #2975, #36892, #58165, #27563, #42857, #21937, #2664, #11942, #47861, #32863 ),
 .UNSPECIFIED., .F., .F.,
 ( 4, 3, 3, 3, 3, 3, 3, 4 ),
 ( 9.813077866774405223E-18, 6.990956068646504110E-05, 0.0001398191187764071506, 0.0002097286751720257728, 0.0002796382307041420643, 0.0003495477861619880676, 0.0004194573423310373568, 0.0005586102576333245792 ),
 .UNSPECIFIED. ) ;
#8715 = EDGE_CURVE ( 'NONE', #43149, #49536, #22498, .T. ) ;
#8716 = DIRECTION ( 'NONE',  ( 0.000000000000000000, -0.01356324068817998940, 0.9999080150203990547 ) ) ;
#8717 = DIRECTION ( 'NONE',  ( 0.000000000000000000, 0.000000000000000000, 1.000000000000000000 ) ) ;
#8718 = CARTESIAN_POINT ( 'NONE',  ( 35.00000000000000000, 11.23004253107771078, 4.732539170486136371 ) ) ;
#8719 = AXIS2_PLACEMENT_3D ( 'NONE', #45720, #11451, #21786 ) ;
#8720 = ORIENTED_EDGE ( 'NONE', *, *, #48662, .T. ) ;
#8721 = CARTESIAN_POINT ( 'NONE',  ( -35.00000000000000000, 3.340853584269533716, 11.26103545359857350 ) ) ;
#8722 = ORIENTED_EDGE ( 'NONE', *, *, #52776, .T. ) ;
#8723 = DIRECTION ( 'NONE',  ( 0.000000000000000000, 0.000000000000000000, 1.000000000000000000 ) ) ;
#8724 = CARTESIAN_POINT ( 'NONE',  ( -22.27721688985630166, -3.631967556481315640, 0.6032462375556733036 ) ) ;
#8725 = CARTESIAN_POINT ( 'NONE',  ( 21.90174657591892071, 25.00000000000000000, -0.7349207973210698519 ) ) ;
#8726 = CARTESIAN_POINT ( 'NONE',  ( 40.42380607987477958, -25.46069350086628091, -4.500000000000000888 ) ) ;
#8727 = ORIENTED_EDGE ( 'NONE', *, *, #33062, .F. ) ;
#8728 = CIRCLE ( 'NONE', #3437, 2.899999999999996358 ) ;
#8729 = ORIENTED_EDGE ( 'NONE', *, *, #23711, .T. ) ;
#8730 = EDGE_LOOP ( 'NONE', ( #46585, #63041, #59448, #36277 ) ) ;
#8731 = CARTESIAN_POINT ( 'NONE',  ( 0.000000000000000000, -7.484036900328550956, 0.4890722589968952150 ) ) ;
#8732 = EDGE_CURVE ( 'NONE', #10033, #20614, #31774, .T. ) ;
#8733 = VECTOR ( 'NONE', #5615, 1000.000000000000000 ) ;
#8734 = CIRCLE ( 'NONE', #40577, 12.18649999999999878 ) ;
#8735 = ORIENTED_EDGE ( 'NONE', *, *, #51640, .F. ) ;
#8736 = EDGE_CURVE ( 'NONE', #4226, #30464, #3443, .T. ) ;
#8737 = LINE ( 'NONE', #53646, #35580 ) ;
#8738 = DIRECTION ( 'NONE',  ( 1.000000000000000000, -0.000000000000000000, 0.000000000000000000 ) ) ;
#8739 = CARTESIAN_POINT ( 'NONE',  ( 0.2676618633000471537, 10.52491907319761033, 6.262131165853769055 ) ) ;
#8740 = CARTESIAN_POINT ( 'NONE',  ( 17.92267017372352456, 8.274325337764011579, 8.703446854781846653 ) ) ;
#8741 = EDGE_LOOP ( 'NONE', ( #29240, #18346 ) ) ;
#8742 =( BOUNDED_SURFACE ( )  B_SPLINE_SURFACE ( 3, 1, ( 
 ( #16466, #31728 ),
 ( #32390, #21791 ),
 ( #1171, #48035 ),
 ( #26427, #31421 ) ),
 .UNSPECIFIED., .F., .F., .F. ) 
 B_SPLINE_SURFACE_WITH_KNOTS ( ( 4, 4 ),
 ( 2, 2 ),
 ( 0.000000000000000000, 1.000000000000000000 ),
 ( 0.000000000000000000, 1.000000000000000000 ),
 .UNSPECIFIED. ) 
 GEOMETRIC_REPRESENTATION_ITEM ( )  RATIONAL_B_SPLINE_SURFACE ( (
 ( 1.000000000000000000, 1.000000000000000000),
 ( 0.9942764183789327692, 0.8450855930916585379),
 ( 0.9942764183789327692, 0.8450855930916585379),
 ( 1.000000000000000000, 1.000000000000000000) ) ) 
 REPRESENTATION_ITEM ( '' )  SURFACE ( )  );
#8743 = CARTESIAN_POINT ( 'NONE',  ( -27.25055598261694456, -10.68287079889101321, 5.469009518302874184 ) ) ;
#8744 = CARTESIAN_POINT ( 'NONE',  ( 35.00000000000000000, 4.705694406421931860E-17, -3.469127814946512892E-15 ) ) ;
#8745 = DIRECTION ( 'NONE',  ( -1.000000000000000000, 0.000000000000000000, 0.000000000000000000 ) ) ;
#8747 = ORIENTED_EDGE ( 'NONE', *, *, #37883, .T. ) ;
#8746 = CARTESIAN_POINT ( 'NONE',  ( 2.941278708680199916, -6.138172921908581436, 0.1348063076486732403 ) ) ;
#8748 = EDGE_CURVE ( 'NONE', #5051, #13765, #40576, .T. ) ;
#8749 = FACE_OUTER_BOUND ( 'NONE', #40962, .T. ) ;
#8750 = ORIENTED_EDGE ( 'NONE', *, *, #2370, .F. ) ;
#8751 = CARTESIAN_POINT ( 'NONE',  ( 0.2834382757448032364, -6.300836243950088900, -10.50792790568174517 ) ) ;
#8752 = EDGE_LOOP ( 'NONE', ( #52665, #34170, #34533, #36288 ) ) ;
#8753 = CARTESIAN_POINT ( 'NONE',  ( 2.241352910868908310, -7.145045428366559648, -2.689314586382423045 ) ) ;
#8754 = AXIS2_PLACEMENT_3D ( 'NONE', #45439, #65703, #238 ) ;
#8755 = CARTESIAN_POINT ( 'NONE',  ( 0.3006302518452061423, 3.979421585299272035, -11.59403866275562223 ) ) ;
#8756 = DIRECTION ( 'NONE',  ( -0.000000000000000000, -0.000000000000000000, -1.000000000000000000 ) ) ;
#8757 = CARTESIAN_POINT ( 'NONE',  ( 0.3006302518452061423, -3.979421585299194764, 11.59403866275565775 ) ) ;
#8758 = CARTESIAN_POINT ( 'NONE',  ( 2.000000000000001776, -6.767909380267597363, 2.119450094687862052 ) ) ;
#8759 = DIRECTION ( 'NONE',  ( 0.000000000000000000, -0.9651210252299766701, -0.2618041379715732586 ) ) ;
#8761 = ORIENTED_EDGE ( 'NONE', *, *, #65525, .F. ) ;
#8760 = LINE ( 'NONE', #29043, #43771 ) ;
#8762 = AXIS2_PLACEMENT_3D ( 'NONE', #32672, #61640, #16442 ) ;
#8763 = ORIENTED_EDGE ( 'NONE', *, *, #24848, .F. ) ;
#8764 = CARTESIAN_POINT ( 'NONE',  ( -37.00000000000000711, -9.926225166347071749, 6.280308599560108007 ) ) ;
#8765 = ORIENTED_EDGE ( 'NONE', *, *, #22552, .T. ) ;
#8766 = AXIS2_PLACEMENT_3D ( 'NONE', #42838, #63761, #37859 ) ;
#8767 = VERTEX_POINT ( 'NONE', #3937 ) ;
#8768 = CARTESIAN_POINT ( 'NONE',  ( -27.08416974970326407, 0.3922151116844109220, 2.257332547928087685 ) ) ;
#8769 = DIRECTION ( 'NONE',  ( 1.000000000000000000, 0.000000000000000000, 0.000000000000000000 ) ) ;
#8770 = FACE_OUTER_BOUND ( 'NONE', #6856, .T. ) ;
#8771 = CARTESIAN_POINT ( 'NONE',  ( 5.514624014163232779, 0.001921576324372452002, 0.003668383633201380105 ) ) ;
#8772 = B_SPLINE_CURVE_WITH_KNOTS ( 'NONE', 3,
 ( #55227, #30292, #14638, #9659, #20953, #15955, #50589, #50906, #14972, #45571, #41232, #54008, #29954, #56204, #5355, #30934 ),
 .UNSPECIFIED., .F., .F.,
 ( 4, 3, 3, 3, 3, 4 ),
 ( 0.000000000000000000, 0.0003017745587525231328, 0.0006035491769808714636, 0.0009053241094668142966, 0.001207275924541012383, 0.001510325902535035502 ),
 .UNSPECIFIED. ) ;
#8773 = CARTESIAN_POINT ( 'NONE',  ( 0.2869720083484335049, 10.71444492121026038, -5.945302302873144207 ) ) ;
#8774 = EDGE_CURVE ( 'NONE', #44861, #42088, #34134, .T. ) ;
#8775 = DIRECTION ( 'NONE',  ( -1.000000000000000000, 0.000000000000000000, -0.000000000000000000 ) ) ;
#8776 = CONICAL_SURFACE ( 'NONE', #49130, 7.938172270156617749, 1.280189991382167047 ) ;
#8777 = ADVANCED_FACE ( 'NONE', ( #13007 ), #63529, .T. ) ;
#8778 = ORIENTED_EDGE ( 'NONE', *, *, #19384, .T. ) ;
#8779 = CARTESIAN_POINT ( 'NONE',  ( 35.00000000000000000, 6.584150480049550502, -10.25474254703955701 ) ) ;
#8780 = CARTESIAN_POINT ( 'NONE',  ( -27.08419797710328325, -1.413289504316732614, -1.803546201758818635 ) ) ;
#8781 = CARTESIAN_POINT ( 'NONE',  ( 6.812204945636112896, -4.138731716409435712, -11.26369831714194092 ) ) ;
#8782 = EDGE_LOOP ( 'NONE', ( #33332, #56272, #45052, #22194 ) ) ;
#8783 = CIRCLE ( 'NONE', #34256, 12.18650000000000233 ) ;
#8784 = ADVANCED_FACE ( 'NONE', ( #60425 ), #8532, .F. ) ;
#8785 = AXIS2_PLACEMENT_3D ( 'NONE', #21879, #52786, #618 ) ;
#8786 = CARTESIAN_POINT ( 'NONE',  ( 2.241352910868909643, -2.532612177304395029, -7.202080440908765979 ) ) ;
#8787 = DIRECTION ( 'NONE',  ( -1.000000000000000000, 0.000000000000000000, 0.000000000000000000 ) ) ;
#8789 = ORIENTED_EDGE ( 'NONE', *, *, #6098, .T. ) ;
#8788 = EDGE_CURVE ( 'NONE', #62166, #8079, #40815, .T. ) ;
#8790 = DIRECTION ( 'NONE',  ( 0.000000000000000000, -0.01356324068817998940, 0.9999080150203990547 ) ) ;
#8791 = DIRECTION ( 'NONE',  ( 0.000000000000000000, 0.000000000000000000, 1.000000000000000000 ) ) ;
#8792 = DIRECTION ( 'NONE',  ( 0.000000000000000000, 0.01356324068817998940, -0.9999080150203990547 ) ) ;
#8793 = AXIS2_PLACEMENT_3D ( 'NONE', #40077, #61341, #15783 ) ;
#8794 = EDGE_CURVE ( 'NONE', #26744, #60178, #65802, .T. ) ;
#8795 = VECTOR ( 'NONE', #16650, 1000.000000000000000 ) ;
#8796 = CARTESIAN_POINT ( 'NONE',  ( 2.305787727787084407, 2.774453000917245671, -7.135468203929955067 ) ) ;
#8797 = CARTESIAN_POINT ( 'NONE',  ( 2.827825597296803384, -0.5449445831287667019, 9.007857251166445423 ) ) ;
#8798 = ORIENTED_EDGE ( 'NONE', *, *, #49107, .F. ) ;
#8799 = FACE_OUTER_BOUND ( 'NONE', #24015, .T. ) ;
#8800 = CARTESIAN_POINT ( 'NONE',  ( -9.634191421358215379, -11.15524410274445621, -4.443362378840637561 ) ) ;
#8801 = CIRCLE ( 'NONE', #2455, 4.999999999999999112 ) ;
#8802 = CARTESIAN_POINT ( 'NONE',  ( -35.04643116707788408, 0.004425962698851801380, -0.01135624435145456135 ) ) ;
#8803 = EDGE_LOOP ( 'NONE', ( #2216, #10108, #48059, #26647 ) ) ;
#8804 = CARTESIAN_POINT ( 'NONE',  ( -35.00000000000000000, 6.891188680298823144, 9.512294188640927572 ) ) ;
#8805 = CARTESIAN_POINT ( 'NONE',  ( 0.2653519991613838558, -4.167757449530341773, -11.51519138201634718 ) ) ;
#8806 = ORIENTED_EDGE ( 'NONE', *, *, #46922, .F. ) ;
#8807 = ORIENTED_EDGE ( 'NONE', *, *, #36821, .T. ) ;
#8808 = LINE ( 'NONE', #44681, #58690 ) ;
#8809 = EDGE_CURVE ( 'NONE', #38245, #37217, #61400, .T. ) ;
#8810 = ORIENTED_EDGE ( 'NONE', *, *, #41815, .F. ) ;
#8811 = EDGE_CURVE ( 'NONE', #31809, #60956, #9758, .T. ) ;
#8812 = LINE ( 'NONE', #43379, #21741 ) ;
#8813 = FACE_OUTER_BOUND ( 'NONE', #16807, .T. ) ;
#8814 = DIRECTION ( 'NONE',  ( 0.000000000000000000, -0.01356324068817998940, 0.9999080150203990547 ) ) ;
#8815 = DIRECTION ( 'NONE',  ( 0.000000000000000000, -0.01356324068818000328, 0.9999080150203990547 ) ) ;
#8816 = CARTESIAN_POINT ( 'NONE',  ( -35.04709527796842394, 0.01117341439754726551, -0.005292201869334239861 ) ) ;
#8818 = ORIENTED_EDGE ( 'NONE', *, *, #7201, .T. ) ;
#8817 = CARTESIAN_POINT ( 'NONE',  ( 37.00000000000000711, 9.913596905230228629, 8.017674001891673896 ) ) ;
#8819 = CARTESIAN_POINT ( 'NONE',  ( -22.27706485742869091, 2.154081322712221969, 2.985151051101477382 ) ) ;
#8820 = ORIENTED_EDGE ( 'NONE', *, *, #172, .T. ) ;
#8821 = CARTESIAN_POINT ( 'NONE',  ( 0.2652384770603679609, 10.63836422907232127, -6.065775245581053632 ) ) ;
#8822 = EDGE_LOOP ( 'NONE', ( #34719, #56140, #14936, #42174 ) ) ;
#8823 = VECTOR ( 'NONE', #36105, 999.9999999999998863 ) ;
#8824 = ORIENTED_EDGE ( 'NONE', *, *, #44511, .F. ) ;
#8825 = CARTESIAN_POINT ( 'NONE',  ( -18.55576795264365941, 5.671152142829758880, 12.25417085568500219 ) ) ;
#8826 = CARTESIAN_POINT ( 'NONE',  ( -1.825668173474303435, -28.16298946971622996, 13.82820292525738459 ) ) ;
#8828 = CARTESIAN_POINT ( 'NONE',  ( -37.00000000000000711, -11.05394794832833583, 5.130401251914692651 ) ) ;
#8827 = AXIS2_PLACEMENT_3D ( 'NONE', #9412, #3828, #44343 ) ;
#8829 = CARTESIAN_POINT ( 'NONE',  ( 24.19939926762688032, 0.7067538267882510494, 11.98446061403317131 ) ) ;
#8830 = CARTESIAN_POINT ( 'NONE',  ( 36.00000000000000711, -2.865935305911542663, 12.42372387097884712 ) ) ;
#8831 = LINE ( 'NONE', #23815, #13945 ) ;
#8832 = ORIENTED_EDGE ( 'NONE', *, *, #12662, .T. ) ;
#8833 = VERTEX_POINT ( 'NONE', #45143 ) ;
#8834 = CARTESIAN_POINT ( 'NONE',  ( -35.00000000000000000, 15.00000000000000000, 1.836970198721029589E-15 ) ) ;
#8835 = VECTOR ( 'NONE', #20297, 1000.000000000000000 ) ;
#8836 = DIRECTION ( 'NONE',  ( 1.000000000000000000, 0.000000000000000000, 0.000000000000000000 ) ) ;
#8837 = B_SPLINE_CURVE_WITH_KNOTS ( 'NONE', 3,
 ( #46787, #61410, #10539, #46152, #60776, #51483, #15210, #30817, #19882, #35148, #40823, #35494, #61101, #10222, #9898, #35801, #51137, #11219 ),
 .UNSPECIFIED., .F., .F.,
 ( 4, 2, 2, 2, 2, 2, 2, 2, 4 ),
 ( 1.409462824231155764E-18, 0.001129207483351105362, 0.002258414966702208988, 0.003387622450053312615, 0.004516829933404417109, 0.005646037416755521170, 0.006775244900106624363, 0.007904452383457728423, 0.009033659866808832484 ),
 .UNSPECIFIED. ) ;
#8838 = VERTEX_POINT ( 'NONE', #61091 ) ;
#8839 = AXIS2_PLACEMENT_3D ( 'NONE', #50507, #25212, #45488 ) ;
#8840 = DIRECTION ( 'NONE',  ( 1.000000000000000000, 0.000000000000000000, 0.000000000000000000 ) ) ;
#8841 = CARTESIAN_POINT ( 'NONE',  ( 0.3401186441510237746, 0.2556125181571556881, -12.26845925752607336 ) ) ;
#8842 = CARTESIAN_POINT ( 'NONE',  ( -35.00000000000000000, 11.91791701451266405, 2.544412758415886877 ) ) ;
#8843 = CARTESIAN_POINT ( 'NONE',  ( -22.31328051695926007, 3.148362328073167404, -2.109671368890616350 ) ) ;
#8844 = CARTESIAN_POINT ( 'NONE',  ( -36.00000000000000711, 12.74921544981111232, -0.1414404973752581562 ) ) ;
#8845 = CARTESIAN_POINT ( 'NONE',  ( 0.3675815128205912052, -12.04510820461657516, -2.391755495700727874 ) ) ;
#8846 = ADVANCED_FACE ( 'NONE', ( #55781 ), #30175, .T. ) ;
#8847 = VERTEX_POINT ( 'NONE', #10212 ) ;
#8848 = VERTEX_POINT ( 'NONE', #20532 ) ;
#8849 = CARTESIAN_POINT ( 'NONE',  ( 0.2648978790185602672, 10.53870023327872474, -6.237101853238436355 ) ) ;
#8850 = DIRECTION ( 'NONE',  ( 1.000000000000000000, 0.000000000000000000, 0.000000000000000000 ) ) ;
#8851 = DIRECTION ( 'NONE',  ( -1.000000000000000000, 0.000000000000000000, 0.000000000000000000 ) ) ;
#8852 = LINE ( 'NONE', #2903, #3688 ) ;
#8853 = EDGE_CURVE ( 'NONE', #63312, #35169, #6605, .T. ) ;
#8854 = VECTOR ( 'NONE', #48272, 1000.000000000000000 ) ;
#8855 = CARTESIAN_POINT ( 'NONE',  ( 1.937114397841932290, 11.72279974487463683, 5.226660192101627800 ) ) ;
#8856 = CARTESIAN_POINT ( 'NONE',  ( -10.75289514965179549, -6.158246205637091464, -10.30132767016891471 ) ) ;
#8857 = DIRECTION ( 'NONE',  ( -1.000000000000000000, 0.000000000000000000, 0.000000000000000000 ) ) ;
#8858 = CARTESIAN_POINT ( 'NONE',  ( -27.10422407540562517, -2.109093808474706844, -1.039355862230284533 ) ) ;
#8859 = CARTESIAN_POINT ( 'NONE',  ( 37.00000000000000711, 11.96656215839374759, 4.400442035670818264 ) ) ;
#8860 = EDGE_CURVE ( 'NONE', #27962, #19209, #43759, .T. ) ;
#8861 = EDGE_LOOP ( 'NONE', ( #45033, #43162 ) ) ;
#8862 = CIRCLE ( 'NONE', #9955, 12.18650000000000055 ) ;
#8863 = CARTESIAN_POINT ( 'NONE',  ( 2.430348790456744901, -6.019963855523536189, -4.796903114819428104 ) ) ;
#8864 = CARTESIAN_POINT ( 'NONE',  ( 17.36549340976883116, 11.88942698613074178, 6.436805334688243008 ) ) ;
#8865 = CARTESIAN_POINT ( 'NONE',  ( 35.00000000000000000, 4.705694406421931860E-17, -3.469127814946512892E-15 ) ) ;
#8866 = EDGE_CURVE ( 'NONE', #40799, #28364, #26764, .T. ) ;
#8867 = AXIS2_PLACEMENT_3D ( 'NONE', #54911, #39942, #49931 ) ;
#8868 = AXIS2_PLACEMENT_3D ( 'NONE', #57735, #17487, #41417 ) ;
#8869 = CARTESIAN_POINT ( 'NONE',  ( -27.08429572838383947, -0.5764601019425836803, -2.217805374070540125 ) ) ;
#8870 = DIRECTION ( 'NONE',  ( 1.000000000000000000, 0.000000000000000000, 0.000000000000000000 ) ) ;
#8871 = EDGE_LOOP ( 'NONE', ( #62124, #54873, #3370, #9589 ) ) ;
#8872 = CARTESIAN_POINT ( 'NONE',  ( 2.263328370261528555, -2.479726736363687234, 7.228205514767161333 ) ) ;
#8873 = CARTESIAN_POINT ( 'NONE',  ( 5.514624014163232779, 0.0001700579043833964205, -0.004137701579365678402 ) ) ;
#8874 = AXIS2_PLACEMENT_3D ( 'NONE', #609, #25200, #45474 ) ;
#8875 = CARTESIAN_POINT ( 'NONE',  ( 5.926183177043330197, -31.73296902231061978, -13.63811545878544607 ) ) ;
#8876 = EDGE_LOOP ( 'NONE', ( #9244, #21220, #56690, #19306 ) ) ;
#8877 = CARTESIAN_POINT ( 'NONE',  ( -11.40165637462999904, -7.742630519260993438, -9.172861531003599467 ) ) ;
#8878 = DIRECTION ( 'NONE',  ( 0.000000000000000000, -0.01356324068817991828, 0.9999080150203990547 ) ) ;
#8879 = FACE_OUTER_BOUND ( 'NONE', #31318, .T. ) ;
#8880 = DIRECTION ( 'NONE',  ( -1.000000000000000000, 0.000000000000000000, 0.000000000000000000 ) ) ;
#8881 = CARTESIAN_POINT ( 'NONE',  ( 1.948354844646284612, 10.97658859989913083, -4.761851831284683811 ) ) ;
#8882 = ADVANCED_FACE ( 'NONE', ( #56426 ), #51125, .T. ) ;
#8883 = CIRCLE ( 'NONE', #5725, 12.18650000000000055 ) ;
#8884 = LINE ( 'NONE', #59419, #62643 ) ;
#8885 = VERTEX_POINT ( 'NONE', #897 ) ;
#8886 = CYLINDRICAL_SURFACE ( 'NONE', #19555, 12.74999999999999822 ) ;
#8887 = DIRECTION ( 'NONE',  ( -1.000000000000000000, -0.000000000000000000, -0.000000000000000000 ) ) ;
#8889 = VECTOR ( 'NONE', #34636, 1000.000000000000000 ) ;
#8888 = CARTESIAN_POINT ( 'NONE',  ( 0.3632410797595258534, -9.572936598843575950, -7.689504457927753833 ) ) ;
#8890 = CARTESIAN_POINT ( 'NONE',  ( -27.28573687977897677, 0.4470060700698672562, -2.862048090118451960 ) ) ;
#8891 = CARTESIAN_POINT ( 'NONE',  ( 37.00000000000000711, 6.753013023069713405, -10.14433819232436917 ) ) ;
#8892 = CARTESIAN_POINT ( 'NONE',  ( 2.000000000000001776, 5.450255447309811707, -4.087611905901392007 ) ) ;
#8893 = CIRCLE ( 'NONE', #17394, 12.18650000000000055 ) ;
#8894 = CARTESIAN_POINT ( 'NONE',  ( -30.15674304214251933, -0.5118533057020833166, -11.99746462915879697 ) ) ;
#8895 = FACE_OUTER_BOUND ( 'NONE', #62220, .T. ) ;
#8896 = ORIENTED_EDGE ( 'NONE', *, *, #10424, .F. ) ;
#8897 = ORIENTED_EDGE ( 'NONE', *, *, #33828, .F. ) ;
#8898 = CARTESIAN_POINT ( 'NONE',  ( 0.2646305136544065406, 12.08286001766538398, -1.996350543472870109 ) ) ;
#8899 = VERTEX_POINT ( 'NONE', #7186 ) ;
#8900 = EDGE_CURVE ( 'NONE', #24451, #48418, #11520, .T. ) ;
#8901 = CARTESIAN_POINT ( 'NONE',  ( 37.00000000000000711, -0.01609748574436820068, 11.74614673114903596 ) ) ;
#8902 = CIRCLE ( 'NONE', #48186, 12.18649999999999878 ) ;
#8903 = VERTEX_POINT ( 'NONE', #21851 ) ;
#8904 = CARTESIAN_POINT ( 'NONE',  ( 0.2834382757447999057, 5.949714385480788792, -10.71064820518736305 ) ) ;
#8905 = CARTESIAN_POINT ( 'NONE',  ( 2.770579946183331366, 1.653873933978976973, -7.633739187313457464 ) ) ;
#8906 = DIRECTION ( 'NONE',  ( 0.000000000000000000, -0.01356324068817991828, 0.9999080150203990547 ) ) ;
#8907 = VERTEX_POINT ( 'NONE', #6554 ) ;
#8908 = ORIENTED_EDGE ( 'NONE', *, *, #15582, .F. ) ;
#8909 = CARTESIAN_POINT ( 'NONE',  ( 2.440552418640496324, 0.1974238147510335439, -7.698292014589403820 ) ) ;
#8911 = CYLINDRICAL_SURFACE ( 'NONE', #39712, 12.18649999999999878 ) ;
#8910 = CIRCLE ( 'NONE', #52458, 12.75000000000000178 ) ;
#8912 = CIRCLE ( 'NONE', #46091, 5.000000000000000888 ) ;
#8913 = ORIENTED_EDGE ( 'NONE', *, *, #1666, .T. ) ;
#8914 = EDGE_LOOP ( 'NONE', ( #43319, #19436, #52977, #16717 ) ) ;
#8915 = DIRECTION ( 'NONE',  ( 1.000000000000000000, -0.000000000000000000, -0.000000000000000000 ) ) ;
#8916 = CARTESIAN_POINT ( 'NONE',  ( 35.00000000000000000, 4.705694406421931860E-17, -3.469127814946512892E-15 ) ) ;
#8917 = VECTOR ( 'NONE', #23036, 1000.000000000000000 ) ;
#8918 = LINE ( 'NONE', #49180, #8693 ) ;
#8919 = DIRECTION ( 'NONE',  ( -1.000000000000000000, 0.000000000000000000, 0.000000000000000000 ) ) ;
#8920 = DIRECTION ( 'NONE',  ( 0.000000000000000000, -0.01356324068817998940, 0.9999080150203990547 ) ) ;
#8921 = CARTESIAN_POINT ( 'NONE',  ( 0.2834382757447976298, 11.58108645293230943, 3.999440312567258626 ) ) ;
#8922 =( BOUNDED_CURVE ( )  B_SPLINE_CURVE ( 3, ( #52051, #56735, #16139, #16786 ),
 .UNSPECIFIED., .F., .F. ) 
 B_SPLINE_CURVE_WITH_KNOTS ( ( 4, 4 ),
 ( 3.502726250925535023, 3.584222553583020332 ),
 .UNSPECIFIED. ) 
 CURVE ( )  GEOMETRIC_REPRESENTATION_ITEM ( )  RATIONAL_B_SPLINE_CURVE ( ( 1.000000000000000000, 0.9994466059659543600, 0.9994466059659543600, 1.000000000000000000 ) ) 
 REPRESENTATION_ITEM ( '' )  );
#8923 = EDGE_CURVE ( 'NONE', #52767, #51541, #827, .T. ) ;
#8924 = ORIENTED_EDGE ( 'NONE', *, *, #29128, .F. ) ;
#8925 = CARTESIAN_POINT ( 'NONE',  ( 2.261269890822072082, -1.464004156081703201, 7.499479675451368621 ) ) ;
#8927 = CARTESIAN_POINT ( 'NONE',  ( 0.2652384770603647413, 7.922175044417105738, -9.338499095996349197 ) ) ;
#8926 = AXIS2_PLACEMENT_3D ( 'NONE', #11867, #12511, #26845 ) ;
#8928 = EDGE_CURVE ( 'NONE', #11758, #7009, #60751, .T. ) ;
#8929 = LINE ( 'NONE', #39832, #20447 ) ;
#8930 = DIRECTION ( 'NONE',  ( -1.000000000000000000, 0.000000000000000000, -0.000000000000000000 ) ) ;
#8931 = CARTESIAN_POINT ( 'NONE',  ( 27.15326549950207635, 11.36256450630621728, 3.875020145684566764 ) ) ;
#8932 = AXIS2_PLACEMENT_3D ( 'NONE', #55121, #9547, #29841 ) ;
#8933 = CARTESIAN_POINT ( 'NONE',  ( -27.08776759928996825, 1.611072893085662594, -1.644157618165827728 ) ) ;
#8934 = DIRECTION ( 'NONE',  ( 0.000000000000000000, 0.000000000000000000, 1.000000000000000000 ) ) ;
#8935 = CARTESIAN_POINT ( 'NONE',  ( -37.00000000000000711, 10.93004082984018588, 6.564808257521811186 ) ) ;
#8936 = CARTESIAN_POINT ( 'NONE',  ( -35.00000000000000000, 0.000000000000000000, 0.000000000000000000 ) ) ;
#8937 = AXIS2_PLACEMENT_3D ( 'NONE', #22053, #33000, #28355 ) ;
#8938 = EDGE_LOOP ( 'NONE', ( #15801, #62516, #12382, #35552 ) ) ;
#8939 = EDGE_CURVE ( 'NONE', #12565, #57350, #38348, .T. ) ;
#8940 = CARTESIAN_POINT ( 'NONE',  ( 0.2717059086739038176, 0.1760722388997856269, 12.24704971877459592 ) ) ;
#8941 =( BOUNDED_SURFACE ( )  B_SPLINE_SURFACE ( 3, 1, ( 
 ( #6827, #16471 ),
 ( #11459, #27097 ),
 ( #52705, #47394 ),
 ( #63309, #59251 ) ),
 .UNSPECIFIED., .F., .F., .F. ) 
 B_SPLINE_SURFACE_WITH_KNOTS ( ( 4, 4 ),
 ( 2, 2 ),
 ( 0.000000000000000000, 1.000000000000000000 ),
 ( 0.000000000000000000, 1.000000000000000000 ),
 .UNSPECIFIED. ) 
 GEOMETRIC_REPRESENTATION_ITEM ( )  RATIONAL_B_SPLINE_SURFACE ( (
 ( 1.000000000000000000, 1.000000000000000000),
 ( 0.6933888150995267674, 0.9895912004443193632),
 ( 0.6933888150995267674, 0.9895912004443193632),
 ( 1.000000000000000000, 1.000000000000000000) ) ) 
 REPRESENTATION_ITEM ( '' )  SURFACE ( )  );
#8942 = ORIENTED_EDGE ( 'NONE', *, *, #15666, .F. ) ;
#8943 = DIRECTION ( 'NONE',  ( 0.000000000000000000, 0.000000000000000000, 1.000000000000000000 ) ) ;
#8944 = CARTESIAN_POINT ( 'NONE',  ( 2.241352910868909643, -7.503490710578223144, -1.407733736974942973 ) ) ;
#8945 = VECTOR ( 'NONE', #34723, 1000.000000000000000 ) ;
#8946 = CARTESIAN_POINT ( 'NONE',  ( -36.00000000000000711, -8.496612874013226957, 9.506317355798342916 ) ) ;
#8947 = CARTESIAN_POINT ( 'NONE',  ( 2.000000000000001776, 7.493043167941614513, -0.3229614270519962638 ) ) ;
#8948 = CARTESIAN_POINT ( 'NONE',  ( -35.00000000000000000, 2.544412758416015219, -11.91791701451263741 ) ) ;
#8949 = VERTEX_POINT ( 'NONE', #31791 ) ;
#8950 = DIRECTION ( 'NONE',  ( 0.000000000000000000, -0.9635499925192201331, -0.2675283385292311911 ) ) ;
#8951 = DIRECTION ( 'NONE',  ( 0.000000000000000000, -0.9796553971857722143, -0.2006870767258996102 ) ) ;
#8952 = DIRECTION ( 'NONE',  ( 0.000000000000000000, -0.9970832820307031774, -0.07632122047557582389 ) ) ;
#8953 = CARTESIAN_POINT ( 'NONE',  ( 15.59244419633001222, -34.16973227397326696, -7.752328951098071741 ) ) ;
#8954 = VECTOR ( 'NONE', #24632, 1000.000000000000000 ) ;
#8955 = EDGE_CURVE ( 'NONE', #37930, #27528, #46852, .T. ) ;
#8956 = DIRECTION ( 'NONE',  ( 1.000000000000000000, 0.000000000000000000, 0.000000000000000000 ) ) ;
#8957 = ORIENTED_EDGE ( 'NONE', *, *, #6293, .F. ) ;
#8958 = DIRECTION ( 'NONE',  ( -0.000000000000000000, -1.000000000000000000, -0.000000000000000000 ) ) ;
#8959 = EDGE_LOOP ( 'NONE', ( #22183, #22202, #65004, #19500 ) ) ;
#8960 = CARTESIAN_POINT ( 'NONE',  ( 1.283627346226763333, -8.503905436511983496, -9.278077665801946594 ) ) ;
#8961 = DIRECTION ( 'NONE',  ( -1.000000000000000000, 0.000000000000000000, 0.000000000000000000 ) ) ;
#8962 = CIRCLE ( 'NONE', #56784, 12.74999999999999822 ) ;
#8963 = VECTOR ( 'NONE', #26215, 1000.000000000000000 ) ;
#8964 = CARTESIAN_POINT ( 'NONE',  ( 37.00000000000000711, 4.705694406421931860E-17, -3.469127814946512892E-15 ) ) ;
#8965 = DIRECTION ( 'NONE',  ( 0.3939253465568944290, 0.5833358547425043783, 0.7103112711423510417 ) ) ;
#8966 = ORIENTED_EDGE ( 'NONE', *, *, #65188, .F. ) ;
#8967 = ORIENTED_EDGE ( 'NONE', *, *, #3894, .T. ) ;
#8968 = CARTESIAN_POINT ( 'NONE',  ( 3.780834652287974773, 8.352030633203074927, -10.60629927458383470 ) ) ;
#8969 = CARTESIAN_POINT ( 'NONE',  ( 2.242418902651891255, 4.983487297755272216, 5.783980263416264478 ) ) ;
#8970 = CYLINDRICAL_SURFACE ( 'NONE', #17300, 12.18649999999999878 ) ;
#8971 = CARTESIAN_POINT ( 'NONE',  ( -37.00000000000000711, 4.237620530777800987, 11.42599468261430928 ) ) ;
#8972 = CARTESIAN_POINT ( 'NONE',  ( 0.2647959493198570047, 9.285851961022064671, -7.983607158780230861 ) ) ;
#8973 = DIRECTION ( 'NONE',  ( -1.000000000000000000, 0.000000000000000000, 0.000000000000000000 ) ) ;
#8974 = CARTESIAN_POINT ( 'NONE',  ( -18.04458733766117362, -11.34280559204704097, 3.916728392552376370 ) ) ;
#8975 = ORIENTED_EDGE ( 'NONE', *, *, #49656, .T. ) ;
#8976 = VERTEX_POINT ( 'NONE', #47450 ) ;
#8977 = EDGE_LOOP ( 'NONE', ( #62373, #58401, #53420, #39294 ) ) ;
#8978 = CARTESIAN_POINT ( 'NONE',  ( 1.014383007554946481, -2.605923236272049692, -12.22116704270660570 ) ) ;
#8979 = AXIS2_PLACEMENT_3D ( 'NONE', #50036, #38747, #55010 ) ;
#8980 = EDGE_CURVE ( 'NONE', #5010, #11924, #52445, .T. ) ;
#8981 = CARTESIAN_POINT ( 'NONE',  ( 1.719304012338199295, 12.70777170743846796, -0.7661785589580241140 ) ) ;
#8982 = VERTEX_POINT ( 'NONE', #6883 ) ;
#8983 = CARTESIAN_POINT ( 'NONE',  ( -37.00000000000000711, -9.348667969174352166, -7.817492529713958582 ) ) ;
#8984 = FACE_BOUND ( 'NONE', #9121, .T. ) ;
#8985 = ORIENTED_EDGE ( 'NONE', *, *, #13, .T. ) ;
#8986 = CARTESIAN_POINT ( 'NONE',  ( 2.835339799623984636, 7.241165502254445663, 2.985412098050525209 ) ) ;
#8987 = DIRECTION ( 'NONE',  ( 0.000000000000000000, 0.000000000000000000, 1.000000000000000000 ) ) ;
#8988 = DIRECTION ( 'NONE',  ( 1.000000000000000000, 1.685093406416449860E-16, -1.011030131491573426E-17 ) ) ;
#8989 = ORIENTED_EDGE ( 'NONE', *, *, #57420, .T. ) ;
#8990 = ORIENTED_EDGE ( 'NONE', *, *, #62250, .T. ) ;
#8991 = FACE_OUTER_BOUND ( 'NONE', #26171, .T. ) ;
#8992 = VERTEX_POINT ( 'NONE', #32451 ) ;
#8993 = CARTESIAN_POINT ( 'NONE',  ( 35.00000000000000000, -11.17622378668003691, 3.614449339633606595 ) ) ;
#8994 = ORIENTED_EDGE ( 'NONE', *, *, #63483, .T. ) ;
#8995 = ORIENTED_EDGE ( 'NONE', *, *, #7441, .F. ) ;
#8996 = ORIENTED_EDGE ( 'NONE', *, *, #27889, .T. ) ;
#8997 = CARTESIAN_POINT ( 'NONE',  ( -27.01437459610461644, 8.723448335974111956, -8.240233560378637634 ) ) ;
#8998 = CARTESIAN_POINT ( 'NONE',  ( -0.4601472316530035300, -30.53649492335513926, -15.30974548841756189 ) ) ;
#8999 = CIRCLE ( 'NONE', #40849, 6.936499999999995225 ) ;
#9000 = ADVANCED_FACE ( 'NONE', ( #27808 ), #38242, .F. ) ;
#9001 = DIRECTION ( 'NONE',  ( 1.000000000000000000, 0.000000000000000000, 0.000000000000000000 ) ) ;
#9002 = CARTESIAN_POINT ( 'NONE',  ( -22.65996813707688062, -4.828298130757413986, -0.2230532344361538521 ) ) ;
#9003 = ORIENTED_EDGE ( 'NONE', *, *, #59582, .F. ) ;
#9004 = CARTESIAN_POINT ( 'NONE',  ( 1.014383007554947147, 11.03701226956417081, 5.859361736620373406 ) ) ;
#9005 = ORIENTED_EDGE ( 'NONE', *, *, #20413, .F. ) ;
#9006 = CARTESIAN_POINT ( 'NONE',  ( 2.241311220309554653, -2.698144003944842328, 7.141707286456117743 ) ) ;
#9007 = EDGE_CURVE ( 'NONE', #5308, #38082, #63053, .T. ) ;
#9008 = CARTESIAN_POINT ( 'NONE',  ( -17.64636966839529109, -7.707522472056596463, -11.08736416828873850 ) ) ;
#9009 = EDGE_CURVE ( 'NONE', #35706, #50717, #58079, .T. ) ;
#9010 = ORIENTED_EDGE ( 'NONE', *, *, #48893, .F. ) ;
#9011 = DIRECTION ( 'NONE',  ( -1.000000000000000000, -1.685093406416449860E-16, 1.011030131491573426E-17 ) ) ;
#9012 = CARTESIAN_POINT ( 'NONE',  ( 5.515539859299206427, 0.002856745161749566376, 0.005336559634876450291 ) ) ;
#9013 = CARTESIAN_POINT ( 'NONE',  ( 2.000000000000001776, 6.338823199656720142, -2.816798305433633853 ) ) ;
#9014 = VERTEX_POINT ( 'NONE', #31484 ) ;
#9015 = ORIENTED_EDGE ( 'NONE', *, *, #41723, .T. ) ;
#9016 = ADVANCED_FACE ( 'NONE', ( #52101 ), #22536, .F. ) ;
#9017 = CARTESIAN_POINT ( 'NONE',  ( 0.4613984246114865573, 6.399144685811715583, 10.51786362586216406 ) ) ;
#9018 = ORIENTED_EDGE ( 'NONE', *, *, #19673, .F. ) ;
#9019 = ADVANCED_FACE ( 'NONE', ( #62378 ), #53077, .T. ) ;
#9020 = DIRECTION ( 'NONE',  ( -1.000000000000000000, 0.000000000000000000, -0.000000000000000000 ) ) ;
#9021 = CARTESIAN_POINT ( 'NONE',  ( 1.372161826075870117, 10.03232826862047133, 7.648244077827104803 ) ) ;
#9022 = CARTESIAN_POINT ( 'NONE',  ( 2.022082860508907398, -26.59007814299271288, 16.17076096363556204 ) ) ;
#9023 = CARTESIAN_POINT ( 'NONE',  ( 2.241352910868908754, -6.652881166698538351, 3.744764251556969903 ) ) ;
#9024 = CARTESIAN_POINT ( 'NONE',  ( -19.55186598411636467, -3.901828651817480953, -12.92480312515320229 ) ) ;
#9025 = AXIS2_PLACEMENT_3D ( 'NONE', #37625, #57922, #52912 ) ;
#9026 = ORIENTED_EDGE ( 'NONE', *, *, #30080, .T. ) ;
#9027 = CARTESIAN_POINT ( 'NONE',  ( 3.152665057736135701, -1.848755561854027452, -7.719888720907647439 ) ) ;
#9028 = CARTESIAN_POINT ( 'NONE',  ( 3.152665057734040488, 0.000000000000000000, 0.000000000000000000 ) ) ;
#9029 = CIRCLE ( 'NONE', #4818, 5.000000000000000000 ) ;
#9030 = EDGE_CURVE ( 'NONE', #64802, #33595, #65122, .T. ) ;
#9031 = CARTESIAN_POINT ( 'NONE',  ( 1.719304012338199517, 0.000000000000000000, 0.000000000000000000 ) ) ;
#9032 = EDGE_CURVE ( 'NONE', #41515, #16757, #59575, .T. ) ;
#9033 = CARTESIAN_POINT ( 'NONE',  ( 2.705197763288545776, -5.217779042888482266, 5.783040721897918068 ) ) ;
#9034 = DIRECTION ( 'NONE',  ( 0.000000000000000000, 0.01356324068817998940, -0.9999080150203990547 ) ) ;
#9035 = CARTESIAN_POINT ( 'NONE',  ( 6.987038089383098338, -8.045544563376781255, -8.914883656081883601 ) ) ;
#9036 = DIRECTION ( 'NONE',  ( -1.000000000000000000, 0.000000000000000000, 0.000000000000000000 ) ) ;
#9037 = AXIS2_PLACEMENT_3D ( 'NONE', #16699, #41641, #61928 ) ;
#9038 = B_SPLINE_CURVE_WITH_KNOTS ( 'NONE', 3,
 ( #64400, #18873, #64090, #9199, #12890, #53800, #3915 ),
 .UNSPECIFIED., .F., .F.,
 ( 4, 3, 4 ),
 ( 0.000000000000000000, 0.001700533616330545143, 0.005002426799371691157 ),
 .UNSPECIFIED. ) ;
#9039 = ORIENTED_EDGE ( 'NONE', *, *, #55650, .F. ) ;
#9040 = CARTESIAN_POINT ( 'NONE',  ( 35.00000000000000000, -5.130401251914806338, -11.05394794832827898 ) ) ;
#9041 = EDGE_LOOP ( 'NONE', ( #30156, #52584, #44895, #39219 ) ) ;
#9042 = DIRECTION ( 'NONE',  ( -1.000000000000000000, 0.000000000000000000, 0.000000000000000000 ) ) ;
#9043 = CARTESIAN_POINT ( 'NONE',  ( -22.27718112499583469, -3.645895996548662588, 0.5110808820053356349 ) ) ;
#9044 = CARTESIAN_POINT ( 'NONE',  ( 2.899286259009684841, -7.494390643303793453, 2.348384892629340470 ) ) ;
#9045 = CARTESIAN_POINT ( 'NONE',  ( 2.241536586108913820, 3.822683724643463066, 6.608496983003799841 ) ) ;
#9046 = VERTEX_POINT ( 'NONE', #18821 ) ;
#9047 = AXIS2_PLACEMENT_3D ( 'NONE', #36784, #56410, #57077 ) ;
#9048 = ORIENTED_EDGE ( 'NONE', *, *, #5789, .T. ) ;
#9049 = ORIENTED_EDGE ( 'NONE', *, *, #39156, .F. ) ;
#9050 = CARTESIAN_POINT ( 'NONE',  ( -17.83419946441818027, -9.720786832536937538, 9.367833439828872955 ) ) ;
#9051 = EDGE_CURVE ( 'NONE', #49400, #11115, #21441, .T. ) ;
#9052 = ORIENTED_EDGE ( 'NONE', *, *, #55805, .F. ) ;
#9053 = DIRECTION ( 'NONE',  ( -1.000000000000000000, 0.000000000000000000, -0.000000000000000000 ) ) ;
#9054 = DIRECTION ( 'NONE',  ( 1.000000000000000000, 0.000000000000000000, 0.000000000000000000 ) ) ;
#9055 = LINE ( 'NONE', #64894, #47162 ) ;
#9056 = CARTESIAN_POINT ( 'NONE',  ( -2.532614230583026593, 25.00000000000000000, 10.89930238848911337 ) ) ;
#9057 = ORIENTED_EDGE ( 'NONE', *, *, #52214, .T. ) ;
#9058 = AXIS2_PLACEMENT_3D ( 'NONE', #62185, #25970, #20952 ) ;
#9059 = DIRECTION ( 'NONE',  ( -1.000000000000000000, 0.000000000000000000, 0.000000000000000000 ) ) ;
#9060 = CARTESIAN_POINT ( 'NONE',  ( -8.639472567035785033, -29.08579227083643559, -11.67554154369979358 ) ) ;
#9061 = CARTESIAN_POINT ( 'NONE',  ( -29.68541646480307250, -1.795142075051132657, -11.87110896435279095 ) ) ;
#9063 = VERTEX_POINT ( 'NONE', #53427 ) ;
#9062 = DIRECTION ( 'NONE',  ( 1.000000000000000000, 0.000000000000000000, 0.000000000000000000 ) ) ;
#9064 = CARTESIAN_POINT ( 'NONE',  ( -35.04643116707788408, 0.008094444324494021181, 0.009112266603801891240 ) ) ;
#9065 = ORIENTED_EDGE ( 'NONE', *, *, #23658, .T. ) ;
#9066 = CARTESIAN_POINT ( 'NONE',  ( -29.43980975494970309, -3.641506875706030488, -11.43413432115371364 ) ) ;
#9067 = ADVANCED_FACE ( 'NONE', ( #23824 ), #12832, .T. ) ;
#9068 = ORIENTED_EDGE ( 'NONE', *, *, #58195, .T. ) ;
#9069 = CARTESIAN_POINT ( 'NONE',  ( 2.000000000000001776, -5.097042323172408906, -5.501832381651512449 ) ) ;
#9070 = CARTESIAN_POINT ( 'NONE',  ( 0.3109076770649062960, 3.971171685427550724, -11.60048803586494692 ) ) ;
#9071 = AXIS2_PLACEMENT_3D ( 'NONE', #38244, #48582, #17983 ) ;
#9072 = CARTESIAN_POINT ( 'NONE',  ( 47.00000000000000711, 4.705694406421931860E-17, -3.469127814946512892E-15 ) ) ;
#9073 = CARTESIAN_POINT ( 'NONE',  ( -35.00000000000000000, 11.47758908105694786, 2.497432891016883261 ) ) ;
#9074 = DIRECTION ( 'NONE',  ( -1.000000000000000000, 0.000000000000000000, 0.000000000000000000 ) ) ;
#9075 = EDGE_CURVE ( 'NONE', #62046, #31684, #53063, .T. ) ;
#9076 = CARTESIAN_POINT ( 'NONE',  ( -27.10422407540562162, -0.1544383239736460967, -2.346206748218708338 ) ) ;
#9077 = CARTESIAN_POINT ( 'NONE',  ( 2.827825597296803384, -3.592949031604475429, 8.278234963587699724 ) ) ;
#9079 = ORIENTED_EDGE ( 'NONE', *, *, #19364, .T. ) ;
#9078 = CARTESIAN_POINT ( 'NONE',  ( 2.000000000000001776, 3.155844197800107498, 6.177028383390443800 ) ) ;
#9080 = ORIENTED_EDGE ( 'NONE', *, *, #62412, .F. ) ;
#9081 = DIRECTION ( 'NONE',  ( 0.000000000000000000, 0.000000000000000000, 1.000000000000000000 ) ) ;
#9082 = ORIENTED_EDGE ( 'NONE', *, *, #7922, .F. ) ;
#9083 = EDGE_CURVE ( 'NONE', #9626, #29988, #44085, .T. ) ;
#9084 = ORIENTED_EDGE ( 'NONE', *, *, #64014, .F. ) ;
#9085 = CARTESIAN_POINT ( 'NONE',  ( 0.000000000000000000, 6.935703035393450122, 0.1051458740707594125 ) ) ;
#9086 = CARTESIAN_POINT ( 'NONE',  ( -37.00000000000000711, -4.426194442447159538, -11.35427606708811332 ) ) ;
#9087 = CARTESIAN_POINT ( 'NONE',  ( 0.2638984909335716500, -11.43908195192326893, -4.375449752477248211 ) ) ;
#9088 = DIRECTION ( 'NONE',  ( 0.000000000000000000, 0.8989688749565142301, 0.4380125133594005016 ) ) ;
#9089 = CARTESIAN_POINT ( 'NONE',  ( -22.29115169517546136, 1.614783311161212875, -3.355084543108099560 ) ) ;
#9090 = FACE_OUTER_BOUND ( 'NONE', #14510, .T. ) ;
#9091 = CYLINDRICAL_SURFACE ( 'NONE', #12000, 12.18650000000000055 ) ;
#9092 = ORIENTED_EDGE ( 'NONE', *, *, #14222, .F. ) ;
#9093 = ADVANCED_FACE ( 'NONE', ( #54067 ), #28760, .T. ) ;
#9094 = CARTESIAN_POINT ( 'NONE',  ( 37.00000000000000711, -6.584150480049477672, 10.25474254703959431 ) ) ;
#9095 = CARTESIAN_POINT ( 'NONE',  ( -27.08416813689867908, -1.467601568343275265, -1.759517419957085549 ) ) ;
#9096 = DIRECTION ( 'NONE',  ( 0.000000000000000000, -0.1118654143051477368, -0.9937233664769776764 ) ) ;
#9097 = EDGE_CURVE ( 'NONE', #16245, #35534, #13524, .T. ) ;
#9098 = VERTEX_POINT ( 'NONE', #38776 ) ;
#9099 = EDGE_CURVE ( 'NONE', #60300, #12134, #52430, .T. ) ;
#9100 = EDGE_CURVE ( 'NONE', #36393, #32874, #20264, .T. ) ;
#9101 = CIRCLE ( 'NONE', #18682, 5.000000000000000888 ) ;
#9102 = CARTESIAN_POINT ( 'NONE',  ( -11.12450214041353291, -5.606564972075692488, 12.28260682454939179 ) ) ;
#9103 = EDGE_CURVE ( 'NONE', #19030, #11939, #24615, .T. ) ;
#9104 = CARTESIAN_POINT ( 'NONE',  ( -10.61430208547403886, -9.391830329834835567, -9.709184090487172014 ) ) ;
#9105 = ORIENTED_EDGE ( 'NONE', *, *, #65433, .T. ) ;
#9106 = CARTESIAN_POINT ( 'NONE',  ( -35.00000000000000000, 2.021542716731397071, 12.01765980939842748 ) ) ;
#9107 = DIRECTION ( 'NONE',  ( -1.000000000000000000, 0.000000000000000000, 0.000000000000000000 ) ) ;
#9108 = CARTESIAN_POINT ( 'NONE',  ( 3.847381992255190841, 5.216794478567112314, 10.80899677692140592 ) ) ;
#9109 = AXIS2_PLACEMENT_3D ( 'NONE', #55699, #36038, #5496 ) ;
#9110 = CARTESIAN_POINT ( 'NONE',  ( 6.812204945636112896, -4.138731716409435712, 12.84993773446340803 ) ) ;
#9111 = CARTESIAN_POINT ( 'NONE',  ( 2.350038591458110560, -0.6402934222729476099, 10.60256821300787422 ) ) ;
#9112 =( BOUNDED_SURFACE ( )  B_SPLINE_SURFACE ( 3, 1, ( 
 ( #14827, #35113 ),
 ( #40109, #19535 ),
 ( #9517, #44777 ),
 ( #36097, #29481 ) ),
 .UNSPECIFIED., .F., .F., .F. ) 
 B_SPLINE_SURFACE_WITH_KNOTS ( ( 4, 4 ),
 ( 2, 2 ),
 ( 0.000000000000000000, 1.000000000000000000 ),
 ( 0.000000000000000000, 1.000000000000000000 ),
 .UNSPECIFIED. ) 
 GEOMETRIC_REPRESENTATION_ITEM ( )  RATIONAL_B_SPLINE_SURFACE ( (
 ( 1.000000000000000000, 1.000000000000000000),
 ( 0.8716676215708681896, 0.8964445200148164483),
 ( 0.8716676215708681896, 0.8964445200148164483),
 ( 1.000000000000000000, 1.000000000000000000) ) ) 
 REPRESENTATION_ITEM ( '' )  SURFACE ( )  );
#9113 = VERTEX_POINT ( 'NONE', #9466 ) ;
#9114 = DIRECTION ( 'NONE',  ( -0.3865475372811021382, -0.9114221272958260567, -0.1410344188397496257 ) ) ;
#9115 = CARTESIAN_POINT ( 'NONE',  ( 35.00000000000000000, 8.029056188533806093, 8.573591947375229338 ) ) ;
#9116 = CARTESIAN_POINT ( 'NONE',  ( 37.00000000000000711, 10.30098186818249673, -5.644643009979106729 ) ) ;
#9117 = ORIENTED_EDGE ( 'NONE', *, *, #23838, .T. ) ;
#9118 = CARTESIAN_POINT ( 'NONE',  ( 21.74669156475645693, 13.45922031030403332, -1.115717662970064694 ) ) ;
#9119 = CARTESIAN_POINT ( 'NONE',  ( 2.080613030138687591, 0.000000000000000000, -1.000000000000000000 ) ) ;
#9120 = ORIENTED_EDGE ( 'NONE', *, *, #44038, .T. ) ;
#9121 = EDGE_LOOP ( 'NONE', ( #40940, #50778, #14602, #13193 ) ) ;
#9122 = VERTEX_POINT ( 'NONE', #30424 ) ;
#9123 = CYLINDRICAL_SURFACE ( 'NONE', #14029, 4.999999999999999112 ) ;
#9124 = EDGE_CURVE ( 'NONE', #53395, #17729, #5429, .T. ) ;
#9125 = VERTEX_POINT ( 'NONE', #29750 ) ;
#9126 = CARTESIAN_POINT ( 'NONE',  ( -37.00000000000000711, 6.753013023069858178, -10.14433819232427147 ) ) ;
#9127 = CARTESIAN_POINT ( 'NONE',  ( 1.000000000000000888, 7.203928197742132333, -2.086484728383096510 ) ) ;
#9128 = CARTESIAN_POINT ( 'NONE',  ( 25.00000000000000355, -30.00000000000000000, 25.00000000000000000 ) ) ;
#9129 = CARTESIAN_POINT ( 'NONE',  ( 0.2648978790185593790, 4.063980959785203240, -11.55204314799259890 ) ) ;
#9130 = CARTESIAN_POINT ( 'NONE',  ( 2.241449424704145432, 0.06135604983228025444, 7.634218943782392408 ) ) ;
#9132 = ORIENTED_EDGE ( 'NONE', *, *, #57008, .F. ) ;
#9131 = CARTESIAN_POINT ( 'NONE',  ( 2.241537034860905386, -7.634469414369387863, -0.004719967007756531788 ) ) ;
#9133 = CARTESIAN_POINT ( 'NONE',  ( 35.00000000000000000, -10.23119532541066867, 7.608228585767831120 ) ) ;
#9134 = VERTEX_POINT ( 'NONE', #5170 ) ;
#9135 = CARTESIAN_POINT ( 'NONE',  ( -35.00000000000000000, 10.62137734850268345, 5.015831474386344802 ) ) ;
#9136 = EDGE_LOOP ( 'NONE', ( #51631, #17796, #10008, #30569 ) ) ;
#9137 = EDGE_CURVE ( 'NONE', #52774, #28155, #18189, .T. ) ;
#9138 = VERTEX_POINT ( 'NONE', #5508 ) ;
#9139 = CARTESIAN_POINT ( 'NONE',  ( -37.00000000000000711, 0.000000000000000000, 0.000000000000000000 ) ) ;
#9140 = CARTESIAN_POINT ( 'NONE',  ( 3.194234995343356420, -28.25772741626087736, 13.63608895903861118 ) ) ;
#9141 = CARTESIAN_POINT ( 'NONE',  ( -24.67206623709094515, 8.916871779494830008, 10.14344027151376615 ) ) ;
#9142 = CARTESIAN_POINT ( 'NONE',  ( 24.40079717985569374, -0.3635673505086269852, 11.99993777491598834 ) ) ;
#9143 = AXIS2_PLACEMENT_3D ( 'NONE', #39002, #29353, #38689 ) ;
#9144 = CARTESIAN_POINT ( 'NONE',  ( 0.9232058338315048962, -12.21058493388772170, -2.536181247095490754 ) ) ;
#9145 = DIRECTION ( 'NONE',  ( 0.000000000000000000, 0.01356324068817999114, -0.9999080150203990547 ) ) ;
#9146 = ORIENTED_EDGE ( 'NONE', *, *, #12435, .T. ) ;
#9147 = AXIS2_PLACEMENT_3D ( 'NONE', #20732, #5785, #60972 ) ;
#9148 = ORIENTED_EDGE ( 'NONE', *, *, #52671, .T. ) ;
#9149 = B_SPLINE_CURVE_WITH_KNOTS ( 'NONE', 3,
 ( #46022, #22631, #26066, #63182, #12301, #6115, #37590, #26374, #5464, #12623, #32901, #56302, #784, #42897, #46659, #37908, #30694, #21048, #7661 ),
 .UNSPECIFIED., .F., .F.,
 ( 4, 3, 3, 3, 3, 3, 4 ),
 ( 7.423420718681438206E-18, 2.825908398831030981E-05, 4.208813692483597913E-05, 5.591713746943513416E-05, 6.279584083231333285E-05, 9.105792820295870052E-05, 0.0001153131102488866381 ),
 .UNSPECIFIED. ) ;
#9150 = LINE ( 'NONE', #24126, #59261 ) ;
#9151 = EDGE_CURVE ( 'NONE', #5538, #59359, #65339, .T. ) ;
#9152 = ORIENTED_EDGE ( 'NONE', *, *, #2718, .T. ) ;
#9153 = CARTESIAN_POINT ( 'NONE',  ( -22.27706485742869091, -0.9221835209182183135, -3.563814065926679042 ) ) ;
#9154 = CARTESIAN_POINT ( 'NONE',  ( 0.3218525148189831375, 0.2444206315274874974, -12.26259572563018807 ) ) ;
#9155 = FACE_OUTER_BOUND ( 'NONE', #56684, .T. ) ;
#9156 = EDGE_CURVE ( 'NONE', #56327, #62784, #15059, .T. ) ;
#9157 = DIRECTION ( 'NONE',  ( 0.000000000000000000, 0.000000000000000000, 1.000000000000000000 ) ) ;
#9158 = CARTESIAN_POINT ( 'NONE',  ( 1.719304012339893939, -12.38166659046436457, -2.961219984258754767 ) ) ;
#9159 = CARTESIAN_POINT ( 'NONE',  ( -22.27706485742869091, 1.508175983031630585, -3.358064672837109743 ) ) ;
#9160 = ORIENTED_EDGE ( 'NONE', *, *, #16306, .T. ) ;
#9161 = ORIENTED_EDGE ( 'NONE', *, *, #15629, .T. ) ;
#9162 = CARTESIAN_POINT ( 'NONE',  ( 1.020182472821641095, 3.852445298735904800, 11.88926988381970062 ) ) ;
#9163 = FILL_AREA_STYLE_COLOUR ( '', #43555 ) ;
#9164 = CARTESIAN_POINT ( 'NONE',  ( -35.00000000000000000, -11.59605747147782928, -5.300372733891765442 ) ) ;
#9165 = ADVANCED_FACE ( 'NONE', ( #35059 ), #10796, .T. ) ;
#9166 = CARTESIAN_POINT ( 'NONE',  ( 47.00000000000000711, 4.705694406421931860E-17, -3.469127814946512892E-15 ) ) ;
#9167 = CARTESIAN_POINT ( 'NONE',  ( -36.00000000000000711, 10.23119532541083743, -7.608228585767615293 ) ) ;
#9168 = EDGE_CURVE ( 'NONE', #35378, #26733, #30097, .T. ) ;
#9169 = CARTESIAN_POINT ( 'NONE',  ( 7.302720544406653858, -6.253920029920363000, -11.96596573125614960 ) ) ;
#9170 = CARTESIAN_POINT ( 'NONE',  ( 35.00000000000000000, 12.17626345777663488, -0.4993900848167889817 ) ) ;
#9171 = EDGE_CURVE ( 'NONE', #38878, #32743, #44722, .T. ) ;
#9172 = CARTESIAN_POINT ( 'NONE',  ( 3.031336079629019409, 6.309383307296303478, 4.750429016921764891 ) ) ;
#9173 = DIRECTION ( 'NONE',  ( -0.9790892447477997917, -0.2034311943119418153, 0.000000000000000000 ) ) ;
#9174 = ORIENTED_EDGE ( 'NONE', *, *, #22821, .F. ) ;
#9175 = CARTESIAN_POINT ( 'NONE',  ( 0.2651627682582915480, 12.07509313786332683, 2.039709641845623533 ) ) ;
#9176 = CARTESIAN_POINT ( 'NONE',  ( 5.516018279890452902, -0.005976902763918694010, -0.003191189039764501679 ) ) ;
#9177 = DIRECTION ( 'NONE',  ( -1.000000000000000000, 0.000000000000000000, 0.000000000000000000 ) ) ;
#9178 = AXIS2_PLACEMENT_3D ( 'NONE', #43999, #3790, #13399 ) ;
#9179 = EDGE_CURVE ( 'NONE', #59672, #60252, #24386, .T. ) ;
#9180 = CIRCLE ( 'NONE', #58045, 12.75000000000000178 ) ;
#9181 = CARTESIAN_POINT ( 'NONE',  ( 3.100650473569728671, -6.622643684997354008, -4.345221797103567596 ) ) ;
#9182 = LINE ( 'NONE', #38805, #44641 ) ;
#9183 = ORIENTED_EDGE ( 'NONE', *, *, #5347, .F. ) ;
#9184 = CARTESIAN_POINT ( 'NONE',  ( -22.51237073810381517, 4.418556976583594142, -0.2145858836691955096 ) ) ;
#9185 = FACE_OUTER_BOUND ( 'NONE', #47747, .T. ) ;
#9186 = CARTESIAN_POINT ( 'NONE',  ( -8.315422948566315142, -32.37591480791618892, -12.77210737139424523 ) ) ;
#9187 = VERTEX_POINT ( 'NONE', #17096 ) ;
#9188 = CARTESIAN_POINT ( 'NONE',  ( 37.00000000000000711, 4.705694406421931860E-17, -3.469127814946512892E-15 ) ) ;
#9189 = CARTESIAN_POINT ( 'NONE',  ( -27.88094468144726790, -11.21297357817068452, -7.541748090003880911 ) ) ;
#9190 = DIRECTION ( 'NONE',  ( 1.000000000000000000, -0.000000000000000000, -0.000000000000000000 ) ) ;
#9191 = CARTESIAN_POINT ( 'NONE',  ( 0.3675815128205894289, -10.50067073900656212, 6.367184624550128014 ) ) ;
#9192 = CARTESIAN_POINT ( 'NONE',  ( 0.3675815128205912052, -11.44679196252412368, 4.447030445008141264 ) ) ;
#9193 = CARTESIAN_POINT ( 'NONE',  ( 0.5547464869798230946, 12.09851097165512535, -2.442933571354846123 ) ) ;
#9194 = VERTEX_POINT ( 'NONE', #51713 ) ;
#9195 = DIRECTION ( 'NONE',  ( -1.000000000000000000, -0.000000000000000000, -0.000000000000000000 ) ) ;
#9196 = EDGE_CURVE ( 'NONE', #21896, #22627, #22405, .T. ) ;
#9197 = CARTESIAN_POINT ( 'NONE',  ( 36.00000000000000711, -11.47561260193572963, 5.556331110570524423 ) ) ;
#9198 = DIRECTION ( 'NONE',  ( 0.000000000000000000, -1.000000000000000000, 0.000000000000000000 ) ) ;
#9199 = CARTESIAN_POINT ( 'NONE',  ( 2.665405856346787061, -7.686816759402902655, 5.696318245876803132 ) ) ;
#9200 = CARTESIAN_POINT ( 'NONE',  ( -35.00000000000000000, 2.772148766916116891, 11.86701198550357361 ) ) ;
#9201 = CARTESIAN_POINT ( 'NONE',  ( 0.3675815128205894289, -5.910255304480521055, 10.76447900494938459 ) ) ;
#9202 = DIRECTION ( 'NONE',  ( 0.000000000000000000, -0.7790879021242440583, 0.6269146997508067143 ) ) ;
#9203 = DIRECTION ( 'NONE',  ( -1.000000000000000000, -0.000000000000000000, 0.000000000000000000 ) ) ;
#9204 = ORIENTED_EDGE ( 'NONE', *, *, #18430, .T. ) ;
#9205 = ORIENTED_EDGE ( 'NONE', *, *, #64676, .T. ) ;
#9206 = CARTESIAN_POINT ( 'NONE',  ( 0.2638984909335716500, 12.09426044257626742, -1.930290337333932627 ) ) ;
#9207 = ORIENTED_EDGE ( 'NONE', *, *, #38065, .F. ) ;
#9208 = CARTESIAN_POINT ( 'NONE',  ( -28.67667724226168602, -1.812862320140641526, 0.5419187306520707459 ) ) ;
#9209 = DIRECTION ( 'NONE',  ( 0.6088860180392798860, 0.7932577242209933877, 0.000000000000000000 ) ) ;
#9210 = EDGE_LOOP ( 'NONE', ( #51044, #42750, #39048, #8165 ) ) ;
#9211 = CARTESIAN_POINT ( 'NONE',  ( 0.2647959493198550618, 5.995292100780939215, -10.67808515296904837 ) ) ;
#9212 = CARTESIAN_POINT ( 'NONE',  ( 12.18100207966124415, 11.65630975953624393, -2.856157803748045509 ) ) ;
#9213 = CARTESIAN_POINT ( 'NONE',  ( 2.273267844205340449, -5.029122824446064399, -5.758000272829230326 ) ) ;
#9214 = ORIENTED_EDGE ( 'NONE', *, *, #27357, .F. ) ;
#9215 = ORIENTED_EDGE ( 'NONE', *, *, #42615, .F. ) ;
#9216 = CARTESIAN_POINT ( 'NONE',  ( 2.835339799623982859, 0.3287452556171773788, -7.825540862019408017 ) ) ;
#9217 = EDGE_CURVE ( 'NONE', #16581, #30718, #4385, .T. ) ;
#9218 = EDGE_CURVE ( 'NONE', #37190, #25841, #53215, .T. ) ;
#9219 = DIRECTION ( 'NONE',  ( 1.000000000000000000, 0.000000000000000000, 0.000000000000000000 ) ) ;
#9220 = ORIENTED_EDGE ( 'NONE', *, *, #3489, .T. ) ;
#9221 = CIRCLE ( 'NONE', #17704, 4.999999999999999112 ) ;
#9222 = LINE ( 'NONE', #49807, #193 ) ;
#9223 = EDGE_LOOP ( 'NONE', ( #19969, #30951, #8666, #33867 ) ) ;
#9224 = CARTESIAN_POINT ( 'NONE',  ( 2.000000000000001776, 5.888698556700818543, -3.665823448873358981 ) ) ;
#9225 = EDGE_CURVE ( 'NONE', #11368, #34549, #56381, .T. ) ;
#9226 = DIRECTION ( 'NONE',  ( -1.000000000000000000, 0.000000000000000000, 0.000000000000000000 ) ) ;
#9227 = DIRECTION ( 'NONE',  ( 1.000000000000000000, -0.000000000000000000, 0.000000000000000000 ) ) ;
#9228 = FACE_OUTER_BOUND ( 'NONE', #51913, .T. ) ;
#9229 = AXIS2_PLACEMENT_3D ( 'NONE', #50296, #4751, #10041 ) ;
#9230 = CARTESIAN_POINT ( 'NONE',  ( 36.00000000000000711, -9.506317355798431734, -8.496612874013129257 ) ) ;
#9231 = ORIENTED_EDGE ( 'NONE', *, *, #41570, .F. ) ;
#9232 = CARTESIAN_POINT ( 'NONE',  ( 2.259830038565000532, -1.462175769136897285, 7.499347412930719159 ) ) ;
#9233 = CARTESIAN_POINT ( 'NONE',  ( -18.08686583997241115, 5.151216734910855521, 10.83812558286605920 ) ) ;
#9234 = CARTESIAN_POINT ( 'NONE',  ( 37.00000000000000711, -12.09831040184922912, 1.463443770872898453 ) ) ;
#9235 = CARTESIAN_POINT ( 'NONE',  ( -37.00000000000000711, 0.000000000000000000, 0.000000000000000000 ) ) ;
#9236 = CARTESIAN_POINT ( 'NONE',  ( 2.241352910868908754, -7.532448145350516988, 1.243507963608069700 ) ) ;
#9237 = CARTESIAN_POINT ( 'NONE',  ( -27.08935880048797529, 1.608762129669642604, -1.653090150968472116 ) ) ;
#9238 = CARTESIAN_POINT ( 'NONE',  ( 19.28625800530497258, -6.413918128308385036, 11.87904264843581537 ) ) ;
#9239 = CARTESIAN_POINT ( 'NONE',  ( 2.000000000000001776, -6.906413915731171471, -0.6453518998148326524 ) ) ;
#9240 = LINE ( 'NONE', #30192, #22547 ) ;
#9241 = EDGE_CURVE ( 'NONE', #55845, #21734, #23449, .T. ) ;
#9242 = VERTEX_POINT ( 'NONE', #52029 ) ;
#9243 = CARTESIAN_POINT ( 'NONE',  ( 0.3341166715381279628, 0.2526177176100057875, 12.26652061402056049 ) ) ;
#9244 = ORIENTED_EDGE ( 'NONE', *, *, #1259, .F. ) ;
#9245 = FACE_OUTER_BOUND ( 'NONE', #11503, .T. ) ;
#9246 = CARTESIAN_POINT ( 'NONE',  ( 2.305787727787084851, -7.508843116234144688, -1.493241775258500770 ) ) ;
#9247 = CARTESIAN_POINT ( 'NONE',  ( 2.241352910868908310, -4.970878533273800137, 5.794346703933830334 ) ) ;
#9248 = FACE_OUTER_BOUND ( 'NONE', #12217, .T. ) ;
#9249 = DIRECTION ( 'NONE',  ( -1.000000000000000000, 0.000000000000000000, 0.000000000000000000 ) ) ;
#9250 = ORIENTED_EDGE ( 'NONE', *, *, #2579, .F. ) ;
#9251 = CARTESIAN_POINT ( 'NONE',  ( 0.2638984909335720941, 7.718810690099187077, -9.508791614589117813 ) ) ;
#9252 = DIRECTION ( 'NONE',  ( 0.000000000000000000, -0.8835120444460272671, 0.4684084406997818251 ) ) ;
#9253 = FACE_OUTER_BOUND ( 'NONE', #52814, .T. ) ;
#9254 = CARTESIAN_POINT ( 'NONE',  ( 10.04668509498159601, -32.26295471731898346, -12.85148783289987939 ) ) ;
#9255 = ADVANCED_FACE ( 'NONE', ( #1819 ), #11139, .T. ) ;
#9256 = CARTESIAN_POINT ( 'NONE',  ( 37.00000000000000711, 11.42599468261429152, -4.237620530777845396 ) ) ;
#9257 = ORIENTED_EDGE ( 'NONE', *, *, #41690, .F. ) ;
#9258 = CARTESIAN_POINT ( 'NONE',  ( -18.55764555710201336, 11.94984199981902862, 1.281878970701318510 ) ) ;
#9259 = ORIENTED_EDGE ( 'NONE', *, *, #28512, .F. ) ;
#9260 = DIRECTION ( 'NONE',  ( 0.000000000000000000, 0.01356324068817992175, -0.9999080150203990547 ) ) ;
#9261 = DIRECTION ( 'NONE',  ( 1.000000000000000000, 0.000000000000000000, 0.000000000000000000 ) ) ;
#9262 = B_SPLINE_CURVE_WITH_KNOTS ( 'NONE', 3,
 ( #40158, #60451, #9916, #30203, #50501, #4944, #25205, #60791, #15227, #55809, #10236, #18923, #6251, #26200, #1602, #15550, #26514, #926, #31191, #31816 ),
 .UNSPECIFIED., .F., .F.,
 ( 4, 2, 2, 2, 2, 2, 2, 2, 2, 4 ),
 ( 0.002662675774314247901, 0.003376488722711035520, 0.004090301671107823139, 0.004804114619504610759, 0.005517927567901398378, 0.006231740516298185997, 0.006945553464694973617, 0.007659366413091766440, 0.008016272887290162852, 0.008373179361488559264 ),
 .UNSPECIFIED. ) ;
#9263 = AXIS2_PLACEMENT_3D ( 'NONE', #8916, #29206, #49503 ) ;
#9264 = CARTESIAN_POINT ( 'NONE',  ( 35.00000000000000000, 12.16632754454236398, -0.7008968033239244555 ) ) ;
#9265 = CARTESIAN_POINT ( 'NONE',  ( 6.521272285098597798, -4.688064980771462942, 12.66474591211187040 ) ) ;
#9266 = VERTEX_POINT ( 'NONE', #22081 ) ;
#9267 = ORIENTED_EDGE ( 'NONE', *, *, #12328, .F. ) ;
#9268 = FACE_OUTER_BOUND ( 'NONE', #21409, .T. ) ;
#9269 = ORIENTED_EDGE ( 'NONE', *, *, #10532, .T. ) ;
#9270 = EDGE_CURVE ( 'NONE', #26831, #49092, #7538, .T. ) ;
#9271 = CARTESIAN_POINT ( 'NONE',  ( 5.515539859299206427, 0.003193223631739254900, 0.005142293699651879005 ) ) ;
#9272 = FACE_OUTER_BOUND ( 'NONE', #11175, .T. ) ;
#9273 = CARTESIAN_POINT ( 'NONE',  ( 2.261269890823173423, 6.546486799462753581, 3.940687015736990872 ) ) ;
#9274 = CARTESIAN_POINT ( 'NONE',  ( 2.000000000000001776, -5.396716205731396876, -4.158041573745144603 ) ) ;
#9275 = CARTESIAN_POINT ( 'NONE',  ( 0.2717059086739047058, 9.268607328094642384, -8.007130974639942167 ) ) ;
#9276 = DIRECTION ( 'NONE',  ( 0.000000000000000000, 0.01356324068817998940, -0.9999080150203990547 ) ) ;
#9277 = CARTESIAN_POINT ( 'NONE',  ( -14.29135464769095520, 7.782112657557433089, 9.134479874907178498 ) ) ;
#9278 = EDGE_CURVE ( 'NONE', #49481, #44729, #51603, .T. ) ;
#9279 = VERTEX_POINT ( 'NONE', #32052 ) ;
#9280 = VERTEX_POINT ( 'NONE', #16459 ) ;
#9281 = ORIENTED_EDGE ( 'NONE', *, *, #31984, .F. ) ;
#9282 = CARTESIAN_POINT ( 'NONE',  ( 1.194176325881334710, -2.684784923266205769, -12.26540585042612186 ) ) ;
#9283 = DIRECTION ( 'NONE',  ( 0.000000000000000000, -0.1764146379942750642, -0.9843159429275485373 ) ) ;
#9284 = EDGE_CURVE ( 'NONE', #54109, #26729, #11446, .T. ) ;
#9285 = EDGE_LOOP ( 'NONE', ( #49688, #8722, #23848, #46499 ) ) ;
#9286 = FACE_BOUND ( 'NONE', #7018, .T. ) ;
#9287 = VERTEX_POINT ( 'NONE', #26753 ) ;
#9288 = CYLINDRICAL_SURFACE ( 'NONE', #49281, 5.000000000000000888 ) ;
#9289 = CARTESIAN_POINT ( 'NONE',  ( 0.2646305136544072623, 1.996350543473155437, -12.08286001766533602 ) ) ;
#9290 = CARTESIAN_POINT ( 'NONE',  ( 7.006458457944364504, -4.543415500168663357, 11.11500136487966195 ) ) ;
#9291 = ORIENTED_EDGE ( 'NONE', *, *, #28278, .T. ) ;
#9292 = ORIENTED_EDGE ( 'NONE', *, *, #54044, .T. ) ;
#9293 = CARTESIAN_POINT ( 'NONE',  ( 37.00000000000000711, -12.08216339958901564, -1.591260454995201412 ) ) ;
#9294 = ORIENTED_EDGE ( 'NONE', *, *, #3077, .F. ) ;
#9295 = EDGE_CURVE ( 'NONE', #23378, #45003, #48419, .T. ) ;
#9296 = EDGE_CURVE ( 'NONE', #43631, #1814, #36401, .T. ) ;
#9297 = ORIENTED_EDGE ( 'NONE', *, *, #19357, .F. ) ;
#9298 = VERTEX_POINT ( 'NONE', #52369 ) ;
#9299 = ORIENTED_EDGE ( 'NONE', *, *, #21661, .F. ) ;
#9300 = CARTESIAN_POINT ( 'NONE',  ( 37.00000000000000711, -1.262958560998847624, -12.12087942037209665 ) ) ;
#9302 = CIRCLE ( 'NONE', #60291, 12.18650000000000233 ) ;
#9301 = CARTESIAN_POINT ( 'NONE',  ( -16.48166895389446296, -34.42998396492354374, -6.120168360281142306 ) ) ;
#9303 = DIRECTION ( 'NONE',  ( 1.000000000000000000, 0.000000000000000000, 0.000000000000000000 ) ) ;
#9304 = CARTESIAN_POINT ( 'NONE',  ( 35.00000000000000000, -8.235637554476710420, -9.733281772932135922 ) ) ;
#9305 = ORIENTED_EDGE ( 'NONE', *, *, #43203, .F. ) ;
#9306 = CARTESIAN_POINT ( 'NONE',  ( 2.298277635560276533, -7.133696409974374930, -2.772101951899035743 ) ) ;
#9307 = ORIENTED_EDGE ( 'NONE', *, *, #53734, .T. ) ;
#9308 =( BOUNDED_SURFACE ( )  B_SPLINE_SURFACE ( 3, 1, ( 
 ( #41469, #62108 ),
 ( #61122, #15556 ),
 ( #61766, #932 ),
 ( #36506, #56815 ) ),
 .UNSPECIFIED., .F., .F., .F. ) 
 B_SPLINE_SURFACE_WITH_KNOTS ( ( 4, 4 ),
 ( 2, 2 ),
 ( 0.000000000000000000, 1.000000000000000000 ),
 ( 0.000000000000000000, 1.000000000000000000 ),
 .UNSPECIFIED. ) 
 GEOMETRIC_REPRESENTATION_ITEM ( )  RATIONAL_B_SPLINE_SURFACE ( (
 ( 1.000000000000000000, 1.000000000000000000),
 ( 0.9942764183789327692, 0.8450855930916585379),
 ( 0.9942764183789327692, 0.8450855930916585379),
 ( 1.000000000000000000, 1.000000000000000000) ) ) 
 REPRESENTATION_ITEM ( '' )  SURFACE ( )  );
#9309 = CYLINDRICAL_SURFACE ( 'NONE', #11502, 5.000000000000000888 ) ;
#9310 = CARTESIAN_POINT ( 'NONE',  ( -35.00000000000000000, 0.000000000000000000, 0.000000000000000000 ) ) ;
#9311 = ORIENTED_EDGE ( 'NONE', *, *, #41123, .F. ) ;
#9312 = CARTESIAN_POINT ( 'NONE',  ( -27.01437459610461644, 13.31613970204373132, -2.220455681983952267 ) ) ;
#9313 = CARTESIAN_POINT ( 'NONE',  ( -47.00000000000000711, 0.000000000000000000, 0.000000000000000000 ) ) ;
#9314 = CARTESIAN_POINT ( 'NONE',  ( 9.687175622948609899, 25.00000000000000000, -0.5854820436212360146 ) ) ;
#9315 = AXIS2_PLACEMENT_3D ( 'NONE', #61660, #22407, #17441 ) ;
#9316 = ORIENTED_EDGE ( 'NONE', *, *, #35720, .F. ) ;
#9317 = ORIENTED_EDGE ( 'NONE', *, *, #10327, .T. ) ;
#9318 = AXIS2_PLACEMENT_3D ( 'NONE', #32033, #61639, #56691 ) ;
#9319 = CARTESIAN_POINT ( 'NONE',  ( 2.266490820343227242, -7.641399530653802508, 0.1453321357832486060 ) ) ;
#9320 = VERTEX_POINT ( 'NONE', #42033 ) ;
#9321 = DIRECTION ( 'NONE',  ( 0.000000000000000000, 0.000000000000000000, -1.000000000000000000 ) ) ;
#9322 = CARTESIAN_POINT ( 'NONE',  ( 1.719304012338249921, 10.22720798541395837, 7.581471372740089976 ) ) ;
#9323 = CARTESIAN_POINT ( 'NONE',  ( -18.06522620542768820, -29.74877956674518487, 8.189528952361769143 ) ) ;
#9324 = CARTESIAN_POINT ( 'NONE',  ( 0.2833330754217411873, -9.254504746325737941, -8.029341648258453645 ) ) ;
#9325 = CARTESIAN_POINT ( 'NONE',  ( 11.70595570239210836, 11.89565203838692575, -1.585121128597035467 ) ) ;
#9326 = EDGE_LOOP ( 'NONE', ( #37507, #20381, #63236, #57303, #16987 ) ) ;
#9327 = EDGE_CURVE ( 'NONE', #28181, #37836, #24537, .T. ) ;
#9328 = DIRECTION ( 'NONE',  ( -1.000000000000000000, 0.000000000000000000, 0.000000000000000000 ) ) ;
#9329 = CARTESIAN_POINT ( 'NONE',  ( 1.198791140418550283, 1.670544840358248351, 12.44572864632773523 ) ) ;
#9330 = EDGE_CURVE ( 'NONE', #56916, #95, #44690, .T. ) ;
#9331 = CARTESIAN_POINT ( 'NONE',  ( 0.2872850955227769787, -12.10187515377841727, -1.921748909352280821 ) ) ;
#9332 = CARTESIAN_POINT ( 'NONE',  ( 2.963017218115622686, -5.350609950027704009, 5.778072204777623178 ) ) ;
#9333 = DIRECTION ( 'NONE',  ( -1.000000000000000000, 0.000000000000000000, 0.000000000000000000 ) ) ;
#9334 = DIRECTION ( 'NONE',  ( 0.000000000000000000, -0.01356324068817998940, 0.9999080150203990547 ) ) ;
#9335 = CARTESIAN_POINT ( 'NONE',  ( 47.00000000000000711, 4.705694406421931860E-17, -3.469127814946512892E-15 ) ) ;
#9336 = AXIS2_PLACEMENT_3D ( 'NONE', #54810, #30495, #55115 ) ;
#9337 = ADVANCED_FACE ( 'NONE', ( #38700 ), #48682, .T. ) ;
#9338 = ORIENTED_EDGE ( 'NONE', *, *, #40363, .T. ) ;
#9339 = DIRECTION ( 'NONE',  ( 1.000000000000000000, 0.000000000000000000, 0.000000000000000000 ) ) ;
#9340 = AXIS2_PLACEMENT_3D ( 'NONE', #24985, #24311, #64227 ) ;
#9342 = ORIENTED_EDGE ( 'NONE', *, *, #62596, .F. ) ;
#9341 = ADVANCED_FACE ( 'NONE', ( #58330 ), #29323, .F. ) ;
#9343 = DIRECTION ( 'NONE',  ( -1.000000000000000000, 0.000000000000000000, 0.000000000000000000 ) ) ;
#9344 = ADVANCED_FACE ( 'NONE', ( #53345 ), #8434, .T. ) ;
#9345 = DIRECTION ( 'NONE',  ( 0.000000000000000000, 0.9467777615094582488, 0.3218879778915939571 ) ) ;
#9346 = FACE_OUTER_BOUND ( 'NONE', #42395, .T. ) ;
#9347 = AXIS2_PLACEMENT_3D ( 'NONE', #4845, #30419, #45710 ) ;
#9348 = CARTESIAN_POINT ( 'NONE',  ( -35.00000000000000000, 9.506317355798367785, 8.496612874013193206 ) ) ;
#9349 = EDGE_CURVE ( 'NONE', #57134, #30777, #17090, .T. ) ;
#9350 = VERTEX_POINT ( 'NONE', #53990 ) ;
#9351 = ORIENTED_EDGE ( 'NONE', *, *, #37764, .F. ) ;
#9352 = CIRCLE ( 'NONE', #19968, 12.74999999999999822 ) ;
#9353 = ORIENTED_EDGE ( 'NONE', *, *, #14028, .F. ) ;
#9354 = CARTESIAN_POINT ( 'NONE',  ( -27.35552965826135008, 3.094132632038936404, 0.2619431035391969198 ) ) ;
#9355 = CARTESIAN_POINT ( 'NONE',  ( -27.01437459610461644, 11.79277645698183363, -2.220455681983952267 ) ) ;
#9356 = EDGE_CURVE ( 'NONE', #38593, #37413, #54271, .T. ) ;
#9357 = ORIENTED_EDGE ( 'NONE', *, *, #25393, .T. ) ;
#9358 = DIRECTION ( 'NONE',  ( 0.000000000000000000, 0.8009703041134188517, 0.5987040770935649903 ) ) ;
#9359 = CARTESIAN_POINT ( 'NONE',  ( 3.347841273039249721, -10.61118957148187825, -8.345816669330458737 ) ) ;
#9360 = CARTESIAN_POINT ( 'NONE',  ( 0.2717059086739019302, -9.268607328094583764, 8.007130974640009669 ) ) ;
#9361 = FACE_OUTER_BOUND ( 'NONE', #30196, .T. ) ;
#9362 = ORIENTED_EDGE ( 'NONE', *, *, #63970, .T. ) ;
#9363 = DIRECTION ( 'NONE',  ( 0.000000000000000000, 0.5243256840888563808, 0.8515178078024868702 ) ) ;
#9364 = EDGE_CURVE ( 'NONE', #21416, #12178, #49021, .T. ) ;
#9365 = CARTESIAN_POINT ( 'NONE',  ( 4.225235259830945722, -26.75987402110986579, -15.91411249164890407 ) ) ;
#9366 = DIRECTION ( 'NONE',  ( -1.000000000000000000, 0.000000000000000000, 0.000000000000000000 ) ) ;
#9368 = ORIENTED_EDGE ( 'NONE', *, *, #62318, .F. ) ;
#9367 = LINE ( 'NONE', #29992, #48967 ) ;
#9369 = CARTESIAN_POINT ( 'NONE',  ( 35.00000000000000000, 9.896810808925392777, -7.110831038798317572 ) ) ;
#9370 = ORIENTED_EDGE ( 'NONE', *, *, #11023, .F. ) ;
#9371 = CARTESIAN_POINT ( 'NONE',  ( 0.8375941296802502656, -9.769835228044227549, 7.696026447556238992 ) ) ;
#9372 = ORIENTED_EDGE ( 'NONE', *, *, #37142, .F. ) ;
#9373 = CYLINDRICAL_SURFACE ( 'NONE', #53923, 1.500000000000000222 ) ;
#9374 = CARTESIAN_POINT ( 'NONE',  ( 11.72287332632499179, -11.90030359961621009, -1.578241357430486769 ) ) ;
#9375 = LINE ( 'NONE', #49007, #11734 ) ;
#9376 = CARTESIAN_POINT ( 'NONE',  ( 0.9232167919969179737, -6.587352952801085237, -10.58277433962388159 ) ) ;
#9378 = CARTESIAN_POINT ( 'NONE',  ( 0.3675815128205894289, -12.27743992903066328, 0.2638082659427993804 ) ) ;
#9377 = AXIS2_PLACEMENT_3D ( 'NONE', #64144, #58516, #39515 ) ;
#9379 = CARTESIAN_POINT ( 'NONE',  ( -5.388163386660410836, -1.427464897260812160, -13.42432405772846238 ) ) ;
#9380 = CARTESIAN_POINT ( 'NONE',  ( -35.00000000000000000, -12.12087942037210553, 1.262958560998716617 ) ) ;
#9382 = ORIENTED_EDGE ( 'NONE', *, *, #35425, .F. ) ;
#9381 = CARTESIAN_POINT ( 'NONE',  ( 35.00000000000000000, -11.95840593935202811, -2.346765782874394635 ) ) ;
#9383 = EDGE_CURVE ( 'NONE', #54788, #22230, #52306, .T. ) ;
#9384 = VERTEX_POINT ( 'NONE', #3479 ) ;
#9385 = DIRECTION ( 'NONE',  ( 0.000000000000000000, -0.7381862504171877726, 0.6745969609292743474 ) ) ;
#9386 = ORIENTED_EDGE ( 'NONE', *, *, #916, .T. ) ;
#9387 = APPLICATION_CONTEXT ( 'automotive_design' ) ;
#9388 = ORIENTED_EDGE ( 'NONE', *, *, #23337, .F. ) ;
#9389 = CARTESIAN_POINT ( 'NONE',  ( 0.2801149460245128120, 8.024198546827475909, 9.257544930777182657 ) ) ;
#9390 = DIRECTION ( 'NONE',  ( 0.000000000000000000, -0.01356324068817998940, 0.9999080150203990547 ) ) ;
#9391 = CARTESIAN_POINT ( 'NONE',  ( -35.00000000000000000, -4.603882218679629545, 10.80631716521665453 ) ) ;
#9392 = CARTESIAN_POINT ( 'NONE',  ( 0.2648978790185584908, 0.1321385342564118659, -12.24533305150758089 ) ) ;
#9393 = DIRECTION ( 'NONE',  ( -1.000000000000000000, 0.000000000000000000, 0.000000000000000000 ) ) ;
#9394 = AXIS2_PLACEMENT_3D ( 'NONE', #28149, #17838, #33465 ) ;
#9395 = CARTESIAN_POINT ( 'NONE',  ( 2.269879328255106188, 7.232310762823190409, 2.474479066009427353 ) ) ;
#9396 = FACE_OUTER_BOUND ( 'NONE', #24379, .T. ) ;
#9397 = AXIS2_PLACEMENT_3D ( 'NONE', #44930, #49927, #23687 ) ;
#9398 = ORIENTED_EDGE ( 'NONE', *, *, #25913, .F. ) ;
#9399 = CARTESIAN_POINT ( 'NONE',  ( -4.989057617119008192, -0.9162120371760335003, -13.46887357958837406 ) ) ;
#9400 = CARTESIAN_POINT ( 'NONE',  ( -35.00000000000000000, 0.000000000000000000, 0.000000000000000000 ) ) ;
#9401 = AXIS2_PLACEMENT_3D ( 'NONE', #6390, #26661, #46956 ) ;
#9402 = CARTESIAN_POINT ( 'NONE',  ( 0.2651627682582908818, -7.938957913267695510, -9.324228491541607156 ) ) ;
#9403 = VERTEX_POINT ( 'NONE', #13413 ) ;
#9404 = CIRCLE ( 'NONE', #46587, 2.899999999999995026 ) ;
#9405 = EDGE_CURVE ( 'NONE', #36570, #5549, #62733, .T. ) ;
#9406 = CARTESIAN_POINT ( 'NONE',  ( -7.358538974955358469, -1.423543355122588672, 13.42505237639485038 ) ) ;
#9407 = CARTESIAN_POINT ( 'NONE',  ( -35.04709527796842394, -0.01232256164996302361, -0.001003525937983557048 ) ) ;
#9408 = CARTESIAN_POINT ( 'NONE',  ( -47.41971561978370175, -0.5128904950766028925, -11.09198065024577851 ) ) ;
#9409 = VERTEX_POINT ( 'NONE', #63294 ) ;
#9410 = CARTESIAN_POINT ( 'NONE',  ( 2.262775599886257538, 6.687241191563714438, -3.697834000591571524 ) ) ;
#9411 = CARTESIAN_POINT ( 'NONE',  ( 0.000000000000000000, 6.906413915731192787, 0.6453518998147528274 ) ) ;
#9412 = CARTESIAN_POINT ( 'NONE',  ( 35.00000000000000000, 0.01609748574445066943, -11.74614673114903773 ) ) ;
#9413 = VECTOR ( 'NONE', #48426, 1000.000000000000000 ) ;
#9414 = EDGE_CURVE ( 'NONE', #8078, #42463, #12748, .T. ) ;
#9415 = CYLINDRICAL_SURFACE ( 'NONE', #20358, 4.999999999999999112 ) ;
#9416 = DIRECTION ( 'NONE',  ( 0.000000000000000000, 0.8169148498130256453, -0.5767582926624997830 ) ) ;
#9417 = ORIENTED_EDGE ( 'NONE', *, *, #18184, .F. ) ;
#9418 = VECTOR ( 'NONE', #33697, 1000.000000000000000 ) ;
#9419 = ADVANCED_FACE ( 'NONE', ( #38020 ), #44016, .T. ) ;
#9420 = CARTESIAN_POINT ( 'NONE',  ( 2.269879328256732887, 0.1483462450597243520, 7.642470739868881147 ) ) ;
#9421 = CARTESIAN_POINT ( 'NONE',  ( -7.904491797223720972, -5.813757704850941899, -10.52499957321815138 ) ) ;
#9422 = CARTESIAN_POINT ( 'NONE',  ( -35.00000000000000000, -7.215058775251326217, 9.821084925794544063 ) ) ;
#9423 = ORIENTED_EDGE ( 'NONE', *, *, #30198, .F. ) ;
#9424 = DIRECTION ( 'NONE',  ( 1.000000000000000000, 0.000000000000000000, 0.000000000000000000 ) ) ;
#9425 = DIRECTION ( 'NONE',  ( 0.000000000000000000, -0.01356324068817998940, 0.9999080150203990547 ) ) ;
#9426 = EDGE_CURVE ( 'NONE', #11008, #41431, #4709, .T. ) ;
#9427 = ORIENTED_EDGE ( 'NONE', *, *, #17776, .T. ) ;
#9428 = VERTEX_POINT ( 'NONE', #48370 ) ;
#9429 = VERTEX_POINT ( 'NONE', #59307 ) ;
#9430 = DIRECTION ( 'NONE',  ( -1.000000000000000000, 0.000000000000000000, 0.000000000000000000 ) ) ;
#9431 = AXIS2_PLACEMENT_3D ( 'NONE', #52028, #46380, #16458 ) ;
#9432 = CIRCLE ( 'NONE', #55113, 12.74999999999999822 ) ;
#9433 = ORIENTED_EDGE ( 'NONE', *, *, #63099, .F. ) ;
#9434 = CARTESIAN_POINT ( 'NONE',  ( 1.375507693218806837, -12.30831170622582071, -2.770709900326205233 ) ) ;
#9435 = CARTESIAN_POINT ( 'NONE',  ( -35.00000000000000000, 0.000000000000000000, 0.000000000000000000 ) ) ;
#9436 = VECTOR ( 'NONE', #22956, 1000.000000000000000 ) ;
#9437 = CARTESIAN_POINT ( 'NONE',  ( 0.3675815128205912052, -6.367184624550238148, 10.50067073900649461 ) ) ;
#9438 = CARTESIAN_POINT ( 'NONE',  ( 0.2652384770603662401, 4.250454630553718971, -11.48486213386621380 ) ) ;
#9439 = ADVANCED_FACE ( 'NONE', ( #34016 ), #54333, .T. ) ;
#9440 = CARTESIAN_POINT ( 'NONE',  ( -9.081998980629425233, -32.61802400030150295, 12.41144404786857081 ) ) ;
#9441 = CARTESIAN_POINT ( 'NONE',  ( 0.3665391374699467075, -7.691255657244228772, -9.576575648339096247 ) ) ;
#9443 = ORIENTED_EDGE ( 'NONE', *, *, #34682, .T. ) ;
#9442 = CARTESIAN_POINT ( 'NONE',  ( -35.00000000000000000, 7.146664589318047156, -9.321877890560362090 ) ) ;
#9444 = CARTESIAN_POINT ( 'NONE',  ( 22.57855258442564761, -4.427776684447072952, 11.15324139578564910 ) ) ;
#9445 = ADVANCED_FACE ( 'NONE', ( #3808 ), #58676, .T. ) ;
#9446 = ORIENTED_EDGE ( 'NONE', *, *, #54269, .F. ) ;
#9447 = CARTESIAN_POINT ( 'NONE',  ( 37.00000000000000711, 4.705694406421931860E-17, -3.469127814946512892E-15 ) ) ;
#9448 = EDGE_LOOP ( 'NONE', ( #4080, #23351, #56160, #53985 ) ) ;
#9449 = CIRCLE ( 'NONE', #20062, 12.73084802173761787 ) ;
#9450 = VERTEX_POINT ( 'NONE', #50333 ) ;
#9451 = CARTESIAN_POINT ( 'NONE',  ( 37.00000000000000711, -2.936739658819788712, 11.37311665002366290 ) ) ;
#9452 = EDGE_CURVE ( 'NONE', #56769, #51818, #29692, .T. ) ;
#9453 = CARTESIAN_POINT ( 'NONE',  ( 15.07617326819577741, -33.99933334076661851, 8.515830899730941539 ) ) ;
#9454 = CARTESIAN_POINT ( 'NONE',  ( -35.00000000000000000, 0.000000000000000000, 0.000000000000000000 ) ) ;
#9455 = FACE_OUTER_BOUND ( 'NONE', #35131, .T. ) ;
#9456 = LINE ( 'NONE', #8830, #61093 ) ;
#9457 = CARTESIAN_POINT ( 'NONE',  ( 37.00000000000000711, 10.49626516989280844, 7.238157050195514586 ) ) ;
#9459 = VERTEX_POINT ( 'NONE', #34665 ) ;
#9458 = EDGE_CURVE ( 'NONE', #39295, #30401, #13181, .T. ) ;
#9460 = VERTEX_POINT ( 'NONE', #19737 ) ;
#9461 = CARTESIAN_POINT ( 'NONE',  ( 22.88594695219327235, -4.822122601967141264, 25.00000000000000000 ) ) ;
#9462 = ORIENTED_EDGE ( 'NONE', *, *, #9270, .F. ) ;
#9463 = EDGE_CURVE ( 'NONE', #57334, #63621, #24716, .T. ) ;
#9464 = ORIENTED_EDGE ( 'NONE', *, *, #14322, .T. ) ;
#9465 = CARTESIAN_POINT ( 'NONE',  ( 2.241352910868909643, -1.243507963608144751, 7.532448145350502777 ) ) ;
#9466 = CARTESIAN_POINT ( 'NONE',  ( -35.00000000000000000, 12.66641127287625856, 1.457575200925591341 ) ) ;
#9467 = CYLINDRICAL_SURFACE ( 'NONE', #43744, 2.899999999999994582 ) ;
#9468 = CYLINDRICAL_SURFACE ( 'NONE', #30532, 2.899999999999994582 ) ;
#9469 = CARTESIAN_POINT ( 'NONE',  ( 2.903928887688550731, 6.032681461746162377, 6.365315087928729021 ) ) ;
#9470 = VECTOR ( 'NONE', #39739, 999.9999999999998863 ) ;
#9471 = CARTESIAN_POINT ( 'NONE',  ( 28.01964047808447944, -12.64055115429361820, 4.742990486147117046 ) ) ;
#9472 = ORIENTED_EDGE ( 'NONE', *, *, #30877, .T. ) ;
#9473 = VERTEX_POINT ( 'NONE', #34355 ) ;
#9474 = DIRECTION ( 'NONE',  ( 0.000000000000000000, 0.6943713148249588407, -0.7196168960969843154 ) ) ;
#9475 = CARTESIAN_POINT ( 'NONE',  ( 37.00000000000000711, -10.84030624090611283, -6.711949091238110121 ) ) ;
#9476 = DIRECTION ( 'NONE',  ( 1.000000000000000000, 0.000000000000000000, 0.000000000000000000 ) ) ;
#9477 = B_SPLINE_CURVE_WITH_KNOTS ( 'NONE', 3,
 ( #6939, #12240, #33173, #58812, #32503, #58133, #52166, #16902, #63422, #53137, #57481, #11906, #12549, #32828, #22560, #53485, #27208, #7581, #26887 ),
 .UNSPECIFIED., .F., .F.,
 ( 4, 3, 3, 3, 3, 3, 4 ),
 ( 0.000000000000000000, 2.831840207625647068E-05, 4.217266860012731824E-05, 5.602024318566616653E-05, 6.290810168138950603E-05, 9.120440631110875748E-05, 0.0001153103026478308337 ),
 .UNSPECIFIED. ) ;
#9478 = CIRCLE ( 'NONE', #40294, 2.899999999999994582 ) ;
#9479 = EDGE_CURVE ( 'NONE', #50460, #13265, #62019, .T. ) ;
#9480 = DIRECTION ( 'NONE',  ( 1.000000000000000000, 0.000000000000000000, 0.000000000000000000 ) ) ;
#9481 = CARTESIAN_POINT ( 'NONE',  ( -37.00000000000000711, -11.68758509253249223, 1.171570255487406786 ) ) ;
#9482 = AXIS2_PLACEMENT_3D ( 'NONE', #22874, #62116, #1615 ) ;
#9483 =( BOUNDED_SURFACE ( )  B_SPLINE_SURFACE ( 3, 1, ( 
 ( #9856, #26459 ),
 ( #50446, #46745 ),
 ( #61701, #10183 ),
 ( #1206, #60734 ) ),
 .UNSPECIFIED., .F., .F., .F. ) 
 B_SPLINE_SURFACE_WITH_KNOTS ( ( 4, 4 ),
 ( 2, 2 ),
 ( 0.000000000000000000, 1.000000000000000000 ),
 ( 0.000000000000000000, 1.000000000000000000 ),
 .UNSPECIFIED. ) 
 GEOMETRIC_REPRESENTATION_ITEM ( )  RATIONAL_B_SPLINE_SURFACE ( (
 ( 1.000000000000000000, 1.000000000000000000),
 ( 0.9856612449720755231, 0.9999558406602322425),
 ( 0.9856612449720755231, 0.9999558406602322425),
 ( 1.000000000000000000, 1.000000000000000000) ) ) 
 REPRESENTATION_ITEM ( '' )  SURFACE ( )  );
#9484 = CARTESIAN_POINT ( 'NONE',  ( -10.78957422984094983, -6.332470062474154560, -10.19518144049010644 ) ) ;
#9485 = CARTESIAN_POINT ( 'NONE',  ( -37.25000000000000711, -45.00200000000000244, -4.500000000000000888 ) ) ;
#9486 = DIRECTION ( 'NONE',  ( 1.000000000000000000, 0.000000000000000000, 0.000000000000000000 ) ) ;
#9487 = DIRECTION ( 'NONE',  ( 0.000000000000000000, 0.01356324068817998940, -0.9999080150203990547 ) ) ;
#9488 = VERTEX_POINT ( 'NONE', #15386 ) ;
#9489 = CARTESIAN_POINT ( 'NONE',  ( 0.2652384529303136174, 12.07141085622972554, 2.061422456317067109 ) ) ;
#9490 = CARTESIAN_POINT ( 'NONE',  ( 2.000000000000001776, -6.606214214351077807, 2.114938770769887455 ) ) ;
#9491 = EDGE_CURVE ( 'NONE', #34871, #50610, #51458, .T. ) ;
#9492 = DIRECTION ( 'NONE',  ( 0.000000000000000000, 0.000000000000000000, 1.000000000000000000 ) ) ;
#9493 = VECTOR ( 'NONE', #36971, 1000.000000000000000 ) ;
#9494 = ADVANCED_FACE ( 'NONE', ( #14393 ), #60948, .T. ) ;
#9495 = DIRECTION ( 'NONE',  ( -1.000000000000000000, 0.000000000000000000, 0.000000000000000000 ) ) ;
#9496 = CARTESIAN_POINT ( 'NONE',  ( 0.4613984246114885002, -4.475519447653911520, -11.46927345719241131 ) ) ;
#9497 = ORIENTED_EDGE ( 'NONE', *, *, #62843, .F. ) ;
#9498 = CYLINDRICAL_SURFACE ( 'NONE', #21657, 4.999999999999999112 ) ;
#9499 = DIRECTION ( 'NONE',  ( 1.000000000000000000, 0.000000000000000000, -0.000000000000000000 ) ) ;
#9500 = CARTESIAN_POINT ( 'NONE',  ( -0.8584944786142326700, -27.82166925786467004, -12.56635396443958719 ) ) ;
#9501 = ORIENTED_EDGE ( 'NONE', *, *, #31815, .F. ) ;
#9502 = CARTESIAN_POINT ( 'NONE',  ( 2.000000000000001776, 0.000000000000000000, 0.000000000000000000 ) ) ;
#9503 = DIRECTION ( 'NONE',  ( -0.000000000000000000, -1.000000000000000000, -0.000000000000000000 ) ) ;
#9504 = CARTESIAN_POINT ( 'NONE',  ( 2.941278708680199916, 5.814102272488615775, -1.972702289975945433 ) ) ;
#9505 = ADVANCED_FACE ( 'NONE', ( #64927 ), #49727, .F. ) ;
#9506 = CARTESIAN_POINT ( 'NONE',  ( -35.00000000000000000, -9.430788938294105250, 7.718225330433773124 ) ) ;
#9507 = CARTESIAN_POINT ( 'NONE',  ( -14.17299601508879014, 8.097942500480233008, 8.858180248946752045 ) ) ;
#9508 = AXIS2_PLACEMENT_3D ( 'NONE', #54512, #55140, #29230 ) ;
#9509 = AXIS2_PLACEMENT_3D ( 'NONE', #32782, #12845, #2232 ) ;
#9510 = CARTESIAN_POINT ( 'NONE',  ( 35.00000000000000000, -2.220215194441986561, -11.98254675519227597 ) ) ;
#9511 = EDGE_LOOP ( 'NONE', ( #5793, #9386, #33307, #14343 ) ) ;
#9512 = FACE_OUTER_BOUND ( 'NONE', #23739, .T. ) ;
#9513 = CARTESIAN_POINT ( 'NONE',  ( -27.08579483061179261, 1.318128465626146051, 1.879952013013905576 ) ) ;
#9514 = CARTESIAN_POINT ( 'NONE',  ( -18.12134786527529684, 6.862502072565634492, -11.62855658186334651 ) ) ;
#9515 = DIRECTION ( 'NONE',  ( 0.000000000000000000, 0.01356324068818000848, -0.9999080150203990547 ) ) ;
#9517 = CARTESIAN_POINT ( 'NONE',  ( -35.05012975565874456, 0.005092487515914018679, -0.01296790604420075023 ) ) ;
#9516 = CIRCLE ( 'NONE', #38200, 1.500000000000000222 ) ;
#9518 = DIRECTION ( 'NONE',  ( -1.000000000000000000, 0.000000000000000000, -0.000000000000000000 ) ) ;
#9519 = CARTESIAN_POINT ( 'NONE',  ( 2.263328370259786393, 1.186889399883084950, -7.548992860188940668 ) ) ;
#9520 = ORIENTED_EDGE ( 'NONE', *, *, #19357, .T. ) ;
#9521 = ORIENTED_EDGE ( 'NONE', *, *, #65428, .F. ) ;
#9522 = CARTESIAN_POINT ( 'NONE',  ( -2.952869152607106251, 11.39722960915212724, 3.755417052241485365 ) ) ;
#9523 = ORIENTED_EDGE ( 'NONE', *, *, #39144, .F. ) ;
#9524 = EDGE_CURVE ( 'NONE', #7525, #29429, #53548, .T. ) ;
#9525 = CIRCLE ( 'NONE', #46713, 6.936499999999990784 ) ;
#9526 = CARTESIAN_POINT ( 'NONE',  ( 0.2648978790185584908, 11.46165506714228322, 4.312320170909275774 ) ) ;
#9527 = EDGE_CURVE ( 'NONE', #36878, #16830, #48285, .T. ) ;
#9528 = CARTESIAN_POINT ( 'NONE',  ( -37.00000000000000711, 4.986700593229701717, 10.63508530065523772 ) ) ;
#9529 = ORIENTED_EDGE ( 'NONE', *, *, #17249, .F. ) ;
#9530 = DIRECTION ( 'NONE',  ( 1.000000000000000000, 0.000000000000000000, 0.000000000000000000 ) ) ;
#9531 = DIRECTION ( 'NONE',  ( 1.000000000000000000, 0.000000000000000000, 0.000000000000000000 ) ) ;
#9532 = CARTESIAN_POINT ( 'NONE',  ( 22.88594695219327235, 3.421158645304719137, 13.05931366970166962 ) ) ;
#9533 = ORIENTED_EDGE ( 'NONE', *, *, #11053, .T. ) ;
#9534 = ORIENTED_EDGE ( 'NONE', *, *, #65400, .F. ) ;
#9535 = EDGE_CURVE ( 'NONE', #45642, #7784, #25304, .T. ) ;
#9536 = DIRECTION ( 'NONE',  ( 0.000000000000000000, 0.000000000000000000, 1.000000000000000000 ) ) ;
#9537 = ORIENTED_EDGE ( 'NONE', *, *, #17377, .T. ) ;
#9538 = VECTOR ( 'NONE', #64108, 1000.000000000000000 ) ;
#9539 = CARTESIAN_POINT ( 'NONE',  ( -27.09125059358653331, 0.5611156659263027979, -2.243253600381625024 ) ) ;
#9540 = ORIENTED_EDGE ( 'NONE', *, *, #20063, .F. ) ;
#9541 = CARTESIAN_POINT ( 'NONE',  ( -27.09364415740217424, 2.313349100776208811, -0.1694361397562743343 ) ) ;
#9542 = DIRECTION ( 'NONE',  ( 0.000000000000000000, -0.01356324068817991828, 0.9999080150203990547 ) ) ;
#9543 = CARTESIAN_POINT ( 'NONE',  ( 2.573738926104371938, -4.074516960797421206, 6.586859681822649470 ) ) ;
#9544 = CARTESIAN_POINT ( 'NONE',  ( 17.05023968204110929, -34.50000000000000000, 4.356789313881321846 ) ) ;
#9545 = ORIENTED_EDGE ( 'NONE', *, *, #48662, .F. ) ;
#9546 = CARTESIAN_POINT ( 'NONE',  ( 1.549075743845271358, -12.12370443967581224, 3.694639393664078231 ) ) ;
#9547 = DIRECTION ( 'NONE',  ( -1.000000000000000000, 0.000000000000000000, 0.000000000000000000 ) ) ;
#9548 = DIRECTION ( 'NONE',  ( 0.000000000000000000, 0.01356324068817998940, -0.9999080150203989437 ) ) ;
#9549 = CARTESIAN_POINT ( 'NONE',  ( 2.000000000000001776, -6.201547234537033937, 2.820401998297862978 ) ) ;
#9550 = CARTESIAN_POINT ( 'NONE',  ( 12.91288097661053236, 12.55977324591722954, -4.965784564771029252 ) ) ;
#9551 = CARTESIAN_POINT ( 'NONE',  ( 22.57855258442565116, 3.026812727784649493, 13.15630665159948975 ) ) ;
#9552 = CARTESIAN_POINT ( 'NONE',  ( -35.00000000000000000, -10.14433819232429812, -6.753013023069823539 ) ) ;
#9553 = DIRECTION ( 'NONE',  ( 0.000000000000000000, 0.9985334138511239299, -0.05413890858541457046 ) ) ;
#9554 = DIRECTION ( 'NONE',  ( -1.000000000000000000, 0.000000000000000000, 0.000000000000000000 ) ) ;
#9555 = AXIS2_PLACEMENT_3D ( 'NONE', #4639, #55148, #54837 ) ;
#9556 = EDGE_CURVE ( 'NONE', #16234, #8848, #30823, .T. ) ;
#9557 = VECTOR ( 'NONE', #40743, 1000.000000000000000 ) ;
#9558 = EDGE_LOOP ( 'NONE', ( #64335, #39643, #41692, #86 ) ) ;
#9559 = CIRCLE ( 'NONE', #64810, 250.0000000000000000 ) ;
#9560 = CARTESIAN_POINT ( 'NONE',  ( 0.3057689695767484839, 0.2309407641932738897, 12.25749431726081973 ) ) ;
#9561 = ADVANCED_FACE ( 'NONE', ( #16379 ), #36650, .T. ) ;
#9562 = ORIENTED_EDGE ( 'NONE', *, *, #31291, .T. ) ;
#9563 = CARTESIAN_POINT ( 'NONE',  ( -27.10719052120871098, -1.714424047991075506, -1.622102031466694072 ) ) ;
#9564 = CARTESIAN_POINT ( 'NONE',  ( -37.00000000000000711, -6.303578524886872536, -10.42955799785326576 ) ) ;
#9565 = CYLINDRICAL_SURFACE ( 'NONE', #5937, 12.18649999999999878 ) ;
#9566 = CARTESIAN_POINT ( 'NONE',  ( 3.092491956585399659, -7.863103788722309417, -0.9322768171845581264 ) ) ;
#9567 = CARTESIAN_POINT ( 'NONE',  ( 41.00000000000000711, -1.694065894508600678E-18, 1.500000000000000222 ) ) ;
#9568 = ORIENTED_EDGE ( 'NONE', *, *, #30256, .F. ) ;
#9569 = CARTESIAN_POINT ( 'NONE',  ( -11.20050441550567299, -9.175587222235860096, -9.916315835339821305 ) ) ;
#9570 = CARTESIAN_POINT ( 'NONE',  ( 2.242418902651939216, -3.730710532463405116, 6.661183998167589770 ) ) ;
#9571 = EDGE_CURVE ( 'NONE', #37505, #62374, #2618, .T. ) ;
#9572 = CARTESIAN_POINT ( 'NONE',  ( 11.32539125054619689, 0.8069478436655108666, 11.97338806366722785 ) ) ;
#9573 = CARTESIAN_POINT ( 'NONE',  ( 11.20282697758643842, -32.63606470323338726, -12.17568710599035420 ) ) ;
#9574 = CIRCLE ( 'NONE', #14835, 7.938172270156617749 ) ;
#9575 = AXIS2_PLACEMENT_3D ( 'NONE', #21136, #21486, #41755 ) ;
#9576 = DIRECTION ( 'NONE',  ( 1.000000000000000000, 0.000000000000000000, 0.000000000000000000 ) ) ;
#9577 = EDGE_LOOP ( 'NONE', ( #12412, #21475, #45405, #1881 ) ) ;
#9578 = CARTESIAN_POINT ( 'NONE',  ( 2.000000000000001776, -3.859771122242995123, -5.613913289150092467 ) ) ;
#9579 = ORIENTED_EDGE ( 'NONE', *, *, #56631, .F. ) ;
#9580 = CARTESIAN_POINT ( 'NONE',  ( 0.2653519789438747445, 12.24619733037256353, -0.02203059356493299384 ) ) ;
#9582 = ADVANCED_FACE ( 'NONE', ( #21701 ), #26030, .T. ) ;
#9581 = CARTESIAN_POINT ( 'NONE',  ( -13.93947072118460007, -33.60066931048350369, 9.878030726377206250 ) ) ;
#9583 = EDGE_CURVE ( 'NONE', #38770, #58222, #50358, .T. ) ;
#9584 = CIRCLE ( 'NONE', #6434, 12.18650000000000055 ) ;
#9585 = CARTESIAN_POINT ( 'NONE',  ( -30.18541646480307250, -1.416020129149132334, 25.00000000000000000 ) ) ;
#9586 = EDGE_CURVE ( 'NONE', #35395, #64071, #22320, .T. ) ;
#9587 = DIRECTION ( 'NONE',  ( 0.000000000000000000, 0.1081190184239352453, 0.9941379571543603744 ) ) ;
#9588 = ORIENTED_EDGE ( 'NONE', *, *, #13841, .F. ) ;
#9589 = ORIENTED_EDGE ( 'NONE', *, *, #36386, .T. ) ;
#9590 = DIRECTION ( 'NONE',  ( 0.000000000000000000, -0.4198891015602527754, -0.9075754196709624466 ) ) ;
#9591 = ORIENTED_EDGE ( 'NONE', *, *, #59929, .F. ) ;
#9592 = VECTOR ( 'NONE', #14049, 1000.000000000000000 ) ;
#9593 = CARTESIAN_POINT ( 'NONE',  ( 3.152665057735260845, 4.377619405893435456, 6.622010822086191517 ) ) ;
#9594 = DIRECTION ( 'NONE',  ( -1.000000000000000000, 0.000000000000000000, 0.000000000000000000 ) ) ;
#9595 = CARTESIAN_POINT ( 'NONE',  ( 35.00000000000000000, -9.493370459201747380, -6.917234959366797220 ) ) ;
#9596 = CARTESIAN_POINT ( 'NONE',  ( 0.3218525148189836371, 12.26259572563018629, 0.2444206315273586283 ) ) ;
#9597 = CYLINDRICAL_SURFACE ( 'NONE', #2488, 12.18649999999999878 ) ;
#9598 = DIRECTION ( 'NONE',  ( 1.000000000000000000, 0.000000000000000000, 0.000000000000000000 ) ) ;
#9599 = FACE_OUTER_BOUND ( 'NONE', #60697, .T. ) ;
#9600 = ORIENTED_EDGE ( 'NONE', *, *, #17354, .F. ) ;
#9601 = CIRCLE ( 'NONE', #62719, 12.18650000000000055 ) ;
#9603 = ORIENTED_EDGE ( 'NONE', *, *, #62214, .F. ) ;
#9602 = CARTESIAN_POINT ( 'NONE',  ( 0.3675815128205912052, -12.04510820461657516, -2.391755495700727874 ) ) ;
#9604 = ORIENTED_EDGE ( 'NONE', *, *, #25662, .T. ) ;
#9605 = CARTESIAN_POINT ( 'NONE',  ( -35.00000000000000000, -10.14408668126209001, -5.921969905510467314 ) ) ;
#9606 = EDGE_CURVE ( 'NONE', #23040, #44827, #20638, .T. ) ;
#9608 = LINE ( 'NONE', #63836, #35284 ) ;
#9607 = CIRCLE ( 'NONE', #57382, 7.938172270156617749 ) ;
#9609 = AXIS2_PLACEMENT_3D ( 'NONE', #65111, #38880, #50500 ) ;
#9610 = VECTOR ( 'NONE', #20082, 1000.000000000000000 ) ;
#9611 = ORIENTED_EDGE ( 'NONE', *, *, #12857, .T. ) ;
#9612 = ADVANCED_FACE ( 'NONE', ( #41956 ), #47612, .T. ) ;
#9613 = CARTESIAN_POINT ( 'NONE',  ( 35.00000000000000000, 7.499679039484058229, -9.040300684349723781 ) ) ;
#9614 = VERTEX_POINT ( 'NONE', #26667 ) ;
#9615 = CARTESIAN_POINT ( 'NONE',  ( 2.655192694324876257, 9.539062147539249636, 1.093661162899515205 ) ) ;
#9616 = CARTESIAN_POINT ( 'NONE',  ( 6.471884597807777695, -7.981883161988641895, -10.89336526951398021 ) ) ;
#9617 = DIRECTION ( 'NONE',  ( 0.000000000000000000, 0.000000000000000000, 1.000000000000000000 ) ) ;
#9618 = CARTESIAN_POINT ( 'NONE',  ( 3.459614771489464946, -11.09853614738469396, 4.563167253695070258 ) ) ;
#9619 = ORIENTED_EDGE ( 'NONE', *, *, #57917, .F. ) ;
#9620 = ORIENTED_EDGE ( 'NONE', *, *, #50827, .F. ) ;
#9621 = CYLINDRICAL_SURFACE ( 'NONE', #40548, 5.000000000000000888 ) ;
#9622 = VERTEX_POINT ( 'NONE', #17013 ) ;
#9623 = DIRECTION ( 'NONE',  ( 1.000000000000000000, 0.000000000000000000, 0.000000000000000000 ) ) ;
#9624 = ORIENTED_EDGE ( 'NONE', *, *, #37993, .F. ) ;
#9625 = ORIENTED_EDGE ( 'NONE', *, *, #3052, .T. ) ;
#9626 = VERTEX_POINT ( 'NONE', #11691 ) ;
#9627 = VECTOR ( 'NONE', #18800, 1000.000000000000114 ) ;
#9628 = FACE_OUTER_BOUND ( 'NONE', #18801, .T. ) ;
#9629 = CARTESIAN_POINT ( 'NONE',  ( 1.989990211274497156, -25.75944405492161593, 15.61385975544041038 ) ) ;
#9630 = DIRECTION ( 'NONE',  ( 0.000000000000000000, 0.04924826701374583615, 0.9987865678893277366 ) ) ;
#9631 = FACE_OUTER_BOUND ( 'NONE', #13253, .T. ) ;
#9632 = ORIENTED_EDGE ( 'NONE', *, *, #16595, .F. ) ;
#9633 = EDGE_CURVE ( 'NONE', #62352, #9772, #18525, .T. ) ;
#9634 = AXIS2_PLACEMENT_3D ( 'NONE', #7531, #54079, #23837 ) ;
#9635 = CARTESIAN_POINT ( 'NONE',  ( -37.00000000000000711, 8.029056188533687077, 8.573591947375351907 ) ) ;
#9636 = CIRCLE ( 'NONE', #31938, 5.000000000000000888 ) ;
#9637 = EDGE_LOOP ( 'NONE', ( #36231, #1011, #64663, #9943 ) ) ;
#9638 = DIRECTION ( 'NONE',  ( 0.000000000000000000, 0.000000000000000000, -1.000000000000000000 ) ) ;
#9639 = CARTESIAN_POINT ( 'NONE',  ( 3.152665057736003362, 6.378477742801834438, 4.725420687649379836 ) ) ;
#9640 = VECTOR ( 'NONE', #20546, 1000.000000000000000 ) ;
#9641 = ORIENTED_EDGE ( 'NONE', *, *, #55033, .T. ) ;
#9642 = CARTESIAN_POINT ( 'NONE',  ( 0.3002738374340808702, -10.72659044316167432, 5.932527270856367885 ) ) ;
#9643 = CARTESIAN_POINT ( 'NONE',  ( 0.2833330754217391889, 3.999965385632591186, 11.58086621621908385 ) ) ;
#9644 = AXIS2_PLACEMENT_3D ( 'NONE', #32216, #49181, #38521 ) ;
#9645 = CARTESIAN_POINT ( 'NONE',  ( 0.2648978790185602672, 11.55204314799263798, 4.063980959785085112 ) ) ;
#9646 = ORIENTED_EDGE ( 'NONE', *, *, #48806, .F. ) ;
#9647 = DIRECTION ( 'NONE',  ( 0.000000000000000000, 1.000000000000000000, 0.000000000000000000 ) ) ;
#9648 = CIRCLE ( 'NONE', #55320, 12.75000000000000178 ) ;
#9649 = EDGE_CURVE ( 'NONE', #47974, #4279, #19545, .T. ) ;
#9650 = ORIENTED_EDGE ( 'NONE', *, *, #39691, .T. ) ;
#9651 = CARTESIAN_POINT ( 'NONE',  ( -24.38812357031636679, -11.02047918387278180, 7.799809501265555056 ) ) ;
#9652 = DIRECTION ( 'NONE',  ( 1.000000000000000000, -0.000000000000000000, 0.000000000000000000 ) ) ;
#9653 = CARTESIAN_POINT ( 'NONE',  ( 2.889800649504073782, -5.267262008933648154, -3.118861721612621096 ) ) ;
#9655 = AXIS2_PLACEMENT_3D ( 'NONE', #3170, #64319, #63648 ) ;
#9654 = CYLINDRICAL_SURFACE ( 'NONE', #3312, 12.75000000000000178 ) ;
#9656 = CARTESIAN_POINT ( 'NONE',  ( 35.00000000000000000, 4.705694406421931860E-17, -3.469127814946512892E-15 ) ) ;
#9657 = EDGE_LOOP ( 'NONE', ( #17365, #12491, #45427, #13759 ) ) ;
#9658 = CARTESIAN_POINT ( 'NONE',  ( 36.00000000000000711, -6.415447294506781084, -11.01837265713071368 ) ) ;
#9659 = CARTESIAN_POINT ( 'NONE',  ( 0.6473888112830221697, 5.898884566269161134, -10.87693551365365074 ) ) ;
#9660 = CARTESIAN_POINT ( 'NONE',  ( 1.719304012341273280, -2.961219984259375160, -12.38166659046469675 ) ) ;
#9661 = DIRECTION ( 'NONE',  ( 0.000000000000000000, 0.1118654143051617117, 0.9937233664769761221 ) ) ;
#9662 = CIRCLE ( 'NONE', #10715, 5.000000000000001776 ) ;
#9663 = VECTOR ( 'NONE', #27024, 1000.000000000000000 ) ;
#9664 = EDGE_CURVE ( 'NONE', #33594, #42155, #41294, .T. ) ;
#9665 = AXIS2_PLACEMENT_3D ( 'NONE', #19845, #51100, #35763 ) ;
#9666 = CARTESIAN_POINT ( 'NONE',  ( 37.00000000000000711, 4.705694406421931860E-17, -3.469127814946512892E-15 ) ) ;
#9667 = AXIS2_PLACEMENT_3D ( 'NONE', #3209, #7869, #24131 ) ;
#9668 = CARTESIAN_POINT ( 'NONE',  ( 3.291290029914074378, 8.250315036047103590, -8.713914264323182834 ) ) ;
#9670 = ADVANCED_FACE ( 'NONE', ( #31338 ), #46128, .T. ) ;
#9669 = CARTESIAN_POINT ( 'NONE',  ( 37.00000000000000711, 9.348667969174517367, 7.817492529713752525 ) ) ;
#9671 = CARTESIAN_POINT ( 'NONE',  ( 5.530133899448235191, -0.009387834778845241188, -0.01293763278443419047 ) ) ;
#9672 = DIRECTION ( 'NONE',  ( 0.000000000000000000, 0.01356324068817998593, -0.9999080150203990547 ) ) ;
#9673 = EDGE_CURVE ( 'NONE', #22062, #55015, #56773, .T. ) ;
#9674 = EDGE_CURVE ( 'NONE', #37639, #20061, #15690, .T. ) ;
#9675 = CIRCLE ( 'NONE', #21368, 7.499999999999988454 ) ;
#9676 = EDGE_LOOP ( 'NONE', ( #24662, #64001, #30634, #61066 ) ) ;
#9677 = CARTESIAN_POINT ( 'NONE',  ( 11.95035458199039624, -11.72822567559551743, -2.544750170429570080 ) ) ;
#9678 = CIRCLE ( 'NONE', #31937, 4.999999999999999112 ) ;
#9679 = AXIS2_PLACEMENT_3D ( 'NONE', #43323, #13716, #38998 ) ;
#9680 =( BOUNDED_SURFACE ( )  B_SPLINE_SURFACE ( 3, 1, ( 
 ( #51645, #60616 ),
 ( #26348, #46635 ),
 ( #1089, #45646 ),
 ( #11069, #100 ) ),
 .UNSPECIFIED., .F., .F., .F. ) 
 B_SPLINE_SURFACE_WITH_KNOTS ( ( 4, 4 ),
 ( 2, 2 ),
 ( 0.000000000000000000, 1.000000000000000000 ),
 ( 0.000000000000000000, 1.000000000000000000 ),
 .UNSPECIFIED. ) 
 GEOMETRIC_REPRESENTATION_ITEM ( )  RATIONAL_B_SPLINE_SURFACE ( (
 ( 1.000000000000000000, 1.000000000000000000),
 ( 0.9932032654565553509, 0.8386279382598740284),
 ( 0.9932032654565553509, 0.8386279382598740284),
 ( 1.000000000000000000, 1.000000000000000000) ) ) 
 REPRESENTATION_ITEM ( '' )  SURFACE ( )  );
#9681 = VERTEX_POINT ( 'NONE', #61919 ) ;
#9682 = CARTESIAN_POINT ( 'NONE',  ( -37.00000000000000711, 12.70128625845194392, -1.113475361586356627 ) ) ;
#9683 = DIRECTION ( 'NONE',  ( -1.000000000000000000, 0.000000000000000000, 0.000000000000000000 ) ) ;
#9684 = CARTESIAN_POINT ( 'NONE',  ( -35.00000000000000000, 1.591260454995410578, -12.08216339958899077 ) ) ;
#9685 = CARTESIAN_POINT ( 'NONE',  ( 0.000000000000000000, 5.585096664091999230, -4.113602740025892324 ) ) ;
#9686 = ORIENTED_EDGE ( 'NONE', *, *, #46922, .T. ) ;
#9687 = CIRCLE ( 'NONE', #58574, 7.499999999999988454 ) ;
#9688 = ORIENTED_EDGE ( 'NONE', *, *, #34802, .F. ) ;
#9689 = VERTEX_POINT ( 'NONE', #32306 ) ;
#9690 = CARTESIAN_POINT ( 'NONE',  ( 29.18521670982013916, -10.00068734037119178, 6.636238164281968999 ) ) ;
#9691 = EDGE_CURVE ( 'NONE', #38228, #53897, #37192, .T. ) ;
#9692 = CARTESIAN_POINT ( 'NONE',  ( 3.092491956585758039, 3.565393530441273828, -7.070043156103592352 ) ) ;
#9693 = ORIENTED_EDGE ( 'NONE', *, *, #4193, .T. ) ;
#9694 = DIRECTION ( 'NONE',  ( 1.000000000000000000, 0.000000000000000000, 0.000000000000000000 ) ) ;
#9695 = CARTESIAN_POINT ( 'NONE',  ( 35.00000000000000000, 5.921969905510355403, -10.14408668126215929 ) ) ;
#9696 = VECTOR ( 'NONE', #31165, 1000.000000000000000 ) ;
#9697 = CARTESIAN_POINT ( 'NONE',  ( 2.000000000000001776, -1.225832621831887792, 6.827324998361543607 ) ) ;
#9698 = ORIENTED_EDGE ( 'NONE', *, *, #9218, .T. ) ;
#9699 = DIRECTION ( 'NONE',  ( 0.000000000000000000, -0.1387779952735679057, 0.9903235168508568442 ) ) ;
#9700 =( BOUNDED_SURFACE ( )  B_SPLINE_SURFACE ( 3, 1, ( 
 ( #12719, #3449 ),
 ( #3776, #53962 ),
 ( #8402, #48992 ),
 ( #43984, #64258 ) ),
 .UNSPECIFIED., .F., .F., .F. ) 
 B_SPLINE_SURFACE_WITH_KNOTS ( ( 4, 4 ),
 ( 2, 2 ),
 ( 0.000000000000000000, 1.000000000000000000 ),
 ( 0.000000000000000000, 1.000000000000000000 ),
 .UNSPECIFIED. ) 
 GEOMETRIC_REPRESENTATION_ITEM ( )  RATIONAL_B_SPLINE_SURFACE ( (
 ( 1.000000000000000000, 1.000000000000000000),
 ( 0.9856612449720755231, 0.9999558406602322425),
 ( 0.9856612449720755231, 0.9999558406602322425),
 ( 1.000000000000000000, 1.000000000000000000) ) ) 
 REPRESENTATION_ITEM ( '' )  SURFACE ( )  );
#9701 = CARTESIAN_POINT ( 'NONE',  ( -10.20982488791469223, -27.71818678970560867, -14.28592212877975420 ) ) ;
#9702 = DIRECTION ( 'NONE',  ( 0.000000000000000000, -0.4935949184179322380, 0.8696919319575150409 ) ) ;
#9704 = ORIENTED_EDGE ( 'NONE', *, *, #63157, .F. ) ;
#9703 = CARTESIAN_POINT ( 'NONE',  ( -27.08702828306202193, 1.639744581306266769, 1.612407531673525796 ) ) ;
#9705 = AXIS2_PLACEMENT_3D ( 'NONE', #33673, #44609, #64899 ) ;
#9706 = DIRECTION ( 'NONE',  ( -1.000000000000000000, 0.000000000000000000, 0.000000000000000000 ) ) ;
#9707 = ORIENTED_EDGE ( 'NONE', *, *, #5209, .F. ) ;
#9708 = CARTESIAN_POINT ( 'NONE',  ( 0.3341166715381334584, -6.352033667906535896, -10.49680960898233195 ) ) ;
#9709 = VERTEX_POINT ( 'NONE', #7357 ) ;
#9710 = CARTESIAN_POINT ( 'NONE',  ( -37.00000000000000711, 0.000000000000000000, 0.000000000000000000 ) ) ;
#9711 = LINE ( 'NONE', #14376, #46813 ) ;
#9712 = DIRECTION ( 'NONE',  ( 0.000000000000000000, -0.9289767198167949713, 0.3701381553399054614 ) ) ;
#9713 = CARTESIAN_POINT ( 'NONE',  ( 0.8320506296491635423, -6.546053790694106311, -10.57268643647781126 ) ) ;
#9714 = EDGE_CURVE ( 'NONE', #24950, #33918, #27641, .T. ) ;
#9715 = CARTESIAN_POINT ( 'NONE',  ( -26.75616027029648691, -10.79764998130141151, 5.236257343771399064 ) ) ;
#9716 = AXIS2_PLACEMENT_3D ( 'NONE', #46995, #1453, #27667 ) ;
#9718 = AXIS2_PLACEMENT_3D ( 'NONE', #38804, #59101, #13512 ) ;
#9717 = CARTESIAN_POINT ( 'NONE',  ( 0.2717059086739037066, -12.24704971877459592, 0.1760722388997425225 ) ) ;
#9719 = DIRECTION ( 'NONE',  ( 1.000000000000000000, -0.000000000000000000, 0.000000000000000000 ) ) ;
#9720 = DIRECTION ( 'NONE',  ( 1.000000000000000000, 0.000000000000000000, -0.000000000000000000 ) ) ;
#9721 = CARTESIAN_POINT ( 'NONE',  ( 37.00000000000000711, 4.705694406421931860E-17, -3.469127814946512892E-15 ) ) ;
#9723 = ORIENTED_EDGE ( 'NONE', *, *, #29247, .T. ) ;
#9722 = DIRECTION ( 'NONE',  ( -1.000000000000000000, 0.000000000000000000, 0.000000000000000000 ) ) ;
#9724 = ORIENTED_EDGE ( 'NONE', *, *, #16703, .T. ) ;
#9725 = CARTESIAN_POINT ( 'NONE',  ( 13.12628618392431079, -11.60359632220612092, -6.913481910311843670 ) ) ;
#9726 = ORIENTED_EDGE ( 'NONE', *, *, #10190, .T. ) ;
#9727 = ORIENTED_EDGE ( 'NONE', *, *, #41227, .F. ) ;
#9728 = LINE ( 'NONE', #46311, #35961 ) ;
#9729 = DIRECTION ( 'NONE',  ( 1.000000000000000000, -0.000000000000000000, 0.000000000000000000 ) ) ;
#9730 = CARTESIAN_POINT ( 'NONE',  ( 5.514970785353741078, 0.004588761610585026345, -0.001117786416802573094 ) ) ;
#9732 = AXIS2_PLACEMENT_3D ( 'NONE', #10861, #51114, #46130 ) ;
#9731 = DIRECTION ( 'NONE',  ( 1.000000000000000000, -0.000000000000000000, 0.000000000000000000 ) ) ;
#9733 = CIRCLE ( 'NONE', #2354, 12.18649999999999700 ) ;
#9734 = DIRECTION ( 'NONE',  ( 0.000000000000000000, 0.9467777615094560284, 0.3218879778916007850 ) ) ;
#9735 = DIRECTION ( 'NONE',  ( 0.000000000000000000, 0.01356324068817992001, -0.9999080150203990547 ) ) ;
#9736 = CIRCLE ( 'NONE', #57517, 12.74999999999999822 ) ;
#9737 = EDGE_CURVE ( 'NONE', #33077, #33641, #43261, .T. ) ;
#9738 = ORIENTED_EDGE ( 'NONE', *, *, #16641, .T. ) ;
#9739 = CARTESIAN_POINT ( 'NONE',  ( 2.781367136451533995, 0.3081277311322765944, 7.808329083463359410 ) ) ;
#9740 = AXIS2_PLACEMENT_3D ( 'NONE', #25021, #9706, #26005 ) ;
#9741 = FACE_OUTER_BOUND ( 'NONE', #24996, .T. ) ;
#9742 = EDGE_CURVE ( 'NONE', #4955, #47398, #3893, .T. ) ;
#9743 = CARTESIAN_POINT ( 'NONE',  ( 1.198791140417704515, 12.26651935498904678, 2.686891236232352487 ) ) ;
#9744 = ORIENTED_EDGE ( 'NONE', *, *, #20406, .T. ) ;
#9745 = CIRCLE ( 'NONE', #8719, 2.899999999999994582 ) ;
#9746 = B_SPLINE_CURVE_WITH_KNOTS ( 'NONE', 3,
 ( #7998, #63175, #17957, #48246, #44201, #63816, #48556, #33245, #12298, #37902, #28915, #22958, #23270, #27936, #43534, #43879, #64469, #58534, #18297 ),
 .UNSPECIFIED., .F., .F.,
 ( 4, 3, 3, 3, 3, 3, 4 ),
 ( 7.046480070129584215E-18, 2.825908398830993712E-05, 4.208813692483719885E-05, 5.591713746943548653E-05, 6.279584083231588073E-05, 9.105792820296273917E-05, 0.0001153131102488845510 ),
 .UNSPECIFIED. ) ;
#9747 = EDGE_CURVE ( 'NONE', #33435, #21760, #59235, .T. ) ;
#9748 = AXIS2_PLACEMENT_3D ( 'NONE', #32053, #1820, #6475 ) ;
#9749 = CARTESIAN_POINT ( 'NONE',  ( 35.31912638668784155, -2.544741887441788197, 22.78557353984778899 ) ) ;
#9750 = DIRECTION ( 'NONE',  ( 1.000000000000000000, 0.000000000000000000, 0.000000000000000000 ) ) ;
#9751 = CARTESIAN_POINT ( 'NONE',  ( -27.01437459610461644, 11.79277645698183363, -2.220455681983952267 ) ) ;
#9752 = ORIENTED_EDGE ( 'NONE', *, *, #37390, .F. ) ;
#9754 = ADVANCED_FACE ( 'NONE', ( #8688 ), #52264, .F. ) ;
#9753 = CARTESIAN_POINT ( 'NONE',  ( 2.249013661412230913, 6.673008335691913651, -3.714035584818151214 ) ) ;
#9755 = CARTESIAN_POINT ( 'NONE',  ( 35.00000000000000000, -11.98254675519226531, 2.220215194442026974 ) ) ;
#9756 = DIRECTION ( 'NONE',  ( 0.000000000000000000, 0.01356324068817992175, -0.9999080150203990547 ) ) ;
#9757 = CIRCLE ( 'NONE', #36295, 5.000000000000000888 ) ;
#9758 = CIRCLE ( 'NONE', #46946, 5.000000000000000000 ) ;
#9759 = EDGE_CURVE ( 'NONE', #44286, #19660, #42717, .T. ) ;
#9760 = DIRECTION ( 'NONE',  ( 1.000000000000000000, 0.000000000000000000, -0.000000000000000000 ) ) ;
#9761 = CARTESIAN_POINT ( 'NONE',  ( 2.889800649504073782, -6.121013568931507720, 0.06738247734048298521 ) ) ;
#9762 = ORIENTED_EDGE ( 'NONE', *, *, #47322, .T. ) ;
#9763 = CARTESIAN_POINT ( 'NONE',  ( 2.241352910868908754, 2.689314586382447914, -7.145045428366549878 ) ) ;
#9764 = CARTESIAN_POINT ( 'NONE',  ( 0.2648978790185584908, -12.08224454301450201, 1.996248716311589400 ) ) ;
#9766 = CARTESIAN_POINT ( 'NONE',  ( -22.28856623400852399, 3.573466130470489333, -1.018212315222179143 ) ) ;
#9765 = B_SPLINE_CURVE_WITH_KNOTS ( 'NONE', 3,
 ( #39181, #34191, #3655, #59471, #42865, #53181, #13897, #23919, #44178, #7630, #27913, #28240, #2983, #58858, #63788, #13274 ),
 .UNSPECIFIED., .F., .F.,
 ( 4, 3, 3, 3, 3, 4 ),
 ( 0.000000000000000000, 0.0002999043160757247639, 0.0005998071753050776903, 0.0008997092107374208420, 0.001204458948194734799, 0.001510329163474717629 ),
 .UNSPECIFIED. ) ;
#9767 = VERTEX_POINT ( 'NONE', #49590 ) ;
#9768 = CARTESIAN_POINT ( 'NONE',  ( 8.460390590667396182, 3.946828837481929586, 12.91309979171136213 ) ) ;
#9769 = CARTESIAN_POINT ( 'NONE',  ( -35.00000000000000000, 0.000000000000000000, 0.000000000000000000 ) ) ;
#9770 = VERTEX_POINT ( 'NONE', #55555 ) ;
#9771 = B_SPLINE_CURVE_WITH_KNOTS ( 'NONE', 3,
 ( #22303, #32598, #21991, #17342, #37620, #3046, #42245 ),
 .UNSPECIFIED., .F., .F.,
 ( 4, 3, 4 ),
 ( 0.000000000000000000, 0.001700533616330532566, 0.005002426799371325131 ),
 .UNSPECIFIED. ) ;
#9772 = VERTEX_POINT ( 'NONE', #24297 ) ;
#9773 = ORIENTED_EDGE ( 'NONE', *, *, #11391, .T. ) ;
#9774 = AXIS2_PLACEMENT_3D ( 'NONE', #13723, #39663, #19398 ) ;
#9775 = AXIS2_PLACEMENT_3D ( 'NONE', #20968, #60554, #39 ) ;
#9776 = VERTEX_POINT ( 'NONE', #9645 ) ;
#9777 = CARTESIAN_POINT ( 'NONE',  ( 35.00000000000000000, 4.705694406421931860E-17, -3.469127814946512892E-15 ) ) ;
#9778 = DIRECTION ( 'NONE',  ( 1.000000000000000000, 0.000000000000000000, 0.000000000000000000 ) ) ;
#9779 = CARTESIAN_POINT ( 'NONE',  ( -47.00000000000000711, 0.000000000000000000, 0.000000000000000000 ) ) ;
#9780 = CARTESIAN_POINT ( 'NONE',  ( 24.82652845881425208, -10.42385221765392700, -8.578654028722157321 ) ) ;
#9781 = CIRCLE ( 'NONE', #23575, 12.74999999999999822 ) ;
#9782 = CARTESIAN_POINT ( 'NONE',  ( -19.56743653832047158, -29.00000000000000000, 5.000000000000000888 ) ) ;
#9783 = CARTESIAN_POINT ( 'NONE',  ( 24.52118107989806006, -2.661457398423999532, -13.23640138053051984 ) ) ;
#9785 = VERTEX_POINT ( 'NONE', #40235 ) ;
#9784 = CARTESIAN_POINT ( 'NONE',  ( -35.00000000000000000, 5.246972444134173408, -10.99909370905151995 ) ) ;
#9786 = DIRECTION ( 'NONE',  ( 0.000000000000000000, -1.000000000000000000, 0.000000000000000000 ) ) ;
#9787 = ORIENTED_EDGE ( 'NONE', *, *, #11728, .T. ) ;
#9788 = CARTESIAN_POINT ( 'NONE',  ( 5.515188684475870851, 0.002355816063606930213, 0.004804816249378836106 ) ) ;
#9789 = VERTEX_POINT ( 'NONE', #59554 ) ;
#9790 = ORIENTED_EDGE ( 'NONE', *, *, #58602, .F. ) ;
#9791 = CARTESIAN_POINT ( 'NONE',  ( 0.3401186441510281044, 9.562489599411641450, -7.690203051555926095 ) ) ;
#9792 = CARTESIAN_POINT ( 'NONE',  ( 11.89229108778294730, -32.87417574757987637, 11.69979538107606665 ) ) ;
#9793 = DIRECTION ( 'NONE',  ( -1.000000000000000000, -0.000000000000000000, 0.000000000000000000 ) ) ;
#9794 = EDGE_CURVE ( 'NONE', #64905, #18784, #44251, .T. ) ;
#9795 = B_SPLINE_CURVE_WITH_KNOTS ( 'NONE', 3,
 ( #34720, #49717, #4505, #500, #65325, #40047, #14762, #35040, #157, #41035, #44700, #50389, #15440, #56005, #29422, #55019, #20106, #40716, #61318, #25758, #64992, #10441 ),
 .UNSPECIFIED., .F., .F.,
 ( 4, 3, 3, 3, 3, 3, 3, 4 ),
 ( 2.611104600503653083E-18, 4.455945684386675046E-05, 6.636307477204036738E-05, 8.816671873158864485E-05, 0.0001099660380492628885, 0.0001317545563165320791, 0.0001762613022895052613, 0.0001867992666138397820 ),
 .UNSPECIFIED. ) ;
#9796 = CARTESIAN_POINT ( 'NONE',  ( 2.373367633546872302, 7.591069096729010646, -1.154895193356554550 ) ) ;
#9797 = DIRECTION ( 'NONE',  ( -1.000000000000000000, -0.000000000000000000, -0.000000000000000000 ) ) ;
#9798 = DIRECTION ( 'NONE',  ( -0.000000000000000000, -0.000000000000000000, -1.000000000000000000 ) ) ;
#9799 = ORIENTED_EDGE ( 'NONE', *, *, #38434, .F. ) ;
#9800 = VECTOR ( 'NONE', #42106, 1000.000000000000000 ) ;
#9801 = ORIENTED_EDGE ( 'NONE', *, *, #13034, .T. ) ;
#9802 = CARTESIAN_POINT ( 'NONE',  ( -28.66013792860432119, 1.770123732198269240, 0.4872053345171892258 ) ) ;
#9803 = VERTEX_POINT ( 'NONE', #9013 ) ;
#9804 = ORIENTED_EDGE ( 'NONE', *, *, #25382, .T. ) ;
#9805 = CARTESIAN_POINT ( 'NONE',  ( 0.3665391374699465965, -3.952034409876375332, 11.62960183138725689 ) ) ;
#9806 = DIRECTION ( 'NONE',  ( 0.000000000000000000, 0.01356324068817998940, -0.9999080150203989437 ) ) ;
#9807 = DIRECTION ( 'NONE',  ( 0.000000000000000000, 0.000000000000000000, 1.000000000000000000 ) ) ;
#9808 = CARTESIAN_POINT ( 'NONE',  ( 2.258463476536646031, 7.638896687393374130, 0.1358786215988430079 ) ) ;
#9809 = CARTESIAN_POINT ( 'NONE',  ( -11.14133641294997901, -5.663661283019989057, -10.58164429124088457 ) ) ;
#9810 = AXIS2_PLACEMENT_3D ( 'NONE', #50162, #14237, #20549 ) ;
#9811 = EDGE_CURVE ( 'NONE', #34853, #47440, #467, .T. ) ;
#9812 = DIRECTION ( 'NONE',  ( 0.000000000000000000, -0.6478160128811839558, 0.7617968321374969376 ) ) ;
#9813 = ORIENTED_EDGE ( 'NONE', *, *, #27217, .T. ) ;
#9814 = EDGE_CURVE ( 'NONE', #23038, #19720, #29315, .T. ) ;
#9815 = EDGE_LOOP ( 'NONE', ( #43636, #46766, #36136, #7176 ) ) ;
#9816 = EDGE_CURVE ( 'NONE', #18660, #28337, #7875, .T. ) ;
#9817 = CARTESIAN_POINT ( 'NONE',  ( 0.3675815128205894289, 12.27743992903066150, 0.2638082659428850896 ) ) ;
#9818 = CARTESIAN_POINT ( 'NONE',  ( 2.273267844204863941, 7.501135923490796387, -1.476347988307392001 ) ) ;
#9819 = DIRECTION ( 'NONE',  ( 0.000000000000000000, -0.01356324068817999114, 0.9999080150203989437 ) ) ;
#9820 = AXIS2_PLACEMENT_3D ( 'NONE', #27596, #47260, #31923 ) ;
#9821 = LINE ( 'NONE', #30114, #46195 ) ;
#9822 = DIRECTION ( 'NONE',  ( 0.000000000000000000, -0.2960891610144577579, -0.9551603052523459647 ) ) ;
#9823 = EDGE_CURVE ( 'NONE', #31241, #2509, #59893, .T. ) ;
#9824 = AXIS2_PLACEMENT_3D ( 'NONE', #46931, #1392, #61232 ) ;
#9825 = CARTESIAN_POINT ( 'NONE',  ( 5.515539859299206427, 0.005924322247675109683, -0.001241880655086952893 ) ) ;
#9826 = ADVANCED_FACE ( 'NONE', ( #50890 ), #14958, .T. ) ;
#9827 = DIRECTION ( 'NONE',  ( 0.000000000000000000, 0.01356324068817991828, -0.9999080150203990547 ) ) ;
#9828 = AXIS2_PLACEMENT_3D ( 'NONE', #585, #56781, #22152 ) ;
#9829 = DIRECTION ( 'NONE',  ( -0.000000000000000000, -1.000000000000000000, -0.000000000000000000 ) ) ;
#9830 = ORIENTED_EDGE ( 'NONE', *, *, #27410, .F. ) ;
#9831 = DIRECTION ( 'NONE',  ( 0.000000000000000000, 0.01356324068817992175, -0.9999080150203990547 ) ) ;
#9832 = CARTESIAN_POINT ( 'NONE',  ( 37.00000000000000711, 6.584150480049550502, -10.25474254703955701 ) ) ;
#9833 = CARTESIAN_POINT ( 'NONE',  ( 1.937114397841935398, 12.80345148322679272, -0.9020203649532142487 ) ) ;
#9834 = EDGE_CURVE ( 'NONE', #57839, #23170, #54634, .T. ) ;
#9835 = EDGE_CURVE ( 'NONE', #19340, #55219, #14316, .T. ) ;
#9836 = CYLINDRICAL_SURFACE ( 'NONE', #25630, 5.000000000000000888 ) ;
#9837 = AXIS2_PLACEMENT_3D ( 'NONE', #21410, #46356, #21754 ) ;
#9838 = CARTESIAN_POINT ( 'NONE',  ( 1.452237505248552996, 12.34692280296791900, 2.778494755359096846 ) ) ;
#9839 = VERTEX_POINT ( 'NONE', #35584 ) ;
#9840 = B_SPLINE_CURVE_WITH_KNOTS ( 'NONE', 3,
 ( #60654, #1787, #36014, #6778, #37007, #21406, #51998, #12070, #57310, #22052, #32018, #62280, #16426, #51361, #21058, #56673 ),
 .UNSPECIFIED., .F., .F.,
 ( 4, 3, 3, 3, 3, 4 ),
 ( 0.000000000000000000, 0.0002999043160757397259, 0.0005998071753051095658, 0.0008997092107374688721, 0.001204458948196129951, 0.001510329163477477140 ),
 .UNSPECIFIED. ) ;
#9841 = CARTESIAN_POINT ( 'NONE',  ( 5.514970785353741078, 0.0005190732562555076942, -0.004694330894494710103 ) ) ;
#9842 = CARTESIAN_POINT ( 'NONE',  ( 2.305787727787084407, 6.545285700970527643, 3.971363876083986888 ) ) ;
#9844 = EDGE_CURVE ( 'NONE', #18330, #3618, #63100, .T. ) ;
#9843 = CARTESIAN_POINT ( 'NONE',  ( 10.20102756488484275, -26.83656875578374112, -13.80782716569073010 ) ) ;
#9845 = VERTEX_POINT ( 'NONE', #30277 ) ;
#9846 = CYLINDRICAL_SURFACE ( 'NONE', #31278, 12.18650000000000055 ) ;
#9847 = CARTESIAN_POINT ( 'NONE',  ( -28.24248022282097992, -12.24705570707973301, -5.688045095021857733 ) ) ;
#9848 = CARTESIAN_POINT ( 'NONE',  ( -22.30398854582848145, -1.062335901716038977, -3.608860109585141362 ) ) ;
#9849 = VECTOR ( 'NONE', #51001, 1000.000000000000000 ) ;
#9850 = AXIS2_PLACEMENT_3D ( 'NONE', #3620, #44149, #64413 ) ;
#9852 = ORIENTED_EDGE ( 'NONE', *, *, #64314, .F. ) ;
#9851 = FACE_OUTER_BOUND ( 'NONE', #931, .T. ) ;
#9853 = CARTESIAN_POINT ( 'NONE',  ( 2.655192694323172731, 8.807900729502561532, -3.822392723568370343 ) ) ;
#9854 = AXIS2_PLACEMENT_3D ( 'NONE', #33789, #13201, #47794 ) ;
#9855 = AXIS2_PLACEMENT_3D ( 'NONE', #715, #5046, #55592 ) ;
#9856 = CARTESIAN_POINT ( 'NONE',  ( 5.514970785353741078, -0.004694330894494374434, 0.0005190732562558384843 ) ) ;
#9857 = ORIENTED_EDGE ( 'NONE', *, *, #30315, .F. ) ;
#9858 = DIRECTION ( 'NONE',  ( -1.000000000000000000, -0.000000000000000000, 0.000000000000000000 ) ) ;
#9859 = CARTESIAN_POINT ( 'NONE',  ( -27.10719052120871098, 1.310802520592036391, 1.962717903527646079 ) ) ;
#9860 = FACE_OUTER_BOUND ( 'NONE', #3992, .T. ) ;
#9861 = CARTESIAN_POINT ( 'NONE',  ( 0.8375941296813791404, -1.780036797758159262, -12.30893872205299111 ) ) ;
#9862 = CARTESIAN_POINT ( 'NONE',  ( 2.000000000000001776, -6.812627895098285258, 2.855765430652660974 ) ) ;
#9863 = CIRCLE ( 'NONE', #29154, 12.74999999999999822 ) ;
#9864 = DIRECTION ( 'NONE',  ( 1.000000000000000000, 0.000000000000000000, 0.000000000000000000 ) ) ;
#9865 = DIRECTION ( 'NONE',  ( 0.000000000000000000, 0.01356324068817998940, -0.9999080150203990547 ) ) ;
#9866 = ORIENTED_EDGE ( 'NONE', *, *, #19391, .T. ) ;
#9867 = FACE_OUTER_BOUND ( 'NONE', #32684, .T. ) ;
#9868 = CIRCLE ( 'NONE', #18394, 12.74999999999999822 ) ;
#9869 = ORIENTED_EDGE ( 'NONE', *, *, #3568, .F. ) ;
#9870 = CARTESIAN_POINT ( 'NONE',  ( 1.000000000000000888, -2.473437528934186780, 7.080403010454960899 ) ) ;
#9871 = ADVANCED_FACE ( 'NONE', ( #50577 ), #4362, .T. ) ;
#9872 = EDGE_CURVE ( 'NONE', #38736, #38939, #36525, .T. ) ;
#9873 = PLANE ( 'NONE',  #54278 ) ;
#9874 = ORIENTED_EDGE ( 'NONE', *, *, #22706, .T. ) ;
#9875 = CYLINDRICAL_SURFACE ( 'NONE', #59505, 4.500000000000000888 ) ;
#9876 = CARTESIAN_POINT ( 'NONE',  ( 12.91052848813855469, 10.81303340823124692, -5.207629998415853834 ) ) ;
#9877 = CARTESIAN_POINT ( 'NONE',  ( -37.00000000000000711, -12.17626345777664021, 0.4993900848166987760 ) ) ;
#9878 = VERTEX_POINT ( 'NONE', #10310 ) ;
#9879 = VECTOR ( 'NONE', #30650, 1000.000000000000000 ) ;
#9880 = EDGE_LOOP ( 'NONE', ( #27692, #3938, #51083, #58335 ) ) ;
#9881 = DIRECTION ( 'NONE',  ( 0.000000000000000000, 0.000000000000000000, 1.000000000000000000 ) ) ;
#9882 = ADVANCED_FACE ( 'NONE', ( #16944 ), #11306, .T. ) ;
#9883 = ORIENTED_EDGE ( 'NONE', *, *, #36721, .F. ) ;
#9884 = CARTESIAN_POINT ( 'NONE',  ( 23.00432781815466754, -10.16387028742533793, -6.387888675388155413 ) ) ;
#9885 = CARTESIAN_POINT ( 'NONE',  ( -27.09342121492585065, 0.5565043948850146860, -2.251107617621284529 ) ) ;
#9886 = DIRECTION ( 'NONE',  ( 0.000000000000000000, 0.000000000000000000, 1.000000000000000000 ) ) ;
#9887 = CARTESIAN_POINT ( 'NONE',  ( 2.256373768223415954, 7.132139410181004280, -2.737361830682253139 ) ) ;
#9888 = LINE ( 'NONE', #25185, #49035 ) ;
#9889 = CARTESIAN_POINT ( 'NONE',  ( 0.2650492433740071485, -10.54996000109279386, 6.218175523534253735 ) ) ;
#9890 = VECTOR ( 'NONE', #25133, 1000.000000000000000 ) ;
#9891 = ADVANCED_FACE ( 'NONE', ( #51881 ), #32230, .T. ) ;
#9892 = B_SPLINE_CURVE_WITH_KNOTS ( 'NONE', 3,
 ( #52016, #62961, #41699, #37360, #2121, #57671, #11435, #7421, #22747, #6462, #42326, #43010, #31706, #62299, #61992, #37026 ),
 .UNSPECIFIED., .F., .F.,
 ( 4, 3, 3, 3, 3, 4 ),
 ( 5.963111948670274387E-19, 0.0003017745587525250302, 0.0006035491769808758004, 0.0009053241094668193923, 0.001207275924539141483, 0.001510325902531265080 ),
 .UNSPECIFIED. ) ;
#9893 = CARTESIAN_POINT ( 'NONE',  ( -28.67667724226168602, 0.1214114860980525235, 1.888227992976667213 ) ) ;
#9894 = ORIENTED_EDGE ( 'NONE', *, *, #44484, .F. ) ;
#9895 =( BOUNDED_CURVE ( )  B_SPLINE_CURVE ( 3, ( #6533, #6209, #26469, #47106 ),
 .UNSPECIFIED., .F., .F. ) 
 B_SPLINE_CURVE_WITH_KNOTS ( ( 4, 4 ),
 ( 1.289274629942205985, 1.297672015718555949 ),
 .UNSPECIFIED. ) 
 CURVE ( )  GEOMETRIC_REPRESENTATION_ITEM ( )  RATIONAL_B_SPLINE_CURVE ( ( 1.000000000000000000, 0.9999941236679763534, 0.9999941236679763534, 1.000000000000000000 ) ) 
 REPRESENTATION_ITEM ( '' )  );
#9896 = CARTESIAN_POINT ( 'NONE',  ( 1.020182472822803499, -11.88926988382020333, 3.852445298735596158 ) ) ;
#9897 = B_SPLINE_CURVE_WITH_KNOTS ( 'NONE', 3,
 ( #37489, #32483, #43443, #64381, #23514, #18849, #23178, #39113, #49129, #8215, #59405, #18202, #58439, #38469, #7902, #48147, #3588, #12867, #63396 ),
 .UNSPECIFIED., .F., .F.,
 ( 4, 3, 3, 3, 3, 3, 4 ),
 ( 6.759600587344756714E-18, 2.825908398830881564E-05, 4.208813692483547768E-05, 5.591713746943374503E-05, 6.279584083231433574E-05, 9.105792820296101800E-05, 0.0001153131102488855539 ),
 .UNSPECIFIED. ) ;
#9898 = CARTESIAN_POINT ( 'NONE',  ( 23.90871877840727322, 9.468420019444938163, -7.376992196490170350 ) ) ;
#9899 = EDGE_CURVE ( 'NONE', #22914, #48293, #61502, .T. ) ;
#9900 = LINE ( 'NONE', #55459, #63563 ) ;
#9902 = CARTESIAN_POINT ( 'NONE',  ( 35.00000000000000000, 12.16893194857555294, 3.805206332242343059 ) ) ;
#9901 = AXIS2_PLACEMENT_3D ( 'NONE', #24667, #65223, #19692 ) ;
#9903 = LINE ( 'NONE', #56442, #45654 ) ;
#9904 = LINE ( 'NONE', #55462, #64841 ) ;
#9905 = LINE ( 'NONE', #19236, #63154 ) ;
#9906 = VECTOR ( 'NONE', #52014, 1000.000000000000000 ) ;
#9907 = DIRECTION ( 'NONE',  ( -1.000000000000000000, 0.000000000000000000, 0.000000000000000000 ) ) ;
#9908 = VECTOR ( 'NONE', #41981, 1000.000000000000000 ) ;
#9909 = AXIS2_PLACEMENT_3D ( 'NONE', #32262, #46919, #22966 ) ;
#9910 = ORIENTED_EDGE ( 'NONE', *, *, #17573, .T. ) ;
#9911 = CARTESIAN_POINT ( 'NONE',  ( 0.2872850955227752023, 0.2089153415334872865, 12.25172867346922700 ) ) ;
#9912 = VERTEX_POINT ( 'NONE', #57196 ) ;
#9913 = CARTESIAN_POINT ( 'NONE',  ( 0.2655924914740778742, -12.05257978623655291, 2.169924872618023581 ) ) ;
#9914 = CARTESIAN_POINT ( 'NONE',  ( 35.00000000000000000, 11.66953048682399441, -3.511814412392164186 ) ) ;
#9915 = EDGE_CURVE ( 'NONE', #45003, #16245, #20619, .T. ) ;
#9916 = CARTESIAN_POINT ( 'NONE',  ( -18.06042000159870042, 5.592353769334478919, -12.28941745365187543 ) ) ;
#9917 = AXIS2_PLACEMENT_3D ( 'NONE', #3065, #53608, #3401 ) ;
#9918 = CARTESIAN_POINT ( 'NONE',  ( 0.000000000000000000, 0.000000000000000000, 0.000000000000000000 ) ) ;
#9919 = CARTESIAN_POINT ( 'NONE',  ( 2.256373768223204124, 2.487510024221536220, -7.223078030710271769 ) ) ;
#9920 = EDGE_CURVE ( 'NONE', #40631, #33417, #56819, .T. ) ;
#9921 = VERTEX_POINT ( 'NONE', #42190 ) ;
#9922 = AXIS2_PLACEMENT_3D ( 'NONE', #25627, #22617, #18629 ) ;
#9923 = DIRECTION ( 'NONE',  ( -1.000000000000000000, 0.000000000000000000, 0.000000000000000000 ) ) ;
#9924 = DIRECTION ( 'NONE',  ( 1.000000000000000000, 0.000000000000000000, 0.000000000000000000 ) ) ;
#9925 = DIRECTION ( 'NONE',  ( 1.000000000000000000, -0.000000000000000000, 0.000000000000000000 ) ) ;
#9926 = CARTESIAN_POINT ( 'NONE',  ( -22.27706089016750113, 2.583072118615372670, 2.622757446538661608 ) ) ;
#9927 = EDGE_CURVE ( 'NONE', #64920, #7749, #14236, .T. ) ;
#9928 = AXIS2_PLACEMENT_3D ( 'NONE', #2859, #43382, #63659 ) ;
#9929 = EDGE_CURVE ( 'NONE', #45204, #25848, #65284, .T. ) ;
#9930 = CARTESIAN_POINT ( 'NONE',  ( -17.34047990058653710, -6.189094570992181410, 10.28225073071224038 ) ) ;
#9931 = DIRECTION ( 'NONE',  ( 0.000000000000000000, 0.01356324068817998940, -0.9999080150203990547 ) ) ;
#9932 = AXIS2_PLACEMENT_3D ( 'NONE', #37344, #10764, #32660 ) ;
#9933 = ORIENTED_EDGE ( 'NONE', *, *, #56000, .T. ) ;
#9934 = CIRCLE ( 'NONE', #57701, 5.000000000000000888 ) ;
#9936 = ADVANCED_FACE ( 'NONE', ( #11621 ), #37211, .T. ) ;
#9935 = CARTESIAN_POINT ( 'NONE',  ( -27.08485414902845179, -0.5917839443963431867, 2.215517476308873412 ) ) ;
#9937 = EDGE_LOOP ( 'NONE', ( #10465, #53987, #49166, #53153 ) ) ;
#9938 = CARTESIAN_POINT ( 'NONE',  ( 0.3474126878361792348, -0.2587235634077174606, -12.27082419038178784 ) ) ;
#9939 = CARTESIAN_POINT ( 'NONE',  ( -35.00000000000000000, -4.732539170486343316, 11.23004253107762906 ) ) ;
#9940 = DIRECTION ( 'NONE',  ( 1.000000000000000000, 0.000000000000000000, 0.000000000000000000 ) ) ;
#9941 = CARTESIAN_POINT ( 'NONE',  ( -37.00000000000000711, 3.614449339633491576, 11.17622378668007777 ) ) ;
#9942 = AXIS2_PLACEMENT_3D ( 'NONE', #63842, #28286, #18324 ) ;
#9943 = ORIENTED_EDGE ( 'NONE', *, *, #5579, .T. ) ;
#9944 = ORIENTED_EDGE ( 'NONE', *, *, #59979, .T. ) ;
#9945 = CARTESIAN_POINT ( 'NONE',  ( 37.00000000000000711, -10.30098186818245409, 5.644643009979177783 ) ) ;
#9946 = ORIENTED_EDGE ( 'NONE', *, *, #62965, .T. ) ;
#9947 = DIRECTION ( 'NONE',  ( 0.000000000000000000, -0.01356324068817998940, 0.9999080150203990547 ) ) ;
#9948 = CARTESIAN_POINT ( 'NONE',  ( 5.515539859299206427, -0.004759416711441706582, 0.003740028639278266016 ) ) ;
#9949 = CARTESIAN_POINT ( 'NONE',  ( -27.10719052120871098, 2.295785794152562787, 0.5475695427849293084 ) ) ;
#9950 = DIRECTION ( 'NONE',  ( 0.000000000000000000, 0.9289767198167898643, 0.3701381553399182289 ) ) ;
#9951 = CYLINDRICAL_SURFACE ( 'NONE', #4622, 4.999999999999997335 ) ;
#9952 = CARTESIAN_POINT ( 'NONE',  ( -17.08907783926314394, 2.790822428529207144, 11.67174978956914266 ) ) ;
#9953 = CARTESIAN_POINT ( 'NONE',  ( 1.287602823386727158, -12.57487505104549541, -0.5522659225150269302 ) ) ;
#9954 = ORIENTED_EDGE ( 'NONE', *, *, #33149, .F. ) ;
#9955 = AXIS2_PLACEMENT_3D ( 'NONE', #17451, #43353, #47393 ) ;
#9956 = AXIS2_PLACEMENT_3D ( 'NONE', #51295, #38172, #58485 ) ;
#9957 = ORIENTED_EDGE ( 'NONE', *, *, #11098, .T. ) ;
#9958 = CARTESIAN_POINT ( 'NONE',  ( -22.66110217412718342, 4.573370147466346403, -1.880032915665380333 ) ) ;
#9959 = AXIS2_PLACEMENT_3D ( 'NONE', #49765, #16488, #855 ) ;
#9960 = CARTESIAN_POINT ( 'NONE',  ( -27.10719052120871098, 1.962717903527675611, -1.310802520592017295 ) ) ;
#9961 = ADVANCED_FACE ( 'NONE', ( #1004 ), #57527, .T. ) ;
#9962 = VERTEX_POINT ( 'NONE', #31892 ) ;
#9963 = B_SPLINE_CURVE_WITH_KNOTS ( 'NONE', 3,
 ( #31627, #31952, #26322, #41937, #57247, #16995, #61899, #32285, #51938, #16673 ),
 .UNSPECIFIED., .F., .F.,
 ( 4, 3, 3, 4 ),
 ( 1.939479807224432123E-18, 6.607638129004445515E-05, 9.911389841680619836E-05, 0.0001667630577588621486 ),
 .UNSPECIFIED. ) ;
#9964 = CARTESIAN_POINT ( 'NONE',  ( -35.00000000000000000, 2.544412758416015219, -11.91791701451263741 ) ) ;
#9965 = ADVANCED_FACE ( 'NONE', ( #59163 ), #47540, .T. ) ;
#9966 = EDGE_LOOP ( 'NONE', ( #41868, #1139, #20932, #33028 ) ) ;
#9967 = DIRECTION ( 'NONE',  ( 0.000000000000000000, -0.01356324068817992175, 0.9999080150203990547 ) ) ;
#9968 = CARTESIAN_POINT ( 'NONE',  ( -35.00000000000000000, 0.000000000000000000, 0.000000000000000000 ) ) ;
#9969 = CARTESIAN_POINT ( 'NONE',  ( 35.00000000000000000, -7.971186206369405447, 9.217970097227802029 ) ) ;
#9970 = CARTESIAN_POINT ( 'NONE',  ( 2.717984159219516194, 7.221467817271548739, -2.930214355830588868 ) ) ;
#9971 = EDGE_LOOP ( 'NONE', ( #19100, #13327, #49482, #62718 ) ) ;
#9972 = CIRCLE ( 'NONE', #55593, 2.899999999999996803 ) ;
#9973 = ORIENTED_EDGE ( 'NONE', *, *, #30239, .T. ) ;
#9974 = DIRECTION ( 'NONE',  ( -1.000000000000000000, 0.000000000000000000, -0.000000000000000000 ) ) ;
#9975 = ORIENTED_EDGE ( 'NONE', *, *, #65269, .T. ) ;
#9976 = CARTESIAN_POINT ( 'NONE',  ( 0.2956976708475478333, 11.59055635407407081, -3.984495122852460103 ) ) ;
#9977 = VERTEX_POINT ( 'NONE', #57862 ) ;
#9978 = AXIS2_PLACEMENT_3D ( 'NONE', #43785, #3892, #9492 ) ;
#9979 = EDGE_CURVE ( 'NONE', #41622, #13578, #36580, .T. ) ;
#9980 = ORIENTED_EDGE ( 'NONE', *, *, #28130, .F. ) ;
#9981 = VERTEX_POINT ( 'NONE', #7284 ) ;
#9982 = DIRECTION ( 'NONE',  ( -1.000000000000000000, 0.000000000000000000, 0.000000000000000000 ) ) ;
#9983 = AXIS2_PLACEMENT_3D ( 'NONE', #43310, #23050, #63584 ) ;
#9984 = CARTESIAN_POINT ( 'NONE',  ( 5.446351735594769927, -26.05211744559319342, 15.16580142939698383 ) ) ;
#9985 = CARTESIAN_POINT ( 'NONE',  ( 37.00000000000000711, 8.235637554476776145, 9.733281772932070197 ) ) ;
#9986 = CARTESIAN_POINT ( 'NONE',  ( 35.00000000000000000, -11.39945968423467448, 5.710938531231826154 ) ) ;
#9987 = DIRECTION ( 'NONE',  ( -1.000000000000000000, -0.000000000000000000, -0.000000000000000000 ) ) ;
#9988 = ORIENTED_EDGE ( 'NONE', *, *, #16472, .F. ) ;
#9989 = DIRECTION ( 'NONE',  ( 0.000000000000000000, 0.9289767198167898643, 0.3701381553399182289 ) ) ;
#9990 = ORIENTED_EDGE ( 'NONE', *, *, #32996, .F. ) ;
#9991 = DIRECTION ( 'NONE',  ( -1.000000000000000000, -0.000000000000000000, -0.000000000000000000 ) ) ;
#9992 = VECTOR ( 'NONE', #27815, 1000.000000000000000 ) ;
#9993 = CYLINDRICAL_SURFACE ( 'NONE', #23541, 12.18649999999999878 ) ;
#9994 = EDGE_CURVE ( 'NONE', #19210, #23964, #42968, .T. ) ;
#9995 = ORIENTED_EDGE ( 'NONE', *, *, #28608, .F. ) ;
#9996 = CARTESIAN_POINT ( 'NONE',  ( 5.536195898058073439, 0.008411485181669240210, 0.001224473329858010925 ) ) ;
#9997 = CARTESIAN_POINT ( 'NONE',  ( 0.2646305136544065406, -12.08286001766534312, -1.996350543473116801 ) ) ;
#9998 = DIRECTION ( 'NONE',  ( -1.000000000000000000, 0.000000000000000000, 0.000000000000000000 ) ) ;
#9999 = EDGE_CURVE ( 'NONE', #34871, #44514, #22253, .T. ) ;
#10000 = AXIS2_PLACEMENT_3D ( 'NONE', #42591, #57265, #31643 ) ;
#10001 = VERTEX_POINT ( 'NONE', #27567 ) ;
#10002 = EDGE_LOOP ( 'NONE', ( #20809, #42729, #2761, #12568 ) ) ;
#10003 = CARTESIAN_POINT ( 'NONE',  ( -24.46505758082295756, -9.480231875006323250, 9.613209244406563769 ) ) ;
#10004 = DIRECTION ( 'NONE',  ( -0.7648446667472313942, 0.000000000000000000, 0.6442147435043042991 ) ) ;
#10005 = CARTESIAN_POINT ( 'NONE',  ( -14.99915657824959325, -28.92607294587372380, 11.47448459775363538 ) ) ;
#10006 = CARTESIAN_POINT ( 'NONE',  ( 2.268878695252930733, -3.692782103667504146, -6.692359410363332373 ) ) ;
#10007 = LINE ( 'NONE', #20647, #28572 ) ;
#10008 = ORIENTED_EDGE ( 'NONE', *, *, #468, .F. ) ;
#10009 = CIRCLE ( 'NONE', #34394, 12.18649999999999878 ) ;
#10010 = DIRECTION ( 'NONE',  ( 0.000000000000000000, 0.2618041379715563277, -0.9651210252299812220 ) ) ;
#10011 = DIRECTION ( 'NONE',  ( 0.000000000000000000, 0.8835120444460208278, 0.4684084406997939265 ) ) ;
#10012 = CARTESIAN_POINT ( 'NONE',  ( 2.889800649504073782, 5.334644486274237707, -3.002151847318860867 ) ) ;
#10013 = CARTESIAN_POINT ( 'NONE',  ( 2.639814597422734277, 3.659458430304349807, 6.851176153958492776 ) ) ;
#10014 = EDGE_CURVE ( 'NONE', #42153, #18413, #2, .T. ) ;
#10015 = EDGE_CURVE ( 'NONE', #18779, #38082, #57844, .T. ) ;
#10016 = CARTESIAN_POINT ( 'NONE',  ( 0.3474126878361842308, -12.12932967384299232, -1.876013288000176971 ) ) ;
#10018 = EDGE_CURVE ( 'NONE', #62900, #58284, #17932, .T. ) ;
#10017 = CARTESIAN_POINT ( 'NONE',  ( -35.04709527796842394, -0.01231589140598780829, -0.001082316405380534530 ) ) ;
#10019 = CARTESIAN_POINT ( 'NONE',  ( -22.27834755396594346, 1.162947663292851930, -3.497967921180566986 ) ) ;
#10020 = CARTESIAN_POINT ( 'NONE',  ( 2.655192694323997848, -1.093661162899882022, 9.539062147542148651 ) ) ;
#10021 = DIRECTION ( 'NONE',  ( 0.3865475372811021382, -0.01937500237529702143, 0.9220659470476458841 ) ) ;
#10022 = CIRCLE ( 'NONE', #15333, 5.000000000000000888 ) ;
#10023 = VECTOR ( 'NONE', #58821, 1000.000000000000227 ) ;
#10024 = ADVANCED_FACE ( 'NONE', ( #17280 ), #28239, .T. ) ;
#10025 = ORIENTED_EDGE ( 'NONE', *, *, #9426, .F. ) ;
#10026 = CARTESIAN_POINT ( 'NONE',  ( -27.09364415740217424, -1.303410551736214229, -1.918701019215953929 ) ) ;
#10027 = ORIENTED_EDGE ( 'NONE', *, *, #38765, .F. ) ;
#10028 = CARTESIAN_POINT ( 'NONE',  ( -14.29135464769095520, 7.782112657557433089, -9.134479874907182051 ) ) ;
#10029 = CARTESIAN_POINT ( 'NONE',  ( -22.27384469013076185, 2.985904959940915759, -2.154627400808017956 ) ) ;
#10030 = LINE ( 'NONE', #30312, #47053 ) ;
#10031 = AXIS2_PLACEMENT_3D ( 'NONE', #16342, #26970, #5724 ) ;
#10032 = CARTESIAN_POINT ( 'NONE',  ( 0.000000000000000000, 5.457833520448724940, -4.281014542496488495 ) ) ;
#10033 = VERTEX_POINT ( 'NONE', #38193 ) ;
#10034 = ORIENTED_EDGE ( 'NONE', *, *, #51532, .F. ) ;
#10035 = VERTEX_POINT ( 'NONE', #48855 ) ;
#10036 = CARTESIAN_POINT ( 'NONE',  ( 2.639814597422740494, 2.896050884406630388, -7.207158938903913459 ) ) ;
#10037 = AXIS2_PLACEMENT_3D ( 'NONE', #30191, #44483, #44823 ) ;
#10038 = CARTESIAN_POINT ( 'NONE',  ( -22.27719443589224113, 0.7635131876695160358, 3.601617131804383476 ) ) ;
#10039 = ORIENTED_EDGE ( 'NONE', *, *, #35088, .F. ) ;
#10040 = CARTESIAN_POINT ( 'NONE',  ( 0.000000000000000000, 0.000000000000000000, 0.000000000000000000 ) ) ;
#10041 = DIRECTION ( 'NONE',  ( 0.000000000000000000, -0.3218879778915842427, 0.9467777615094616905 ) ) ;
#10042 = DIRECTION ( 'NONE',  ( -1.000000000000000000, -0.000000000000000000, 0.000000000000000000 ) ) ;
#10043 = EDGE_CURVE ( 'NONE', #20774, #29997, #59986, .T. ) ;
#10044 = VERTEX_POINT ( 'NONE', #27249 ) ;
#10045 = CARTESIAN_POINT ( 'NONE',  ( 2.263328370262056133, 4.802372801874240871, -5.944174889971576725 ) ) ;
#10046 = CARTESIAN_POINT ( 'NONE',  ( 3.643024398545976261, -28.29981509102550419, -13.54931501599924815 ) ) ;
#10047 = DIRECTION ( 'NONE',  ( 0.000000000000000000, 0.01356324068817998940, -0.9999080150203990547 ) ) ;
#10049 = ORIENTED_EDGE ( 'NONE', *, *, #43881, .F. ) ;
#10048 = CARTESIAN_POINT ( 'NONE',  ( -27.08429572838383947, 1.608131779585724619, 1.632445743623414325 ) ) ;
#10050 = DIRECTION ( 'NONE',  ( -1.000000000000000000, -0.000000000000000000, -0.000000000000000000 ) ) ;
#10051 = ORIENTED_EDGE ( 'NONE', *, *, #58894, .T. ) ;
#10052 = AXIS2_PLACEMENT_3D ( 'NONE', #39055, #29409, #59682 ) ;
#10053 = VERTEX_POINT ( 'NONE', #13273 ) ;
#10054 = CARTESIAN_POINT ( 'NONE',  ( -25.54417658651491863, 4.240019242199842608, 11.22596262356930197 ) ) ;
#10055 = DIRECTION ( 'NONE',  ( 0.000000000000000000, -0.01356324068817999114, 0.9999080150203989437 ) ) ;
#10056 = CARTESIAN_POINT ( 'NONE',  ( -35.00000000000000000, 9.040300684349693583, 7.499679039484089316 ) ) ;
#10057 = CARTESIAN_POINT ( 'NONE',  ( 35.00000000000000000, -4.237620530777882699, -11.42599468261427909 ) ) ;
#10058 = CARTESIAN_POINT ( 'NONE',  ( -26.26840407548881018, 3.532089703364137634, 0.2990196765638852838 ) ) ;
#10059 = CARTESIAN_POINT ( 'NONE',  ( 0.2915757698887292970, -12.25305747416128099, 0.2147157799034387915 ) ) ;
#10060 = DIRECTION ( 'NONE',  ( 0.000000000000000000, 0.01356324068817991481, -0.9999080150203990547 ) ) ;
#10061 = CARTESIAN_POINT ( 'NONE',  ( -27.08506889328344158, -0.2104793012480451475, -2.284141197253904298 ) ) ;
#10062 = CARTESIAN_POINT ( 'NONE',  ( 19.28625800530496903, 25.00000000000000000, 11.87904264843580471 ) ) ;
#10064 = VERTEX_POINT ( 'NONE', #33554 ) ;
#10063 = DIRECTION ( 'NONE',  ( -1.000000000000000000, 0.000000000000000000, 0.000000000000000000 ) ) ;
#10065 = CARTESIAN_POINT ( 'NONE',  ( -37.00000000000000711, -2.527899948230555971, -12.49688848680887077 ) ) ;
#10066 = CIRCLE ( 'NONE', #56838, 12.75000000000000178 ) ;
#10067 = EDGE_LOOP ( 'NONE', ( #61829, #56095, #43312, #8765 ) ) ;
#10068 = DIRECTION ( 'NONE',  ( 1.000000000000000000, 0.000000000000000000, -0.000000000000000000 ) ) ;
#10069 = VERTEX_POINT ( 'NONE', #53844 ) ;
#10070 = EDGE_CURVE ( 'NONE', #31308, #173, #43853, .T. ) ;
#10071 = CIRCLE ( 'NONE', #38737, 5.000000000000001776 ) ;
#10072 = EDGE_LOOP ( 'NONE', ( #21246, #360, #3436, #583 ) ) ;
#10073 = FACE_OUTER_BOUND ( 'NONE', #36918, .T. ) ;
#10074 = DIRECTION ( 'NONE',  ( 0.000000000000000000, -0.8009703041134232926, -0.5987040770935588840 ) ) ;
#10075 = CARTESIAN_POINT ( 'NONE',  ( -27.09030469827880339, -2.221523195520537008, 0.6314616953885225925 ) ) ;
#10076 = FACE_OUTER_BOUND ( 'NONE', #51856, .T. ) ;
#10077 = EDGE_CURVE ( 'NONE', #42334, #34961, #32331, .T. ) ;
#10078 = CIRCLE ( 'NONE', #18600, 4.999999999999999112 ) ;
#10079 = DIRECTION ( 'NONE',  ( 1.000000000000000000, 0.000000000000000000, 0.000000000000000000 ) ) ;
#10080 = DIRECTION ( 'NONE',  ( 1.000000000000000000, 0.000000000000000000, 0.000000000000000000 ) ) ;
#10081 = VERTEX_POINT ( 'NONE', #14545 ) ;
#10082 = CARTESIAN_POINT ( 'NONE',  ( 37.25000000000000711, -1.694065894508600678E-18, 0.000000000000000000 ) ) ;
#10083 = CARTESIAN_POINT ( 'NONE',  ( 35.00000000000000000, 12.18359334611896116, 0.2661492558803733588 ) ) ;
#10084 = CARTESIAN_POINT ( 'NONE',  ( 1.462291587748590027, 12.32753368892810286, 2.816455204775825560 ) ) ;
#10085 = ORIENTED_EDGE ( 'NONE', *, *, #3840, .T. ) ;
#10086 = EDGE_CURVE ( 'NONE', #47572, #18051, #34190, .T. ) ;
#10087 = AXIS2_PLACEMENT_3D ( 'NONE', #56277, #50343, #50659 ) ;
#10088 =( BOUNDED_CURVE ( )  B_SPLINE_CURVE ( 3, ( #56801, #11862, #31807, #913 ),
 .UNSPECIFIED., .F., .F. ) 
 B_SPLINE_CURVE_WITH_KNOTS ( ( 4, 4 ),
 ( 5.040318585505245252, 5.044875135688600132 ),
 .UNSPECIFIED. ) 
 CURVE ( )  GEOMETRIC_REPRESENTATION_ITEM ( )  RATIONAL_B_SPLINE_CURVE ( ( 1.000000000000000000, 0.9999982698216172139, 0.9999982698216172139, 1.000000000000000000 ) ) 
 REPRESENTATION_ITEM ( '' )  );
#10089 = CARTESIAN_POINT ( 'NONE',  ( 44.86048679285936913, -0.9948977233718069302, 15.27141897285095951 ) ) ;
#10090 = CARTESIAN_POINT ( 'NONE',  ( -22.66110217412718697, 2.319520136975695479, 4.366928509133826353 ) ) ;
#10091 = CARTESIAN_POINT ( 'NONE',  ( -49.19530910174992044, -0.1631003452855646629, -6.502801691937063033 ) ) ;
#10092 = VERTEX_POINT ( 'NONE', #9239 ) ;
#10093 = CARTESIAN_POINT ( 'NONE',  ( 36.00000000000000711, 9.621072037176993774, -8.366449238204399563 ) ) ;
#10094 = AXIS2_PLACEMENT_3D ( 'NONE', #25011, #30321, #14360 ) ;
#10095 = CARTESIAN_POINT ( 'NONE',  ( 11.20282697759287771, -32.63606470323558284, 12.17568710598608028 ) ) ;
#10096 = CARTESIAN_POINT ( 'NONE',  ( 29.51976981715666781, 25.00000000000000000, 11.09513982864076276 ) ) ;
#10097 = B_SPLINE_CURVE_WITH_KNOTS ( 'NONE', 3,
 ( #33279, #42925, #8337, #7337, #58572, #48588, #27621, #63850 ),
 .UNSPECIFIED., .F., .F.,
 ( 4, 2, 2, 4 ),
 ( 8.673617379884035472E-19, 0.002302291593524604611, 0.003453437390286906265, 0.004604583187049208354 ),
 .UNSPECIFIED. ) ;
#10098 = EDGE_CURVE ( 'NONE', #58893, #12098, #58919, .T. ) ;
#10099 = CARTESIAN_POINT ( 'NONE',  ( -35.00000000000000000, -9.063649021439015740, 8.146229107149364879 ) ) ;
#10100 = CARTESIAN_POINT ( 'NONE',  ( -37.00000000000000711, 0.000000000000000000, 0.000000000000000000 ) ) ;
#10101 = VERTEX_POINT ( 'NONE', #3654 ) ;
#10102 = LINE ( 'NONE', #55322, #56738 ) ;
#10103 = CARTESIAN_POINT ( 'NONE',  ( -22.27722015946439171, 3.455127654605130161, 1.271715168852039168 ) ) ;
#10104 = CARTESIAN_POINT ( 'NONE',  ( -35.00000000000000000, -11.96656215839365700, -4.400442035671072283 ) ) ;
#10105 = ORIENTED_EDGE ( 'NONE', *, *, #9999, .F. ) ;
#10106 = DIRECTION ( 'NONE',  ( -1.000000000000000000, -0.000000000000000000, -0.000000000000000000 ) ) ;
#10107 = DIRECTION ( 'NONE',  ( -1.000000000000000000, 0.000000000000000000, -0.000000000000000000 ) ) ;
#10108 = ORIENTED_EDGE ( 'NONE', *, *, #61134, .F. ) ;
#10109 = ORIENTED_EDGE ( 'NONE', *, *, #21555, .F. ) ;
#10110 = VERTEX_POINT ( 'NONE', #55128 ) ;
#10111 = AXIS2_PLACEMENT_3D ( 'NONE', #20018, #58, #25018 ) ;
#10112 = B_SPLINE_CURVE_WITH_KNOTS ( 'NONE', 3,
 ( #5531, #25797, #30756, #51072, #31433, #46088, #538, #36068, #14798, #61349, #20803, #41070, #15789 ),
 .UNSPECIFIED., .F., .F.,
 ( 4, 3, 3, 3, 4 ),
 ( 3.127317220692750759E-18, 6.607593386745688247E-05, 0.0001321518677373565267, 0.0001982171734706204261, 0.0002642860854759485545 ),
 .UNSPECIFIED. ) ;
#10113 = VERTEX_POINT ( 'NONE', #18914 ) ;
#10114 = CYLINDRICAL_SURFACE ( 'NONE', #65250, 12.18649999999999878 ) ;
#10115 = FACE_OUTER_BOUND ( 'NONE', #61842, .T. ) ;
#10116 = CARTESIAN_POINT ( 'NONE',  ( -39.82770826892757299, -25.90431001312668968, 4.499999999999997335 ) ) ;
#10117 = FACE_OUTER_BOUND ( 'NONE', #27229, .T. ) ;
#10118 = EDGE_CURVE ( 'NONE', #44987, #1336, #40483, .T. ) ;
#10119 = CARTESIAN_POINT ( 'NONE',  ( 2.406456491625455829, 8.704497555694503674, -5.751891873092491281 ) ) ;
#10120 = CARTESIAN_POINT ( 'NONE',  ( -8.775649586809111113, -28.78513225414202026, 9.890132258253697017 ) ) ;
#10121 = CARTESIAN_POINT ( 'NONE',  ( 23.97054589082751974, -3.699621146969923391, -12.98704298055938011 ) ) ;
#10123 = ORIENTED_EDGE ( 'NONE', *, *, #5635, .T. ) ;
#10122 = CARTESIAN_POINT ( 'NONE',  ( 0.2651627923886318849, -12.04449855907066791, -2.213220384814395647 ) ) ;
#10124 = ADVANCED_FACE ( 'NONE', ( #39179 ), #4933, .T. ) ;
#10125 = DIRECTION ( 'NONE',  ( 0.000000000000000000, -0.9289767198167949713, 0.3701381553399054614 ) ) ;
#10126 = VERTEX_POINT ( 'NONE', #55463 ) ;
#10127 = CARTESIAN_POINT ( 'NONE',  ( 37.00000000000000711, 3.704519465651471499, 11.60979404548630178 ) ) ;
#10128 = VERTEX_POINT ( 'NONE', #29847 ) ;
#10129 = ORIENTED_EDGE ( 'NONE', *, *, #51586, .T. ) ;
#10130 = CARTESIAN_POINT ( 'NONE',  ( 0.2869720083484446627, 9.519277517057210147, -7.715523637151659564 ) ) ;
#10131 = CARTESIAN_POINT ( 'NONE',  ( 18.66975156949834513, -29.88417193384195159, 7.188590896528484819 ) ) ;
#10132 = CARTESIAN_POINT ( 'NONE',  ( -35.04643116707788408, 0.007621814750502498015, 0.009511118309123156589 ) ) ;
#10133 = CIRCLE ( 'NONE', #45162, 12.74999999999999822 ) ;
#10134 = ADVANCED_FACE ( 'NONE', ( #19887 ), #50161, .T. ) ;
#10135 = LINE ( 'NONE', #20109, #4742 ) ;
#10136 = DIRECTION ( 'NONE',  ( -1.000000000000000000, -0.000000000000000000, 0.000000000000000000 ) ) ;
#10137 = CARTESIAN_POINT ( 'NONE',  ( 0.3665391374699464300, -11.62960183138730130, 3.952034409876256316 ) ) ;
#10138 = VERTEX_POINT ( 'NONE', #24884 ) ;
#10139 = EDGE_LOOP ( 'NONE', ( #49889, #45438, #616, #63226 ) ) ;
#10140 = CYLINDRICAL_SURFACE ( 'NONE', #31621, 12.74999999999999822 ) ;
#10141 = ORIENTED_EDGE ( 'NONE', *, *, #10014, .F. ) ;
#10142 = EDGE_CURVE ( 'NONE', #42915, #57650, #8999, .T. ) ;
#10143 = ORIENTED_EDGE ( 'NONE', *, *, #42753, .T. ) ;
#10144 = CARTESIAN_POINT ( 'NONE',  ( 1.452237505248555660, -3.767214359061207052, 12.08199618361511796 ) ) ;
#10145 = CARTESIAN_POINT ( 'NONE',  ( 0.2648978790185602672, 10.53870023327872474, -6.237101853238436355 ) ) ;
#10146 = CARTESIAN_POINT ( 'NONE',  ( -22.27706485742869091, 0.9832726768967819941, -3.547445275915930285 ) ) ;
#10147 = CARTESIAN_POINT ( 'NONE',  ( 18.78223320782606010, 0.2848378300378480721, 11.99965915797046989 ) ) ;
#10148 = CARTESIAN_POINT ( 'NONE',  ( 2.247206125382827935, 7.635476611656033974, 0.1157489416151797346 ) ) ;
#10149 = CARTESIAN_POINT ( 'NONE',  ( -35.00000000000000000, 10.02106554660708859, 7.882940143791811849 ) ) ;
#10150 = CARTESIAN_POINT ( 'NONE',  ( 3.152665057735448251, 0.9030954876725900693, -7.886634106564547331 ) ) ;
#10151 = ORIENTED_EDGE ( 'NONE', *, *, #63115, .F. ) ;
#10152 = ORIENTED_EDGE ( 'NONE', *, *, #7972, .F. ) ;
#10153 = CARTESIAN_POINT ( 'NONE',  ( 1.000000000000000888, -7.203928197742085260, -2.086484728383230181 ) ) ;
#10154 = CARTESIAN_POINT ( 'NONE',  ( 2.276905613633648962, 7.501802783089493332, -1.479235344773081939 ) ) ;
#10155 = DIRECTION ( 'NONE',  ( -1.000000000000000000, 0.000000000000000000, 0.000000000000000000 ) ) ;
#10156 = AXIS2_PLACEMENT_3D ( 'NONE', #60032, #60339, #39401 ) ;
#10157 = CARTESIAN_POINT ( 'NONE',  ( 3.533297333898360204, -10.56865501033795773, 5.684349346051587482 ) ) ;
#10158 = CARTESIAN_POINT ( 'NONE',  ( -22.35190811654611664, 2.161847148103716698, 3.252894036332493855 ) ) ;
#10159 = CARTESIAN_POINT ( 'NONE',  ( 23.56133193085831934, -3.409936927882566859, -13.06535930819385882 ) ) ;
#10160 = CARTESIAN_POINT ( 'NONE',  ( 3.915429104661797055, 7.704244136310878233, -9.244377499037618406 ) ) ;
#10161 = CARTESIAN_POINT ( 'NONE',  ( 2.368238019615093393, 5.994627685102951631, 4.795442552787996249 ) ) ;
#10162 = ORIENTED_EDGE ( 'NONE', *, *, #47460, .F. ) ;
#10163 = CARTESIAN_POINT ( 'NONE',  ( 2.305787727787084407, -0.1666591538753222634, 7.654065630109506024 ) ) ;
#10164 = CARTESIAN_POINT ( 'NONE',  ( -29.43980975494970309, -3.641506875706030488, -11.43413432115371364 ) ) ;
#10165 = CARTESIAN_POINT ( 'NONE',  ( 15.96337567072113650, -34.98223374851989576, 4.998641903492888616 ) ) ;
#10166 = EDGE_CURVE ( 'NONE', #12385, #37272, #21729, .T. ) ;
#10167 = AXIS2_PLACEMENT_3D ( 'NONE', #57121, #11547, #52131 ) ;
#10168 = FACE_OUTER_BOUND ( 'NONE', #21414, .T. ) ;
#10169 = FACE_OUTER_BOUND ( 'NONE', #27780, .T. ) ;
#10170 = ORIENTED_EDGE ( 'NONE', *, *, #7307, .F. ) ;
#10171 = CARTESIAN_POINT ( 'NONE',  ( -17.79128287606087255, -5.234468747551053625, -12.44476184210350844 ) ) ;
#10172 = CARTESIAN_POINT ( 'NONE',  ( 0.3040950598368152291, -12.02925914197706447, 2.376091969481177291 ) ) ;
#10173 = CARTESIAN_POINT ( 'NONE',  ( 15.45515798858408907, -34.86679772354910511, -6.222782430144768284 ) ) ;
#10174 = ORIENTED_EDGE ( 'NONE', *, *, #9007, .F. ) ;
#10175 = CARTESIAN_POINT ( 'NONE',  ( 1.634816307075121378, -6.964001572435194021, 10.62369813896840043 ) ) ;
#10176 = CARTESIAN_POINT ( 'NONE',  ( -22.71097035706203116, 4.965150228107710006, 0.4203397252017151420 ) ) ;
#10177 = CARTESIAN_POINT ( 'NONE',  ( -22.28546858134833286, -1.005093225210831553, -3.567529619157811638 ) ) ;
#10179 = ORIENTED_EDGE ( 'NONE', *, *, #39239, .F. ) ;
#10178 = DIRECTION ( 'NONE',  ( 1.000000000000000000, 0.000000000000000000, -0.000000000000000000 ) ) ;
#10180 = DIRECTION ( 'NONE',  ( 0.000000000000000000, 0.000000000000000000, -1.000000000000000000 ) ) ;
#10181 = EDGE_CURVE ( 'NONE', #42983, #30009, #60442, .T. ) ;
#10182 = AXIS2_PLACEMENT_3D ( 'NONE', #14381, #30985, #44623 ) ;
#10183 = CARTESIAN_POINT ( 'NONE',  ( 0.2655924914740778187, 9.409507842006130218, -7.838010948424953384 ) ) ;
#10184 = ORIENTED_EDGE ( 'NONE', *, *, #30193, .F. ) ;
#10185 = CARTESIAN_POINT ( 'NONE',  ( 0.2706063244538031154, 7.737788863017306618, 9.494160524941712254 ) ) ;
#10186 = FACE_BOUND ( 'NONE', #26852, .T. ) ;
#10188 = VECTOR ( 'NONE', #28334, 1000.000000000000000 ) ;
#10187 = CARTESIAN_POINT ( 'NONE',  ( 22.85866972464958025, -4.209424148273988919, -11.23992617506626601 ) ) ;
#10189 = CARTESIAN_POINT ( 'NONE',  ( 8.534769016306631428, 5.427010460188671281, -12.36273961895021323 ) ) ;
#10190 = EDGE_CURVE ( 'NONE', #14144, #53550, #9905, .T. ) ;
#10191 = DIRECTION ( 'NONE',  ( 1.000000000000000000, -0.000000000000000000, 0.000000000000000000 ) ) ;
#10192 = CARTESIAN_POINT ( 'NONE',  ( 0.3223008802179261889, 11.43958962819738900, -4.423848692584580355 ) ) ;
#10193 = ADVANCED_FACE ( 'NONE', ( #45469 ), #28886, .T. ) ;
#10194 = VERTEX_POINT ( 'NONE', #8935 ) ;
#10195 = FACE_OUTER_BOUND ( 'NONE', #63488, .T. ) ;
#10196 = ORIENTED_EDGE ( 'NONE', *, *, #50810, .F. ) ;
#10197 = CARTESIAN_POINT ( 'NONE',  ( -35.00000000000000000, -12.73293890771483028, -0.6593684648221820321 ) ) ;
#10198 = AXIS2_PLACEMENT_3D ( 'NONE', #63605, #4432, #8759 ) ;
#10199 = CARTESIAN_POINT ( 'NONE',  ( 0.2657645697724688727, 11.45515365350261838, 4.330388001246444851 ) ) ;
#10200 = EDGE_CURVE ( 'NONE', #56470, #24059, #38714, .T. ) ;
#10201 = FACE_OUTER_BOUND ( 'NONE', #18358, .T. ) ;
#10202 = VERTEX_POINT ( 'NONE', #49195 ) ;
#10203 = CARTESIAN_POINT ( 'NONE',  ( 35.00000000000000000, -1.771820996347075017, 11.61175578952787113 ) ) ;
#10204 = CARTESIAN_POINT ( 'NONE',  ( 12.83856522484696860, 11.13998188696922398, -4.465410698652262589 ) ) ;
#10206 = ADVANCED_FACE ( 'NONE', ( #50492 ), #65737, .T. ) ;
#10205 = DIRECTION ( 'NONE',  ( -1.000000000000000000, 0.000000000000000000, 0.000000000000000000 ) ) ;
#10207 = EDGE_LOOP ( 'NONE', ( #44859, #34245, #33535, #34305 ) ) ;
#10208 = VERTEX_POINT ( 'NONE', #24216 ) ;
#10209 = LINE ( 'NONE', #14845, #13028 ) ;
#10210 = ORIENTED_EDGE ( 'NONE', *, *, #25769, .F. ) ;
#10211 = CARTESIAN_POINT ( 'NONE',  ( 0.3040950598368152291, 2.376091969481216370, 12.02925914197705559 ) ) ;
#10212 = CARTESIAN_POINT ( 'NONE',  ( -35.00000000000000000, -0.6593684648221378453, 12.73293890771483028 ) ) ;
#10213 = CARTESIAN_POINT ( 'NONE',  ( 5.514970785353741078, 0.0005190732562555056342, -0.004694330894494712705 ) ) ;
#10214 = CARTESIAN_POINT ( 'NONE',  ( -29.11697232824620940, 1.969303236402622170, 11.84416604000747064 ) ) ;
#10215 = CARTESIAN_POINT ( 'NONE',  ( 2.000000000000001776, 0.000000000000000000, 0.000000000000000000 ) ) ;
#10216 = FACE_OUTER_BOUND ( 'NONE', #7473, .T. ) ;
#10217 = EDGE_CURVE ( 'NONE', #26820, #6851, #47229, .T. ) ;
#10218 = LINE ( 'NONE', #60434, #32278 ) ;
#10219 = ORIENTED_EDGE ( 'NONE', *, *, #19673, .T. ) ;
#10220 = CARTESIAN_POINT ( 'NONE',  ( 2.251152103363646351, 7.636644423939539905, -0.1252683866805369139 ) ) ;
#10221 = EDGE_CURVE ( 'NONE', #29813, #18977, #14235, .T. ) ;
#10222 = CARTESIAN_POINT ( 'NONE',  ( 23.65879480623153341, 9.643861506414504348, -7.147527680982785903 ) ) ;
#10223 = CARTESIAN_POINT ( 'NONE',  ( 0.3665391374699467075, -10.50279796150432610, -6.368473106897240221 ) ) ;
#10224 = CARTESIAN_POINT ( 'NONE',  ( 11.98572745786314719, 10.93103263098930178, -7.928810397812742217 ) ) ;
#10225 = CARTESIAN_POINT ( 'NONE',  ( -19.62351202312758502, -4.052328796303131142, 12.87840960595547557 ) ) ;
#10226 = DIRECTION ( 'NONE',  ( 1.000000000000000000, -0.000000000000000000, -0.000000000000000000 ) ) ;
#10227 = CARTESIAN_POINT ( 'NONE',  ( 2.665405856346780844, 8.776564688671614434, 3.808819464940459643 ) ) ;
#10228 = DIRECTION ( 'NONE',  ( 0.000000000000000000, -0.01356324068817991828, 0.9999080150203990547 ) ) ;
#10229 = VERTEX_POINT ( 'NONE', #42346 ) ;
#10230 = DIRECTION ( 'NONE',  ( 0.000000000000000000, 0.01356324068817998940, -0.9999080150203990547 ) ) ;
#10231 = AXIS2_PLACEMENT_3D ( 'NONE', #37756, #8474, #54033 ) ;
#10232 = AXIS2_PLACEMENT_3D ( 'NONE', #25980, #20963, #45265 ) ;
#10233 = ORIENTED_EDGE ( 'NONE', *, *, #5397, .F. ) ;
#10234 = CARTESIAN_POINT ( 'NONE',  ( -2.532614230583026593, -5.020478806276874373, 10.89930238848911337 ) ) ;
#10235 = CARTESIAN_POINT ( 'NONE',  ( -22.30986928587821794, -3.771068405887398889, 0.2539257557460667392 ) ) ;
#10236 = CARTESIAN_POINT ( 'NONE',  ( -16.58812090467340283, 7.647128368881745075, -11.12581290275694457 ) ) ;
#10237 = CARTESIAN_POINT ( 'NONE',  ( 2.556980015513528048, -7.658710847181453119, -1.116161541731783835 ) ) ;
#10238 = FACE_OUTER_BOUND ( 'NONE', #37710, .T. ) ;
#10239 = ORIENTED_EDGE ( 'NONE', *, *, #3322, .T. ) ;
#10240 = LINE ( 'NONE', #5614, #65382 ) ;
#10241 = CARTESIAN_POINT ( 'NONE',  ( 36.00000000000000711, -10.49626516989275693, -7.238157050195595410 ) ) ;
#10242 = LINE ( 'NONE', #20568, #33281 ) ;
#10243 = CARTESIAN_POINT ( 'NONE',  ( 2.241451721903217731, -6.581017239736936197, -3.869794645251186882 ) ) ;
#10244 = EDGE_CURVE ( 'NONE', #42103, #57333, #31179, .T. ) ;
#10245 = CARTESIAN_POINT ( 'NONE',  ( -19.16048775240928848, -3.902570516164022507, 11.34881310738079740 ) ) ;
#10246 = CARTESIAN_POINT ( 'NONE',  ( -28.41827485489077532, 3.509237424706437292, 25.00000000000000000 ) ) ;
#10247 = EDGE_LOOP ( 'NONE', ( #3276, #48861, #1039, #41677 ) ) ;
#10248 = CARTESIAN_POINT ( 'NONE',  ( 0.9232058338315048962, 12.34162163148536351, -1.793035206307219243 ) ) ;
#10249 = ORIENTED_EDGE ( 'NONE', *, *, #10342, .T. ) ;
#10250 = CARTESIAN_POINT ( 'NONE',  ( -35.00000000000000000, 0.000000000000000000, 0.000000000000000000 ) ) ;
#10251 = CARTESIAN_POINT ( 'NONE',  ( -26.43258404273187168, -3.148308537883188318, 1.478864324198218450 ) ) ;
#10252 = EDGE_CURVE ( 'NONE', #18553, #13952, #48034, .T. ) ;
#10253 = CARTESIAN_POINT ( 'NONE',  ( 28.26028539291078800, -10.45631606572639249, 5.900903393808790476 ) ) ;
#10254 = CARTESIAN_POINT ( 'NONE',  ( 0.3537226245948391634, -11.62199823003436805, 3.952322262392347518 ) ) ;
#10255 = EDGE_CURVE ( 'NONE', #7701, #55855, #29174, .T. ) ;
#10256 = EDGE_LOOP ( 'NONE', ( #49796, #511, #19972, #21706 ) ) ;
#10257 = ORIENTED_EDGE ( 'NONE', *, *, #51663, .F. ) ;
#10258 = FACE_OUTER_BOUND ( 'NONE', #22737, .T. ) ;
#10259 = B_SPLINE_CURVE_WITH_KNOTS ( 'NONE', 3,
 ( #55515, #15270, #19286, #45206, #29260, #29565, #65468 ),
 .UNSPECIFIED., .F., .F.,
 ( 4, 3, 4 ),
 ( 6.408539315702728266E-15, 0.002398160485434724411, 0.005002426799383169823 ),
 .UNSPECIFIED. ) ;
#10260 = EDGE_LOOP ( 'NONE', ( #56909, #24664, #6707, #9472 ) ) ;
#10261 = CARTESIAN_POINT ( 'NONE',  ( -35.00000000000000000, 5.130401251914729954, 11.05394794832831451 ) ) ;
#10262 = DIRECTION ( 'NONE',  ( 0.000000000000000000, 0.01356324068817998940, -0.9999080150203990547 ) ) ;
#10263 = CARTESIAN_POINT ( 'NONE',  ( 5.530133899448235191, -0.006998616117863969491, 0.01437126147332079724 ) ) ;
#10264 = CARTESIAN_POINT ( 'NONE',  ( 0.4626703367442814852, 9.247028139127523971, 8.128802338754262280 ) ) ;
#10265 = CARTESIAN_POINT ( 'NONE',  ( 1.459561108994217760, 9.267924853468691992, -8.601340491611662031 ) ) ;
#10266 = CARTESIAN_POINT ( 'NONE',  ( 0.4626703367448971038, 10.80124546303580324, -5.909149965570888341 ) ) ;
#10267 = CARTESIAN_POINT ( 'NONE',  ( 2.000000000000001776, -6.201547234536999298, -2.820401998297984214 ) ) ;
#10268 = VERTEX_POINT ( 'NONE', #5934 ) ;
#10269 = EDGE_CURVE ( 'NONE', #36872, #24889, #39792, .T. ) ;
#10270 = CARTESIAN_POINT ( 'NONE',  ( 2.705197763288551993, -2.399370654839219963, -7.410249563424446961 ) ) ;
#10271 = ORIENTED_EDGE ( 'NONE', *, *, #44522, .T. ) ;
#10272 = CIRCLE ( 'NONE', #32564, 4.999999999999999112 ) ;
#10273 = CARTESIAN_POINT ( 'NONE',  ( 0.000000000000000000, -1.734723475976807094E-15, 13.50000000000000178 ) ) ;
#10274 = CARTESIAN_POINT ( 'NONE',  ( -27.08579483061178905, 1.879952013013922674, -1.318128465626136059 ) ) ;
#10275 = VERTEX_POINT ( 'NONE', #43027 ) ;
#10276 = CARTESIAN_POINT ( 'NONE',  ( -22.27721038036499834, 3.635620891621742512, -0.5802312083658389685 ) ) ;
#10277 = EDGE_LOOP ( 'NONE', ( #28068, #25256, #62941, #16891, #51375, #41468 ) ) ;
#10278 = DIRECTION ( 'NONE',  ( -1.000000000000000000, -0.000000000000000000, 0.000000000000000000 ) ) ;
#10279 =( BOUNDED_SURFACE ( )  B_SPLINE_SURFACE ( 3, 1, ( 
 ( #13456, #9441 ),
 ( #29728, #53723 ),
 ( #48730, #23120 ),
 ( #64007, #14112 ) ),
 .UNSPECIFIED., .F., .F., .F. ) 
 B_SPLINE_SURFACE_WITH_KNOTS ( ( 4, 4 ),
 ( 2, 2 ),
 ( 0.000000000000000000, 1.000000000000000000 ),
 ( 0.000000000000000000, 1.000000000000000000 ),
 .UNSPECIFIED. ) 
 GEOMETRIC_REPRESENTATION_ITEM ( )  RATIONAL_B_SPLINE_SURFACE ( (
 ( 1.000000000000000000, 1.000000000000000000),
 ( 0.6933888150995267674, 0.9895912004443193632),
 ( 0.6933888150995267674, 0.9895912004443193632),
 ( 1.000000000000000000, 1.000000000000000000) ) ) 
 REPRESENTATION_ITEM ( '' )  SURFACE ( )  );
#10280 = DIRECTION ( 'NONE',  ( 1.000000000000000000, -0.000000000000000000, 0.000000000000000000 ) ) ;
#10282 = EDGE_CURVE ( 'NONE', #22247, #41192, #61415, .T. ) ;
#10281 = CARTESIAN_POINT ( 'NONE',  ( 35.00000000000000000, 11.47758908105697806, 2.497432891016712286 ) ) ;
#10283 = CARTESIAN_POINT ( 'NONE',  ( -27.10512513516277977, -2.289566223068223216, -0.5469390009826222698 ) ) ;
#10284 = ORIENTED_EDGE ( 'NONE', *, *, #3045, .T. ) ;
#10285 = ORIENTED_EDGE ( 'NONE', *, *, #65148, .T. ) ;
#10286 = CARTESIAN_POINT ( 'NONE',  ( 2.963017218115620022, -7.004145770368796597, 3.599595431209464902 ) ) ;
#10288 = ORIENTED_EDGE ( 'NONE', *, *, #48209, .F. ) ;
#10287 = ADVANCED_FACE ( 'NONE', ( #26190 ), #15854, .T. ) ;
#10289 = DIRECTION ( 'NONE',  ( -1.000000000000000000, 0.000000000000000000, 0.000000000000000000 ) ) ;
#10290 = VERTEX_POINT ( 'NONE', #275 ) ;
#10291 = VERTEX_POINT ( 'NONE', #10891 ) ;
#10293 = EDGE_CURVE ( 'NONE', #37272, #15604, #12426, .T. ) ;
#10292 = EDGE_LOOP ( 'NONE', ( #44199, #48579, #40581, #51056 ) ) ;
#10294 = LINE ( 'NONE', #55863, #26701 ) ;
#10295 = CARTESIAN_POINT ( 'NONE',  ( 13.26780778037857900, -27.53645921949368258, 12.33502842928021792 ) ) ;
#10296 = CARTESIAN_POINT ( 'NONE',  ( 1.719304012338199517, 0.000000000000000000, 0.000000000000000000 ) ) ;
#10297 = DIRECTION ( 'NONE',  ( -1.000000000000000000, -1.836970198721029688E-16, -0.000000000000000000 ) ) ;
#10298 = CARTESIAN_POINT ( 'NONE',  ( 37.00000000000000711, -11.47561260193572963, 5.556331110570524423 ) ) ;
#10299 = ORIENTED_EDGE ( 'NONE', *, *, #11984, .T. ) ;
#10300 = EDGE_CURVE ( 'NONE', #19566, #60035, #17108, .T. ) ;
#10301 = ADVANCED_FACE ( 'NONE', ( #57692 ), #47700, .T. ) ;
#10302 = DIRECTION ( 'NONE',  ( 1.000000000000000000, 0.000000000000000000, 0.000000000000000000 ) ) ;
#10303 = VERTEX_POINT ( 'NONE', #47385 ) ;
#10304 = DIRECTION ( 'NONE',  ( 0.000000000000000000, 0.01356324068817998940, -0.9999080150203990547 ) ) ;
#10305 = FACE_OUTER_BOUND ( 'NONE', #59680, .T. ) ;
#10306 = EDGE_CURVE ( 'NONE', #6062, #44602, #48321, .T. ) ;
#10307 = ORIENTED_EDGE ( 'NONE', *, *, #6654, .T. ) ;
#10308 = CARTESIAN_POINT ( 'NONE',  ( 0.2706063244537997847, -10.69357582853951172, 5.971590789837488700 ) ) ;
#10309 = CARTESIAN_POINT ( 'NONE',  ( 1.937114397841932290, -9.228205347192393049, -8.920887662793566264 ) ) ;
#10310 = CARTESIAN_POINT ( 'NONE',  ( -37.00000000000000711, 12.18632975068353197, 0.06441628369840694812 ) ) ;
#10311 = VERTEX_POINT ( 'NONE', #52700 ) ;
#10312 = CARTESIAN_POINT ( 'NONE',  ( -22.27384469013076185, 1.508555848190777926, -3.358914544760239540 ) ) ;
#10313 = AXIS2_PLACEMENT_3D ( 'NONE', #20372, #30019, #50332 ) ;
#10314 = EDGE_LOOP ( 'NONE', ( #47846, #39668, #12776, #5483 ) ) ;
#10315 = CARTESIAN_POINT ( 'NONE',  ( -10.48620311856347875, -9.720786832536937538, -7.036071585506805448 ) ) ;
#10316 = CARTESIAN_POINT ( 'NONE',  ( -15.65911990706704593, -28.15205781829745035, -10.62195165830229726 ) ) ;
#10317 = CARTESIAN_POINT ( 'NONE',  ( 2.705197763288547552, 6.881024880055393922, -3.649695155981438344 ) ) ;
#10318 = CARTESIAN_POINT ( 'NONE',  ( 2.781367136451930566, 4.171010984502898644, 6.608147481822022939 ) ) ;
#10319 = CARTESIAN_POINT ( 'NONE',  ( 3.092491956584929369, 7.863103788722181520, 0.9322768171848894170 ) ) ;
#10320 = ORIENTED_EDGE ( 'NONE', *, *, #8646, .T. ) ;
#10321 = CARTESIAN_POINT ( 'NONE',  ( -35.00000000000000000, -10.32377448871672598, 6.475373545682264975 ) ) ;
#10322 = CARTESIAN_POINT ( 'NONE',  ( 35.00000000000000000, -8.534258022646033837, 8.699265615723071221 ) ) ;
#10323 = DIRECTION ( 'NONE',  ( 1.000000000000000000, -0.000000000000000000, 0.000000000000000000 ) ) ;
#10324 = CIRCLE ( 'NONE', #40031, 5.000000000000002665 ) ;
#10325 = CARTESIAN_POINT ( 'NONE',  ( 22.22052407907419180, -12.61035851597580049, -4.822980926764052434 ) ) ;
#10326 = B_SPLINE_CURVE_WITH_KNOTS ( 'NONE', 3,
 ( #9437, #23793, #39381, #44059, #60013, #14110, #64977, #14433, #35026, #3847, #60655, #15093, #13772, #34064, #24103, #34708, #29411, #44363, #34404 ),
 .UNSPECIFIED., .F., .F.,
 ( 4, 3, 3, 3, 3, 3, 4 ),
 ( 9.600547486887170186E-18, 4.457896483015377217E-05, 6.639290541542671223E-05, 8.820687556479552720E-05, 0.0001100173248778994853, 0.0001545671401658188244, 0.0001830328308068574113 ),
 .UNSPECIFIED. ) ;
#10327 = EDGE_CURVE ( 'NONE', #14666, #43301, #37063, .T. ) ;
#10328 = AXIS2_PLACEMENT_3D ( 'NONE', #1564, #31469, #51769 ) ;
#10329 = LINE ( 'NONE', #15639, #27605 ) ;
#10330 = DIRECTION ( 'NONE',  ( -1.000000000000000000, 0.000000000000000000, 0.000000000000000000 ) ) ;
#10331 = CARTESIAN_POINT ( 'NONE',  ( 0.3665391374699465965, 11.44911061034392574, -4.447929964102732114 ) ) ;
#10332 = CARTESIAN_POINT ( 'NONE',  ( 1.452237505248555660, 9.303501428256145900, -8.579708443906651993 ) ) ;
#10333 = CARTESIAN_POINT ( 'NONE',  ( 2.290907136833252533, 0.1622757685886151990, -7.649199419879185058 ) ) ;
#10334 = EDGE_CURVE ( 'NONE', #14286, #44679, #54720, .T. ) ;
#10335 = ORIENTED_EDGE ( 'NONE', *, *, #19283, .T. ) ;
#10336 = ORIENTED_EDGE ( 'NONE', *, *, #36913, .T. ) ;
#10337 = LINE ( 'NONE', #5370, #28973 ) ;
#10338 = CARTESIAN_POINT ( 'NONE',  ( 45.36026561873625695, -0.9018867892165788325, -12.73108497882287793 ) ) ;
#10339 = CYLINDRICAL_SURFACE ( 'NONE', #7736, 12.18650000000000055 ) ;
#10340 = CARTESIAN_POINT ( 'NONE',  ( 2.000000000000001776, -6.164400007374764456, -2.900694413976575792 ) ) ;
#10341 = ORIENTED_EDGE ( 'NONE', *, *, #9103, .T. ) ;
#10342 = EDGE_CURVE ( 'NONE', #2029, #6394, #27401, .T. ) ;
#10343 = ORIENTED_EDGE ( 'NONE', *, *, #40054, .T. ) ;
#10344 = ORIENTED_EDGE ( 'NONE', *, *, #20981, .T. ) ;
#10345 = DIRECTION ( 'NONE',  ( -1.000000000000000000, 0.000000000000000000, -0.000000000000000000 ) ) ;
#10346 = CIRCLE ( 'NONE', #44333, 5.000000000000000000 ) ;
#10347 = CARTESIAN_POINT ( 'NONE',  ( -22.39032720737627002, 1.170177197944874958, 3.847057950743270283 ) ) ;
#10348 = ORIENTED_EDGE ( 'NONE', *, *, #37229, .T. ) ;
#10349 = CARTESIAN_POINT ( 'NONE',  ( 2.177405672431371730, -0.6747479782259577785, -11.17876532285605151 ) ) ;
#10350 = FACE_OUTER_BOUND ( 'NONE', #3561, .T. ) ;
#10351 = FACE_OUTER_BOUND ( 'NONE', #44024, .T. ) ;
#10353 = ORIENTED_EDGE ( 'NONE', *, *, #49107, .T. ) ;
#10352 = AXIS2_PLACEMENT_3D ( 'NONE', #6234, #16540, #36808 ) ;
#10354 = LINE ( 'NONE', #61891, #1425 ) ;
#10355 = CARTESIAN_POINT ( 'NONE',  ( -1.806230668642109460, -30.59323697347973336, -15.24264478004127987 ) ) ;
#10356 = CARTESIAN_POINT ( 'NONE',  ( 1.000000000000000888, 2.315790869867174528, -7.133520354428103616 ) ) ;
#10357 = ORIENTED_EDGE ( 'NONE', *, *, #25890, .T. ) ;
#10358 = FACE_OUTER_BOUND ( 'NONE', #54527, .T. ) ;
#10359 = ORIENTED_EDGE ( 'NONE', *, *, #30338, .T. ) ;
#10360 = CARTESIAN_POINT ( 'NONE',  ( 0.3654063281920756356, -6.366443614636611237, -10.50027211615253542 ) ) ;
#10361 = ORIENTED_EDGE ( 'NONE', *, *, #65354, .T. ) ;
#10362 = DIRECTION ( 'NONE',  ( 0.000000000000000000, -1.000000000000000000, 0.000000000000000000 ) ) ;
#10363 = EDGE_CURVE ( 'NONE', #10393, #40729, #5600, .T. ) ;
#10364 = DIRECTION ( 'NONE',  ( 0.000000000000000000, -0.01356324068818000328, 0.9999080150203990547 ) ) ;
#10365 = CYLINDRICAL_SURFACE ( 'NONE', #46045, 5.000000000000000888 ) ;
#10366 = DIRECTION ( 'NONE',  ( 0.000000000000000000, 0.000000000000000000, 1.000000000000000000 ) ) ;
#10367 = CARTESIAN_POINT ( 'NONE',  ( 35.00000000000000000, -6.547236723513950807, 9.752226076388957665 ) ) ;
#10368 = CIRCLE ( 'NONE', #5081, 5.000000000000000000 ) ;
#10369 = CARTESIAN_POINT ( 'NONE',  ( 12.52750123246316072, 0.4973700281276248192, -11.98968819674306374 ) ) ;
#10370 = CARTESIAN_POINT ( 'NONE',  ( -27.08429572838383947, -0.2296550094122856711, -2.279961732801603080 ) ) ;
#10371 = CARTESIAN_POINT ( 'NONE',  ( 0.3160775863651080209, -3.967735865794275618, -11.60348481172939472 ) ) ;
#10373 = ORIENTED_EDGE ( 'NONE', *, *, #33838, .T. ) ;
#10372 = CARTESIAN_POINT ( 'NONE',  ( 7.283637096917835230, -6.822343376425546779, 11.65715530555193347 ) ) ;
#10374 = EDGE_CURVE ( 'NONE', #29318, #24195, #53010, .T. ) ;
#10375 = CARTESIAN_POINT ( 'NONE',  ( 1.719304012338199517, 12.20344780065974888, 3.626341562670754914 ) ) ;
#10376 = VERTEX_POINT ( 'NONE', #17447 ) ;
#10377 = CARTESIAN_POINT ( 'NONE',  ( 0.3401186441510225533, -4.436257390736900952, 11.44115600261389254 ) ) ;
#10378 = ORIENTED_EDGE ( 'NONE', *, *, #64756, .F. ) ;
#10379 = CYLINDRICAL_SURFACE ( 'NONE', #40779, 4.999999999999999112 ) ;
#10380 = EDGE_CURVE ( 'NONE', #12727, #15829, #39839, .T. ) ;
#10381 = ORIENTED_EDGE ( 'NONE', *, *, #21842, .T. ) ;
#10382 = DIRECTION ( 'NONE',  ( -1.000000000000000000, -0.000000000000000000, 0.000000000000000000 ) ) ;
#10383 = CARTESIAN_POINT ( 'NONE',  ( 1.287602823388412254, 12.00540336274551656, -3.781900355161493366 ) ) ;
#10384 = DIRECTION ( 'NONE',  ( 0.000000000000000000, -0.01356324068817998940, 0.9999080150203990547 ) ) ;
#10385 = CARTESIAN_POINT ( 'NONE',  ( -22.29677679919927868, 1.633785040807725686, -3.364642266483119482 ) ) ;
#10386 = LINE ( 'NONE', #40986, #47874 ) ;
#10387 = ORIENTED_EDGE ( 'NONE', *, *, #48130, .F. ) ;
#10388 = DIRECTION ( 'NONE',  ( 0.000000000000000000, 0.01356324068817998940, -0.9999080150203990547 ) ) ;
#10389 = ORIENTED_EDGE ( 'NONE', *, *, #60502, .T. ) ;
#10390 = DIRECTION ( 'NONE',  ( -1.000000000000000000, 0.000000000000000000, 0.000000000000000000 ) ) ;
#10391 = CARTESIAN_POINT ( 'NONE',  ( 47.00000000000000711, 4.705694406421931860E-17, -3.469127814946512892E-15 ) ) ;
#10392 = FACE_OUTER_BOUND ( 'NONE', #21931, .T. ) ;
#10393 = VERTEX_POINT ( 'NONE', #48694 ) ;
#10394 = CARTESIAN_POINT ( 'NONE',  ( 0.000000000000000000, 0.000000000000000000, 0.000000000000000000 ) ) ;
#10395 = VECTOR ( 'NONE', #24786, 1000.000000000000000 ) ;
#10396 = EDGE_CURVE ( 'NONE', #49910, #9776, #64297, .T. ) ;
#10397 = ADVANCED_FACE ( 'NONE', ( #34366 ), #24381, .T. ) ;
#10398 = AXIS2_PLACEMENT_3D ( 'NONE', #37965, #48312, #58609 ) ;
#10399 = CARTESIAN_POINT ( 'NONE',  ( -35.00000000000000000, -11.78977382767499194, 4.245927698352017110 ) ) ;
#10400 = DIRECTION ( 'NONE',  ( -0.000000000000000000, -0.000000000000000000, -1.000000000000000000 ) ) ;
#10402 = AXIS2_PLACEMENT_3D ( 'NONE', #40726, #65643, #61016 ) ;
#10401 = LINE ( 'NONE', #5783, #33849 ) ;
#10403 = EDGE_LOOP ( 'NONE', ( #52241, #18499, #40685, #19672 ) ) ;
#10404 = DIRECTION ( 'NONE',  ( -1.000000000000000000, 0.000000000000000000, 0.000000000000000000 ) ) ;
#10405 = DIRECTION ( 'NONE',  ( 1.000000000000000000, 0.000000000000000000, -0.000000000000000000 ) ) ;
#10406 = CARTESIAN_POINT ( 'NONE',  ( 1.198791140419924739, -3.806343609710814757, -11.96656299555120029 ) ) ;
#10407 = EDGE_CURVE ( 'NONE', #57508, #56892, #32385, .T. ) ;
#10408 = AXIS2_PLACEMENT_3D ( 'NONE', #61920, #56269, #51639 ) ;
#10409 = B_SPLINE_CURVE_WITH_KNOTS ( 'NONE', 3,
 ( #39266, #54897, #59562, #23331, #58604, #13026, #13350, #28640, #33635, #13996, #58938, #64222, #34282, #19974, #30926, #9651, #5348, #35898, #25619, #45249, #41224, #10003, #45912, #65198, #14631, #10635, #55885, #40242 ),
 .UNSPECIFIED., .F., .F.,
 ( 4, 2, 2, 2, 2, 2, 2, 2, 2, 2, 2, 2, 2, 4 ),
 ( 0.000000000000000000, 0.0005977287619976828954, 0.001195457523995365791, 0.001793186285993048686, 0.002390915047990731582, 0.002988643809988414477, 0.003586372571986097373, 0.004184101333983779834, 0.004781830095981463163, 0.005977287619976825485, 0.006575016381974505345, 0.007172745143972185204, 0.008368202667967547526, 0.009563660191962908980 ),
 .UNSPECIFIED. ) ;
#10410 = CARTESIAN_POINT ( 'NONE',  ( 35.00000000000000000, -12.15823808070322798, -0.8294751490778934366 ) ) ;
#10411 = CARTESIAN_POINT ( 'NONE',  ( 0.000000000000000000, 6.812627895098307462, -0.04423456934727655609 ) ) ;
#10412 = ORIENTED_EDGE ( 'NONE', *, *, #38275, .T. ) ;
#10413 = CARTESIAN_POINT ( 'NONE',  ( 22.88594695219327235, -4.822122601967141264, -10.98850006195556261 ) ) ;
#10414 = CARTESIAN_POINT ( 'NONE',  ( 0.3540037536853123390, 0.2457215634581275676, -11.99999999999999467 ) ) ;
#10415 = DIRECTION ( 'NONE',  ( -1.000000000000000000, 0.000000000000000000, -0.000000000000000000 ) ) ;
#10416 = ORIENTED_EDGE ( 'NONE', *, *, #58787, .F. ) ;
#10417 = CARTESIAN_POINT ( 'NONE',  ( -18.58686583997219088, 4.911748662621227446, 10.95194156811396269 ) ) ;
#10418 = CARTESIAN_POINT ( 'NONE',  ( -37.00000000000000711, 0.000000000000000000, 0.000000000000000000 ) ) ;
#10419 = ORIENTED_EDGE ( 'NONE', *, *, #35354, .T. ) ;
#10420 = EDGE_CURVE ( 'NONE', #45313, #43566, #57004, .T. ) ;
#10421 = EDGE_CURVE ( 'NONE', #57976, #56864, #33443, .T. ) ;
#10422 = ORIENTED_EDGE ( 'NONE', *, *, #42884, .F. ) ;
#10423 = VERTEX_POINT ( 'NONE', #7798 ) ;
#10424 = EDGE_CURVE ( 'NONE', #60869, #8336, #63967, .T. ) ;
#10425 = ORIENTED_EDGE ( 'NONE', *, *, #35309, .F. ) ;
#10426 = DIRECTION ( 'NONE',  ( 1.000000000000000000, -0.000000000000000000, 0.000000000000000000 ) ) ;
#10427 = CARTESIAN_POINT ( 'NONE',  ( 0.2653141334712546540, 6.084912053827487455, -10.62748186152491492 ) ) ;
#10428 = CARTESIAN_POINT ( 'NONE',  ( 2.000000000000001776, 1.956810415765277922, -6.654767106875532967 ) ) ;
#10429 = FACE_OUTER_BOUND ( 'NONE', #61644, .T. ) ;
#10430 = DIRECTION ( 'NONE',  ( 0.000000000000000000, -0.01356324068817998940, 0.9999080150203990547 ) ) ;
#10431 = AXIS2_PLACEMENT_3D ( 'NONE', #6553, #7868, #36798 ) ;
#10432 = CARTESIAN_POINT ( 'NONE',  ( -14.82145243739236129, -34.67135967094819193, 7.359580590752245577 ) ) ;
#10433 = DIRECTION ( 'NONE',  ( -1.000000000000000000, 0.000000000000000000, 0.000000000000000000 ) ) ;
#10435 = ORIENTED_EDGE ( 'NONE', *, *, #6633, .T. ) ;
#10434 = LINE ( 'NONE', #149, #63734 ) ;
#10436 = DIRECTION ( 'NONE',  ( 1.000000000000000000, -0.000000000000000000, -0.000000000000000000 ) ) ;
#10437 = ORIENTED_EDGE ( 'NONE', *, *, #28967, .T. ) ;
#10438 = FACE_OUTER_BOUND ( 'NONE', #48008, .T. ) ;
#10439 = ORIENTED_EDGE ( 'NONE', *, *, #29602, .F. ) ;
#10440 = ORIENTED_EDGE ( 'NONE', *, *, #20784, .F. ) ;
#10441 = CARTESIAN_POINT ( 'NONE',  ( -22.27706485742869091, -0.9832726768967594566, 3.547445275915920071 ) ) ;
#10442 = CARTESIAN_POINT ( 'NONE',  ( 4.513117160428492980, -30.90576903066112990, 14.85933548762089274 ) ) ;
#10443 = ADVANCED_FACE ( 'NONE', ( #49670 ), #18451, .T. ) ;
#10444 = AXIS2_PLACEMENT_3D ( 'NONE', #55786, #44809, #19221 ) ;
#10445 = DIRECTION ( 'NONE',  ( 1.000000000000000000, -0.000000000000000000, 0.000000000000000000 ) ) ;
#10446 = CYLINDRICAL_SURFACE ( 'NONE', #56763, 12.18649999999999878 ) ;
#10447 = CARTESIAN_POINT ( 'NONE',  ( 0.8375941296792197566, -2.537217542321857255, 12.17542732751276979 ) ) ;
#10448 = CARTESIAN_POINT ( 'NONE',  ( 37.00000000000000711, -11.16627499335657703, -3.645068577059991988 ) ) ;
#10449 = ORIENTED_EDGE ( 'NONE', *, *, #50429, .T. ) ;
#10450 = EDGE_CURVE ( 'NONE', #43107, #1369, #3074, .T. ) ;
#10451 = VECTOR ( 'NONE', #4379, 1000.000000000000000 ) ;
#10452 = AXIS2_PLACEMENT_3D ( 'NONE', #2114, #26087, #42649 ) ;
#10453 = ORIENTED_EDGE ( 'NONE', *, *, #28790, .F. ) ;
#10454 = CARTESIAN_POINT ( 'NONE',  ( 0.3537226245948369430, 12.04110684114372809, 2.388187631842557668 ) ) ;
#10455 = ORIENTED_EDGE ( 'NONE', *, *, #35006, .T. ) ;
#10456 = VECTOR ( 'NONE', #60861, 1000.000000000000000 ) ;
#10457 = ORIENTED_EDGE ( 'NONE', *, *, #36148, .T. ) ;
#10458 = LINE ( 'NONE', #25433, #32776 ) ;
#10459 = CARTESIAN_POINT ( 'NONE',  ( 9.402029343886097124, 7.266669477869928784, -9.551391452522942416 ) ) ;
#10460 = VECTOR ( 'NONE', #1900, 1000.000000000000000 ) ;
#10461 = CARTESIAN_POINT ( 'NONE',  ( 0.2676618633000450442, 0.1607051348609344621, -12.24591287309138998 ) ) ;
#10462 = CARTESIAN_POINT ( 'NONE',  ( 17.76182939893871193, -6.980167179982016634, 9.764583834413022245 ) ) ;
#10463 = CARTESIAN_POINT ( 'NONE',  ( 0.000000000000000000, 0.000000000000000000, 0.000000000000000000 ) ) ;
#10464 = CARTESIAN_POINT ( 'NONE',  ( -37.00000000000000711, -7.717887834988307105, 8.854740511458828678 ) ) ;
#10465 = ORIENTED_EDGE ( 'NONE', *, *, #998, .F. ) ;
#10466 =( BOUNDED_CURVE ( )  B_SPLINE_CURVE ( 3, ( #5767, #15389, #20377, #55954 ),
 .UNSPECIFIED., .F., .F. ) 
 B_SPLINE_CURVE_WITH_KNOTS ( ( 4, 4 ),
 ( 2.228289365106484343, 2.237843681065574852 ),
 .UNSPECIFIED. ) 
 CURVE ( )  GEOMETRIC_REPRESENTATION_ITEM ( )  RATIONAL_B_SPLINE_CURVE ( ( 1.000000000000000000, 0.9999923929350129637, 0.9999923929350129637, 1.000000000000000000 ) ) 
 REPRESENTATION_ITEM ( '' )  );
#10467 = ORIENTED_EDGE ( 'NONE', *, *, #56, .F. ) ;
#10468 = DIRECTION ( 'NONE',  ( -1.000000000000000000, 0.000000000000000000, 0.000000000000000000 ) ) ;
#10469 = CARTESIAN_POINT ( 'NONE',  ( 2.297017764050093280, 7.506328781223023938, -1.490897313050607353 ) ) ;
#10470 = CARTESIAN_POINT ( 'NONE',  ( 2.827825597296806492, 8.965636292765729820, -1.027532345921593260 ) ) ;
#10471 = CARTESIAN_POINT ( 'NONE',  ( 5.975816529957111101, -8.873589895540870742, 8.086295541294113320 ) ) ;
#10472 = AXIS2_PLACEMENT_3D ( 'NONE', #3742, #63544, #63884 ) ;
#10473 = FACE_OUTER_BOUND ( 'NONE', #21965, .T. ) ;
#10474 = EDGE_CURVE ( 'NONE', #24723, #14755, #28084, .T. ) ;
#10475 = CIRCLE ( 'NONE', #40240, 5.000000000000001776 ) ;
#10476 = DIRECTION ( 'NONE',  ( 1.000000000000000000, -0.000000000000000000, -0.000000000000000000 ) ) ;
#10477 = CARTESIAN_POINT ( 'NONE',  ( 1.462291587751446409, 2.816455204777454480, -12.32753368892871393 ) ) ;
#10478 = CARTESIAN_POINT ( 'NONE',  ( 35.00000000000000000, -1.262958560998847624, -12.12087942037209665 ) ) ;
#10479 = VERTEX_POINT ( 'NONE', #43348 ) ;
#10480 = CARTESIAN_POINT ( 'NONE',  ( -37.00000000000000711, 2.527899948230636795, 12.49688848680885300 ) ) ;
#10481 = CARTESIAN_POINT ( 'NONE',  ( 2.430348790457661057, 1.144258029164405777, -7.611893186157544733 ) ) ;
#10482 = DIRECTION ( 'NONE',  ( 0.000000000000000000, -1.000000000000000000, 0.000000000000000000 ) ) ;
#10483 = CIRCLE ( 'NONE', #47673, 4.999999999999999112 ) ;
#10484 = EDGE_CURVE ( 'NONE', #25959, #48365, #8126, .T. ) ;
#10485 = CARTESIAN_POINT ( 'NONE',  ( 2.931247277082683844, -6.618030015945706168, -4.248542803114408350 ) ) ;
#10486 = CARTESIAN_POINT ( 'NONE',  ( 2.589278595513622605, -7.197074516942377542, 2.875840518181560501 ) ) ;
#10487 = AXIS2_PLACEMENT_3D ( 'NONE', #29, #56211, #10651 ) ;
#10488 = ORIENTED_EDGE ( 'NONE', *, *, #7381, .T. ) ;
#10489 = DIRECTION ( 'NONE',  ( -1.000000000000000000, 0.000000000000000000, -0.000000000000000000 ) ) ;
#10490 = CARTESIAN_POINT ( 'NONE',  ( 12.85491158824215496, -28.99999999999999645, -3.284771503683511007 ) ) ;
#10491 = EDGE_LOOP ( 'NONE', ( #14427, #35217, #39288, #1397 ) ) ;
#10492 = CONICAL_SURFACE ( 'NONE', #13681, 7.938172270156617749, 1.280189991382167047 ) ;
#10493 = CARTESIAN_POINT ( 'NONE',  ( 22.88594695219327235, 3.421158645304719137, -13.05931366970166962 ) ) ;
#10494 = CARTESIAN_POINT ( 'NONE',  ( 37.00000000000000711, 4.705694406421931860E-17, -3.469127814946512892E-15 ) ) ;
#10495 = CARTESIAN_POINT ( 'NONE',  ( 5.514970785353741078, 0.003929719953530106356, -0.002619824551223715308 ) ) ;
#10496 = VECTOR ( 'NONE', #4533, 1000.000000000000000 ) ;
#10498 = VERTEX_POINT ( 'NONE', #4455 ) ;
#10497 = CARTESIAN_POINT ( 'NONE',  ( 0.000000000000000000, 6.338823199656684615, 2.816798305433696470 ) ) ;
#10499 = CARTESIAN_POINT ( 'NONE',  ( 2.000000000000001776, 0.000000000000000000, 0.000000000000000000 ) ) ;
#10500 = DIRECTION ( 'NONE',  ( -0.3939253465568944290, 0.3234796780324307175, 0.8603393047164971108 ) ) ;
#10501 = ORIENTED_EDGE ( 'NONE', *, *, #45732, .F. ) ;
#10502 = CARTESIAN_POINT ( 'NONE',  ( 0.3002738374340832572, 7.705051734330280233, 9.533456882268664501 ) ) ;
#10503 = CARTESIAN_POINT ( 'NONE',  ( -8.648406403777006091, 10.29074439593462742, -8.744330510103520027 ) ) ;
#10504 = CARTESIAN_POINT ( 'NONE',  ( -22.27706485742869091, -0.3729136217355977778, -3.662257305743823022 ) ) ;
#10505 = FACE_OUTER_BOUND ( 'NONE', #2848, .T. ) ;
#10506 = CARTESIAN_POINT ( 'NONE',  ( 0.000000000000000000, -1.734723475976807094E-15, -13.50000000000000178 ) ) ;
#10507 = DIRECTION ( 'NONE',  ( 1.000000000000000000, 0.000000000000000000, 0.000000000000000000 ) ) ;
#10508 = DIRECTION ( 'NONE',  ( 1.000000000000000000, 0.000000000000000000, -0.000000000000000000 ) ) ;
#10509 = EDGE_LOOP ( 'NONE', ( #64100, #31033, #1428, #35788 ) ) ;
#10510 = CARTESIAN_POINT ( 'NONE',  ( 2.247206125382828379, -4.996658593545098448, 5.774712443419435459 ) ) ;
#10511 = ORIENTED_EDGE ( 'NONE', *, *, #43169, .F. ) ;
#10512 =( NAMED_UNIT ( * ) PLANE_ANGLE_UNIT ( ) SI_UNIT ( $, .RADIAN. ) );
#10513 = CARTESIAN_POINT ( 'NONE',  ( 42.50000000000000000, -2.710505431213761085E-17, 1.201363017033314212E-18 ) ) ;
#10514 = EDGE_CURVE ( 'NONE', #39567, #35917, #4796, .T. ) ;
#10515 = LINE ( 'NONE', #60411, #49196 ) ;
#10516 = CIRCLE ( 'NONE', #41317, 2.899999999999994582 ) ;
#10517 = B_SPLINE_CURVE_WITH_KNOTS ( 'NONE', 3,
 ( #13271, #40144, #34519, #3954, #50159, #39506, #24543, #44821, #65100, #39835, #24882, #65415, #60122, #48853, #14543, #18613, #3304, #9551 ),
 .UNSPECIFIED., .F., .F.,
 ( 4, 2, 2, 2, 2, 2, 2, 2, 4 ),
 ( 3.878959614448864246E-18, 0.001078534962646972685, 0.002157069925293941468, 0.003235604887940910033, 0.004314139850587879466, 0.005392674813234849332, 0.006471209775881817464, 0.007549744738528786463, 0.008628279701175755462 ),
 .UNSPECIFIED. ) ;
#10518 = DIRECTION ( 'NONE',  ( 1.000000000000000000, 0.000000000000000000, 0.000000000000000000 ) ) ;
#10519 = ORIENTED_EDGE ( 'NONE', *, *, #59374, .F. ) ;
#10520 = CARTESIAN_POINT ( 'NONE',  ( 37.00000000000000711, 1.903127969211351189, 11.59095880812005497 ) ) ;
#10521 = VECTOR ( 'NONE', #14955, 1000.000000000000000 ) ;
#10522 = DIRECTION ( 'NONE',  ( 0.000000000000000000, 0.01356324068817992522, -0.9999080150203990547 ) ) ;
#10523 = ORIENTED_EDGE ( 'NONE', *, *, #6916, .T. ) ;
#10524 = ORIENTED_EDGE ( 'NONE', *, *, #36354, .T. ) ;
#10525 = CARTESIAN_POINT ( 'NONE',  ( 2.653899356899941164, 7.604196386057505919, -1.606012885791470168 ) ) ;
#10526 = ORIENTED_EDGE ( 'NONE', *, *, #60566, .T. ) ;
#10527 = CARTESIAN_POINT ( 'NONE',  ( 23.66565572653340510, -9.638793819117626782, -7.154491854832797593 ) ) ;
#10528 = DIRECTION ( 'NONE',  ( 0.000000000000000000, 0.6943713148249588407, -0.7196168960969843154 ) ) ;
#10529 = CARTESIAN_POINT ( 'NONE',  ( -27.09150307427447757, 2.306459590995634468, -0.1754204729056216827 ) ) ;
#10531 = AXIS2_PLACEMENT_3D ( 'NONE', #32167, #38481, #58800 ) ;
#10530 = CARTESIAN_POINT ( 'NONE',  ( -27.10128162969832744, 1.032914450114655436, -2.102429195189573718 ) ) ;
#10532 = EDGE_CURVE ( 'NONE', #60581, #16289, #1611, .T. ) ;
#10533 = CARTESIAN_POINT ( 'NONE',  ( -35.05012975565874456, -0.01296790604420075023, -0.005092487515917999003 ) ) ;
#10534 = DIRECTION ( 'NONE',  ( -1.000000000000000000, 0.000000000000000000, 0.000000000000000000 ) ) ;
#10535 = CARTESIAN_POINT ( 'NONE',  ( -14.17344535826537744, 8.096743466816491264, -10.80418385471381448 ) ) ;
#10536 = AXIS2_PLACEMENT_3D ( 'NONE', #9578, #3336, #43876 ) ;
#10537 = ORIENTED_EDGE ( 'NONE', *, *, #61870, .T. ) ;
#10538 = LINE ( 'NONE', #46150, #50868 ) ;
#10539 = CARTESIAN_POINT ( 'NONE',  ( 22.11571975030548387, 11.89373260142252597, -1.635920820979222645 ) ) ;
#10540 = DIRECTION ( 'NONE',  ( -1.000000000000000000, 0.000000000000000000, 0.000000000000000000 ) ) ;
#10541 = DIRECTION ( 'NONE',  ( 1.000000000000000000, 0.000000000000000000, 0.000000000000000000 ) ) ;
#10542 = DIRECTION ( 'NONE',  ( 0.000000000000000000, 0.000000000000000000, 1.000000000000000000 ) ) ;
#10543 = CARTESIAN_POINT ( 'NONE',  ( 0.2671309869109518842, -10.68612389951472608, -5.982543484153332258 ) ) ;
#10544 = DIRECTION ( 'NONE',  ( -1.000000000000000000, 0.000000000000000000, -0.000000000000000000 ) ) ;
#10545 = AXIS2_PLACEMENT_3D ( 'NONE', #26683, #6095, #62252 ) ;
#10546 = DIRECTION ( 'NONE',  ( 1.000000000000000000, 0.000000000000000000, 0.000000000000000000 ) ) ;
#10547 = ADVANCED_FACE ( 'NONE', ( #51323 ), #65586, .T. ) ;
#10548 = EDGE_LOOP ( 'NONE', ( #33613, #54630, #65716, #39387 ) ) ;
#10549 = CARTESIAN_POINT ( 'NONE',  ( 0.3665391374699465965, -10.50279796150441314, 6.368473106897091895 ) ) ;
#10550 = EDGE_CURVE ( 'NONE', #13578, #18352, #24725, .T. ) ;
#10551 = ORIENTED_EDGE ( 'NONE', *, *, #27123, .T. ) ;
#10552 = EDGE_CURVE ( 'NONE', #14292, #19644, #15700, .T. ) ;
#10553 = DIRECTION ( 'NONE',  ( -0.000000000000000000, -0.000000000000000000, -1.000000000000000000 ) ) ;
#10554 = CARTESIAN_POINT ( 'NONE',  ( 0.2655924914740778187, 0.04405032194320256805, -12.24627751708824341 ) ) ;
#10555 = CARTESIAN_POINT ( 'NONE',  ( 0.2653141334712572075, -12.05242949860145707, 2.169900597054481572 ) ) ;
#10556 = ADVANCED_FACE ( 'NONE', ( #60617 ), #26039, .T. ) ;
#10557 = CARTESIAN_POINT ( 'NONE',  ( 2.941278708680199916, -5.721889327162167582, 2.226055275041770809 ) ) ;
#10558 = ORIENTED_EDGE ( 'NONE', *, *, #62484, .F. ) ;
#10559 = CARTESIAN_POINT ( 'NONE',  ( -22.27384469013076185, 2.985904959940915759, -2.154627400808017956 ) ) ;
#10560 = CARTESIAN_POINT ( 'NONE',  ( 0.000000000000000000, 4.570217215903443986, -5.218059682435596258 ) ) ;
#10561 = CARTESIAN_POINT ( 'NONE',  ( 0.000000000000000000, -3.230174184210014232, -5.998318953995379843 ) ) ;
#10562 = DIRECTION ( 'NONE',  ( 0.8914382917301157949, 0.000000000000000000, -0.4531421102008653112 ) ) ;
#10563 = B_SPLINE_CURVE_WITH_KNOTS ( 'NONE', 3,
 ( #22877, #28188, #33802, #22196, #28494, #42454, #3251 ),
 .UNSPECIFIED., .F., .F.,
 ( 4, 3, 4 ),
 ( 0.000000000000000000, 0.001700533616330527579, 0.005002426799372427547 ),
 .UNSPECIFIED. ) ;
#10564 = CIRCLE ( 'NONE', #61540, 2.899999999999995914 ) ;
#10565 = ADVANCED_FACE ( 'NONE', ( #45006 ), #14713, .T. ) ;
#10566 = CARTESIAN_POINT ( 'NONE',  ( -17.15987333477080057, -7.887593880017340631, 9.050383707664092725 ) ) ;
#10567 = CARTESIAN_POINT ( 'NONE',  ( 2.080613030138687591, 0.000000000000000000, 1.000000000000000000 ) ) ;
#10568 = VERTEX_POINT ( 'NONE', #35665 ) ;
#10569 = AXIS2_PLACEMENT_3D ( 'NONE', #61585, #65585, #36324 ) ;
#10570 = EDGE_CURVE ( 'NONE', #44077, #19066, #40323, .T. ) ;
#10571 = CARTESIAN_POINT ( 'NONE',  ( 5.520433897694421610, 0.0005131706886598308426, 0.01505375422439123381 ) ) ;
#10572 = ORIENTED_EDGE ( 'NONE', *, *, #8636, .T. ) ;
#10573 = CARTESIAN_POINT ( 'NONE',  ( 0.2653519991613815243, 12.24619736885324350, 0.02201648635046494357 ) ) ;
#10574 = CYLINDRICAL_SURFACE ( 'NONE', #45868, 2.899999999999994582 ) ;
#10575 = FACE_OUTER_BOUND ( 'NONE', #37628, .T. ) ;
#10576 = CARTESIAN_POINT ( 'NONE',  ( 0.000000000000000000, 4.604744433234674972, 5.919993978425482695 ) ) ;
#10577 = AXIS2_PLACEMENT_3D ( 'NONE', #20002, #15344, #4062 ) ;
#10578 = ORIENTED_EDGE ( 'NONE', *, *, #20439, .F. ) ;
#10579 = EDGE_LOOP ( 'NONE', ( #58734, #63860, #28043, #56975 ) ) ;
#10581 = ADVANCED_FACE ( 'NONE', ( #35978 ), #15055, .T. ) ;
#10580 = CARTESIAN_POINT ( 'NONE',  ( -29.25731281466803324, 2.966737866142446833, 11.63518418675907817 ) ) ;
#10582 = VERTEX_POINT ( 'NONE', #19746 ) ;
#10583 = AXIS2_PLACEMENT_3D ( 'NONE', #9116, #43710, #44352 ) ;
#10584 = DIRECTION ( 'NONE',  ( 1.000000000000000000, -0.000000000000000000, 0.000000000000000000 ) ) ;
#10585 = CARTESIAN_POINT ( 'NONE',  ( 35.00000000000000000, 4.705694406421931860E-17, -3.469127814946512892E-15 ) ) ;
#10586 = DIRECTION ( 'NONE',  ( 1.000000000000000000, 0.000000000000000000, 0.000000000000000000 ) ) ;
#10587 = CARTESIAN_POINT ( 'NONE',  ( -27.35552965826137140, 2.810569013793760007, -1.320216934008374920 ) ) ;
#10588 = CARTESIAN_POINT ( 'NONE',  ( 0.6473888112830228359, 9.263269341114897415, -8.203438694127560993 ) ) ;
#10589 = DIRECTION ( 'NONE',  ( -0.000000000000000000, -1.000000000000000000, -0.000000000000000000 ) ) ;
#10590 = CARTESIAN_POINT ( 'NONE',  ( 35.00000000000000000, 4.705694406421931860E-17, -3.469127814946512892E-15 ) ) ;
#10591 = ORIENTED_EDGE ( 'NONE', *, *, #1355, .T. ) ;
#10592 = CARTESIAN_POINT ( 'NONE',  ( 2.899286259009693278, -2.348384892629313825, -7.494390643303798782 ) ) ;
#10593 = AXIS2_PLACEMENT_3D ( 'NONE', #11596, #41519, #61811 ) ;
#10594 = ORIENTED_EDGE ( 'NONE', *, *, #17917, .T. ) ;
#10595 = CARTESIAN_POINT ( 'NONE',  ( -22.27718150314433387, 2.479231311682841277, 2.721613812022944945 ) ) ;
#10596 = DIRECTION ( 'NONE',  ( 1.000000000000000000, 0.000000000000000000, 0.000000000000000000 ) ) ;
#10597 = DIRECTION ( 'NONE',  ( 1.000000000000000000, -0.000000000000000000, 0.000000000000000000 ) ) ;
#10598 = EDGE_LOOP ( 'NONE', ( #38697, #19696, #24129, #16519 ) ) ;
#10599 = CARTESIAN_POINT ( 'NONE',  ( -22.27721056931765631, 3.610969226755196715, -0.7178530073137425749 ) ) ;
#10600 = ORIENTED_EDGE ( 'NONE', *, *, #12462, .T. ) ;
#10601 = CARTESIAN_POINT ( 'NONE',  ( 2.177405672433375017, 11.12610351584940815, 1.276675186593112743 ) ) ;
#10602 = DIRECTION ( 'NONE',  ( -1.000000000000000000, 0.000000000000000000, 0.000000000000000000 ) ) ;
#10603 = CARTESIAN_POINT ( 'NONE',  ( 2.653899356899894091, 7.209790345489538232, -2.902068786425278546 ) ) ;
#10604 = ORIENTED_EDGE ( 'NONE', *, *, #32866, .T. ) ;
#10605 = ORIENTED_EDGE ( 'NONE', *, *, #7068, .F. ) ;
#10606 = DIRECTION ( 'NONE',  ( -1.000000000000000000, 0.000000000000000000, -0.000000000000000000 ) ) ;
#10607 = ORIENTED_EDGE ( 'NONE', *, *, #16469, .T. ) ;
#10608 = DIRECTION ( 'NONE',  ( -0.000000000000000000, -0.000000000000000000, -1.000000000000000000 ) ) ;
#10609 = VERTEX_POINT ( 'NONE', #55648 ) ;
#10610 = VERTEX_POINT ( 'NONE', #54973 ) ;
#10611 = VERTEX_POINT ( 'NONE', #65280 ) ;
#10612 = DIRECTION ( 'NONE',  ( -0.000000000000000000, -0.000000000000000000, -1.000000000000000000 ) ) ;
#10613 = CARTESIAN_POINT ( 'NONE',  ( 16.71517827323052430, -28.42750353049531498, 9.642361815241610401 ) ) ;
#10614 = ADVANCED_FACE ( 'NONE', ( #40005 ), #60286, .T. ) ;
#10615 = AXIS2_PLACEMENT_3D ( 'NONE', #16704, #51330, #6415 ) ;
#10617 = VECTOR ( 'NONE', #47539, 1000.000000000000000 ) ;
#10616 = DIRECTION ( 'NONE',  ( 0.000000000000000000, 0.3554799084908968343, 0.9346839223284540976 ) ) ;
#10618 = CARTESIAN_POINT ( 'NONE',  ( 22.61491127797214062, 25.00000000000000000, 9.376349503825034404 ) ) ;
#10619 = CARTESIAN_POINT ( 'NONE',  ( 37.00000000000000711, 9.926225166347027340, -6.280308599560179061 ) ) ;
#10620 = ORIENTED_EDGE ( 'NONE', *, *, #43943, .F. ) ;
#10621 = CARTESIAN_POINT ( 'NONE',  ( 1.459561108992494027, 11.25243317554858713, 5.767168887069277439 ) ) ;
#10622 = ORIENTED_EDGE ( 'NONE', *, *, #28061, .T. ) ;
#10623 = DIRECTION ( 'NONE',  ( -1.000000000000000000, 0.000000000000000000, 0.000000000000000000 ) ) ;
#10624 = CARTESIAN_POINT ( 'NONE',  ( 0.000000000000000000, -0.8935325819928070512, -7.446583077151393226 ) ) ;
#10625 = CARTESIAN_POINT ( 'NONE',  ( 2.305787727787084407, -5.970480882365190034, -4.792270232040956479 ) ) ;
#10626 = DIRECTION ( 'NONE',  ( 1.000000000000000000, 0.000000000000000000, -0.000000000000000000 ) ) ;
#10627 = CARTESIAN_POINT ( 'NONE',  ( 2.990245332647858856, -3.789007530133526203, -7.587819667496388476 ) ) ;
#10628 = CARTESIAN_POINT ( 'NONE',  ( 1.287602823388592554, -10.61402828236312423, -6.765713844066213234 ) ) ;
#10629 = ADVANCED_FACE ( 'NONE', ( #9741 ), #40992, .T. ) ;
#10630 = ORIENTED_EDGE ( 'NONE', *, *, #42655, .F. ) ;
#10631 = CARTESIAN_POINT ( 'NONE',  ( 37.00000000000000711, 12.74921544981111055, -0.1414404973752615424 ) ) ;
#10632 = AXIS2_PLACEMENT_3D ( 'NONE', #63737, #58803, #28193 ) ;
#10633 = VERTEX_POINT ( 'NONE', #49995 ) ;
#10634 = ADVANCED_FACE ( 'NONE', ( #102 ), #25706, .T. ) ;
#10635 = CARTESIAN_POINT ( 'NONE',  ( -25.13178613359605507, -8.065324219543505535, 10.83205263566206078 ) ) ;
#10636 = CARTESIAN_POINT ( 'NONE',  ( 9.372867312212076030, -27.54793913079790713, 14.59713702163756288 ) ) ;
#10637 = CARTESIAN_POINT ( 'NONE',  ( -35.00000000000000000, 0.000000000000000000, 0.000000000000000000 ) ) ;
#10638 = ADVANCED_FACE ( 'NONE', ( #20384 ), #45991, .T. ) ;
#10639 = DIRECTION ( 'NONE',  ( 0.000000000000000000, -0.4698238015817425839, -0.8827602140260283337 ) ) ;
#10640 = ORIENTED_EDGE ( 'NONE', *, *, #60930, .T. ) ;
#10641 = DIRECTION ( 'NONE',  ( -0.6147887355352408267, -0.7886918350401376232, 0.000000000000000000 ) ) ;
#10643 = AXIS2_PLACEMENT_3D ( 'NONE', #19863, #40125, #35129 ) ;
#10642 = CARTESIAN_POINT ( 'NONE',  ( 37.00000000000000711, 8.366449238204499039, 9.621072037176899627 ) ) ;
#10644 = CARTESIAN_POINT ( 'NONE',  ( 2.406456491626456806, 2.427896847126206126, 10.14681500356066124 ) ) ;
#10645 = CARTESIAN_POINT ( 'NONE',  ( 22.62155329971168172, -12.20561453419441200, -5.777527435223176688 ) ) ;
#10646 = B_SPLINE_CURVE_WITH_KNOTS ( 'NONE', 3,
 ( #10655, #5708, #36602, #17553, #35608, #30301, #36257, #61216, #30608, #50597, #1030, #40600, #16325, #5040, #55899, #25981, #10333, #21297, #56904 ),
 .UNSPECIFIED., .F., .F.,
 ( 4, 3, 3, 3, 3, 3, 4 ),
 ( 1.355252715606880543E-20, 2.831840207499286354E-05, 4.217266859840029938E-05, 5.602024318395480761E-05, 6.290810167968589916E-05, 9.120440630944714989E-05, 0.0001153103026479765912 ),
 .UNSPECIFIED. ) ;
#10647 = EDGE_CURVE ( 'NONE', #3974, #57258, #47270, .T. ) ;
#10648 = AXIS2_PLACEMENT_3D ( 'NONE', #64910, #44976, #54653 ) ;
#10649 = CARTESIAN_POINT ( 'NONE',  ( 0.3223008802179241905, 12.26274332232494224, -0.2444878876723663164 ) ) ;
#10650 = EDGE_CURVE ( 'NONE', #1853, #1800, #40899, .T. ) ;
#10651 = DIRECTION ( 'NONE',  ( 0.000000000000000000, 0.01356324068817998940, -0.9999080150203990547 ) ) ;
#10652 = AXIS2_PLACEMENT_3D ( 'NONE', #45770, #35458, #232 ) ;
#10653 = DIRECTION ( 'NONE',  ( -1.000000000000000000, 0.000000000000000000, 0.000000000000000000 ) ) ;
#10654 = FACE_OUTER_BOUND ( 'NONE', #42201, .T. ) ;
#10655 = CARTESIAN_POINT ( 'NONE',  ( 2.241352910868908310, 0.08337961031714861970, -7.633946224498473043 ) ) ;
#10656 = EDGE_CURVE ( 'NONE', #15829, #40279, #6915, .T. ) ;
#10657 = VECTOR ( 'NONE', #7903, 1000.000000000000000 ) ;
#10658 = PRESENTATION_LAYER_ASSIGNMENT (  '', '', ( #22337 ) ) ;
#10659 = CIRCLE ( 'NONE', #61647, 5.000000000000000000 ) ;
#10660 = ORIENTED_EDGE ( 'NONE', *, *, #32319, .F. ) ;
#10661 = ADVANCED_FACE ( 'NONE', ( #6406 ), #7367, .T. ) ;
#10662 = VERTEX_POINT ( 'NONE', #22017 ) ;
#10664 = FACE_OUTER_BOUND ( 'NONE', #54885, .T. ) ;
#10663 =( BOUNDED_CURVE ( )  B_SPLINE_CURVE ( 3, ( #11113, #4497, #5142, #30711 ),
 .UNSPECIFIED., .F., .F. ) 
 B_SPLINE_CURVE_WITH_KNOTS ( ( 4, 4 ),
 ( 2.222160218901154227, 2.254442315838258271 ),
 .UNSPECIFIED. ) 
 CURVE ( )  GEOMETRIC_REPRESENTATION_ITEM ( )  RATIONAL_B_SPLINE_CURVE ( ( 1.000000000000000000, 0.9999131574035865500, 0.9999131574035865500, 1.000000000000000000 ) ) 
 REPRESENTATION_ITEM ( '' )  );
#10665 = CARTESIAN_POINT ( 'NONE',  ( 35.62380706382416662, -2.504225566391072189, -21.57767586339569732 ) ) ;
#10666 = DIRECTION ( 'NONE',  ( -1.000000000000000000, 0.000000000000000000, 0.000000000000000000 ) ) ;
#10667 = EDGE_CURVE ( 'NONE', #50465, #32047, #37718, .T. ) ;
#10668 = CARTESIAN_POINT ( 'NONE',  ( -35.00000000000000000, 6.657191900728318679, 9.677500615117924809 ) ) ;
#10669 = ORIENTED_EDGE ( 'NONE', *, *, #25384, .T. ) ;
#10670 = ORIENTED_EDGE ( 'NONE', *, *, #6516, .T. ) ;
#10671 = ORIENTED_EDGE ( 'NONE', *, *, #9100, .T. ) ;
#10672 = CARTESIAN_POINT ( 'NONE',  ( 2.440552418640498544, 2.818488640081671548, -7.166505277347694047 ) ) ;
#10673 = AXIS2_PLACEMENT_3D ( 'NONE', #5821, #1132, #16434 ) ;
#10674 = DIRECTION ( 'NONE',  ( -1.000000000000000000, 0.000000000000000000, 0.000000000000000000 ) ) ;
#10675 = VERTEX_POINT ( 'NONE', #31345 ) ;
#10676 = CARTESIAN_POINT ( 'NONE',  ( -17.90400865550613574, 4.131545694691102000, -11.26818433703756384 ) ) ;
#10677 = VECTOR ( 'NONE', #56445, 1000.000000000000000 ) ;
#10678 = VECTOR ( 'NONE', #56597, 1000.000000000000000 ) ;
#10679 = DIRECTION ( 'NONE',  ( -1.000000000000000000, 0.000000000000000000, 0.000000000000000000 ) ) ;
#10680 = ORIENTED_EDGE ( 'NONE', *, *, #25667, .T. ) ;
#10681 = CARTESIAN_POINT ( 'NONE',  ( 2.269879328257222717, 4.798845682293883641, -5.949827370244219260 ) ) ;
#10682 = CARTESIAN_POINT ( 'NONE',  ( 13.98043512791030096, -30.12632228061958273, -5.689268883804940558 ) ) ;
#10683 = DIRECTION ( 'NONE',  ( -0.000000000000000000, -0.000000000000000000, -1.000000000000000000 ) ) ;
#10684 = ORIENTED_EDGE ( 'NONE', *, *, #40794, .T. ) ;
#10685 = AXIS2_PLACEMENT_3D ( 'NONE', #4448, #53995, #8438 ) ;
#10686 = DIRECTION ( 'NONE',  ( -0.000000000000000000, -0.000000000000000000, -1.000000000000000000 ) ) ;
#10687 = ORIENTED_EDGE ( 'NONE', *, *, #43508, .F. ) ;
#10688 = DIRECTION ( 'NONE',  ( -1.000000000000000000, 0.000000000000000000, 0.000000000000000000 ) ) ;
#10689 = AXIS2_PLACEMENT_3D ( 'NONE', #49580, #19648, #54574 ) ;
#10690 = ORIENTED_EDGE ( 'NONE', *, *, #48125, .F. ) ;
#10691 = CYLINDRICAL_SURFACE ( 'NONE', #12820, 4.999999999999999112 ) ;
#10692 = CARTESIAN_POINT ( 'NONE',  ( -6.824045466191706488, -31.96248520358720668, 13.34027024243480319 ) ) ;
#10693 = CARTESIAN_POINT ( 'NONE',  ( 2.259025283528086181, 3.937899517809479999, 6.547290863799049454 ) ) ;
#10694 = DIRECTION ( 'NONE',  ( 0.000000000000000000, 0.8009703041134146329, 0.5987040770935705414 ) ) ;
#10695 = ADVANCED_FACE ( 'NONE', ( #41964 ), #21363, .T. ) ;
#10696 = EDGE_CURVE ( 'NONE', #44942, #58777, #50444, .T. ) ;
#10697 = CARTESIAN_POINT ( 'NONE',  ( -35.00000000000000000, -1.463443770872689509, -12.09831040184925577 ) ) ;
#10698 = CARTESIAN_POINT ( 'NONE',  ( 35.00000000000000000, -4.725891942574827809, -10.75351884295726101 ) ) ;
#10699 = CARTESIAN_POINT ( 'NONE',  ( 35.00000000000000000, 0.1652884326465054732, -12.18537902504609427 ) ) ;
#10700 = CARTESIAN_POINT ( 'NONE',  ( 1.000000000000000888, 7.387287142779352500, 1.295372019972176103 ) ) ;
#10702 = ORIENTED_EDGE ( 'NONE', *, *, #46129, .T. ) ;
#10701 = CARTESIAN_POINT ( 'NONE',  ( -17.50079231878650177, 2.685795310841043282, -13.23113775294028649 ) ) ;
#10703 = CARTESIAN_POINT ( 'NONE',  ( -25.00000000000000355, -9.999999999999998224, -25.00000000000000000 ) ) ;
#10704 = VERTEX_POINT ( 'NONE', #16387 ) ;
#10705 = CYLINDRICAL_SURFACE ( 'NONE', #63517, 12.18650000000000055 ) ;
#10706 = CARTESIAN_POINT ( 'NONE',  ( 2.994568964204217920, -5.775954174106896488, -5.368337437440318105 ) ) ;
#10707 = AXIS2_PLACEMENT_3D ( 'NONE', #58039, #32727, #48067 ) ;
#10708 = ORIENTED_EDGE ( 'NONE', *, *, #24455, .F. ) ;
#10709 = EDGE_CURVE ( 'NONE', #54583, #15438, #51965, .T. ) ;
#10710 = CYLINDRICAL_SURFACE ( 'NONE', #28575, 5.000000000000000888 ) ;
#10711 = CARTESIAN_POINT ( 'NONE',  ( 5.520433897694421610, 0.007971295965052416221, -0.01278034823631966389 ) ) ;
#10712 = CARTESIAN_POINT ( 'NONE',  ( -27.10719052120871098, -2.261993590776032459, 0.6736837626858792616 ) ) ;
#10713 = CARTESIAN_POINT ( 'NONE',  ( -35.04582288351658548, 0.01107592729722563576, 0.006225574250530754340 ) ) ;
#10714 = CARTESIAN_POINT ( 'NONE',  ( 5.514970785353741078, -0.002093325033903842454, 0.004233694591582945477 ) ) ;
#10715 = AXIS2_PLACEMENT_3D ( 'NONE', #36754, #12131, #1533 ) ;
#10716 = AXIS2_PLACEMENT_3D ( 'NONE', #48133, #33479, #6581 ) ;
#10717 = AXIS2_PLACEMENT_3D ( 'NONE', #21490, #42383, #12152 ) ;
#10718 = ADVANCED_FACE ( 'NONE', ( #762 ), #26681, .T. ) ;
#10719 = EDGE_LOOP ( 'NONE', ( #14831, #12509, #12085, #51539, #30525, #48290 ) ) ;
#10720 = CARTESIAN_POINT ( 'NONE',  ( -19.32000128823278118, -3.826633625541849160, -11.37379849559869527 ) ) ;
#10721 = AXIS2_PLACEMENT_3D ( 'NONE', #39083, #49099, #44389 ) ;
#10722 = ORIENTED_EDGE ( 'NONE', *, *, #27939, .F. ) ;
#10723 = CARTESIAN_POINT ( 'NONE',  ( 2.969415267403874292, 0.3878973768015938628, 7.867532449842894238 ) ) ;
#10724 = DIRECTION ( 'NONE',  ( 1.000000000000000000, 0.000000000000000000, 0.000000000000000000 ) ) ;
#10725 = CARTESIAN_POINT ( 'NONE',  ( -2.952869152607111136, 4.384817011589738911, 11.17020052527586138 ) ) ;
#10726 = EDGE_CURVE ( 'NONE', #50602, #37599, #22868, .T. ) ;
#10727 = ORIENTED_EDGE ( 'NONE', *, *, #59806, .T. ) ;
#10728 = DIRECTION ( 'NONE',  ( -1.000000000000000000, 0.000000000000000000, 0.000000000000000000 ) ) ;
#10729 = AXIS2_PLACEMENT_3D ( 'NONE', #60754, #49795, #50464 ) ;
#10730 = CIRCLE ( 'NONE', #22410, 12.18649999999999878 ) ;
#10731 = AXIS2_PLACEMENT_3D ( 'NONE', #22388, #32365, #27376 ) ;
#10732 = CARTESIAN_POINT ( 'NONE',  ( 28.33327753883506261, 12.08535766013368473, 6.028296700677072906 ) ) ;
#10733 = CARTESIAN_POINT ( 'NONE',  ( -29.68541646480307250, -2.179156473586586262, 11.82547580031049606 ) ) ;
#10734 = AXIS2_PLACEMENT_3D ( 'NONE', #7489, #2191, #61462 ) ;
#10735 = DIRECTION ( 'NONE',  ( 0.000000000000000000, 0.000000000000000000, 1.000000000000000000 ) ) ;
#10736 = DIRECTION ( 'NONE',  ( 0.9606638835031802159, 0.2535400141108153371, 0.1133241553124300777 ) ) ;
#10737 = DIRECTION ( 'NONE',  ( -1.000000000000000000, 0.000000000000000000, 0.000000000000000000 ) ) ;
#10738 = CARTESIAN_POINT ( 'NONE',  ( 37.00000000000000711, 4.705694406421931860E-17, -3.469127814946512892E-15 ) ) ;
#10739 = CARTESIAN_POINT ( 'NONE',  ( 0.6511581176968128659, -3.919972364658588670, -11.73752429815142229 ) ) ;
#10740 = AXIS2_PLACEMENT_3D ( 'NONE', #46146, #10878, #36803 ) ;
#10741 = EDGE_CURVE ( 'NONE', #32235, #49156, #48374, .T. ) ;
#10742 = EDGE_CURVE ( 'NONE', #47877, #30464, #36970, .T. ) ;
#10743 = CARTESIAN_POINT ( 'NONE',  ( -37.25000000000000711, -20.00000000000000000, -1.499999999999998002 ) ) ;
#10744 = FACE_OUTER_BOUND ( 'NONE', #41589, .T. ) ;
#10745 = CIRCLE ( 'NONE', #27740, 5.000000000000000888 ) ;
#10746 = ORIENTED_EDGE ( 'NONE', *, *, #63625, .T. ) ;
#10747 = DIRECTION ( 'NONE',  ( -0.3939253465568943735, -0.3234796780324251109, -0.8603393047164992202 ) ) ;
#10748 = DIRECTION ( 'NONE',  ( 0.000000000000000000, 0.9651210252299803338, 0.2618041379715598249 ) ) ;
#10749 = CARTESIAN_POINT ( 'NONE',  ( -22.27710395300133683, 3.562137928983405644, -0.9291085174899351706 ) ) ;
#10750 = ORIENTED_EDGE ( 'NONE', *, *, #51177, .T. ) ;
#10751 = EDGE_CURVE ( 'NONE', #27227, #61808, #12264, .T. ) ;
#10752 = DIRECTION ( 'NONE',  ( 0.000000000000000000, -0.01356324068817999114, 0.9999080150203989437 ) ) ;
#10753 = ORIENTED_EDGE ( 'NONE', *, *, #64156, .T. ) ;
#10754 = EDGE_LOOP ( 'NONE', ( #1720, #1426, #29249, #23632 ) ) ;
#10755 = VERTEX_POINT ( 'NONE', #11698 ) ;
#10756 = CIRCLE ( 'NONE', #31975, 2.899999999999995026 ) ;
#10757 = LINE ( 'NONE', #5808, #32695 ) ;
#10758 = AXIS2_PLACEMENT_3D ( 'NONE', #26358, #1097, #21373 ) ;
#10759 = AXIS2_PLACEMENT_3D ( 'NONE', #41739, #56739, #32405 ) ;
#10760 = ORIENTED_EDGE ( 'NONE', *, *, #44969, .F. ) ;
#10761 = FACE_OUTER_BOUND ( 'NONE', #61238, .T. ) ;
#10762 = CARTESIAN_POINT ( 'NONE',  ( -22.27878402819508352, -3.558531829368155375, 0.9624056734348110931 ) ) ;
#10763 = DIRECTION ( 'NONE',  ( -0.3939253465568944290, -0.4679616473074788563, -0.7910971609033250473 ) ) ;
#10764 = DIRECTION ( 'NONE',  ( 1.000000000000000000, 0.000000000000000000, 0.000000000000000000 ) ) ;
#10765 = ORIENTED_EDGE ( 'NONE', *, *, #64422, .T. ) ;
#10766 = CARTESIAN_POINT ( 'NONE',  ( -35.00000000000000000, -9.752226076388847531, -6.547236723514122225 ) ) ;
#10767 = CARTESIAN_POINT ( 'NONE',  ( -12.50548042261300097, -29.27747730776768975, 5.013933227252732827 ) ) ;
#10768 = CARTESIAN_POINT ( 'NONE',  ( 35.00000000000000000, 0.8294751490779324055, -12.15823808070322798 ) ) ;
#10770 = ORIENTED_EDGE ( 'NONE', *, *, #31666, .T. ) ;
#10769 = CARTESIAN_POINT ( 'NONE',  ( 35.00000000000000000, 4.705694406421931860E-17, -3.469127814946512892E-15 ) ) ;
#10771 = CARTESIAN_POINT ( 'NONE',  ( 5.516018279890452902, 0.001397286410094317416, -0.006629829924290979969 ) ) ;
#10772 = ORIENTED_EDGE ( 'NONE', *, *, #6293, .T. ) ;
#10773 = CARTESIAN_POINT ( 'NONE',  ( -27.35552965826136429, -2.810569013793742688, 1.320216934008381804 ) ) ;
#10774 = ORIENTED_EDGE ( 'NONE', *, *, #45243, .T. ) ;
#10775 = ORIENTED_EDGE ( 'NONE', *, *, #2370, .T. ) ;
#10776 = B_SPLINE_CURVE_WITH_KNOTS ( 'NONE', 3,
 ( #5750, #61564, #65566, #15371, #50637, #20036, #5083, #25345, #40301, #20695, #26016, #35314, #15678, #30646, #50958, #65261 ),
 .UNSPECIFIED., .F., .F.,
 ( 4, 3, 3, 3, 3, 4 ),
 ( 0.000000000000000000, 6.991367980366403740E-05, 0.0001398269368981361522, 0.0002097400188389093899, 0.0002811534801551363776, 0.0003526297678872490952 ),
 .UNSPECIFIED. ) ;
#10777 = DIRECTION ( 'NONE',  ( -1.000000000000000000, 0.000000000000000000, 0.000000000000000000 ) ) ;
#10778 = AXIS2_PLACEMENT_3D ( 'NONE', #10448, #21428, #26097 ) ;
#10779 = CARTESIAN_POINT ( 'NONE',  ( 13.26995653566893019, -33.36016745060648958, 10.56634385159335388 ) ) ;
#10780 = DIRECTION ( 'NONE',  ( -1.000000000000000000, -0.000000000000000000, -0.000000000000000000 ) ) ;
#10781 = AXIS2_PLACEMENT_3D ( 'NONE', #16323, #6033, #1697 ) ;
#10783 = ADVANCED_FACE ( 'NONE', ( #36326 ), #31980, .T. ) ;
#10782 = EDGE_LOOP ( 'NONE', ( #21133, #52625, #46600, #36797 ) ) ;
#10784 = DIRECTION ( 'NONE',  ( 0.000000000000000000, -0.01356324068817998940, 0.9999080150203990547 ) ) ;
#10785 = FACE_OUTER_BOUND ( 'NONE', #36261, .T. ) ;
#10786 = CARTESIAN_POINT ( 'NONE',  ( 0.2739690278137256185, -12.02985305092652268, 2.307031017960411656 ) ) ;
#10787 = ORIENTED_EDGE ( 'NONE', *, *, #41177, .T. ) ;
#10788 = EDGE_CURVE ( 'NONE', #15077, #10081, #1659, .T. ) ;
#10789 = VERTEX_POINT ( 'NONE', #21711 ) ;
#10790 = DIRECTION ( 'NONE',  ( 0.000000000000000000, 0.01356324068817998940, -0.9999080150203990547 ) ) ;
#10791 = EDGE_LOOP ( 'NONE', ( #61445, #55190, #19663, #59478 ) ) ;
#10792 = VERTEX_POINT ( 'NONE', #52627 ) ;
#10793 = AXIS2_PLACEMENT_3D ( 'NONE', #62317, #62011, #61336 ) ;
#10794 = EDGE_CURVE ( 'NONE', #44565, #32207, #52173, .T. ) ;
#10795 = FACE_OUTER_BOUND ( 'NONE', #32513, .T. ) ;
#10796 = CYLINDRICAL_SURFACE ( 'NONE', #22399, 12.18649999999999878 ) ;
#10797 = CARTESIAN_POINT ( 'NONE',  ( 18.62706029620522941, 2.680501531300553797, 11.70880161399673902 ) ) ;
#10798 = DIRECTION ( 'NONE',  ( -1.000000000000000000, 0.000000000000000000, 0.000000000000000000 ) ) ;
#10799 = FACE_OUTER_BOUND ( 'NONE', #6958, .T. ) ;
#10800 = DIRECTION ( 'NONE',  ( 0.000000000000000000, 0.01356324068817991828, -0.9999080150203990547 ) ) ;
#10801 = VECTOR ( 'NONE', #14138, 1000.000000000000000 ) ;
#10802 = EDGE_LOOP ( 'NONE', ( #58935, #24867, #1545, #1034 ) ) ;
#10803 = FACE_OUTER_BOUND ( 'NONE', #349, .T. ) ;
#10804 = EDGE_CURVE ( 'NONE', #32432, #15657, #36380, .T. ) ;
#10805 = LINE ( 'NONE', #31422, #31879 ) ;
#10806 = CARTESIAN_POINT ( 'NONE',  ( -35.04709527796842394, -0.01117341439755767385, 0.005292201869320362073 ) ) ;
#10807 = EDGE_CURVE ( 'NONE', #29673, #60341, #8054, .T. ) ;
#10808 = AXIS2_PLACEMENT_3D ( 'NONE', #52493, #6927, #32815 ) ;
#10809 = CIRCLE ( 'NONE', #3397, 24.00000000000000000 ) ;
#10810 = CARTESIAN_POINT ( 'NONE',  ( 2.000000000000001776, 0.2704997240206042930, -6.931223712253475000 ) ) ;
#10811 = VECTOR ( 'NONE', #5119, 1000.000000000000000 ) ;
#10812 = CARTESIAN_POINT ( 'NONE',  ( -22.38932658256920760, 2.201197575855971866, 3.361598243548623799 ) ) ;
#10813 = CARTESIAN_POINT ( 'NONE',  ( 22.86325106016951736, 2.804889020532796096, -13.20736364802678509 ) ) ;
#10814 = DIRECTION ( 'NONE',  ( -1.000000000000000000, 0.000000000000000000, 0.000000000000000000 ) ) ;
#10815 = CARTESIAN_POINT ( 'NONE',  ( -19.69476066079020171, -4.201994156881551312, 25.00000000000000000 ) ) ;
#10816 = ORIENTED_EDGE ( 'NONE', *, *, #55768, .T. ) ;
#10817 = CARTESIAN_POINT ( 'NONE',  ( -36.00000000000000711, -11.96656215839366055, -4.400442035671074059 ) ) ;
#10818 = CARTESIAN_POINT ( 'NONE',  ( 2.305787727787084407, 1.164987321564833422, -7.566723232958059597 ) ) ;
#10819 = DIRECTION ( 'NONE',  ( 0.000000000000000000, 0.000000000000000000, 1.000000000000000000 ) ) ;
#10820 = AXIS2_PLACEMENT_3D ( 'NONE', #59297, #34974, #24704 ) ;
#10821 = EDGE_CURVE ( 'NONE', #54202, #4686, #10133, .T. ) ;
#10822 = VECTOR ( 'NONE', #2262, 1000.000000000000000 ) ;
#10823 = AXIS2_PLACEMENT_3D ( 'NONE', #19753, #40010, #14720 ) ;
#10824 = EDGE_CURVE ( 'NONE', #30241, #44540, #18655, .T. ) ;
#10825 = CARTESIAN_POINT ( 'NONE',  ( -26.91319780901507386, 10.55334688052688819, 5.712466060832438686 ) ) ;
#10826 = CARTESIAN_POINT ( 'NONE',  ( 26.08439714455133185, 11.40113243194252846, 3.743551691817327942 ) ) ;
#10827 = ORIENTED_EDGE ( 'NONE', *, *, #8636, .F. ) ;
#10828 = CARTESIAN_POINT ( 'NONE',  ( -17.14251155165674234, -7.213546477669500412, -11.41604601608509562 ) ) ;
#10829 = CARTESIAN_POINT ( 'NONE',  ( 11.74548640120467979, 25.00000000000000000, -8.184666801472349817 ) ) ;
#10830 = AXIS2_PLACEMENT_3D ( 'NONE', #31947, #52268, #37614 ) ;
#10831 = CARTESIAN_POINT ( 'NONE',  ( 16.03117610287102579, -28.25087052915268870, -10.32844618003480619 ) ) ;
#10832 = VERTEX_POINT ( 'NONE', #8700 ) ;
#10833 = ADVANCED_FACE ( 'NONE', ( #43947 ), #31400, .F. ) ;
#10834 = DIRECTION ( 'NONE',  ( 0.000000000000000000, -1.000000000000000000, 0.000000000000000000 ) ) ;
#10835 = CARTESIAN_POINT ( 'NONE',  ( 5.514970785353741078, 0.003929719953530106356, -0.002619824551223718344 ) ) ;
#10836 = CYLINDRICAL_SURFACE ( 'NONE', #41504, 12.75000000000000178 ) ;
#10837 = AXIS2_PLACEMENT_3D ( 'NONE', #46315, #10079, #11375 ) ;
#10839 = ORIENTED_EDGE ( 'NONE', *, *, #13510, .T. ) ;
#10838 = CARTESIAN_POINT ( 'NONE',  ( 2.835339799623980639, 1.035140033450052011, 7.763739326985116485 ) ) ;
#10840 = DIRECTION ( 'NONE',  ( 0.9688695217174486674, 0.000000000000000000, 0.2475719085175097645 ) ) ;
#10841 = CARTESIAN_POINT ( 'NONE',  ( -35.00000000000000000, -8.927548052240956267, 8.295159312811819063 ) ) ;
#10842 = VERTEX_POINT ( 'NONE', #13352 ) ;
#10843 = DIRECTION ( 'NONE',  ( -0.9015184547431841500, -0.4327406564646559262, 0.000000000000000000 ) ) ;
#10844 = AXIS2_PLACEMENT_3D ( 'NONE', #38438, #53749, #18822 ) ;
#10845 = CARTESIAN_POINT ( 'NONE',  ( -47.00000000000000711, 0.000000000000000000, 0.000000000000000000 ) ) ;
#10846 = CARTESIAN_POINT ( 'NONE',  ( 0.2651627682582891055, -7.803986935114077816, 9.437482589529949450 ) ) ;
#10847 = CARTESIAN_POINT ( 'NONE',  ( 0.5572780756289471560, -1.841882550626719794, -12.20533540249727800 ) ) ;
#10848 = CARTESIAN_POINT ( 'NONE',  ( -9.552061971074056856, 9.047766850818582895, -7.885493295094908817 ) ) ;
#10849 = DIRECTION ( 'NONE',  ( 0.1034490876700550344, -0.000000000000000000, 0.9946347501772866417 ) ) ;
#10851 = ORIENTED_EDGE ( 'NONE', *, *, #46528, .F. ) ;
#10850 = DIRECTION ( 'NONE',  ( 0.000000000000000000, -0.8169148498130213154, 0.5767582926625057782 ) ) ;
#10852 = ORIENTED_EDGE ( 'NONE', *, *, #1281, .T. ) ;
#10853 = CARTESIAN_POINT ( 'NONE',  ( 3.152665057734121756, -0.4801242025592447060, 7.923639299008720549 ) ) ;
#10854 = ORIENTED_EDGE ( 'NONE', *, *, #30627, .F. ) ;
#10855 = AXIS2_PLACEMENT_3D ( 'NONE', #62056, #11497, #32428 ) ;
#10856 = DIRECTION ( 'NONE',  ( -0.7256567719371089797, -2.743705601699970915E-17, -0.6880568649042131391 ) ) ;
#10857 = DIRECTION ( 'NONE',  ( 0.000000000000000000, 0.000000000000000000, 1.000000000000000000 ) ) ;
#10859 = CARTESIAN_POINT ( 'NONE',  ( 0.2833330754217355252, 11.44258640049861242, 4.379886056890929247 ) ) ;
#10858 = CIRCLE ( 'NONE', #60801, 5.000000000000000000 ) ;
#10860 = AXIS2_PLACEMENT_3D ( 'NONE', #55465, #276, #34522 ) ;
#10861 = CARTESIAN_POINT ( 'NONE',  ( -10.00000000000000178, 0.000000000000000000, 0.000000000000000000 ) ) ;
#10862 = ORIENTED_EDGE ( 'NONE', *, *, #55900, .T. ) ;
#10863 = DIRECTION ( 'NONE',  ( 0.000000000000000000, -0.8835120444460178302, -0.4684084406997996441 ) ) ;
#10864 = ADVANCED_FACE ( 'NONE', ( #53928 ), #63301, .F. ) ;
#10865 =( BOUNDED_SURFACE ( )  B_SPLINE_SURFACE ( 3, 1, ( 
 ( #1082, #2667 ),
 ( #36651, #58502 ),
 ( #10713, #57266 ),
 ( #21353, #6399 ) ),
 .UNSPECIFIED., .F., .F., .F. ) 
 B_SPLINE_SURFACE_WITH_KNOTS ( ( 4, 4 ),
 ( 2, 2 ),
 ( 0.000000000000000000, 1.000000000000000000 ),
 ( 0.000000000000000000, 1.000000000000000000 ),
 .UNSPECIFIED. ) 
 GEOMETRIC_REPRESENTATION_ITEM ( )  RATIONAL_B_SPLINE_SURFACE ( (
 ( 1.000000000000000000, 1.000000000000000000),
 ( 0.9257577194822556033, 0.9980522942447415113),
 ( 0.9257577194822556033, 0.9980522942447415113),
 ( 1.000000000000000000, 1.000000000000000000) ) ) 
 REPRESENTATION_ITEM ( '' )  SURFACE ( )  );
#10866 = CARTESIAN_POINT ( 'NONE',  ( 5.514970785353741078, -0.004588761610584819045, -0.001117786416802158496 ) ) ;
#10867 = CARTESIAN_POINT ( 'NONE',  ( -22.27711653538342773, -1.465933162149059665, 3.377206745424981449 ) ) ;
#10868 = VERTEX_POINT ( 'NONE', #3070 ) ;
#10869 = EDGE_LOOP ( 'NONE', ( #44542, #21197, #50305, #36012 ) ) ;
#10870 = CARTESIAN_POINT ( 'NONE',  ( 2.000000000000001776, -5.457833520448679643, 4.281014542496493824 ) ) ;
#10871 = ORIENTED_EDGE ( 'NONE', *, *, #47635, .T. ) ;
#10872 = CYLINDRICAL_SURFACE ( 'NONE', #59300, 2.899999999999994582 ) ;
#10873 = CARTESIAN_POINT ( 'NONE',  ( -27.08429572838383947, 0.6096735944848206135, -2.208905845566032866 ) ) ;
#10874 = AXIS2_PLACEMENT_3D ( 'NONE', #37519, #52512, #2284 ) ;
#10875 = CARTESIAN_POINT ( 'NONE',  ( -36.00000000000000711, -4.561791185930499815, 11.90598845858532329 ) ) ;
#10876 = CARTESIAN_POINT ( 'NONE',  ( -29.68541646480307250, -1.416020129149132334, 11.91616074890920451 ) ) ;
#10877 = CIRCLE ( 'NONE', #51253, 2.899999999999995914 ) ;
#10879 = EDGE_CURVE ( 'NONE', #51547, #22753, #50494, .T. ) ;
#10878 = DIRECTION ( 'NONE',  ( -1.000000000000000000, 0.000000000000000000, 0.000000000000000000 ) ) ;
#10880 = DIRECTION ( 'NONE',  ( -1.000000000000000000, 0.000000000000000000, 0.000000000000000000 ) ) ;
#10881 = DIRECTION ( 'NONE',  ( -1.000000000000000000, 0.000000000000000000, 0.000000000000000000 ) ) ;
#10882 = ORIENTED_EDGE ( 'NONE', *, *, #14239, .F. ) ;
#10883 = CARTESIAN_POINT ( 'NONE',  ( 1.283627346226323240, 12.57362488724964145, -0.5505361391623029288 ) ) ;
#10884 = CIRCLE ( 'NONE', #21530, 6.000000000000000888 ) ;
#10885 = FACE_OUTER_BOUND ( 'NONE', #29259, .T. ) ;
#10886 = EDGE_CURVE ( 'NONE', #16429, #64737, #30302, .T. ) ;
#10887 = CARTESIAN_POINT ( 'NONE',  ( 0.9232058338315048962, -10.60677148422239924, -6.559496812049772529 ) ) ;
#10888 = CARTESIAN_POINT ( 'NONE',  ( -9.317739297035824819, 10.04120852590977186, -6.581867252412223479 ) ) ;
#10889 = CARTESIAN_POINT ( 'NONE',  ( -37.00000000000000711, 0.000000000000000000, 0.000000000000000000 ) ) ;
#10890 = FACE_OUTER_BOUND ( 'NONE', #25396, .T. ) ;
#10891 = CARTESIAN_POINT ( 'NONE',  ( 17.27839441901508621, 10.52068335315811076, 5.771933972472480967 ) ) ;
#10892 = CARTESIAN_POINT ( 'NONE',  ( -42.50000000000000000, -2.710505431213761085E-17, 1.399999999999999911 ) ) ;
#10893 = EDGE_CURVE ( 'NONE', #37431, #2532, #33061, .T. ) ;
#10894 = ORIENTED_EDGE ( 'NONE', *, *, #13397, .F. ) ;
#10895 = ORIENTED_EDGE ( 'NONE', *, *, #33665, .F. ) ;
#10896 = DIRECTION ( 'NONE',  ( 0.000000000000000000, 0.9246979985058736418, 0.3807014730195186214 ) ) ;
#10897 = AXIS2_PLACEMENT_3D ( 'NONE', #53175, #2665, #7623 ) ;
#10898 = ORIENTED_EDGE ( 'NONE', *, *, #56497, .T. ) ;
#10899 = CYLINDRICAL_SURFACE ( 'NONE', #55292, 4.000030059823568074 ) ;
#10900 = CARTESIAN_POINT ( 'NONE',  ( 2.000000000000001776, -1.058508696395003890, 6.730038252034888480 ) ) ;
#10901 = LINE ( 'NONE', #57786, #35214 ) ;
#10902 = FACE_OUTER_BOUND ( 'NONE', #18474, .T. ) ;
#10903 = ORIENTED_EDGE ( 'NONE', *, *, #21371, .T. ) ;
#10904 = AXIS2_PLACEMENT_3D ( 'NONE', #64624, #50017, #40686 ) ;
#10905 = CARTESIAN_POINT ( 'NONE',  ( -10.95212338237647920, -9.902220863987562183, -9.175839033069911110 ) ) ;
#10906 = CARTESIAN_POINT ( 'NONE',  ( 37.00000000000000711, 4.705694406421931860E-17, -3.469127814946512892E-15 ) ) ;
#10907 = CIRCLE ( 'NONE', #19421, 12.18650000000000055 ) ;
#10908 = DIRECTION ( 'NONE',  ( 1.000000000000000000, 0.000000000000000000, 0.000000000000000000 ) ) ;
#10909 = CARTESIAN_POINT ( 'NONE',  ( -22.28169757117799321, 2.633129923220830282, 2.592369810060362934 ) ) ;
#10910 = EDGE_CURVE ( 'NONE', #35534, #64984, #54899, .T. ) ;
#10911 = CIRCLE ( 'NONE', #11950, 12.74999999999999822 ) ;
#10912 = VECTOR ( 'NONE', #64244, 1000.000000000000000 ) ;
#10913 = CARTESIAN_POINT ( 'NONE',  ( 0.9232058338315048962, 12.46548196349786153, 0.3773051331668418329 ) ) ;
#10914 = DIRECTION ( 'NONE',  ( -0.000000000000000000, -0.000000000000000000, -1.000000000000000000 ) ) ;
#10915 = ORIENTED_EDGE ( 'NONE', *, *, #13824, .T. ) ;
#10916 = LINE ( 'NONE', #56469, #47718 ) ;
#10917 = EDGE_LOOP ( 'NONE', ( #19690, #60843, #19941, #4006 ) ) ;
#10918 = CARTESIAN_POINT ( 'NONE',  ( 35.00000000000000000, 4.705694406421931860E-17, -3.469127814946512892E-15 ) ) ;
#10919 = DIRECTION ( 'NONE',  ( 0.000000000000000000, -0.2618041379715704275, 0.9651210252299774472 ) ) ;
#10920 = VECTOR ( 'NONE', #5183, 1000.000000000000000 ) ;
#10921 = CARTESIAN_POINT ( 'NONE',  ( -22.27384469013075829, -3.564715702084494175, 0.9224151068931482067 ) ) ;
#10922 = CARTESIAN_POINT ( 'NONE',  ( 0.3401186441510284375, -11.61600526280573220, 3.955862996551460231 ) ) ;
#10923 = ADVANCED_FACE ( 'NONE', ( #5350 ), #29948, .T. ) ;
#10924 = CIRCLE ( 'NONE', #57648, 4.999999999999998224 ) ;
#10925 = VERTEX_POINT ( 'NONE', #61200 ) ;
#10926 = ORIENTED_EDGE ( 'NONE', *, *, #50048, .F. ) ;
#10927 = DIRECTION ( 'NONE',  ( 0.000000000000000000, 0.000000000000000000, 1.000000000000000000 ) ) ;
#10928 = VERTEX_POINT ( 'NONE', #40584 ) ;
#10929 = CARTESIAN_POINT ( 'NONE',  ( 2.290907136833248980, -6.543263131934267562, -3.965134647955961711 ) ) ;
#10930 = CARTESIAN_POINT ( 'NONE',  ( -37.00000000000000711, 11.68758509253248334, -1.171570255487489609 ) ) ;
#10931 = DIRECTION ( 'NONE',  ( -1.000000000000000000, -0.000000000000000000, -0.000000000000000000 ) ) ;
#10932 = DIRECTION ( 'NONE',  ( 0.000000000000000000, 0.000000000000000000, 1.000000000000000000 ) ) ;
#10933 = CARTESIAN_POINT ( 'NONE',  ( 22.78397477906666069, 3.290341966830223175, 11.54089583822153031 ) ) ;
#10934 = B_SPLINE_CURVE_WITH_KNOTS ( 'NONE', 3,
 ( #52433, #6871, #42741, #27142, #17160, #12480, #37437, #57748, #12167, #37772, #58066, #8487, #48743, #28771, #58388, #3860, #54719, #63354, #38759, #8168 ),
 .UNSPECIFIED., .F., .F.,
 ( 4, 2, 2, 2, 2, 2, 2, 2, 2, 4 ),
 ( 4.249187360970369464E-18, 0.001349386060196310121, 0.002024079090294461820, 0.002698772120392613737, 0.004048158180588917569, 0.004722851210687068618, 0.005397544240785222269, 0.006746930300981533908, 0.008096316361177842078, 0.01079508848157046189 ),
 .UNSPECIFIED. ) ;
#10935 = VECTOR ( 'NONE', #42411, 1000.000000000000000 ) ;
#10936 = DIRECTION ( 'NONE',  ( 0.000000000000000000, 0.000000000000000000, -1.000000000000000000 ) ) ;
#10937 = CARTESIAN_POINT ( 'NONE',  ( 1.634816307079405506, 12.61459884933078435, -1.494046826340906575 ) ) ;
#10938 = ORIENTED_EDGE ( 'NONE', *, *, #3982, .F. ) ;
#10939 = CARTESIAN_POINT ( 'NONE',  ( 1.549075743845170772, -11.29795072957498547, 5.743768701986912362 ) ) ;
#10940 = EDGE_LOOP ( 'NONE', ( #30979, #5430, #7222, #60646 ) ) ;
#10941 = LINE ( 'NONE', #31858, #38703 ) ;
#10942 = FACE_OUTER_BOUND ( 'NONE', #20676, .T. ) ;
#10943 = VECTOR ( 'NONE', #39984, 1000.000000000000000 ) ;
#10944 = B_SPLINE_CURVE_WITH_KNOTS ( 'NONE', 3,
 ( #25456, #30123, #36421, #35430, #35081, #26439, #46723 ),
 .UNSPECIFIED., .F., .F.,
 ( 4, 3, 4 ),
 ( 1.191827804620218263E-14, 0.002398160485435229215, 0.005002426799390250096 ),
 .UNSPECIFIED. ) ;
#10945 = ORIENTED_EDGE ( 'NONE', *, *, #18101, .F. ) ;
#10946 = CARTESIAN_POINT ( 'NONE',  ( -22.27716857039623477, 3.591587580808003555, -0.8090275962000442744 ) ) ;
#10947 = ORIENTED_EDGE ( 'NONE', *, *, #1512, .F. ) ;
#10948 = LINE ( 'NONE', #4676, #48241 ) ;
#10949 = EDGE_CURVE ( 'NONE', #6328, #14103, #65554, .T. ) ;
#10950 = DIRECTION ( 'NONE',  ( 0.000000000000000000, 0.000000000000000000, 1.000000000000000000 ) ) ;
#10951 = CARTESIAN_POINT ( 'NONE',  ( 3.092491956585685653, 3.124176487320323936, 7.275786042219381855 ) ) ;
#10952 = CARTESIAN_POINT ( 'NONE',  ( -45.77110135055801265, -0.8256172497425255941, 12.04909734191307003 ) ) ;
#10953 = ORIENTED_EDGE ( 'NONE', *, *, #45563, .F. ) ;
#10954 = ORIENTED_EDGE ( 'NONE', *, *, #19020, .T. ) ;
#10955 = CARTESIAN_POINT ( 'NONE',  ( 2.061095049060549744, 2.059564177347529945, 13.34611721626114189 ) ) ;
#10956 = EDGE_CURVE ( 'NONE', #14997, #16004, #29609, .T. ) ;
#10957 = VERTEX_POINT ( 'NONE', #59903 ) ;
#10958 = CARTESIAN_POINT ( 'NONE',  ( 2.000000000000001776, -6.796153407501448029, 1.388283512725787761 ) ) ;
#10959 = VERTEX_POINT ( 'NONE', #65507 ) ;
#10960 = VECTOR ( 'NONE', #29116, 1000.000000000000000 ) ;
#10961 = ORIENTED_EDGE ( 'NONE', *, *, #9737, .T. ) ;
#10962 = EDGE_LOOP ( 'NONE', ( #56045, #55764, #16608, #48414 ) ) ;
#10963 = CARTESIAN_POINT ( 'NONE',  ( 6.812204945636112896, -4.138731716409435712, -11.26369831714194092 ) ) ;
#10964 = CARTESIAN_POINT ( 'NONE',  ( 1.109979610368935665, 11.59954799439076112, 4.732439402373389115 ) ) ;
#10965 = AXIS2_PLACEMENT_3D ( 'NONE', #49611, #14646, #59920 ) ;
#10966 = AXIS2_PLACEMENT_3D ( 'NONE', #21226, #42471, #51837 ) ;
#10967 = CARTESIAN_POINT ( 'NONE',  ( 2.507146904658099640, -1.127530020444445613, -7.640248566386912188 ) ) ;
#10969 = ADVANCED_FACE ( 'NONE', ( #50256 ), #34605, .T. ) ;
#10968 = CARTESIAN_POINT ( 'NONE',  ( 1.937114397841932290, 5.620553190832977108, 11.53912442307257358 ) ) ;
#10970 = DIRECTION ( 'NONE',  ( 0.000000000000000000, 0.8009703041134188517, 0.5987040770935649903 ) ) ;
#10971 = ORIENTED_EDGE ( 'NONE', *, *, #9835, .F. ) ;
#10972 = DIRECTION ( 'NONE',  ( 1.000000000000000000, 0.000000000000000000, 0.000000000000000000 ) ) ;
#10973 = ORIENTED_EDGE ( 'NONE', *, *, #48425, .F. ) ;
#10974 = DIRECTION ( 'NONE',  ( 0.000000000000000000, 0.6051742151937661296, -0.7960930657056429771 ) ) ;
#10976 = CARTESIAN_POINT ( 'NONE',  ( -2.532614230583023041, 12.88560382747354005, 4.026315189028235153 ) ) ;
#10975 = VECTOR ( 'NONE', #27644, 1000.000000000000000 ) ;
#10977 = CARTESIAN_POINT ( 'NONE',  ( 35.00000000000000000, 12.18359334611896116, 0.2661492558803733588 ) ) ;
#10978 = EDGE_CURVE ( 'NONE', #64767, #52558, #39421, .T. ) ;
#10979 = CARTESIAN_POINT ( 'NONE',  ( 0.2739690278137251744, -8.012873994335626193, -9.264642836915912838 ) ) ;
#10980 = AXIS2_PLACEMENT_3D ( 'NONE', #31281, #21639, #57210 ) ;
#10981 = CARTESIAN_POINT ( 'NONE',  ( 5.516018279890452902, 0.006440244342253413461, -0.002104829434641034870 ) ) ;
#10982 = CARTESIAN_POINT ( 'NONE',  ( 2.994568964204210815, -7.875338388187470784, -0.3996732855055539768 ) ) ;
#10983 = AXIS2_PLACEMENT_3D ( 'NONE', #45431, #45769, #54459 ) ;
#10984 = ORIENTED_EDGE ( 'NONE', *, *, #17187, .F. ) ;
#10985 = FACE_OUTER_BOUND ( 'NONE', #35332, .T. ) ;
#10986 = AXIS2_PLACEMENT_3D ( 'NONE', #49331, #64896, #50617 ) ;
#10987 = VERTEX_POINT ( 'NONE', #57534 ) ;
#10988 = DIRECTION ( 'NONE',  ( 0.000000000000000000, 0.000000000000000000, 1.000000000000000000 ) ) ;
#10989 = DIRECTION ( 'NONE',  ( 0.000000000000000000, -0.7196168960969719919, -0.6943713148249717193 ) ) ;
#10990 = CIRCLE ( 'NONE', #65127, 5.000000000000000000 ) ;
#10991 = CARTESIAN_POINT ( 'NONE',  ( 7.002886717044668252, -27.11012757947471741, 15.35900505431296281 ) ) ;
#10992 = DIRECTION ( 'NONE',  ( -1.000000000000000000, 0.000000000000000000, 0.000000000000000000 ) ) ;
#10993 = CARTESIAN_POINT ( 'NONE',  ( 2.241352910868908754, 7.532448145350508995, 1.243507963608119438 ) ) ;
#10994 = ORIENTED_EDGE ( 'NONE', *, *, #23326, .T. ) ;
#10995 = DIRECTION ( 'NONE',  ( 0.000000000000000000, -0.01356324068817992175, 0.9999080150203990547 ) ) ;
#10996 = CARTESIAN_POINT ( 'NONE',  ( 0.2676618633000454328, 2.284744117040236500, -12.03196378632208763 ) ) ;
#10997 = CYLINDRICAL_SURFACE ( 'NONE', #10980, 2.899999999999994582 ) ;
#10998 = AXIS2_PLACEMENT_3D ( 'NONE', #32196, #2294, #11594 ) ;
#10999 = CARTESIAN_POINT ( 'NONE',  ( 0.2872850955227737590, 12.25172867346923233, -0.2089153415335295583 ) ) ;
#11000 = CARTESIAN_POINT ( 'NONE',  ( 2.241526690369557429, 2.627393882429315930, 7.168108047190845156 ) ) ;
#11001 = CARTESIAN_POINT ( 'NONE',  ( 0.4626703367447430049, -5.909149965570928309, -10.80124546303572330 ) ) ;
#11002 = LINE ( 'NONE', #38132, #65159 ) ;
#11003 = FACE_BOUND ( 'NONE', #13857, .T. ) ;
#11004 = CIRCLE ( 'NONE', #49236, 2.899999999999994138 ) ;
#11005 = AXIS2_PLACEMENT_3D ( 'NONE', #20690, #14050, #30641 ) ;
#11006 = AXIS2_PLACEMENT_3D ( 'NONE', #19833, #35093, #19516 ) ;
#11007 = EDGE_CURVE ( 'NONE', #31314, #41256, #38619, .T. ) ;
#11008 = VERTEX_POINT ( 'NONE', #52222 ) ;
#11009 = EDGE_LOOP ( 'NONE', ( #141, #19135, #62848, #49453 ) ) ;
#11011 = VECTOR ( 'NONE', #43446, 1000.000000000000000 ) ;
#11010 = CARTESIAN_POINT ( 'NONE',  ( -22.39032720737627358, 3.847057950743288490, -1.170177197944845426 ) ) ;
#11012 = DIRECTION ( 'NONE',  ( 1.000000000000000000, 0.000000000000000000, 0.000000000000000000 ) ) ;
#11013 = CARTESIAN_POINT ( 'NONE',  ( 37.00000000000000711, -9.512294188640847636, 6.891188680298922620 ) ) ;
#11014 = AXIS2_PLACEMENT_3D ( 'NONE', #6245, #35809, #46162 ) ;
#11015 = CARTESIAN_POINT ( 'NONE',  ( 0.2767916011545371036, -1.940025653808925554, 12.09541651105896776 ) ) ;
#11016 = ORIENTED_EDGE ( 'NONE', *, *, #20103, .F. ) ;
#11017 = CIRCLE ( 'NONE', #48218, 4.999999999999999112 ) ;
#11018 = VERTEX_POINT ( 'NONE', #16633 ) ;
#11019 = EDGE_LOOP ( 'NONE', ( #34898, #43294, #50887, #28961 ) ) ;
#11020 = CARTESIAN_POINT ( 'NONE',  ( 2.994568964204215256, 7.875338388187474337, 0.3996732855055006306 ) ) ;
#11021 = AXIS2_PLACEMENT_3D ( 'NONE', #55007, #57312, #36016 ) ;
#11022 = CARTESIAN_POINT ( 'NONE',  ( -22.27718150314433387, 0.7862703917636705286, 3.596602356343891138 ) ) ;
#11023 = EDGE_CURVE ( 'NONE', #57274, #39511, #44112, .T. ) ;
#11024 = ORIENTED_EDGE ( 'NONE', *, *, #34159, .T. ) ;
#11025 = DIRECTION ( 'NONE',  ( -1.000000000000000000, 0.000000000000000000, 0.000000000000000000 ) ) ;
#11026 = DIRECTION ( 'NONE',  ( 0.000000000000000000, -0.01356324068817991828, 0.9999080150203990547 ) ) ;
#11027 = ORIENTED_EDGE ( 'NONE', *, *, #41730, .F. ) ;
#11028 = CARTESIAN_POINT ( 'NONE',  ( -22.27945548916780183, 0.3299677273100789510, 3.673577025288749187 ) ) ;
#11029 = EDGE_CURVE ( 'NONE', #39390, #58474, #32421, .T. ) ;
#11030 = VECTOR ( 'NONE', #52451, 1000.000000000000000 ) ;
#11031 = CARTESIAN_POINT ( 'NONE',  ( 16.79298069408831751, -34.48269025770164120, -5.249417709786706965 ) ) ;
#11032 = CARTESIAN_POINT ( 'NONE',  ( 23.20038713279159026, 3.176051149014137653, 11.57489057894666651 ) ) ;
#11033 = ORIENTED_EDGE ( 'NONE', *, *, #60960, .F. ) ;
#11034 = CARTESIAN_POINT ( 'NONE',  ( -37.00000000000000711, 0.8294751490781091530, -12.15823808070321910 ) ) ;
#11035 = EDGE_CURVE ( 'NONE', #58225, #32302, #11630, .T. ) ;
#11036 = ORIENTED_EDGE ( 'NONE', *, *, #17449, .F. ) ;
#11037 = DIRECTION ( 'NONE',  ( -1.000000000000000000, 0.000000000000000000, 0.000000000000000000 ) ) ;
#11038 = ORIENTED_EDGE ( 'NONE', *, *, #29967, .T. ) ;
#11039 = CARTESIAN_POINT ( 'NONE',  ( -18.25006854224444908, -9.443202773001939221, 9.647586298549914119 ) ) ;
#11040 = CARTESIAN_POINT ( 'NONE',  ( 5.514970785353741078, 0.004588761610585025477, -0.001117786416802570059 ) ) ;
#11041 = DIRECTION ( 'NONE',  ( -1.000000000000000000, 0.000000000000000000, 0.000000000000000000 ) ) ;
#11042 = CARTESIAN_POINT ( 'NONE',  ( -35.00000000000000000, -11.66664283989676321, -5.143145423404402727 ) ) ;
#11043 = DIRECTION ( 'NONE',  ( -1.000000000000000000, 0.000000000000000000, 0.000000000000000000 ) ) ;
#11045 = ADVANCED_FACE ( 'NONE', ( #26937 ), #6984, .T. ) ;
#11044 = DIRECTION ( 'NONE',  ( -1.000000000000000000, 0.000000000000000000, 0.000000000000000000 ) ) ;
#11046 = DIRECTION ( 'NONE',  ( -1.000000000000000000, 0.000000000000000000, 0.000000000000000000 ) ) ;
#11047 = CARTESIAN_POINT ( 'NONE',  ( 0.2653141617321028156, 4.147035654172719354, 11.52265685897330449 ) ) ;
#11049 = ORIENTED_EDGE ( 'NONE', *, *, #35267, .F. ) ;
#11048 = CARTESIAN_POINT ( 'NONE',  ( 3.865165140261278331, -11.00552270324296700, 7.820176569034111402 ) ) ;
#11050 = DIRECTION ( 'NONE',  ( -1.000000000000000000, 0.000000000000000000, 0.000000000000000000 ) ) ;
#11051 = ORIENTED_EDGE ( 'NONE', *, *, #55031, .F. ) ;
#11052 = CARTESIAN_POINT ( 'NONE',  ( 1.937114397841935398, -1.334979369128509674, 12.76557247858998068 ) ) ;
#11053 = EDGE_CURVE ( 'NONE', #58632, #17370, #41784, .T. ) ;
#11054 = FACE_OUTER_BOUND ( 'NONE', #44230, .T. ) ;
#11055 = AXIS2_PLACEMENT_3D ( 'NONE', #4894, #50448, #51756 ) ;
#11056 = ORIENTED_EDGE ( 'NONE', *, *, #52253, .T. ) ;
#11058 = AXIS2_PLACEMENT_3D ( 'NONE', #51820, #11887, #7224 ) ;
#11057 = DIRECTION ( 'NONE',  ( 1.000000000000000000, 0.000000000000000000, 0.000000000000000000 ) ) ;
#11059 = DIRECTION ( 'NONE',  ( 0.000000000000000000, 1.000000000000000000, 0.000000000000000000 ) ) ;
#11060 = CARTESIAN_POINT ( 'NONE',  ( 3.152665057734040488, 0.000000000000000000, 0.000000000000000000 ) ) ;
#11061 = CARTESIAN_POINT ( 'NONE',  ( -22.66110217412718342, 3.020638270782550094, -3.914841338650321578 ) ) ;
#11062 = VECTOR ( 'NONE', #48326, 1000.000000000000000 ) ;
#11063 = CARTESIAN_POINT ( 'NONE',  ( -41.00000000000000711, -1.694065894508793271E-18, 4.500000000000001776 ) ) ;
#11064 = ORIENTED_EDGE ( 'NONE', *, *, #39016, .F. ) ;
#11065 = CARTESIAN_POINT ( 'NONE',  ( -17.19897187406723305, -8.155961655565807433, -8.809094555608780297 ) ) ;
#11066 = EDGE_CURVE ( 'NONE', #46955, #55862, #35418, .T. ) ;
#11067 = VECTOR ( 'NONE', #29790, 1000.000000000000000 ) ;
#11068 = ORIENTED_EDGE ( 'NONE', *, *, #19601, .T. ) ;
#11069 = CARTESIAN_POINT ( 'NONE',  ( -35.04709527796842394, -0.01120703303052195121, 0.005220632200989699934 ) ) ;
#11070 = EDGE_CURVE ( 'NONE', #31482, #60850, #43194, .T. ) ;
#11071 = CARTESIAN_POINT ( 'NONE',  ( 37.00000000000000711, 4.705694406421931860E-17, -3.469127814946512892E-15 ) ) ;
#11072 = CARTESIAN_POINT ( 'NONE',  ( 35.00000000000000000, 12.12087942037209842, -1.262958560998807656 ) ) ;
#11073 = VERTEX_POINT ( 'NONE', #53539 ) ;
#11074 = CIRCLE ( 'NONE', #39731, 2.899999999999995914 ) ;
#11075 = CARTESIAN_POINT ( 'NONE',  ( 0.000000000000000000, -33.00000000000000000, 0.000000000000000000 ) ) ;
#11076 = CIRCLE ( 'NONE', #17442, 12.18650000000000233 ) ;
#11077 = CARTESIAN_POINT ( 'NONE',  ( -35.05012975565874456, 0.01039213056759654037, -0.009279204628456355630 ) ) ;
#11078 =( BOUNDED_SURFACE ( )  B_SPLINE_SURFACE ( 3, 1, ( 
 ( #41344, #15739 ),
 ( #40704, #52002 ),
 ( #61628, #30709 ),
 ( #5139, #36019 ) ),
 .UNSPECIFIED., .F., .F., .T. ) 
 B_SPLINE_SURFACE_WITH_KNOTS ( ( 4, 4 ),
 ( 2, 2 ),
 ( 0.000000000000000000, 1.000000000000000000 ),
 ( 0.000000000000000000, 1.000000000000000000 ),
 .UNSPECIFIED. ) 
 GEOMETRIC_REPRESENTATION_ITEM ( )  RATIONAL_B_SPLINE_SURFACE ( (
 ( 1.000000000000000000, 1.000000000000000000),
 ( 0.9942764183789327692, 0.8450855930916580938),
 ( 0.9942764183789327692, 0.8450855930916580938),
 ( 1.000000000000000000, 1.000000000000000000) ) ) 
 REPRESENTATION_ITEM ( '' )  SURFACE ( )  );
#11079 = CARTESIAN_POINT ( 'NONE',  ( -35.00000000000000000, -10.62137734850264614, -5.015831474386418520 ) ) ;
#11080 = DIRECTION ( 'NONE',  ( 0.000000000000000000, 0.4198891015602592147, 0.9075754196709596711 ) ) ;
#11081 = CARTESIAN_POINT ( 'NONE',  ( 8.437200413559443390, 4.861907246157027629, 12.60074865033406688 ) ) ;
#11082 = CARTESIAN_POINT ( 'NONE',  ( -28.41827485489077532, 3.509237424706436403, 13.03592162821792222 ) ) ;
#11083 = CARTESIAN_POINT ( 'NONE',  ( 0.000000000000000000, -6.796153407501448029, 1.388283512725787761 ) ) ;
#11084 = DIRECTION ( 'NONE',  ( 1.000000000000000000, 0.000000000000000000, -0.000000000000000000 ) ) ;
#11085 = ADVANCED_FACE ( 'NONE', ( #53189 ), #42874, .T. ) ;
#11086 = ORIENTED_EDGE ( 'NONE', *, *, #48249, .T. ) ;
#11087 = LINE ( 'NONE', #11398, #18292 ) ;
#11088 = DIRECTION ( 'NONE',  ( 0.000000000000000000, 0.000000000000000000, 1.000000000000000000 ) ) ;
#11089 = VERTEX_POINT ( 'NONE', #23926 ) ;
#11090 = EDGE_CURVE ( 'NONE', #24439, #30430, #56905, .T. ) ;
#11091 = CARTESIAN_POINT ( 'NONE',  ( 35.00000000000000000, 5.428340790341703581, -10.91072401419412685 ) ) ;
#11092 = DIRECTION ( 'NONE',  ( 0.000000000000000000, -0.01356324068817999114, 0.9999080150203989437 ) ) ;
#11093 = CARTESIAN_POINT ( 'NONE',  ( -37.00000000000000711, 11.73463472867576129, 3.287724142101457137 ) ) ;
#11094 = ORIENTED_EDGE ( 'NONE', *, *, #37797, .F. ) ;
#11095 = CARTESIAN_POINT ( 'NONE',  ( 5.516018279890452902, -0.005976902763919015801, 0.003191189039764900665 ) ) ;
#11096 = CARTESIAN_POINT ( 'NONE',  ( 47.00000000000000711, 4.705694406421931860E-17, -3.469127814946512892E-15 ) ) ;
#11097 = ORIENTED_EDGE ( 'NONE', *, *, #27086, .F. ) ;
#11098 = EDGE_CURVE ( 'NONE', #53717, #25218, #3663, .T. ) ;
#11099 = AXIS2_PLACEMENT_3D ( 'NONE', #10918, #47805, #41830 ) ;
#11100 = CARTESIAN_POINT ( 'NONE',  ( 0.2648978790185610999, -6.008231198269058382, 10.67083876753489946 ) ) ;
#11101 = VERTEX_POINT ( 'NONE', #54170 ) ;
#11102 = VERTEX_POINT ( 'NONE', #44186 ) ;
#11103 = DIRECTION ( 'NONE',  ( 0.000000000000000000, -1.000000000000000000, 0.000000000000000000 ) ) ;
#11104 = EDGE_CURVE ( 'NONE', #44042, #44597, #16497, .T. ) ;
#11105 = ORIENTED_EDGE ( 'NONE', *, *, #37462, .F. ) ;
#11106 = CARTESIAN_POINT ( 'NONE',  ( -24.90342394282648186, -7.521682070300208522, 9.357467395294243317 ) ) ;
#11107 = DIRECTION ( 'NONE',  ( 1.000000000000000000, 0.000000000000000000, -0.000000000000000000 ) ) ;
#11108 = DIRECTION ( 'NONE',  ( -1.000000000000000000, -0.000000000000000000, -0.000000000000000000 ) ) ;
#11109 = CARTESIAN_POINT ( 'NONE',  ( 10.21897715134382700, 7.428883895067158960, 9.428733153766255981 ) ) ;
#11110 = ORIENTED_EDGE ( 'NONE', *, *, #62578, .F. ) ;
#11111 = CARTESIAN_POINT ( 'NONE',  ( 37.00000000000000711, 2.216820770815085773, -11.53507381115584529 ) ) ;
#11112 = CARTESIAN_POINT ( 'NONE',  ( 15.30590914263659386, -28.05839919878968303, 10.93630420992710128 ) ) ;
#11113 = CARTESIAN_POINT ( 'NONE',  ( 11.74548640120467979, -10.73597826697111124, -8.184666801472349817 ) ) ;
#11115 = VERTEX_POINT ( 'NONE', #48541 ) ;
#11114 = CARTESIAN_POINT ( 'NONE',  ( 0.2653519991613820239, -12.05632699103097494, -2.148211862903036451 ) ) ;
#11116 = LINE ( 'NONE', #20432, #35223 ) ;
#11117 = ADVANCED_FACE ( 'NONE', ( #7637 ), #64454, .T. ) ;
#11118 = ORIENTED_EDGE ( 'NONE', *, *, #46953, .T. ) ;
#11119 = CARTESIAN_POINT ( 'NONE',  ( -37.00000000000000711, 2.497432891017006718, -11.47758908105691766 ) ) ;
#11120 = ORIENTED_EDGE ( 'NONE', *, *, #36006, .F. ) ;
#11121 = ORIENTED_EDGE ( 'NONE', *, *, #18776, .T. ) ;
#11122 = CARTESIAN_POINT ( 'NONE',  ( -35.00000000000000000, 10.92721691015462149, -4.309077947445535628 ) ) ;
#11123 = CARTESIAN_POINT ( 'NONE',  ( -35.00000000000000000, 3.093009498344089447, -11.78745411414836930 ) ) ;
#11124 = AXIS2_PLACEMENT_3D ( 'NONE', #18799, #38410, #8477 ) ;
#11125 = FACE_OUTER_BOUND ( 'NONE', #26136, .T. ) ;
#11126 = ORIENTED_EDGE ( 'NONE', *, *, #23872, .F. ) ;
#11127 = LINE ( 'NONE', #16446, #37609 ) ;
#11128 = CARTESIAN_POINT ( 'NONE',  ( 2.000000000000001776, 6.936109781200682889, 2.853135311045038591 ) ) ;
#11129 = CARTESIAN_POINT ( 'NONE',  ( 5.515188684475870851, 0.002355816063606810083, -0.004804816249379317492 ) ) ;
#11130 = VERTEX_POINT ( 'NONE', #37889 ) ;
#11131 = ORIENTED_EDGE ( 'NONE', *, *, #33005, .F. ) ;
#11132 = DIRECTION ( 'NONE',  ( -1.000000000000000000, 0.000000000000000000, 0.000000000000000000 ) ) ;
#11133 = ORIENTED_EDGE ( 'NONE', *, *, #63620, .T. ) ;
#11134 = EDGE_CURVE ( 'NONE', #33743, #38347, #35609, .T. ) ;
#11135 = EDGE_CURVE ( 'NONE', #38796, #60499, #41971, .T. ) ;
#11136 = ORIENTED_EDGE ( 'NONE', *, *, #54987, .T. ) ;
#11137 = CARTESIAN_POINT ( 'NONE',  ( 1.937114397841935398, -3.531416430611377777, 12.33981801388256550 ) ) ;
#11138 = CARTESIAN_POINT ( 'NONE',  ( -27.08429572838383947, 0.2296550094123047669, 2.279961732801582208 ) ) ;
#11139 = CYLINDRICAL_SURFACE ( 'NONE', #8590, 4.999999999999999112 ) ;
#11140 = B_SPLINE_CURVE_WITH_KNOTS ( 'NONE', 3,
 ( #10993, #45568, #30931, #26281, #15631, #46559, #5352, #20, #50586, #35902 ),
 .UNSPECIFIED., .F., .F.,
 ( 4, 3, 3, 4 ),
 ( 8.673617379884035472E-19, 6.607638129004486172E-05, 9.911389841680512771E-05, 0.0001667630577588619318 ),
 .UNSPECIFIED. ) ;
#11141 = DIRECTION ( 'NONE',  ( -1.000000000000000000, 0.000000000000000000, -0.000000000000000000 ) ) ;
#11142 = EDGE_CURVE ( 'NONE', #10138, #58567, #64147, .T. ) ;
#11143 = CARTESIAN_POINT ( 'NONE',  ( -37.00000000000000711, 0.2661492558805056974, -12.18359334611896116 ) ) ;
#11144 = CARTESIAN_POINT ( 'NONE',  ( -37.00000000000000711, 0.000000000000000000, 0.000000000000000000 ) ) ;
#11145 = EDGE_CURVE ( 'NONE', #14988, #31123, #29261, .T. ) ;
#11146 = CARTESIAN_POINT ( 'NONE',  ( 22.57855258442565116, 3.026812727784649493, -11.61199400236326973 ) ) ;
#11147 = VERTEX_POINT ( 'NONE', #27576 ) ;
#11148 = ADVANCED_FACE ( 'NONE', ( #47873 ), #45433, .F. ) ;
#11149 = CARTESIAN_POINT ( 'NONE',  ( -22.28023996335807766, -3.022323476748280502, 2.118259050016073175 ) ) ;
#11150 =( NAMED_UNIT ( * ) SI_UNIT ( $, .STERADIAN. ) SOLID_ANGLE_UNIT ( ) );
#11151 = CARTESIAN_POINT ( 'NONE',  ( 2.241352910868909643, -7.202080440908757986, 2.532612177304417678 ) ) ;
#11152 = DIRECTION ( 'NONE',  ( -1.000000000000000000, 0.000000000000000000, 0.000000000000000000 ) ) ;
#11153 = DIRECTION ( 'NONE',  ( 1.000000000000000000, 0.000000000000000000, 0.000000000000000000 ) ) ;
#11154 = CARTESIAN_POINT ( 'NONE',  ( 3.734305248975252400, 4.620446052658566671, -11.08365692675047498 ) ) ;
#11155 = CARTESIAN_POINT ( 'NONE',  ( -27.08426504710140392, -2.202478235133281892, -0.6326154899769481643 ) ) ;
#11156 = ORIENTED_EDGE ( 'NONE', *, *, #23529, .T. ) ;
#11157 = CARTESIAN_POINT ( 'NONE',  ( 0.3665391374699472626, 0.2638605131387167790, 12.27992639892678461 ) ) ;
#11158 = LINE ( 'NONE', #6178, #12279 ) ;
#11159 = DIRECTION ( 'NONE',  ( 1.000000000000000000, 0.000000000000000000, 0.000000000000000000 ) ) ;
#11160 = CARTESIAN_POINT ( 'NONE',  ( 0.000000000000000000, -45.00000000000000000, -23.66025403784440684 ) ) ;
#11161 = CIRCLE ( 'NONE', #49402, 12.18649999999999878 ) ;
#11162 = ADVANCED_FACE ( 'NONE', ( #59814 ), #59065, .F. ) ;
#11163 = CARTESIAN_POINT ( 'NONE',  ( 0.2646305136544072623, -12.03696649559613441, -2.256625640822436996 ) ) ;
#11164 = CARTESIAN_POINT ( 'NONE',  ( 2.653899356900250694, -7.209790345489586194, 2.902068786425478386 ) ) ;
#11165 = ORIENTED_EDGE ( 'NONE', *, *, #50001, .F. ) ;
#11166 = FACE_OUTER_BOUND ( 'NONE', #21386, .T. ) ;
#11167 = CARTESIAN_POINT ( 'NONE',  ( -18.58686583997218378, 5.151216734910788908, 25.00000000000000000 ) ) ;
#11168 = CARTESIAN_POINT ( 'NONE',  ( 2.268878695253355726, 1.181158368266951308, 7.551766617932576864 ) ) ;
#11169 = ORIENTED_EDGE ( 'NONE', *, *, #61174, .T. ) ;
#11170 = DIRECTION ( 'NONE',  ( 0.000000000000000000, -0.01356324068817998940, 0.9999080150203990547 ) ) ;
#11171 = CARTESIAN_POINT ( 'NONE',  ( -18.06081662158740642, 5.589072243798248074, -10.62163489563124763 ) ) ;
#11172 = CARTESIAN_POINT ( 'NONE',  ( 35.00000000000000000, 4.705694406421931860E-17, -3.469127814946512892E-15 ) ) ;
#11173 = EDGE_CURVE ( 'NONE', #33373, #16971, #17602, .T. ) ;
#11175 = EDGE_LOOP ( 'NONE', ( #25756, #65718, #62624, #47304 ) ) ;
#11174 = CARTESIAN_POINT ( 'NONE',  ( 3.152665057733966769, 0.9030954876739563097, 7.886634106564108571 ) ) ;
#11176 = LINE ( 'NONE', #41753, #38440 ) ;
#11177 = AXIS2_PLACEMENT_3D ( 'NONE', #57942, #41305, #37645 ) ;
#11178 = CARTESIAN_POINT ( 'NONE',  ( -23.41523303002441736, -4.681453266967030125, -0.3963225057405078133 ) ) ;
#11179 = VERTEX_POINT ( 'NONE', #14554 ) ;
#11180 = CARTESIAN_POINT ( 'NONE',  ( 0.2833330754217382452, 7.719627479384659985, 9.514385791198117559 ) ) ;
#11181 = CARTESIAN_POINT ( 'NONE',  ( 0.2646305136544065406, -6.008537389229490877, 10.67138229758227652 ) ) ;
#11182 = CARTESIAN_POINT ( 'NONE',  ( 23.74704636295951587, -3.121621105806414498, -11.59142313195714635 ) ) ;
#11183 = DIRECTION ( 'NONE',  ( -1.000000000000000000, 0.000000000000000000, 0.000000000000000000 ) ) ;
#11184 = CARTESIAN_POINT ( 'NONE',  ( 0.2648321136542705623, -11.45826514585340306, -4.321267941897623643 ) ) ;
#11185 = CARTESIAN_POINT ( 'NONE',  ( 2.241526690369556096, 2.594870554108938521, -7.179945570618733619 ) ) ;
#11187 = VERTEX_POINT ( 'NONE', #54828 ) ;
#11186 = CARTESIAN_POINT ( 'NONE',  ( 0.2655924914740778742, 10.62761259256416935, 6.084990060696545910 ) ) ;
#11188 = EDGE_CURVE ( 'NONE', #44435, #49368, #65112, .T. ) ;
#11189 = ORIENTED_EDGE ( 'NONE', *, *, #45323, .F. ) ;
#11190 = DIRECTION ( 'NONE',  ( -1.000000000000000000, 0.000000000000000000, 0.000000000000000000 ) ) ;
#11191 = ORIENTED_EDGE ( 'NONE', *, *, #63463, .F. ) ;
#11192 = DIRECTION ( 'NONE',  ( 0.000000000000000000, 0.000000000000000000, 1.000000000000000000 ) ) ;
#11193 = EDGE_CURVE ( 'NONE', #54941, #37857, #44144, .T. ) ;
#11194 = DIRECTION ( 'NONE',  ( 0.000000000000000000, 0.9937233664769756780, -0.1118654143051654171 ) ) ;
#11195 = CARTESIAN_POINT ( 'NONE',  ( -16.98800322446194855, 2.922502605998049674, 11.63868456991315625 ) ) ;
#11196 = DIRECTION ( 'NONE',  ( -1.000000000000000000, 0.000000000000000000, 0.000000000000000000 ) ) ;
#11197 = ORIENTED_EDGE ( 'NONE', *, *, #9349, .T. ) ;
#11198 = CARTESIAN_POINT ( 'NONE',  ( 1.452237505248552996, 8.579708443906870485, -9.303501428255941619 ) ) ;
#11199 = CIRCLE ( 'NONE', #48386, 12.74999999999999822 ) ;
#11200 = CARTESIAN_POINT ( 'NONE',  ( 0.2638984909335720941, 1.930290337334216622, -12.09426044257622479 ) ) ;
#11201 = FACE_OUTER_BOUND ( 'NONE', #24798, .T. ) ;
#11202 = ORIENTED_EDGE ( 'NONE', *, *, #8619, .T. ) ;
#11203 = ORIENTED_EDGE ( 'NONE', *, *, #44402, .T. ) ;
#11204 = CARTESIAN_POINT ( 'NONE',  ( 2.844750968615874509, 7.651810733888815719, -1.686994672842110798 ) ) ;
#11205 = ORIENTED_EDGE ( 'NONE', *, *, #65077, .T. ) ;
#11206 = CARTESIAN_POINT ( 'NONE',  ( 21.99454477296592714, -11.37209199534426318, -3.835509361899974046 ) ) ;
#11207 = CARTESIAN_POINT ( 'NONE',  ( 0.2638984909335720941, -4.001111175853819368, 11.57533005135177717 ) ) ;
#11208 = DIRECTION ( 'NONE',  ( -1.000000000000000000, 0.000000000000000000, 0.000000000000000000 ) ) ;
#11209 = EDGE_CURVE ( 'NONE', #40162, #1597, #39847, .T. ) ;
#11210 = CIRCLE ( 'NONE', #34547, 12.18650000000000055 ) ;
#11211 = DIRECTION ( 'NONE',  ( -0.000000000000000000, -1.000000000000000000, -0.000000000000000000 ) ) ;
#11212 = FACE_OUTER_BOUND ( 'NONE', #37202, .T. ) ;
#11213 = DIRECTION ( 'NONE',  ( 0.000000000000000000, 0.9999080150203989437, 0.01356324068817649567 ) ) ;
#11214 = EDGE_CURVE ( 'NONE', #23613, #14430, #24995, .T. ) ;
#11215 = CARTESIAN_POINT ( 'NONE',  ( 2.242819959140647246, 7.500446639314770181, 1.426511055719334564 ) ) ;
#11216 = ORIENTED_EDGE ( 'NONE', *, *, #51506, .F. ) ;
#11217 = CARTESIAN_POINT ( 'NONE',  ( 1.719304012338199295, 12.70777170743846796, -0.7661785589580241140 ) ) ;
#11218 = ADVANCED_FACE ( 'NONE', ( #29529 ), #9565, .T. ) ;
#11219 = CARTESIAN_POINT ( 'NONE',  ( 25.05309951391468459, 8.823569016628493245, -8.132934882857099979 ) ) ;
#11220 = CARTESIAN_POINT ( 'NONE',  ( -18.49080574448680991, -12.00000000000057909, -4.407108900774715188E-13 ) ) ;
#11221 = CARTESIAN_POINT ( 'NONE',  ( 5.515188684475870851, 0.002983184900675330160, 0.004442604682416625983 ) ) ;
#11222 = CARTESIAN_POINT ( 'NONE',  ( 37.00000000000000711, -10.99909370905160699, -5.246972444133983338 ) ) ;
#11223 = CARTESIAN_POINT ( 'NONE',  ( 5.520433897694421610, -0.01278034823632010972, 0.007971295965052730206 ) ) ;
#11224 = DIRECTION ( 'NONE',  ( -1.000000000000000000, 0.000000000000000000, 0.000000000000000000 ) ) ;
#11225 = EDGE_LOOP ( 'NONE', ( #27801, #54857, #64465, #20701 ) ) ;
#11226 = VECTOR ( 'NONE', #42122, 1000.000000000000000 ) ;
#11227 = ORIENTED_EDGE ( 'NONE', *, *, #15126, .F. ) ;
#11228 = LINE ( 'NONE', #65742, #56705 ) ;
#11229 = EDGE_CURVE ( 'NONE', #47974, #4532, #29859, .T. ) ;
#11230 = B_SPLINE_CURVE_WITH_KNOTS ( 'NONE', 3,
 ( #44089, #65655, #64361, #60694, #64668, #54736, #9158 ),
 .UNSPECIFIED., .F., .F.,
 ( 4, 3, 4 ),
 ( 0.000000000000000000, 0.001700533616330602389, 0.005002426799371321661 ),
 .UNSPECIFIED. ) ;
#11231 = VERTEX_POINT ( 'NONE', #19895 ) ;
#11232 = CARTESIAN_POINT ( 'NONE',  ( 2.000000000000001776, 3.341639490130849488, -6.078525953551423555 ) ) ;
#11233 = CARTESIAN_POINT ( 'NONE',  ( 35.00000000000000000, -9.506317355798429958, -8.496612874013125705 ) ) ;
#11234 = CARTESIAN_POINT ( 'NONE',  ( 1.547277799339146664, -10.12789507952348167, -7.618736734813534639 ) ) ;
#11235 = ORIENTED_EDGE ( 'NONE', *, *, #55133, .F. ) ;
#11236 = LINE ( 'NONE', #55814, #64301 ) ;
#11237 = CARTESIAN_POINT ( 'NONE',  ( 2.241531873784870399, -0.01153688368838857656, -7.634454672504356054 ) ) ;
#11238 = LINE ( 'NONE', #61430, #25833 ) ;
#11239 = CARTESIAN_POINT ( 'NONE',  ( -22.31328051695926007, 1.671726071983979711, -3.401210163132561082 ) ) ;
#11240 = CIRCLE ( 'NONE', #39908, 2.899999999999996803 ) ;
#11241 = DIRECTION ( 'NONE',  ( 0.000000000000000000, -0.01356324068817998940, 0.9999080150203989437 ) ) ;
#11242 = EDGE_CURVE ( 'NONE', #1249, #153, #9262, .T. ) ;
#11243 = DIRECTION ( 'NONE',  ( -1.000000000000000000, 0.000000000000000000, 0.000000000000000000 ) ) ;
#11244 = AXIS2_PLACEMENT_3D ( 'NONE', #57125, #16224, #20222 ) ;
#11245 = ORIENTED_EDGE ( 'NONE', *, *, #40574, .T. ) ;
#11246 = CARTESIAN_POINT ( 'NONE',  ( -27.08430792439084556, -0.6005833784278348242, 2.211452765398279841 ) ) ;
#11247 = VERTEX_POINT ( 'NONE', #46800 ) ;
#11248 = FACE_OUTER_BOUND ( 'NONE', #19854, .T. ) ;
#11249 = DIRECTION ( 'NONE',  ( 0.000000000000000000, 0.000000000000000000, 1.000000000000000000 ) ) ;
#11250 = CARTESIAN_POINT ( 'NONE',  ( 1.719304012339867516, -12.38166659046446938, 2.961219984258617544 ) ) ;
#11251 = ADVANCED_FACE ( 'NONE', ( #32147 ), #6820, .F. ) ;
#11253 = FACE_OUTER_BOUND ( 'NONE', #49004, .T. ) ;
#11252 = B_SPLINE_CURVE_WITH_KNOTS ( 'NONE', 3,
 ( #23134, #59700, #19469, #43399, #54055, #44706, #8829, #14128, #9142, #29425, #29118, #64343, #49721, #64657, #59366, #3861, #33751, #24119, #24433, #39400, #63675, #7857 ),
 .UNSPECIFIED., .F., .F.,
 ( 4, 2, 2, 2, 2, 2, 2, 2, 2, 2, 4 ),
 ( 8.673617379884035472E-19, 0.001081624167374303650, 0.002163248334748606432, 0.003244872502122908564, 0.004326496669497210262, 0.004867308753184361111, 0.005408120836871511961, 0.005948932920558663677, 0.006489745004245815393, 0.007571369171620122296, 0.008652993338994427464 ),
 .UNSPECIFIED. ) ;
#11254 = CARTESIAN_POINT ( 'NONE',  ( -9.842799140981188799, -4.069970586457803741, 11.29001410203253108 ) ) ;
#11255 = CIRCLE ( 'NONE', #20794, 7.938172270156617749 ) ;
#11256 = ORIENTED_EDGE ( 'NONE', *, *, #12025, .F. ) ;
#11257 = VERTEX_POINT ( 'NONE', #21874 ) ;
#11258 = FACE_OUTER_BOUND ( 'NONE', #59544, .T. ) ;
#11259 = ORIENTED_EDGE ( 'NONE', *, *, #55830, .F. ) ;
#11260 = CARTESIAN_POINT ( 'NONE',  ( 35.00000000000000000, -8.954052073409666690, -9.076753354953966735 ) ) ;
#11262 = CARTESIAN_POINT ( 'NONE',  ( -35.04643116707788408, -0.008094444324497490628, -0.009112266603826177369 ) ) ;
#11261 =( BOUNDED_CURVE ( )  B_SPLINE_CURVE ( 3, ( #5096, #45641, #35660, #56623 ),
 .UNSPECIFIED., .F., .F. ) 
 B_SPLINE_CURVE_WITH_KNOTS ( ( 4, 4 ),
 ( 2.321366128334107160, 2.361114018676058635 ),
 .UNSPECIFIED. ) 
 CURVE ( )  GEOMETRIC_REPRESENTATION_ITEM ( )  RATIONAL_B_SPLINE_CURVE ( ( 1.000000000000000000, 0.9998683464345071714, 0.9998683464345071714, 1.000000000000000000 ) ) 
 REPRESENTATION_ITEM ( '' )  );
#11263 = DIRECTION ( 'NONE',  ( 0.000000000000000000, -0.9651210252299822212, -0.2618041379715529970 ) ) ;
#11264 = CARTESIAN_POINT ( 'NONE',  ( -27.16343335735464493, 10.63351257863160981, -8.317934404008967775 ) ) ;
#11265 = CARTESIAN_POINT ( 'NONE',  ( 1.375507693219674143, -7.647735792764906115, -10.03411718356184856 ) ) ;
#11266 = CARTESIAN_POINT ( 'NONE',  ( 0.000000000000000000, -3.979254915827311390, -5.681598592373819478 ) ) ;
#11267 = CARTESIAN_POINT ( 'NONE',  ( -10.87446691779126695, -4.893491060116321734, 10.96515481982397766 ) ) ;
#11268 = ORIENTED_EDGE ( 'NONE', *, *, #57452, .F. ) ;
#11269 = EDGE_CURVE ( 'NONE', #8493, #59819, #43055, .T. ) ;
#11270 = EDGE_CURVE ( 'NONE', #25074, #50979, #60066, .T. ) ;
#11271 = CARTESIAN_POINT ( 'NONE',  ( 0.8375941296801195923, -10.95781044612433064, 5.882592429484332364 ) ) ;
#11272 = VERTEX_POINT ( 'NONE', #6906 ) ;
#11273 = EDGE_CURVE ( 'NONE', #50124, #53881, #46472, .T. ) ;
#11274 = DIRECTION ( 'NONE',  ( 1.000000000000000000, 0.000000000000000000, 0.000000000000000000 ) ) ;
#11275 = CARTESIAN_POINT ( 'NONE',  ( 1.198791140421116008, 8.460175745279389758, -9.279671759317686508 ) ) ;
#11276 = ORIENTED_EDGE ( 'NONE', *, *, #11581, .F. ) ;
#11277 = FACE_OUTER_BOUND ( 'NONE', #55749, .T. ) ;
#11278 = EDGE_LOOP ( 'NONE', ( #20895, #9724, #33905, #33593 ) ) ;
#11279 = CARTESIAN_POINT ( 'NONE',  ( -35.00000000000000000, 2.527899948230635907, 12.49688848680885123 ) ) ;
#11280 = CARTESIAN_POINT ( 'NONE',  ( -16.81745777873098646, -34.49999999816794372, -5.267778333666905510 ) ) ;
#11281 = DIRECTION ( 'NONE',  ( 1.000000000000000000, -0.000000000000000000, 0.000000000000000000 ) ) ;
#11282 = VERTEX_POINT ( 'NONE', #21194 ) ;
#11283 = VERTEX_POINT ( 'NONE', #36501 ) ;
#11284 = CARTESIAN_POINT ( 'NONE',  ( 5.514970785353741078, -0.001897634820904511074, 0.004324946436530178843 ) ) ;
#11285 = ORIENTED_EDGE ( 'NONE', *, *, #50914, .F. ) ;
#11286 = CARTESIAN_POINT ( 'NONE',  ( -35.00000000000000000, -0.2661492558804205988, 12.18359334611896472 ) ) ;
#11287 = ORIENTED_EDGE ( 'NONE', *, *, #46751, .T. ) ;
#11288 = VERTEX_POINT ( 'NONE', #27177 ) ;
#11289 = ORIENTED_EDGE ( 'NONE', *, *, #39024, .T. ) ;
#11290 = CARTESIAN_POINT ( 'NONE',  ( 2.556980015513156790, -5.777953785406852560, 5.149458076504425996 ) ) ;
#11291 = ADVANCED_FACE ( 'NONE', ( #51154 ), #13357, .T. ) ;
#11292 = CARTESIAN_POINT ( 'NONE',  ( 2.000000000000001776, 0.000000000000000000, 0.000000000000000000 ) ) ;
#11293 = CARTESIAN_POINT ( 'NONE',  ( 2.963017218115627127, -0.9869543242667578875, -7.812878240621082604 ) ) ;
#11294 = CARTESIAN_POINT ( 'NONE',  ( 2.245754705088393255, 2.715960966012193278, -7.136529175883334020 ) ) ;
#11295 = CYLINDRICAL_SURFACE ( 'NONE', #18958, 12.18649999999999878 ) ;
#11296 = VERTEX_POINT ( 'NONE', #41465 ) ;
#11297 = CIRCLE ( 'NONE', #65423, 7.938172270156617749 ) ;
#11298 = CARTESIAN_POINT ( 'NONE',  ( 16.78263030916553689, 12.17295508002146320, 5.836879698929895888 ) ) ;
#11299 = AXIS2_PLACEMENT_3D ( 'NONE', #63561, #49610, #23346 ) ;
#11300 = ORIENTED_EDGE ( 'NONE', *, *, #12249, .F. ) ;
#11301 = CARTESIAN_POINT ( 'NONE',  ( 12.47628546223243617, 0.000000000000000000, -11.99999999999998224 ) ) ;
#11302 = FACE_OUTER_BOUND ( 'NONE', #22913, .T. ) ;
#11303 = CARTESIAN_POINT ( 'NONE',  ( 37.00000000000000711, 12.63095688309029008, -1.738225594540043772 ) ) ;
#11304 = CARTESIAN_POINT ( 'NONE',  ( 36.00000000000000711, 0.1414404973753900230, 12.74921544981110522 ) ) ;
#11305 = CARTESIAN_POINT ( 'NONE',  ( 2.665405856346790170, -4.274976649834401954, -8.559192023451558384 ) ) ;
#11306 = CYLINDRICAL_SURFACE ( 'NONE', #19647, 13.50000000000000178 ) ;
#11307 = B_SPLINE_CURVE_WITH_KNOTS ( 'NONE', 3,
 ( #17250, #46516, #55264, #36544, #20019, #27219, #56852, #971 ),
 .UNSPECIFIED., .F., .F.,
 ( 4, 2, 2, 4 ),
 ( 0.01146705142166408280, 0.01597709677061664654, 0.01823211944509292928, 0.02048714211956921202 ),
 .UNSPECIFIED. ) ;
#11308 = EDGE_CURVE ( 'NONE', #35397, #25443, #46166, .T. ) ;
#11309 = ORIENTED_EDGE ( 'NONE', *, *, #28671, .F. ) ;
#11310 = FACE_OUTER_BOUND ( 'NONE', #21277, .T. ) ;
#11311 = ORIENTED_EDGE ( 'NONE', *, *, #63633, .F. ) ;
#11312 = CARTESIAN_POINT ( 'NONE',  ( 1.937114397841935398, 8.920887662793472117, 9.228205347192481867 ) ) ;
#11313 = CARTESIAN_POINT ( 'NONE',  ( 4.953976645022760472, -25.99587143922706645, -15.25378271594936841 ) ) ;
#11314 = CARTESIAN_POINT ( 'NONE',  ( 18.04777717444646612, -29.74456712077427412, 8.215504029118749330 ) ) ;
#11315 = DIRECTION ( 'NONE',  ( 0.000000000000000000, -0.01356324068817999114, 0.9999080150203989437 ) ) ;
#11316 = ORIENTED_EDGE ( 'NONE', *, *, #38114, .F. ) ;
#11317 = CARTESIAN_POINT ( 'NONE',  ( -35.00000000000000000, 0.000000000000000000, 0.000000000000000000 ) ) ;
#11318 = LINE ( 'NONE', #37225, #435 ) ;
#11319 = CARTESIAN_POINT ( 'NONE',  ( 21.74395625310401314, 11.95369699707849165, -1.122435266587093139 ) ) ;
#11320 = CARTESIAN_POINT ( 'NONE',  ( 2.899286259009681288, 3.614094927251937595, 6.972741252562068226 ) ) ;
#11321 = ADVANCED_FACE ( 'NONE', ( #21544 ), #612, .T. ) ;
#11322 = CARTESIAN_POINT ( 'NONE',  ( 47.00000000000000711, 4.705694406421931860E-17, -3.469127814946512892E-15 ) ) ;
#11323 = CARTESIAN_POINT ( 'NONE',  ( 2.241506898688419902, 2.648071636522731698, 7.160521809579504016 ) ) ;
#11324 = CARTESIAN_POINT ( 'NONE',  ( 0.8375941296809087389, -5.882592429484210683, -10.95781044612470012 ) ) ;
#11325 = CARTESIAN_POINT ( 'NONE',  ( -22.27384469013076185, -3.663183248998797659, 0.3730095848193237251 ) ) ;
#11326 = CARTESIAN_POINT ( 'NONE',  ( 0.9232058338315058954, 7.723624854284846464, -9.791640253608070665 ) ) ;
#11327 = VECTOR ( 'NONE', #49091, 1000.000000000000227 ) ;
#11328 = ADVANCED_FACE ( 'NONE', ( #284 ), #16217, .F. ) ;
#11329 = AXIS2_PLACEMENT_3D ( 'NONE', #20091, #9778, #59683 ) ;
#11330 = ORIENTED_EDGE ( 'NONE', *, *, #49457, .T. ) ;
#11331 = ORIENTED_EDGE ( 'NONE', *, *, #45730, .T. ) ;
#11332 = DIRECTION ( 'NONE',  ( 1.000000000000000000, -0.000000000000000000, 0.000000000000000000 ) ) ;
#11333 = CARTESIAN_POINT ( 'NONE',  ( 0.2646305136544065406, -9.465888453932908675, -7.770320294339271960 ) ) ;
#11334 = DIRECTION ( 'NONE',  ( 1.000000000000000000, 0.000000000000000000, 0.000000000000000000 ) ) ;
#11335 = DIRECTION ( 'NONE',  ( -1.000000000000000000, 0.000000000000000000, 0.000000000000000000 ) ) ;
#11336 = ORIENTED_EDGE ( 'NONE', *, *, #54192, .T. ) ;
#11337 = EDGE_CURVE ( 'NONE', #54245, #48534, #53716, .T. ) ;
#11338 = ADVANCED_FACE ( 'NONE', ( #20559 ), #62403, .T. ) ;
#11339 = VERTEX_POINT ( 'NONE', #11233 ) ;
#11340 = EDGE_LOOP ( 'NONE', ( #21274, #61112, #23396, #64478 ) ) ;
#11341 = DIRECTION ( 'NONE',  ( 0.000000000000000000, 0.01356324068817992175, -0.9999080150203990547 ) ) ;
#11342 = CARTESIAN_POINT ( 'NONE',  ( 0.3675815128205894289, 1.872154644482245889, -12.13672785388548547 ) ) ;
#11343 = ORIENTED_EDGE ( 'NONE', *, *, #30281, .F. ) ;
#11344 = DIRECTION ( 'NONE',  ( 0.000000000000000000, 0.01356324068817998940, -0.9999080150203990547 ) ) ;
#11345 = DIRECTION ( 'NONE',  ( -1.000000000000000000, -0.000000000000000000, -0.000000000000000000 ) ) ;
#11346 = ORIENTED_EDGE ( 'NONE', *, *, #1936, .T. ) ;
#11347 = CARTESIAN_POINT ( 'NONE',  ( -22.30986928587821794, 0.2539257557460806169, 3.771068405887386898 ) ) ;
#11348 = CARTESIAN_POINT ( 'NONE',  ( 15.82775651593353672, -34.24354600359633594, -7.361827980272592775 ) ) ;
#11349 = CARTESIAN_POINT ( 'NONE',  ( 24.70884604468378498, -2.111405277004652969, 11.81439423874797257 ) ) ;
#11350 = EDGE_LOOP ( 'NONE', ( #309, #13698, #40033, #4175 ) ) ;
#11351 = FACE_OUTER_BOUND ( 'NONE', #50388, .T. ) ;
#11352 = ORIENTED_EDGE ( 'NONE', *, *, #50230, .F. ) ;
#11353 = CARTESIAN_POINT ( 'NONE',  ( 0.4613984246114869459, 7.694922453052268629, -9.610550265395774616 ) ) ;
#11354 = CARTESIAN_POINT ( 'NONE',  ( 0.000000000000000000, 2.473437528934141483, 7.080403010454977775 ) ) ;
#11355 = CARTESIAN_POINT ( 'NONE',  ( -13.53218314550735357, -34.21215502346591819, 9.055742533985885245 ) ) ;
#11356 = DIRECTION ( 'NONE',  ( 1.000000000000000000, 0.000000000000000000, 0.000000000000000000 ) ) ;
#11357 = CARTESIAN_POINT ( 'NONE',  ( 5.515539859299206427, -0.005924322247674730646, -0.001241880655086653002 ) ) ;
#11358 = CARTESIAN_POINT ( 'NONE',  ( 35.00000000000000000, 9.621072037176993774, -8.366449238204399563 ) ) ;
#11359 = CARTESIAN_POINT ( 'NONE',  ( 1.020182472824531672, 6.631405022220766554, -10.59341968305531623 ) ) ;
#11360 = CARTESIAN_POINT ( 'NONE',  ( 47.00000000000000711, 4.705694406421931860E-17, -3.469127814946512892E-15 ) ) ;
#11361 = ORIENTED_EDGE ( 'NONE', *, *, #1424, .T. ) ;
#11362 = DIRECTION ( 'NONE',  ( -1.000000000000000000, 0.000000000000000000, 0.000000000000000000 ) ) ;
#11363 = EDGE_LOOP ( 'NONE', ( #52916, #16375, #28528, #54466 ) ) ;
#11364 = CIRCLE ( 'NONE', #24137, 12.75000000000000178 ) ;
#11365 = CARTESIAN_POINT ( 'NONE',  ( 0.9232058338315058954, -1.793035206307428853, 12.34162163148533153 ) ) ;
#11366 = CARTESIAN_POINT ( 'NONE',  ( 35.00000000000000000, -2.216820770815006725, 11.53507381115585417 ) ) ;
#11368 = VERTEX_POINT ( 'NONE', #17854 ) ;
#11367 = ADVANCED_FACE ( 'NONE', ( #36146 ), #56455, .T. ) ;
#11369 = CARTESIAN_POINT ( 'NONE',  ( -18.43818118241833659, 6.164186468232681904, 10.29965514685089367 ) ) ;
#11370 = CYLINDRICAL_SURFACE ( 'NONE', #56335, 7.011478057721953761 ) ;
#11371 = DIRECTION ( 'NONE',  ( 1.000000000000000000, 0.000000000000000000, 0.000000000000000000 ) ) ;
#11372 = CIRCLE ( 'NONE', #41116, 12.18650000000000055 ) ;
#11373 = CARTESIAN_POINT ( 'NONE',  ( -22.70624764888619751, 2.702761586319180509, -4.501516772829864621 ) ) ;
#11374 = EDGE_CURVE ( 'NONE', #61765, #48935, #52781, .T. ) ;
#11375 = DIRECTION ( 'NONE',  ( 0.000000000000000000, 0.000000000000000000, -1.000000000000000000 ) ) ;
#11376 = VERTEX_POINT ( 'NONE', #32793 ) ;
#11377 = AXIS2_PLACEMENT_3D ( 'NONE', #56923, #1049, #5384 ) ;
#11378 = CARTESIAN_POINT ( 'NONE',  ( -17.34002536255959015, -6.190470376513365736, -10.28142836167298135 ) ) ;
#11379 = EDGE_LOOP ( 'NONE', ( #53958, #41932, #9944, #26194 ) ) ;
#11380 = CARTESIAN_POINT ( 'NONE',  ( 0.000000000000000000, -4.604744433234619017, -5.919993978425545755 ) ) ;
#11381 = DIRECTION ( 'NONE',  ( 1.000000000000000000, 0.000000000000000000, -0.000000000000000000 ) ) ;
#11382 = FACE_OUTER_BOUND ( 'NONE', #25042, .T. ) ;
#11383 = VERTEX_POINT ( 'NONE', #64054 ) ;
#11384 = CYLINDRICAL_SURFACE ( 'NONE', #25542, 2.899999999999994582 ) ;
#11385 = EDGE_CURVE ( 'NONE', #50140, #34717, #47362, .T. ) ;
#11386 = EDGE_CURVE ( 'NONE', #16455, #40131, #20348, .T. ) ;
#11387 = CARTESIAN_POINT ( 'NONE',  ( 26.77130308255667401, 12.82903357082578921, 4.213245553477073635 ) ) ;
#11388 = CARTESIAN_POINT ( 'NONE',  ( -15.27729454824424948, 5.151216734910788908, 25.00000000000000000 ) ) ;
#11389 = LINE ( 'NONE', #460, #2356 ) ;
#11390 = CYLINDRICAL_SURFACE ( 'NONE', #37030, 4.999999999999999112 ) ;
#11391 = EDGE_CURVE ( 'NONE', #31684, #41765, #47789, .T. ) ;
#11392 = DIRECTION ( 'NONE',  ( 0.000000000000000000, -0.01356324068817991828, 0.9999080150203990547 ) ) ;
#11393 = CARTESIAN_POINT ( 'NONE',  ( 0.9232167919969077596, 4.649596781010405522, 11.56588005394299934 ) ) ;
#11394 = CARTESIAN_POINT ( 'NONE',  ( 0.000000000000000000, -3.155844197800145690, 6.177028383390419819 ) ) ;
#11395 = AXIS2_PLACEMENT_3D ( 'NONE', #26648, #16994, #42242 ) ;
#11396 = EDGE_CURVE ( 'NONE', #51437, #11726, #19591, .T. ) ;
#11397 = ORIENTED_EDGE ( 'NONE', *, *, #40669, .F. ) ;
#11398 = CARTESIAN_POINT ( 'NONE',  ( 6.812204945636112896, -4.138731716409435712, 25.00000000000000000 ) ) ;
#11399 = CARTESIAN_POINT ( 'NONE',  ( 0.3160775863651104634, -12.26075464248083868, -0.2401734240704150591 ) ) ;
#11400 = ORIENTED_EDGE ( 'NONE', *, *, #19514, .T. ) ;
#11401 = CARTESIAN_POINT ( 'NONE',  ( 1.287602823384993878, 10.61402828236296436, 6.765713844064224602 ) ) ;
#11402 = EDGE_CURVE ( 'NONE', #53826, #25430, #59091, .T. ) ;
#11403 = CARTESIAN_POINT ( 'NONE',  ( 1.299397328467618129, 1.108794299602723132, -11.95234461178691276 ) ) ;
#11404 = DIRECTION ( 'NONE',  ( -1.000000000000000000, -0.000000000000000000, -0.000000000000000000 ) ) ;
#11405 = ORIENTED_EDGE ( 'NONE', *, *, #38538, .F. ) ;
#11406 = CARTESIAN_POINT ( 'NONE',  ( -35.00000000000000000, 11.95840593935201213, 2.346765782874477679 ) ) ;
#11407 = VERTEX_POINT ( 'NONE', #28167 ) ;
#11408 = DIRECTION ( 'NONE',  ( 0.000000000000000000, 0.9987865678893278476, -0.04924826701374234589 ) ) ;
#11409 = EDGE_LOOP ( 'NONE', ( #18806, #41643, #27731, #2081 ) ) ;
#11410 = AXIS2_PLACEMENT_3D ( 'NONE', #34506, #54807, #9226 ) ;
#11411 = VERTEX_POINT ( 'NONE', #33783 ) ;
#11412 = CARTESIAN_POINT ( 'NONE',  ( 2.941278708680199916, 1.972702289976081991, -5.814102272488566925 ) ) ;
#11413 = AXIS2_PLACEMENT_3D ( 'NONE', #9451, #15752, #36032 ) ;
#11414 = ORIENTED_EDGE ( 'NONE', *, *, #32713, .T. ) ;
#11415 = ADVANCED_FACE ( 'NONE', ( #54085 ), #22522, .T. ) ;
#11416 = CARTESIAN_POINT ( 'NONE',  ( -25.54554785668764438, -5.744669996086663843, 10.54128946422876290 ) ) ;
#11417 = CARTESIAN_POINT ( 'NONE',  ( -22.27706089016750113, -3.562910635974989138, 0.9256273512588475416 ) ) ;
#11418 = DIRECTION ( 'NONE',  ( 0.000000000000000000, -0.4198891015602529420, -0.9075754196709625576 ) ) ;
#11419 = DIRECTION ( 'NONE',  ( -1.000000000000000000, 0.000000000000000000, -0.000000000000000000 ) ) ;
#11420 = ORIENTED_EDGE ( 'NONE', *, *, #9927, .T. ) ;
#11421 = CYLINDRICAL_SURFACE ( 'NONE', #38525, 6.511478057721953761 ) ;
#11422 = CARTESIAN_POINT ( 'NONE',  ( 11.58535936493820273, -27.13779202276463920, 13.20710129366601926 ) ) ;
#11423 = CARTESIAN_POINT ( 'NONE',  ( 5.536195898058073439, -0.008411485181669250619, -0.001224473329857952162 ) ) ;
#11425 = VERTEX_POINT ( 'NONE', #38118 ) ;
#11424 = CARTESIAN_POINT ( 'NONE',  ( 2.000000000000001776, 0.000000000000000000, 0.000000000000000000 ) ) ;
#11426 = CYLINDRICAL_SURFACE ( 'NONE', #44759, 5.000000000000000888 ) ;
#11427 = B_SPLINE_CURVE_WITH_KNOTS ( 'NONE', 3,
 ( #65474, #46213, #10601, #30885, #9615, #29912, #655 ),
 .UNSPECIFIED., .F., .F.,
 ( 4, 3, 4 ),
 ( 3.660687858773823404E-18, 0.002398160485434294199, 0.005002426799376703641 ),
 .UNSPECIFIED. ) ;
#11428 = VERTEX_POINT ( 'NONE', #8518 ) ;
#11429 = CARTESIAN_POINT ( 'NONE',  ( -37.00000000000000711, 0.000000000000000000, 0.000000000000000000 ) ) ;
#11430 = ORIENTED_EDGE ( 'NONE', *, *, #7984, .F. ) ;
#11431 = CARTESIAN_POINT ( 'NONE',  ( 42.50000000000000000, 1.443454975684918283E-16, -1.399999999999999911 ) ) ;
#11432 = CARTESIAN_POINT ( 'NONE',  ( 47.00000000000000711, 4.705694406421931860E-17, -3.469127814946512892E-15 ) ) ;
#11433 = CARTESIAN_POINT ( 'NONE',  ( 2.276198483117257698, -7.644465698238554374, -0.1540629821339100092 ) ) ;
#11434 = ORIENTED_EDGE ( 'NONE', *, *, #16204, .T. ) ;
#11435 = CARTESIAN_POINT ( 'NONE',  ( 0.9232167919969117564, 8.324955738482477940, 9.278116382137406859 ) ) ;
#11436 = DIRECTION ( 'NONE',  ( 0.000000000000000000, 0.04924826701374598187, 0.9987865678893278476 ) ) ;
#11437 = CARTESIAN_POINT ( 'NONE',  ( 0.3040950598368144520, -11.60568999039897875, 3.956873563689492279 ) ) ;
#11438 = ORIENTED_EDGE ( 'NONE', *, *, #24628, .T. ) ;
#11439 =( BOUNDED_SURFACE ( )  B_SPLINE_SURFACE ( 3, 1, ( 
 ( #13435, #33718 ),
 ( #37733, #43360 ),
 ( #28405, #22784 ),
 ( #63315, #17782 ) ),
 .UNSPECIFIED., .F., .F., .F. ) 
 B_SPLINE_SURFACE_WITH_KNOTS ( ( 4, 4 ),
 ( 2, 2 ),
 ( 0.000000000000000000, 1.000000000000000000 ),
 ( 0.000000000000000000, 1.000000000000000000 ),
 .UNSPECIFIED. ) 
 GEOMETRIC_REPRESENTATION_ITEM ( )  RATIONAL_B_SPLINE_SURFACE ( (
 ( 1.000000000000000000, 1.000000000000000000),
 ( 0.9257577194822556033, 0.9980522942447415113),
 ( 0.9257577194822556033, 0.9980522942447415113),
 ( 1.000000000000000000, 1.000000000000000000) ) ) 
 REPRESENTATION_ITEM ( '' )  SURFACE ( )  );
#11440 = ORIENTED_EDGE ( 'NONE', *, *, #37222, .T. ) ;
#11441 = CARTESIAN_POINT ( 'NONE',  ( 35.00000000000000000, -4.725891942574827809, -10.75351884295726101 ) ) ;
#11442 = ORIENTED_EDGE ( 'NONE', *, *, #60204, .F. ) ;
#11443 = ORIENTED_EDGE ( 'NONE', *, *, #27126, .F. ) ;
#11444 = DIRECTION ( 'NONE',  ( 0.000000000000000000, 0.01356324068817998940, -0.9999080150203990547 ) ) ;
#11445 = CARTESIAN_POINT ( 'NONE',  ( 2.000000000000001776, 6.812627895098307462, 0.04423456934733380197 ) ) ;
#11446 = LINE ( 'NONE', #31719, #11759 ) ;
#11447 = CARTESIAN_POINT ( 'NONE',  ( -22.28546858134833286, 1.005093225210857977, 3.567529619157783660 ) ) ;
#11448 = CARTESIAN_POINT ( 'NONE',  ( 0.2646305136544065406, -6.237419468587005689, -10.53923716745253003 ) ) ;
#11449 = CIRCLE ( 'NONE', #1917, 12.18649999999999878 ) ;
#11450 = EDGE_CURVE ( 'NONE', #30305, #12197, #18278, .T. ) ;
#11451 = DIRECTION ( 'NONE',  ( -1.000000000000000000, 0.000000000000000000, 0.000000000000000000 ) ) ;
#11452 = DIRECTION ( 'NONE',  ( 0.000000000000000000, 0.01356324068817998940, -0.9999080150203990547 ) ) ;
#11453 = CIRCLE ( 'NONE', #28446, 12.18649999999999700 ) ;
#11454 =( BOUNDED_SURFACE ( )  B_SPLINE_SURFACE ( 3, 1, ( 
 ( #57495, #52823 ),
 ( #6950, #22571 ),
 ( #22904, #1955 ),
 ( #63124, #42487 ) ),
 .UNSPECIFIED., .F., .F., .F. ) 
 B_SPLINE_SURFACE_WITH_KNOTS ( ( 4, 4 ),
 ( 2, 2 ),
 ( 0.000000000000000000, 1.000000000000000000 ),
 ( 0.000000000000000000, 1.000000000000000000 ),
 .UNSPECIFIED. ) 
 GEOMETRIC_REPRESENTATION_ITEM ( )  RATIONAL_B_SPLINE_SURFACE ( (
 ( 1.000000000000000000, 1.000000000000000000),
 ( 0.6933888150995267674, 0.9895912004443193632),
 ( 0.6933888150995267674, 0.9895912004443193632),
 ( 1.000000000000000000, 1.000000000000000000) ) ) 
 REPRESENTATION_ITEM ( '' )  SURFACE ( )  );
#11455 = ORIENTED_EDGE ( 'NONE', *, *, #59667, .T. ) ;
#11456 = DIRECTION ( 'NONE',  ( 0.000000000000000000, 0.000000000000000000, -1.000000000000000000 ) ) ;
#11457 = CARTESIAN_POINT ( 'NONE',  ( 37.00000000000000711, 11.35427606708806003, -4.426194442447284771 ) ) ;
#11458 = EDGE_CURVE ( 'NONE', #34717, #28861, #65229, .T. ) ;
#11459 = CARTESIAN_POINT ( 'NONE',  ( 5.530133899448235191, 0.009387834778845326189, 0.01293763278443411935 ) ) ;
#11460 = CARTESIAN_POINT ( 'NONE',  ( 0.2651627923886318294, 12.07509237025073645, -2.039714259676051800 ) ) ;
#11461 = ADVANCED_FACE ( 'NONE', ( #63387 ), #45063, .F. ) ;
#11462 = CARTESIAN_POINT ( 'NONE',  ( 0.3675815128205894289, 2.391755495700764289, -12.04510820461657161 ) ) ;
#11463 = CARTESIAN_POINT ( 'NONE',  ( -22.27384469013076185, 2.581192766446265274, 2.625926801827853208 ) ) ;
#11464 = EDGE_CURVE ( 'NONE', #61567, #35169, #8206, .T. ) ;
#11465 = ORIENTED_EDGE ( 'NONE', *, *, #17683, .F. ) ;
#11466 = CARTESIAN_POINT ( 'NONE',  ( 2.000000000000001776, 0.000000000000000000, 0.000000000000000000 ) ) ;
#11467 = CARTESIAN_POINT ( 'NONE',  ( -35.00000000000000000, 11.47758908105694786, 2.497432891016883261 ) ) ;
#11468 = CARTESIAN_POINT ( 'NONE',  ( -19.47984447937493613, -1.416020129149132334, 25.00000000000000000 ) ) ;
#11469 = CARTESIAN_POINT ( 'NONE',  ( 35.00000000000000000, 4.705694406421931860E-17, -3.469127814946512892E-15 ) ) ;
#11470 = CARTESIAN_POINT ( 'NONE',  ( 10.10599715024921963, 1.639952862261359501, -13.40131696041721909 ) ) ;
#11471 = CARTESIAN_POINT ( 'NONE',  ( 5.530133899448235191, -0.01437126147332039479, 0.006998616117863549688 ) ) ;
#11472 = ORIENTED_EDGE ( 'NONE', *, *, #48508, .T. ) ;
#11473 = AXIS2_PLACEMENT_3D ( 'NONE', #50062, #4520, #33457 ) ;
#11474 = LINE ( 'NONE', #4878, #48257 ) ;
#11475 = LINE ( 'NONE', #26781, #52464 ) ;
#11476 = EDGE_CURVE ( 'NONE', #14758, #44370, #14152, .T. ) ;
#11477 = CARTESIAN_POINT ( 'NONE',  ( -22.51237073810381162, -0.9543406717316460508, 4.319597983500818472 ) ) ;
#11478 = ORIENTED_EDGE ( 'NONE', *, *, #12834, .T. ) ;
#11479 = CARTESIAN_POINT ( 'NONE',  ( 0.2648978790185593790, 4.063980959785203240, -11.55204314799259890 ) ) ;
#11480 = CARTESIAN_POINT ( 'NONE',  ( 35.00000000000000000, -0.01609748574436820068, 11.74614673114903596 ) ) ;
#11481 = CARTESIAN_POINT ( 'NONE',  ( 0.2646305136544072623, -10.53923716745242700, -6.237419468587187765 ) ) ;
#11482 = EDGE_CURVE ( 'NONE', #21985, #36221, #59236, .T. ) ;
#11484 = EDGE_LOOP ( 'NONE', ( #55180, #30582, #22314, #37029 ) ) ;
#11483 = CARTESIAN_POINT ( 'NONE',  ( 35.00000000000000000, 4.705694406421931860E-17, -3.469127814946512892E-15 ) ) ;
#11485 = CARTESIAN_POINT ( 'NONE',  ( 37.00000000000000711, -5.428340790341627198, 10.91072401419415883 ) ) ;
#11486 = ADVANCED_FACE ( 'NONE', ( #49449 ), #19819, .T. ) ;
#11487 = AXIS2_PLACEMENT_3D ( 'NONE', #45149, #65408, #19875 ) ;
#11488 = DIRECTION ( 'NONE',  ( -1.000000000000000000, 0.000000000000000000, 0.000000000000000000 ) ) ;
#11489 = ORIENTED_EDGE ( 'NONE', *, *, #14063, .T. ) ;
#11490 = EDGE_CURVE ( 'NONE', #63372, #7682, #55055, .T. ) ;
#11491 = CYLINDRICAL_SURFACE ( 'NONE', #4721, 12.75000000000000178 ) ;
#11492 = CARTESIAN_POINT ( 'NONE',  ( 0.3665391374699472626, -5.911453292029678508, 10.76665847464310843 ) ) ;
#11493 = AXIS2_PLACEMENT_3D ( 'NONE', #59252, #65209, #64860 ) ;
#11494 = CARTESIAN_POINT ( 'NONE',  ( 24.20270661733482953, 0.6951122250270121983, -11.98503915607300208 ) ) ;
#11495 = VECTOR ( 'NONE', #35382, 1000.000000000000000 ) ;
#11496 = CARTESIAN_POINT ( 'NONE',  ( -17.05023968204110929, -34.50000000000000000, 4.356789313881321846 ) ) ;
#11497 = DIRECTION ( 'NONE',  ( 1.000000000000000000, -0.000000000000000000, 0.000000000000000000 ) ) ;
#11498 = EDGE_CURVE ( 'NONE', #53160, #21602, #20537, .T. ) ;
#11499 = DIRECTION ( 'NONE',  ( 0.000000000000000000, 0.6745969609292663538, 0.7381862504171952111 ) ) ;
#11501 = ORIENTED_EDGE ( 'NONE', *, *, #3810, .T. ) ;
#11500 = CARTESIAN_POINT ( 'NONE',  ( 5.514624014163232779, -0.003060352188290796274, -0.002789935220458035839 ) ) ;
#11502 = AXIS2_PLACEMENT_3D ( 'NONE', #24963, #24625, #39588 ) ;
#11503 = EDGE_LOOP ( 'NONE', ( #49978, #4082, #63642, #29431 ) ) ;
#11504 = CARTESIAN_POINT ( 'NONE',  ( 2.000000000000001776, 5.997115278587632936, 3.485633455389514523 ) ) ;
#11505 = VERTEX_POINT ( 'NONE', #28808 ) ;
#11506 = VECTOR ( 'NONE', #46788, 1000.000000000000114 ) ;
#11507 = CARTESIAN_POINT ( 'NONE',  ( 0.000000000000000000, 0.000000000000000000, 0.000000000000000000 ) ) ;
#11508 = CARTESIAN_POINT ( 'NONE',  ( 37.00000000000000711, 6.265926637539651622, 11.10408318471052347 ) ) ;
#11509 = CARTESIAN_POINT ( 'NONE',  ( 1.452237505248552996, -10.06489946308207095, 7.672309600508662619 ) ) ;
#11510 = DIRECTION ( 'NONE',  ( -1.000000000000000000, 0.000000000000000000, 0.000000000000000000 ) ) ;
#11511 = ORIENTED_EDGE ( 'NONE', *, *, #3144, .T. ) ;
#11512 = DIRECTION ( 'NONE',  ( -1.000000000000000000, 0.000000000000000000, -0.000000000000000000 ) ) ;
#11513 = CYLINDRICAL_SURFACE ( 'NONE', #26192, 7.499999999999988454 ) ;
#11514 = FACE_BOUND ( 'NONE', #28244, .T. ) ;
#11515 = ORIENTED_EDGE ( 'NONE', *, *, #48571, .F. ) ;
#11516 = VERTEX_POINT ( 'NONE', #9170 ) ;
#11517 = CARTESIAN_POINT ( 'NONE',  ( 3.092491956585539103, 7.707758057368735649, -1.813286239165393665 ) ) ;
#11518 = ORIENTED_EDGE ( 'NONE', *, *, #45855, .T. ) ;
#11519 = CARTESIAN_POINT ( 'NONE',  ( 2.241536586108911600, 1.319514354261297484, -7.519576125149795232 ) ) ;
#11520 = LINE ( 'NONE', #41785, #35248 ) ;
#11521 = LINE ( 'NONE', #52102, #53291 ) ;
#11522 = DIRECTION ( 'NONE',  ( 0.000000000000000000, 0.01356324068817998940, -0.9999080150203990547 ) ) ;
#11523 = EDGE_CURVE ( 'NONE', #46786, #60151, #50265, .T. ) ;
#11524 = CARTESIAN_POINT ( 'NONE',  ( 2.931247277082686065, -7.800615791174664082, 0.9994150891046047480 ) ) ;
#11525 = AXIS2_PLACEMENT_3D ( 'NONE', #8607, #33562, #38544 ) ;
#11526 = DIRECTION ( 'NONE',  ( 1.000000000000000000, 0.000000000000000000, 0.000000000000000000 ) ) ;
#11527 = ORIENTED_EDGE ( 'NONE', *, *, #35566, .F. ) ;
#11528 = DIRECTION ( 'NONE',  ( 1.000000000000000000, 0.000000000000000000, 0.000000000000000000 ) ) ;
#11529 = AXIS2_PLACEMENT_3D ( 'NONE', #43018, #52027, #48024 ) ;
#11530 = ORIENTED_EDGE ( 'NONE', *, *, #21895, .T. ) ;
#11531 = DIRECTION ( 'NONE',  ( 1.000000000000000000, 0.000000000000000000, -0.000000000000000000 ) ) ;
#11532 = CARTESIAN_POINT ( 'NONE',  ( 35.00000000000000000, 7.474872387601131152, 9.060822531525964507 ) ) ;
#11533 = DIRECTION ( 'NONE',  ( 0.000000000000000000, -0.01356324068817998940, 0.9999080150203990547 ) ) ;
#11534 = DIRECTION ( 'NONE',  ( 1.000000000000000000, 0.000000000000000000, -0.000000000000000000 ) ) ;
#11535 = DIRECTION ( 'NONE',  ( 0.000000000000000000, 0.000000000000000000, 1.000000000000000000 ) ) ;
#11536 = EDGE_CURVE ( 'NONE', #62548, #33917, #27940, .T. ) ;
#11537 = CARTESIAN_POINT ( 'NONE',  ( -37.00000000000000711, -11.78745411414837818, -3.093009498344053032 ) ) ;
#11538 = AXIS2_PLACEMENT_3D ( 'NONE', #33341, #59850, #4659 ) ;
#11539 = ORIENTED_EDGE ( 'NONE', *, *, #28810, .F. ) ;
#11540 = ORIENTED_EDGE ( 'NONE', *, *, #58947, .T. ) ;
#11541 = EDGE_CURVE ( 'NONE', #46746, #43998, #19497, .T. ) ;
#11542 = CARTESIAN_POINT ( 'NONE',  ( -27.10422407540562517, 0.1544383239736529800, 2.346206748218693239 ) ) ;
#11543 = B_SPLINE_CURVE_WITH_KNOTS ( 'NONE', 3,
 ( #24449, #65012, #30429, #14464, #40393, #9471, #30103, #65656, #12709, #48648, #29016, #23362, #23707, #2785, #32994, #63919, #3770, #58968, #53956, #19032, #18397, #33664 ),
 .UNSPECIFIED., .F., .F.,
 ( 4, 2, 2, 2, 2, 2, 2, 2, 2, 2, 4 ),
 ( 0.000000000000000000, 0.001345449967898921465, 0.002018174951848381981, 0.002690899935797842930, 0.004036349903696756156, 0.004709074887646215804, 0.005381799871595674585, 0.006727249839494598219, 0.008072699807393519250, 0.009418149775292443751, 0.01076359974319136478 ),
 .UNSPECIFIED. ) ;
#11544 = CIRCLE ( 'NONE', #47541, 2.899999999999996358 ) ;
#11545 = ORIENTED_EDGE ( 'NONE', *, *, #61493, .F. ) ;
#11546 = CARTESIAN_POINT ( 'NONE',  ( -35.00000000000000000, -6.917234959366895808, 9.493370459201672773 ) ) ;
#11547 = DIRECTION ( 'NONE',  ( -1.000000000000000000, 0.000000000000000000, 0.000000000000000000 ) ) ;
#11548 = CIRCLE ( 'NONE', #40211, 4.999999999999998224 ) ;
#11549 = CARTESIAN_POINT ( 'NONE',  ( 2.261269890822091622, 4.803890999604312206, 5.942064862945645842 ) ) ;
#11550 = CARTESIAN_POINT ( 'NONE',  ( 0.2652384529303136174, -0.06607367983845134629, -12.24598125395191772 ) ) ;
#11551 = ADVANCED_FACE ( 'NONE', ( #24809 ), #45092, .T. ) ;
#11552 = ORIENTED_EDGE ( 'NONE', *, *, #54959, .T. ) ;
#11553 = CARTESIAN_POINT ( 'NONE',  ( 34.00000000000000000, -14.99999999999997513, 0.000000000000000000 ) ) ;
#11554 = DIRECTION ( 'NONE',  ( 0.3939253465568943735, 0.5982248387291241309, -0.6978179301705739190 ) ) ;
#11555 = DIRECTION ( 'NONE',  ( 0.000000000000000000, -0.9985334138511243740, 0.05413890858540768014 ) ) ;
#11556 = AXIS2_PLACEMENT_3D ( 'NONE', #65349, #40070, #35416 ) ;
#11557 = CARTESIAN_POINT ( 'NONE',  ( -46.63605190621407814, -0.6629852496305224108, 12.55202432522572664 ) ) ;
#11558 = CYLINDRICAL_SURFACE ( 'NONE', #56433, 5.000000000000000888 ) ;
#11559 = CARTESIAN_POINT ( 'NONE',  ( 2.266490820343225465, 2.750080098241514115, 7.130860233521858049 ) ) ;
#11560 = VERTEX_POINT ( 'NONE', #40080 ) ;
#11561 = CARTESIAN_POINT ( 'NONE',  ( -15.98984497772178770, -34.99999999818471963, -5.008554314762531767 ) ) ;
#11562 = ORIENTED_EDGE ( 'NONE', *, *, #59559, .F. ) ;
#11563 = DIRECTION ( 'NONE',  ( -1.000000000000000000, 0.000000000000000000, 0.000000000000000000 ) ) ;
#11564 = FACE_OUTER_BOUND ( 'NONE', #44710, .T. ) ;
#11565 = CARTESIAN_POINT ( 'NONE',  ( -37.00000000000000711, 9.926225166347114381, -6.280308599560036065 ) ) ;
#11566 = CARTESIAN_POINT ( 'NONE',  ( -22.28506771379528573, -1.050362426369332303, -3.575989816848478942 ) ) ;
#11567 = CARTESIAN_POINT ( 'NONE',  ( -9.480571072184686088, -3.591719512060966402, 11.45094271422924415 ) ) ;
#11568 = EDGE_CURVE ( 'NONE', #10423, #9409, #3570, .T. ) ;
#11569 = CIRCLE ( 'NONE', #34905, 5.000000000000000000 ) ;
#11570 = ORIENTED_EDGE ( 'NONE', *, *, #178, .T. ) ;
#11571 = EDGE_LOOP ( 'NONE', ( #57072, #57301, #51841, #14954, #43242, #9353 ) ) ;
#11572 = CARTESIAN_POINT ( 'NONE',  ( -30.14922989771758566, -0.5076506010579284744, 11.99141041789170892 ) ) ;
#11573 = EDGE_CURVE ( 'NONE', #16668, #41187, #7775, .T. ) ;
#11574 = ORIENTED_EDGE ( 'NONE', *, *, #21521, .T. ) ;
#11575 = CARTESIAN_POINT ( 'NONE',  ( 3.441315431463302765, 6.040220126836617354, 10.37118595071527594 ) ) ;
#11576 = CARTESIAN_POINT ( 'NONE',  ( 0.2648978790185619880, -10.53870023327867855, 6.237101853238509186 ) ) ;
#11577 = DIRECTION ( 'NONE',  ( 0.000000000000000000, 0.4698238015817302604, 0.8827602140260348840 ) ) ;
#11578 = DIRECTION ( 'NONE',  ( -1.000000000000000000, -0.000000000000000000, -0.000000000000000000 ) ) ;
#11580 = CARTESIAN_POINT ( 'NONE',  ( 2.556980015511752136, 7.736177238086046515, -0.2307166419790108725 ) ) ;
#11579 = VECTOR ( 'NONE', #7116, 1000.000000000000000 ) ;
#11581 = EDGE_CURVE ( 'NONE', #17960, #61044, #4543, .T. ) ;
#11582 = DIRECTION ( 'NONE',  ( 1.000000000000000000, 0.000000000000000000, 0.000000000000000000 ) ) ;
#11583 = CARTESIAN_POINT ( 'NONE',  ( -6.748373723087907727, -1.202078537604638342, 11.93986841932145104 ) ) ;
#11584 = VERTEX_POINT ( 'NONE', #39103 ) ;
#11585 = CARTESIAN_POINT ( 'NONE',  ( -27.20102706715913499, 0.8206313329276082591, 2.512061365242583388 ) ) ;
#11586 = VERTEX_POINT ( 'NONE', #4197 ) ;
#11587 = LINE ( 'NONE', #65237, #523 ) ;
#11588 = VECTOR ( 'NONE', #22080, 1000.000000000000000 ) ;
#11589 = CARTESIAN_POINT ( 'NONE',  ( -47.00000000000000711, 0.000000000000000000, 0.000000000000000000 ) ) ;
#11590 = FACE_OUTER_BOUND ( 'NONE', #9657, .T. ) ;
#11591 = CARTESIAN_POINT ( 'NONE',  ( 37.00000000000000711, 10.23119532541072552, -7.608228585767763619 ) ) ;
#11593 = ORIENTED_EDGE ( 'NONE', *, *, #43608, .F. ) ;
#11592 = AXIS2_PLACEMENT_3D ( 'NONE', #29542, #8958, #19263 ) ;
#11594 = DIRECTION ( 'NONE',  ( 0.000000000000000000, -0.4380125133593850140, 0.8989688749565217796 ) ) ;
#11595 = CARTESIAN_POINT ( 'NONE',  ( -19.30028543097103366, -30.00000000000000355, -5.909123879098586052 ) ) ;
#11596 = CARTESIAN_POINT ( 'NONE',  ( 35.00000000000000000, -10.43555801961471552, 5.391785509271064925 ) ) ;
#11597 = ORIENTED_EDGE ( 'NONE', *, *, #16087, .F. ) ;
#11598 = ORIENTED_EDGE ( 'NONE', *, *, #61393, .F. ) ;
#11599 = DIRECTION ( 'NONE',  ( -1.000000000000000000, -0.000000000000000000, 0.000000000000000000 ) ) ;
#11600 = ORIENTED_EDGE ( 'NONE', *, *, #44574, .F. ) ;
#11601 = ORIENTED_EDGE ( 'NONE', *, *, #47085, .F. ) ;
#11602 = B_SPLINE_CURVE_WITH_KNOTS ( 'NONE', 3,
 ( #34474, #54455, #9193, #49470, #24168, #3257, #44433, #24836, #19182, #65052, #39454, #19528, #59757, #55081, #4224, #14185 ),
 .UNSPECIFIED., .F., .F.,
 ( 4, 3, 3, 3, 3, 4 ),
 ( 1.946286347258496500E-18, 0.0003017745587525237291, 0.0006035491769808725478, 0.0009053241094668148387, 0.001207275924542836228, 0.001510325902538653484 ),
 .UNSPECIFIED. ) ;
#11603 = VERTEX_POINT ( 'NONE', #34449 ) ;
#11604 = AXIS2_PLACEMENT_3D ( 'NONE', #62561, #32314, #47312 ) ;
#11605 = ORIENTED_EDGE ( 'NONE', *, *, #22826, .T. ) ;
#11606 = CARTESIAN_POINT ( 'NONE',  ( 0.3109076770649015220, 4.414555973477820139, 11.43910935267333784 ) ) ;
#11607 = FACE_OUTER_BOUND ( 'NONE', #4558, .T. ) ;
#11608 = ADVANCED_FACE ( 'NONE', ( #39767 ), #60710, .T. ) ;
#11609 = FACE_OUTER_BOUND ( 'NONE', #37259, .T. ) ;
#11610 = LINE ( 'NONE', #31880, #12830 ) ;
#11611 = CARTESIAN_POINT ( 'NONE',  ( 37.00000000000000711, 4.705694406421931860E-17, -3.469127814946512892E-15 ) ) ;
#11612 = ORIENTED_EDGE ( 'NONE', *, *, #38461, .T. ) ;
#11613 = CARTESIAN_POINT ( 'NONE',  ( -37.00000000000000711, 0.000000000000000000, 0.000000000000000000 ) ) ;
#11614 = EDGE_CURVE ( 'NONE', #43541, #9242, #54428, .T. ) ;
#11615 = ORIENTED_EDGE ( 'NONE', *, *, #40699, .T. ) ;
#11616 = CARTESIAN_POINT ( 'NONE',  ( -10.79842706929647989, -9.842369975612385247, -9.240427863961665267 ) ) ;
#11617 = CARTESIAN_POINT ( 'NONE',  ( 2.705197763288458734, 4.789125516644123337, 6.142723737672358908 ) ) ;
#11618 = CARTESIAN_POINT ( 'NONE',  ( 2.257661810676945713, 3.702552158175147046, -6.682681612748679889 ) ) ;
#11619 = CARTESIAN_POINT ( 'NONE',  ( 0.2834382757448010715, -8.029794915379490305, -9.254160138069030594 ) ) ;
#11620 = CARTESIAN_POINT ( 'NONE',  ( 0.2638984909335720941, 11.57533005135178783, 4.001111175853780288 ) ) ;
#11621 = FACE_OUTER_BOUND ( 'NONE', #54711, .T. ) ;
#11622 = EDGE_CURVE ( 'NONE', #57938, #50060, #29150, .T. ) ;
#11623 = CIRCLE ( 'NONE', #23310, 12.75000000000000178 ) ;
#11624 = ORIENTED_EDGE ( 'NONE', *, *, #63552, .T. ) ;
#11625 = DIRECTION ( 'NONE',  ( 0.000000000000000000, 0.000000000000000000, -1.000000000000000000 ) ) ;
#11626 = AXIS2_PLACEMENT_3D ( 'NONE', #21350, #7355, #27312 ) ;
#11627 = ORIENTED_EDGE ( 'NONE', *, *, #48794, .T. ) ;
#11628 = CARTESIAN_POINT ( 'NONE',  ( -35.00000000000000000, 12.63095688309031495, -1.738225594539862584 ) ) ;
#11629 = CARTESIAN_POINT ( 'NONE',  ( 1.989990211274500043, -25.75944405492161948, -15.61385975544041216 ) ) ;
#11630 = LINE ( 'NONE', #52555, #54759 ) ;
#11631 = DIRECTION ( 'NONE',  ( -1.000000000000000000, 0.000000000000000000, 0.000000000000000000 ) ) ;
#11632 = CARTESIAN_POINT ( 'NONE',  ( 2.000000000000001776, 0.000000000000000000, 0.000000000000000000 ) ) ;
#11633 = EDGE_CURVE ( 'NONE', #59691, #23443, #375, .T. ) ;
#11634 = VERTEX_POINT ( 'NONE', #533 ) ;
#11635 = CYLINDRICAL_SURFACE ( 'NONE', #30282, 5.000000000000000888 ) ;
#11636 = LINE ( 'NONE', #6672, #55671 ) ;
#11637 = CARTESIAN_POINT ( 'NONE',  ( 24.82652845881425208, 8.390869743685042792, -8.578654028722157321 ) ) ;
#11638 = DIRECTION ( 'NONE',  ( 0.000000000000000000, 0.9105187689795969375, -0.4134677391718481476 ) ) ;
#11639 = EDGE_CURVE ( 'NONE', #61418, #24889, #61345, .T. ) ;
#11640 = AXIS2_PLACEMENT_3D ( 'NONE', #44947, #29326, #14658 ) ;
#11641 = AXIS2_PLACEMENT_3D ( 'NONE', #63822, #38567, #36352 ) ;
#11642 = CARTESIAN_POINT ( 'NONE',  ( 0.3665391374699467075, -10.76665847464316883, 5.911453292029565709 ) ) ;
#11643 =( BOUNDED_CURVE ( )  B_SPLINE_CURVE ( 3, ( #46877, #62167, #11616, #31886 ),
 .UNSPECIFIED., .F., .F. ) 
 B_SPLINE_CURVE_WITH_KNOTS ( ( 4, 4 ),
 ( 5.516275288668797572, 5.535842959799285090 ),
 .UNSPECIFIED. ) 
 CURVE ( )  GEOMETRIC_REPRESENTATION_ITEM ( )  RATIONAL_B_SPLINE_CURVE ( ( 1.000000000000000000, 0.9999680924417370109, 0.9999680924417370109, 1.000000000000000000 ) ) 
 REPRESENTATION_ITEM ( '' )  );
#11644 = VERTEX_POINT ( 'NONE', #46718 ) ;
#11645 = CARTESIAN_POINT ( 'NONE',  ( 2.241451721903216843, 2.553895636571935857, 7.194631024842649047 ) ) ;
#11646 = FACE_OUTER_BOUND ( 'NONE', #10791, .T. ) ;
#11647 = CIRCLE ( 'NONE', #49922, 12.18649999999999878 ) ;
#11648 = EDGE_CURVE ( 'NONE', #63071, #16758, #2514, .T. ) ;
#11649 = ORIENTED_EDGE ( 'NONE', *, *, #34099, .T. ) ;
#11650 = EDGE_CURVE ( 'NONE', #19209, #63267, #19543, .T. ) ;
#11651 = ORIENTED_EDGE ( 'NONE', *, *, #38039, .F. ) ;
#11652 = CARTESIAN_POINT ( 'NONE',  ( 0.2650492594609224484, 2.017987075343959269, 12.07870403910582269 ) ) ;
#11653 = CARTESIAN_POINT ( 'NONE',  ( 37.00000000000000711, -7.376655759824808811, 9.700295462048739381 ) ) ;
#11654 = CYLINDRICAL_SURFACE ( 'NONE', #19468, 12.18650000000000055 ) ;
#11655 = DIRECTION ( 'NONE',  ( -1.000000000000000000, 0.000000000000000000, -0.000000000000000000 ) ) ;
#11656 = ORIENTED_EDGE ( 'NONE', *, *, #47928, .F. ) ;
#11657 = VERTEX_POINT ( 'NONE', #26435 ) ;
#11658 = EDGE_LOOP ( 'NONE', ( #36696, #64405, #44353, #10488 ) ) ;
#11659 = LINE ( 'NONE', #52256, #2610 ) ;
#11661 = CARTESIAN_POINT ( 'NONE',  ( -27.01437459610461644, 13.31613970204373132, -2.220455681983952267 ) ) ;
#11660 = CIRCLE ( 'NONE', #57345, 19.00000000000000355 ) ;
#11663 = ADVANCED_FACE ( 'NONE', ( #30439 ), #31102, .T. ) ;
#11662 = ORIENTED_EDGE ( 'NONE', *, *, #38114, .T. ) ;
#11664 = DIRECTION ( 'NONE',  ( 1.000000000000000000, 0.000000000000000000, 0.000000000000000000 ) ) ;
#11665 = FACE_OUTER_BOUND ( 'NONE', #35589, .T. ) ;
#11666 = ORIENTED_EDGE ( 'NONE', *, *, #39350, .T. ) ;
#11667 = CYLINDRICAL_SURFACE ( 'NONE', #37523, 2.899999999999994582 ) ;
#11668 = CYLINDRICAL_SURFACE ( 'NONE', #55175, 12.18650000000000055 ) ;
#11669 = CARTESIAN_POINT ( 'NONE',  ( 2.305787727787083519, 7.135468203929983488, 2.774453000917173284 ) ) ;
#11670 = ORIENTED_EDGE ( 'NONE', *, *, #48480, .F. ) ;
#11671 = CARTESIAN_POINT ( 'NONE',  ( -35.00000000000000000, 11.61175578952786047, 1.771820996347196697 ) ) ;
#11672 = ORIENTED_EDGE ( 'NONE', *, *, #42860, .T. ) ;
#11673 = CARTESIAN_POINT ( 'NONE',  ( 1.014383007554944705, 7.686901933424285183, -9.851867765302106505 ) ) ;
#11674 = CARTESIAN_POINT ( 'NONE',  ( -28.67667724226168602, -1.375746547601631287, -1.299025457479364043 ) ) ;
#11675 = CARTESIAN_POINT ( 'NONE',  ( 11.32672149591984123, -33.39346531321197631, -11.05302976540055582 ) ) ;
#11676 = DIRECTION ( 'NONE',  ( 1.000000000000000000, 0.000000000000000000, 0.000000000000000000 ) ) ;
#11677 = CYLINDRICAL_SURFACE ( 'NONE', #60583, 5.000000000000000888 ) ;
#11678 = FACE_OUTER_BOUND ( 'NONE', #61004, .T. ) ;
#11679 = LINE ( 'NONE', #10700, #15029 ) ;
#11680 = ORIENTED_EDGE ( 'NONE', *, *, #17039, .T. ) ;
#11681 = AXIS2_PLACEMENT_3D ( 'NONE', #52070, #43056, #57385 ) ;
#11682 = DIRECTION ( 'NONE',  ( 0.000000000000000000, -0.01356324068817991828, 0.9999080150203990547 ) ) ;
#11683 = EDGE_CURVE ( 'NONE', #64921, #29384, #16357, .T. ) ;
#11684 = VERTEX_POINT ( 'NONE', #56036 ) ;
#11685 = CARTESIAN_POINT ( 'NONE',  ( 0.2657645697724701495, -4.330388001246489260, 11.45515365350260240 ) ) ;
#11686 = CARTESIAN_POINT ( 'NONE',  ( -35.00000000000000000, 3.614449339633491576, 11.17622378668007777 ) ) ;
#11687 = ORIENTED_EDGE ( 'NONE', *, *, #28170, .T. ) ;
#11688 = CARTESIAN_POINT ( 'NONE',  ( -18.58686583997218378, 5.413691226207714813, 10.71337495308983634 ) ) ;
#11689 = CARTESIAN_POINT ( 'NONE',  ( 0.9232058338315058954, 9.791640253608150601, 7.723624854284749652 ) ) ;
#11690 = AXIS2_PLACEMENT_3D ( 'NONE', #30251, #60175, #29914 ) ;
#11691 = CARTESIAN_POINT ( 'NONE',  ( -37.00000000000000711, 12.42372387097882580, 2.865935305911671449 ) ) ;
#11692 = ORIENTED_EDGE ( 'NONE', *, *, #18030, .F. ) ;
#11693 = ADVANCED_FACE ( 'NONE', ( #20800 ), #30346, .T. ) ;
#11694 = ORIENTED_EDGE ( 'NONE', *, *, #63719, .F. ) ;
#11695 = DIRECTION ( 'NONE',  ( 0.000000000000000000, -0.3554799084908835116, -0.9346839223284592046 ) ) ;
#11696 = VERTEX_POINT ( 'NONE', #9380 ) ;
#11697 = DIRECTION ( 'NONE',  ( -1.000000000000000000, 0.000000000000000000, -0.000000000000000000 ) ) ;
#11698 = CARTESIAN_POINT ( 'NONE',  ( 2.000000000000001776, 3.795144977083718008, -6.468916029978776017 ) ) ;
#11699 = CARTESIAN_POINT ( 'NONE',  ( 5.536195898058073439, 0.007896796515810338216, 0.003145317580921177386 ) ) ;
#11700 = EDGE_CURVE ( 'NONE', #26284, #47440, #46494, .T. ) ;
#11701 = ORIENTED_EDGE ( 'NONE', *, *, #22336, .F. ) ;
#11702 = CARTESIAN_POINT ( 'NONE',  ( 2.000000000000001776, -0.4129979343797593461, 6.800241778083677247 ) ) ;
#11703 = EDGE_CURVE ( 'NONE', #21834, #25882, #47074, .T. ) ;
#11704 = VECTOR ( 'NONE', #10914, 1000.000000000000000 ) ;
#11705 = CIRCLE ( 'NONE', #31882, 12.18650000000000055 ) ;
#11706 = CARTESIAN_POINT ( 'NONE',  ( 26.08439714455133185, 12.97057518889166516, 3.743551691817328386 ) ) ;
#11707 = CARTESIAN_POINT ( 'NONE',  ( 2.406456491626455474, 0.6290357040720031545, 10.41426194695389995 ) ) ;
#11708 = CARTESIAN_POINT ( 'NONE',  ( 11.86852745065355208, 10.64790170674535474, -8.300198448557052799 ) ) ;
#11709 = DIRECTION ( 'NONE',  ( 0.000000000000000000, -0.01356324068817992175, 0.9999080150203990547 ) ) ;
#11710 = CARTESIAN_POINT ( 'NONE',  ( -47.00000000000000711, 0.000000000000000000, 0.000000000000000000 ) ) ;
#11711 = DIRECTION ( 'NONE',  ( 0.000000000000000000, 0.01356324068817998940, -0.9999080150203990547 ) ) ;
#11712 = CARTESIAN_POINT ( 'NONE',  ( -22.71097035706202405, -2.846599994298329328, 4.089776368546542251 ) ) ;
#11713 = AXIS2_PLACEMENT_3D ( 'NONE', #26083, #41688, #60662 ) ;
#11714 = EDGE_CURVE ( 'NONE', #16892, #41673, #61922, .T. ) ;
#11715 = ORIENTED_EDGE ( 'NONE', *, *, #53495, .F. ) ;
#11716 = CARTESIAN_POINT ( 'NONE',  ( 0.2655924914740778742, 9.409507842006028966, 7.838010948425079505 ) ) ;
#11717 = CARTESIAN_POINT ( 'NONE',  ( 0.2676618633000463210, -12.24591287309138821, -0.1607051348608917463 ) ) ;
#11718 = ORIENTED_EDGE ( 'NONE', *, *, #35490, .T. ) ;
#11719 = CARTESIAN_POINT ( 'NONE',  ( 0.000000000000000000, 4.444115772890121718, 5.163689623839328391 ) ) ;
#11720 = CARTESIAN_POINT ( 'NONE',  ( 1.549075743846920483, -9.261503792573559934, -8.652116335902379163 ) ) ;
#11721 = ORIENTED_EDGE ( 'NONE', *, *, #30605, .T. ) ;
#11722 = DIRECTION ( 'NONE',  ( 0.000000000000000000, 0.2149704402110245716, -0.9766205557100865464 ) ) ;
#11723 = ORIENTED_EDGE ( 'NONE', *, *, #63507, .T. ) ;
#11724 = VECTOR ( 'NONE', #52754, 1000.000000000000000 ) ;
#11725 = CARTESIAN_POINT ( 'NONE',  ( 37.00000000000000711, -8.854740511458901508, -7.717887834988215623 ) ) ;
#11726 = VERTEX_POINT ( 'NONE', #44982 ) ;
#11727 = VERTEX_POINT ( 'NONE', #29665 ) ;
#11728 = EDGE_CURVE ( 'NONE', #34225, #786, #19728, .T. ) ;
#11729 = CARTESIAN_POINT ( 'NONE',  ( -27.08419797710328680, -1.803546201758814860, 1.413289504316734613 ) ) ;
#11730 = ORIENTED_EDGE ( 'NONE', *, *, #30714, .F. ) ;
#11731 = CARTESIAN_POINT ( 'NONE',  ( 3.152665057734040488, 0.000000000000000000, 0.000000000000000000 ) ) ;
#11732 = CARTESIAN_POINT ( 'NONE',  ( -22.29018399051993526, -3.576688584977250951, 1.024613686459453055 ) ) ;
#11733 = CARTESIAN_POINT ( 'NONE',  ( 35.00000000000000000, 8.699265615723106748, 8.534258022645994757 ) ) ;
#11734 = VECTOR ( 'NONE', #15025, 1000.000000000000000 ) ;
#11735 = CARTESIAN_POINT ( 'NONE',  ( 1.372161826076905067, -0.5897614319405121153, -12.60140585080819875 ) ) ;
#11736 = ORIENTED_EDGE ( 'NONE', *, *, #14244, .F. ) ;
#11737 = CARTESIAN_POINT ( 'NONE',  ( -4.984431264850669230, -1.083143072858141487, -11.95218935805936056 ) ) ;
#11738 = CARTESIAN_POINT ( 'NONE',  ( 7.310206959902322055, -26.30114832292194649, 14.76431686918209785 ) ) ;
#11739 = CARTESIAN_POINT ( 'NONE',  ( 2.941278708680199916, 0.9331242451665799909, -6.068329152486366063 ) ) ;
#11741 = ORIENTED_EDGE ( 'NONE', *, *, #23124, .F. ) ;
#11740 = CARTESIAN_POINT ( 'NONE',  ( -26.75731680663163559, 10.79779643724861593, 5.235948385342425127 ) ) ;
#11743 = CIRCLE ( 'NONE', #20250, 12.18650000000000055 ) ;
#11742 = DIRECTION ( 'NONE',  ( -1.000000000000000000, 0.000000000000000000, 0.000000000000000000 ) ) ;
#11744 = EDGE_LOOP ( 'NONE', ( #39629, #508, #9611, #45062 ) ) ;
#11745 = CARTESIAN_POINT ( 'NONE',  ( 0.2652384770603688491, 9.423432754625833851, -7.820955051613227127 ) ) ;
#11746 = VERTEX_POINT ( 'NONE', #20037 ) ;
#11747 = CARTESIAN_POINT ( 'NONE',  ( -35.00000000000000000, -8.766823244862047559, 7.817610399097479679 ) ) ;
#11748 = DIRECTION ( 'NONE',  ( 0.000000000000000000, 0.01356324068817998940, -0.9999080150203990547 ) ) ;
#11749 = CARTESIAN_POINT ( 'NONE',  ( 1.198791140417940326, -4.776130053252316543, 11.61358959650655187 ) ) ;
#11750 = CIRCLE ( 'NONE', #56375, 5.000000000000000000 ) ;
#11751 = ORIENTED_EDGE ( 'NONE', *, *, #55046, .T. ) ;
#11753 = CIRCLE ( 'NONE', #14921, 12.18650000000000055 ) ;
#11752 = CARTESIAN_POINT ( 'NONE',  ( -35.00000000000000000, 11.86701198550360203, -2.772148766915989881 ) ) ;
#11754 = DIRECTION ( 'NONE',  ( 0.000000000000000000, 0.5155538571770230671, -0.8568571761675883858 ) ) ;
#11755 = CARTESIAN_POINT ( 'NONE',  ( 36.00000000000000711, 9.506317355798490354, 8.496612874013054650 ) ) ;
#11756 = ORIENTED_EDGE ( 'NONE', *, *, #18933, .F. ) ;
#11757 = EDGE_CURVE ( 'NONE', #21481, #4753, #29672, .T. ) ;
#11758 = VERTEX_POINT ( 'NONE', #65262 ) ;
#11759 = VECTOR ( 'NONE', #5846, 1000.000000000000000 ) ;
#11760 = FACE_OUTER_BOUND ( 'NONE', #10277, .T. ) ;
#11761 = ORIENTED_EDGE ( 'NONE', *, *, #19065, .F. ) ;
#11762 = EDGE_CURVE ( 'NONE', #18188, #648, #35368, .T. ) ;
#11763 = ORIENTED_EDGE ( 'NONE', *, *, #46297, .F. ) ;
#11764 = CARTESIAN_POINT ( 'NONE',  ( 19.28625800530497258, -6.413918128308385036, 11.87904264843581537 ) ) ;
#11765 = CARTESIAN_POINT ( 'NONE',  ( -35.00000000000000000, -7.499679039484122178, 9.040300684349668714 ) ) ;
#11766 = CARTESIAN_POINT ( 'NONE',  ( 2.241536586108915152, -7.176205604390190729, -2.605228657247420365 ) ) ;
#11767 = FACE_OUTER_BOUND ( 'NONE', #42712, .T. ) ;
#11768 = CARTESIAN_POINT ( 'NONE',  ( 1.719304012341412724, 1.452142814149018690, -12.64775761152637301 ) ) ;
#11769 = DIRECTION ( 'NONE',  ( 1.000000000000000000, 0.000000000000000000, -0.000000000000000000 ) ) ;
#11770 = EDGE_CURVE ( 'NONE', #25415, #55675, #34344, .T. ) ;
#11771 = CARTESIAN_POINT ( 'NONE',  ( -35.00000000000000000, 0.000000000000000000, 0.000000000000000000 ) ) ;
#11772 = VECTOR ( 'NONE', #50257, 1000.000000000000000 ) ;
#11773 = AXIS2_PLACEMENT_3D ( 'NONE', #944, #21565, #27195 ) ;
#11774 = EDGE_LOOP ( 'NONE', ( #17526, #21089, #25097, #19387 ) ) ;
#11775 = AXIS2_PLACEMENT_3D ( 'NONE', #65783, #5303, #45866 ) ;
#11776 = LINE ( 'NONE', #46710, #19019 ) ;
#11777 = EDGE_CURVE ( 'NONE', #18204, #26747, #50319, .T. ) ;
#11778 = DIRECTION ( 'NONE',  ( 1.000000000000000000, 0.000000000000000000, 0.000000000000000000 ) ) ;
#11779 = VECTOR ( 'NONE', #47931, 1000.000000000000000 ) ;
#11780 = CARTESIAN_POINT ( 'NONE',  ( 35.00000000000000000, -12.16632754454236043, 0.7008968033240018380 ) ) ;
#11781 = FACE_OUTER_BOUND ( 'NONE', #15660, .T. ) ;
#11782 = EDGE_CURVE ( 'NONE', #42485, #29713, #5084, .T. ) ;
#11783 = AXIS2_PLACEMENT_3D ( 'NONE', #39578, #34579, #4692 ) ;
#11784 = FACE_OUTER_BOUND ( 'NONE', #55099, .T. ) ;
#11785 = AXIS2_PLACEMENT_3D ( 'NONE', #38734, #54368, #2525 ) ;
#11786 = ORIENTED_EDGE ( 'NONE', *, *, #43914, .T. ) ;
#11787 = CARTESIAN_POINT ( 'NONE',  ( -41.00000000000000711, -25.18551001833413139, 3.766049837354531249 ) ) ;
#11788 = CARTESIAN_POINT ( 'NONE',  ( 47.00000000000000711, 4.705694406421931860E-17, -3.469127814946512892E-15 ) ) ;
#11789 = CARTESIAN_POINT ( 'NONE',  ( 2.717984159220126816, 1.073093837952427965, -7.719081760284447036 ) ) ;
#11790 = CARTESIAN_POINT ( 'NONE',  ( -25.86628395826706850, -5.139808748864358456, 10.84354029019568522 ) ) ;
#11791 = AXIS2_PLACEMENT_3D ( 'NONE', #40338, #35680, #36348 ) ;
#11792 = AXIS2_PLACEMENT_3D ( 'NONE', #52636, #2073, #7374 ) ;
#11793 = CIRCLE ( 'NONE', #57492, 5.000000000000000888 ) ;
#11794 = CARTESIAN_POINT ( 'NONE',  ( -25.10197438393668889, 9.577105551445603382, 7.239297392635676509 ) ) ;
#11795 = CARTESIAN_POINT ( 'NONE',  ( -25.13764408299829256, -11.42471432779190188, 7.193830867856458866 ) ) ;
#11796 = EDGE_LOOP ( 'NONE', ( #3766, #16075, #61722, #4036 ) ) ;
#11797 = CARTESIAN_POINT ( 'NONE',  ( 35.00000000000000000, -7.971186206369405447, 9.217970097227802029 ) ) ;
#11798 = DIRECTION ( 'NONE',  ( 0.000000000000000000, 0.9847383929261623869, -0.1740410799127578845 ) ) ;
#11799 = CARTESIAN_POINT ( 'NONE',  ( 2.261269890821705264, -4.803890999604552015, -5.942064862945291459 ) ) ;
#11800 = CARTESIAN_POINT ( 'NONE',  ( 2.276198483117263915, 1.175725118478853526, 7.555081843354693127 ) ) ;
#11801 = ORIENTED_EDGE ( 'NONE', *, *, #63896, .T. ) ;
#11802 = CARTESIAN_POINT ( 'NONE',  ( 3.152665057735396736, -5.761241965768377327, 5.461013642406604696 ) ) ;
#11803 = CARTESIAN_POINT ( 'NONE',  ( -35.00000000000000000, 0.000000000000000000, 0.000000000000000000 ) ) ;
#11805 = ORIENTED_EDGE ( 'NONE', *, *, #4975, .F. ) ;
#11804 = CARTESIAN_POINT ( 'NONE',  ( 38.56928140186735021, -26.58605982982061988, -4.500000000000001776 ) ) ;
#11806 = CARTESIAN_POINT ( 'NONE',  ( 37.00000000000000711, 5.246972444134017977, -10.99909370905159101 ) ) ;
#11807 = AXIS2_PLACEMENT_3D ( 'NONE', #18509, #7501, #43742 ) ;
#11808 = ADVANCED_FACE ( 'NONE', ( #34973 ), #4775, .F. ) ;
#11809 = VECTOR ( 'NONE', #36984, 1000.000000000000000 ) ;
#11810 = CARTESIAN_POINT ( 'NONE',  ( 2.000000000000001776, 0.2704997240205054276, 6.931223712253452796 ) ) ;
#11811 = ORIENTED_EDGE ( 'NONE', *, *, #7151, .F. ) ;
#11812 = CIRCLE ( 'NONE', #5497, 4.999999999999999112 ) ;
#11813 = CARTESIAN_POINT ( 'NONE',  ( 35.00000000000000000, -4.946702696913249042, -11.13736569743272753 ) ) ;
#11814 = CYLINDRICAL_SURFACE ( 'NONE', #64380, 5.000000000000000888 ) ;
#11816 = DIRECTION ( 'NONE',  ( 0.000000000000000000, -0.01356324068817999114, 0.9999080150203989437 ) ) ;
#11815 =( BOUNDED_SURFACE ( )  B_SPLINE_SURFACE ( 3, 1, ( 
 ( #44695, #64986 ),
 ( #43730, #64010 ),
 ( #59051, #8161 ),
 ( #19458, #24109 ) ),
 .UNSPECIFIED., .F., .F., .F. ) 
 B_SPLINE_SURFACE_WITH_KNOTS ( ( 4, 4 ),
 ( 2, 2 ),
 ( 0.000000000000000000, 1.000000000000000000 ),
 ( 0.000000000000000000, 1.000000000000000000 ),
 .UNSPECIFIED. ) 
 GEOMETRIC_REPRESENTATION_ITEM ( )  RATIONAL_B_SPLINE_SURFACE ( (
 ( 1.000000000000000000, 1.000000000000000000),
 ( 0.9942764183789327692, 0.8450855930916580938),
 ( 0.9942764183789327692, 0.8450855930916580938),
 ( 1.000000000000000000, 1.000000000000000000) ) ) 
 REPRESENTATION_ITEM ( '' )  SURFACE ( )  );
#11817 = CARTESIAN_POINT ( 'NONE',  ( -3.570318967459569226, -9.097864018429371313, 9.981632988681457874 ) ) ;
#11818 = B_SPLINE_CURVE_WITH_KNOTS ( 'NONE', 3,
 ( #38199, #7976, #53847, #12595, #47867, #58861, #32875, #28242, #2986, #11952, #43511, #2326, #32233, #63793, #18277, #13277 ),
 .UNSPECIFIED., .F., .F.,
 ( 4, 3, 3, 3, 3, 4 ),
 ( 0.000000000000000000, 0.0002176109881720225063, 0.0004352086762394585524, 0.0006528017811446870742, 0.0007615147961451692411, 0.0009453342004947387980 ),
 .UNSPECIFIED. ) ;
#11819 = CARTESIAN_POINT ( 'NONE',  ( 0.2833330754217405767, -11.44258640049858577, -4.379886056891013624 ) ) ;
#11820 = DIRECTION ( 'NONE',  ( -1.000000000000000000, 0.000000000000000000, 0.000000000000000000 ) ) ;
#11822 = ORIENTED_EDGE ( 'NONE', *, *, #28978, .F. ) ;
#11821 = DIRECTION ( 'NONE',  ( -1.000000000000000000, -0.000000000000000000, 0.000000000000000000 ) ) ;
#11823 = CARTESIAN_POINT ( 'NONE',  ( -22.27721056931765631, 2.427163553894384762, 2.768264578996945335 ) ) ;
#11824 = EDGE_LOOP ( 'NONE', ( #5612, #29734, #54369, #3560 ) ) ;
#11825 = CARTESIAN_POINT ( 'NONE',  ( -35.00000000000000000, 1.771820996347319710, -11.61175578952784448 ) ) ;
#11826 = EDGE_LOOP ( 'NONE', ( #22579, #19529, #4422, #48621 ) ) ;
#11827 = PRODUCT_CONTEXT ( 'NONE', #36599, 'mechanical' ) ;
#11828 = DIRECTION ( 'NONE',  ( 0.000000000000000000, -0.01356324068817991828, 0.9999080150203990547 ) ) ;
#11829 = DIRECTION ( 'NONE',  ( -1.000000000000000000, -0.000000000000000000, -0.000000000000000000 ) ) ;
#11830 = ADVANCED_FACE ( 'NONE', ( #35315 ), #55627, .T. ) ;
#11831 = DIRECTION ( 'NONE',  ( 0.000000000000000000, 0.9105187689795940509, -0.4134677391718546424 ) ) ;
#11832 = ORIENTED_EDGE ( 'NONE', *, *, #41570, .T. ) ;
#11833 = AXIS2_PLACEMENT_3D ( 'NONE', #4600, #898, #9886 ) ;
#11834 = CARTESIAN_POINT ( 'NONE',  ( -36.00000000000000711, 12.68495603654572079, 1.286231064351356368 ) ) ;
#11835 =( BOUNDED_SURFACE ( )  B_SPLINE_SURFACE ( 3, 1, ( 
 ( #41146, #10559 ),
 ( #36828, #51501 ),
 ( #61428, #15868 ),
 ( #50505, #5269 ) ),
 .UNSPECIFIED., .F., .F., .F. ) 
 B_SPLINE_SURFACE_WITH_KNOTS ( ( 4, 4 ),
 ( 2, 2 ),
 ( 0.000000000000000000, 1.000000000000000000 ),
 ( 0.000000000000000000, 1.000000000000000000 ),
 .UNSPECIFIED. ) 
 GEOMETRIC_REPRESENTATION_ITEM ( )  RATIONAL_B_SPLINE_SURFACE ( (
 ( 1.000000000000000000, 1.000000000000000000),
 ( 0.9257577194822556033, 0.9980522942447415113),
 ( 0.9257577194822556033, 0.9980522942447415113),
 ( 1.000000000000000000, 1.000000000000000000) ) ) 
 REPRESENTATION_ITEM ( '' )  SURFACE ( )  );
#11836 = ADVANCED_FACE ( 'NONE', ( #25328 ), #21322, .T. ) ;
#11837 = DIRECTION ( 'NONE',  ( -1.000000000000000000, 0.000000000000000000, 0.000000000000000000 ) ) ;
#11838 = ORIENTED_EDGE ( 'NONE', *, *, #16393, .F. ) ;
#11839 = ORIENTED_EDGE ( 'NONE', *, *, #13570, .F. ) ;
#11840 = CARTESIAN_POINT ( 'NONE',  ( -25.00000000000000355, -30.00000000000000000, 1.530808498934191521E-15 ) ) ;
#11841 = CIRCLE ( 'NONE', #40511, 5.000000000000000000 ) ;
#11842 = EDGE_CURVE ( 'NONE', #28065, #12917, #45288, .T. ) ;
#11843 = ORIENTED_EDGE ( 'NONE', *, *, #50547, .T. ) ;
#11844 = DIRECTION ( 'NONE',  ( 0.000000000000000000, -0.9987865678893282917, 0.04924826701373502535 ) ) ;
#11845 = DIRECTION ( 'NONE',  ( 0.000000000000000000, 0.5155538571770169609, 0.8568571761675920495 ) ) ;
#11846 = CARTESIAN_POINT ( 'NONE',  ( 12.03537186402451731, 0.5714996694917733322, 13.48808163914964808 ) ) ;
#11847 = CARTESIAN_POINT ( 'NONE',  ( -37.00000000000000711, -1.457575200925635528, 12.66641127287625501 ) ) ;
#11848 = CIRCLE ( 'NONE', #62835, 12.18649999999999878 ) ;
#11849 = AXIS2_PLACEMENT_3D ( 'NONE', #10296, #15610, #30901 ) ;
#11850 = CARTESIAN_POINT ( 'NONE',  ( -22.70624764888619751, 0.08990180771019894157, -5.249808673992000685 ) ) ;
#11851 = CARTESIAN_POINT ( 'NONE',  ( 26.08439714455133185, -11.40113243194250359, 3.743551691817327942 ) ) ;
#11852 = EDGE_CURVE ( 'NONE', #9459, #48048, #47957, .T. ) ;
#11853 = LINE ( 'NONE', #32132, #11030 ) ;
#11854 = ORIENTED_EDGE ( 'NONE', *, *, #60423, .T. ) ;
#11855 = DIRECTION ( 'NONE',  ( -1.000000000000000000, -0.000000000000000000, -0.000000000000000000 ) ) ;
#11856 = ADVANCED_FACE ( 'NONE', ( #40280 ), #20984, .T. ) ;
#11857 = ORIENTED_EDGE ( 'NONE', *, *, #20271, .T. ) ;
#11858 = CARTESIAN_POINT ( 'NONE',  ( 36.00000000000000711, 10.59380114696469910, -7.094637218249395971 ) ) ;
#11859 = CARTESIAN_POINT ( 'NONE',  ( -35.04683013664716640, 0.01235741808124560595, -0.0001018103929620997795 ) ) ;
#11860 = FACE_OUTER_BOUND ( 'NONE', #25125, .T. ) ;
#11861 = CARTESIAN_POINT ( 'NONE',  ( -37.00000000000000711, -9.908974237959601084, -6.307491713049132365 ) ) ;
#11862 = CARTESIAN_POINT ( 'NONE',  ( -17.71317172853713373, 11.35466418304649139, 3.882258812239216095 ) ) ;
#11863 = CYLINDRICAL_SURFACE ( 'NONE', #37216, 12.18650000000000055 ) ;
#11864 = ORIENTED_EDGE ( 'NONE', *, *, #4744, .F. ) ;
#11865 = CIRCLE ( 'NONE', #205, 5.000000000000000000 ) ;
#11866 = EDGE_LOOP ( 'NONE', ( #47189, #2003, #16445, #35869 ) ) ;
#11867 = CARTESIAN_POINT ( 'NONE',  ( -35.00000000000000000, 1.171570255487447643, 11.68758509253248867 ) ) ;
#11869 = EDGE_CURVE ( 'NONE', #12850, #10311, #13085, .T. ) ;
#11868 = VECTOR ( 'NONE', #22427, 1000.000000000000000 ) ;
#11870 = ORIENTED_EDGE ( 'NONE', *, *, #53758, .F. ) ;
#11871 = CARTESIAN_POINT ( 'NONE',  ( 0.3341166715381309604, 7.691251065848466517, -9.559079491641789161 ) ) ;
#11872 = DIRECTION ( 'NONE',  ( -1.000000000000000000, 0.000000000000000000, -0.000000000000000000 ) ) ;
#11873 = VECTOR ( 'NONE', #34252, 1000.000000000000114 ) ;
#11874 = EDGE_CURVE ( 'NONE', #9962, #47648, #10354, .T. ) ;
#11875 = CARTESIAN_POINT ( 'NONE',  ( 2.268878695253375710, 4.798796461778038314, 5.949442550447435529 ) ) ;
#11876 = CARTESIAN_POINT ( 'NONE',  ( -22.66110217412718342, 1.880032915665426740, 4.573370147466317981 ) ) ;
#11877 = ORIENTED_EDGE ( 'NONE', *, *, #28100, .T. ) ;
#11878 = DIRECTION ( 'NONE',  ( 0.000000000000000000, -0.01356324068817998940, 0.9999080150203990547 ) ) ;
#11879 = DIRECTION ( 'NONE',  ( 1.000000000000000000, 0.000000000000000000, 0.000000000000000000 ) ) ;
#11880 = CARTESIAN_POINT ( 'NONE',  ( 2.368238019615397150, -1.155661230551800145, 7.589221137922757876 ) ) ;
#11881 = DIRECTION ( 'NONE',  ( 0.000000000000000000, -0.1764146379942750642, -0.9843159429275484262 ) ) ;
#11882 = DIRECTION ( 'NONE',  ( -0.000000000000000000, -1.000000000000000000, -0.000000000000000000 ) ) ;
#11883 = CARTESIAN_POINT ( 'NONE',  ( 9.687175622948609899, -11.98570860552670325, -0.5854820436212360146 ) ) ;
#11884 = EDGE_LOOP ( 'NONE', ( #51710, #58521, #29911, #45842 ) ) ;
#11885 = CARTESIAN_POINT ( 'NONE',  ( -14.82145243739236129, -34.67135967094819193, -7.359580590752245577 ) ) ;
#11886 = ORIENTED_EDGE ( 'NONE', *, *, #14272, .F. ) ;
#11887 = DIRECTION ( 'NONE',  ( 1.000000000000000000, 0.000000000000000000, 0.000000000000000000 ) ) ;
#11888 = DIRECTION ( 'NONE',  ( -1.000000000000000000, 0.000000000000000000, 0.000000000000000000 ) ) ;
#11889 = CARTESIAN_POINT ( 'NONE',  ( 2.000000000000001776, 6.250523986463984549, 3.007653927006597172 ) ) ;
#11890 = VECTOR ( 'NONE', #55758, 1000.000000000000000 ) ;
#11891 = CARTESIAN_POINT ( 'NONE',  ( -29.73183716147547173, 1.699799061024255264, -13.39970470410835368 ) ) ;
#11892 = DIRECTION ( 'NONE',  ( -0.000000000000000000, -1.000000000000000000, -0.000000000000000000 ) ) ;
#11893 = AXIS2_PLACEMENT_3D ( 'NONE', #45831, #60796, #40846 ) ;
#11894 = EDGE_CURVE ( 'NONE', #9785, #22078, #1901, .T. ) ;
#11895 = EDGE_CURVE ( 'NONE', #6336, #26369, #40757, .T. ) ;
#11896 = AXIS2_PLACEMENT_3D ( 'NONE', #19237, #9554, #10228 ) ;
#11897 = EDGE_LOOP ( 'NONE', ( #7877, #25535, #38672, #14922 ) ) ;
#11898 = VERTEX_POINT ( 'NONE', #37266 ) ;
#11899 = DIRECTION ( 'NONE',  ( -1.000000000000000000, 0.000000000000000000, 0.000000000000000000 ) ) ;
#11900 = ORIENTED_EDGE ( 'NONE', *, *, #47778, .T. ) ;
#11901 = CARTESIAN_POINT ( 'NONE',  ( -27.08417473062937120, -2.249064769433619659, 0.4370481938669266153 ) ) ;
#11902 = FACE_OUTER_BOUND ( 'NONE', #2379, .T. ) ;
#11903 = CARTESIAN_POINT ( 'NONE',  ( -35.00000000000000000, -2.544412758415929066, 11.91791701451265340 ) ) ;
#11904 = CARTESIAN_POINT ( 'NONE',  ( 1.014383007554950700, 3.853787798429566092, -11.88680274101309564 ) ) ;
#11905 = CYLINDRICAL_SURFACE ( 'NONE', #7794, 5.000000000000000888 ) ;
#11906 = CARTESIAN_POINT ( 'NONE',  ( 2.261269890823179640, 5.762737836064523833, 5.017604628139654466 ) ) ;
#11907 = CARTESIAN_POINT ( 'NONE',  ( -4.989057617119011745, -0.9162120371760335003, 11.96497202265570259 ) ) ;
#11908 = ORIENTED_EDGE ( 'NONE', *, *, #21422, .T. ) ;
#11909 = ADVANCED_FACE ( 'NONE', ( #2720 ), #47582, .T. ) ;
#11910 = LINE ( 'NONE', #57825, #7654 ) ;
#11911 = VERTEX_POINT ( 'NONE', #7327 ) ;
#11912 = CARTESIAN_POINT ( 'NONE',  ( 35.00000000000000000, 4.705694406421931860E-17, -3.469127814946512892E-15 ) ) ;
#11913 = CIRCLE ( 'NONE', #46966, 4.999999999999999112 ) ;
#11914 = CARTESIAN_POINT ( 'NONE',  ( 0.3675815128205912052, 8.093875121226199454, -9.235491948679927177 ) ) ;
#11915 = EDGE_CURVE ( 'NONE', #19302, #47299, #63511, .T. ) ;
#11916 = CARTESIAN_POINT ( 'NONE',  ( -27.09342121492660738, 1.671264186073228464, 1.607500752098841135 ) ) ;
#11917 = VERTEX_POINT ( 'NONE', #47916 ) ;
#11918 = DIRECTION ( 'NONE',  ( 0.000000000000000000, 0.01356324068817998940, -0.9999080150203990547 ) ) ;
#11919 = AXIS2_PLACEMENT_3D ( 'NONE', #29910, #50216, #65786 ) ;
#11920 = CARTESIAN_POINT ( 'NONE',  ( -18.19295774167957092, -29.77901320112238892, -7.993354913176282217 ) ) ;
#11921 = CYLINDRICAL_SURFACE ( 'NONE', #23383, 7.499999999999988454 ) ;
#11922 = ORIENTED_EDGE ( 'NONE', *, *, #8273, .T. ) ;
#11923 = AXIS2_PLACEMENT_3D ( 'NONE', #3283, #47841, #58151 ) ;
#11924 = VERTEX_POINT ( 'NONE', #26980 ) ;
#11925 = CARTESIAN_POINT ( 'NONE',  ( -17.08907783926314394, 2.790822428529209809, -11.67174978956914089 ) ) ;
#11926 = EDGE_CURVE ( 'NONE', #61427, #28685, #41575, .T. ) ;
#11927 = ORIENTED_EDGE ( 'NONE', *, *, #52120, .F. ) ;
#11928 = VERTEX_POINT ( 'NONE', #12639 ) ;
#11929 = ORIENTED_EDGE ( 'NONE', *, *, #13202, .F. ) ;
#11930 = ORIENTED_EDGE ( 'NONE', *, *, #34321, .T. ) ;
#11931 = CARTESIAN_POINT ( 'NONE',  ( 2.241352910868909643, -7.145045428366594287, 2.689314586382326677 ) ) ;
#11932 = DIRECTION ( 'NONE',  ( 0.000000000000000000, 0.000000000000000000, 1.000000000000000000 ) ) ;
#11933 = FACE_OUTER_BOUND ( 'NONE', #12681, .T. ) ;
#11934 = CARTESIAN_POINT ( 'NONE',  ( 2.000000000000001776, 2.469490258309423591, 6.482025155313315246 ) ) ;
#11935 = CARTESIAN_POINT ( 'NONE',  ( -7.489022030332961322, 25.00000000000000000, -10.84914964302385521 ) ) ;
#11936 = VERTEX_POINT ( 'NONE', #12322 ) ;
#11937 = DIRECTION ( 'NONE',  ( 1.000000000000000000, -0.000000000000000000, 0.000000000000000000 ) ) ;
#11938 = AXIS2_PLACEMENT_3D ( 'NONE', #39676, #16295, #1339 ) ;
#11939 = VERTEX_POINT ( 'NONE', #2376 ) ;
#11940 = LINE ( 'NONE', #37550, #2016 ) ;
#11941 = ADVANCED_FACE ( 'NONE', ( #17981 ), #57240, .T. ) ;
#11942 = CARTESIAN_POINT ( 'NONE',  ( -22.27715526084302056, 2.930376837866846884, -2.228953214080618750 ) ) ;
#11943 = CARTESIAN_POINT ( 'NONE',  ( 2.297017764050233612, 3.682881532880140529, -6.708511771223914621 ) ) ;
#11944 = EDGE_CURVE ( 'NONE', #30241, #23572, #63197, .T. ) ;
#11945 = DIRECTION ( 'NONE',  ( 0.000000000000000000, 0.000000000000000000, 1.000000000000000000 ) ) ;
#11946 = CARTESIAN_POINT ( 'NONE',  ( -35.00000000000000000, 8.854740511458851770, 7.717887834988275131 ) ) ;
#11947 = CARTESIAN_POINT ( 'NONE',  ( -35.00000000000000000, 5.672855678558835102, -10.28547182238001767 ) ) ;
#11948 = VECTOR ( 'NONE', #15003, 1000.000000000000114 ) ;
#11949 = ADVANCED_FACE ( 'NONE', ( #17664 ), #11667, .T. ) ;
#11950 = AXIS2_PLACEMENT_3D ( 'NONE', #10906, #17209, #6258 ) ;
#11951 = EDGE_LOOP ( 'NONE', ( #38503, #63863, #6623, #46467 ) ) ;
#11952 = CARTESIAN_POINT ( 'NONE',  ( 2.899286259009683953, -7.250549018622921338, -3.018334250363155835 ) ) ;
#11953 = EDGE_CURVE ( 'NONE', #23142, #58933, #58218, .T. ) ;
#11954 = EDGE_LOOP ( 'NONE', ( #64322, #17310, #24125, #25529 ) ) ;
#11955 = DIRECTION ( 'NONE',  ( 1.000000000000000000, 0.000000000000000000, 0.000000000000000000 ) ) ;
#11956 = CARTESIAN_POINT ( 'NONE',  ( 37.00000000000000711, -1.488153103996881610, 11.65150730582935701 ) ) ;
#11957 = CARTESIAN_POINT ( 'NONE',  ( 18.57729641407471277, -29.86520738451961776, 7.358162954095265107 ) ) ;
#11958 = EDGE_CURVE ( 'NONE', #25095, #48019, #7679, .T. ) ;
#11959 = DIRECTION ( 'NONE',  ( 1.000000000000000000, 0.000000000000000000, 0.000000000000000000 ) ) ;
#11960 = CARTESIAN_POINT ( 'NONE',  ( 37.00000000000000711, -12.31350058095520339, 3.307597835713371737 ) ) ;
#11961 = ORIENTED_EDGE ( 'NONE', *, *, #8732, .T. ) ;
#11962 = CARTESIAN_POINT ( 'NONE',  ( 1.719304012339819332, -8.755325027794356174, 9.242227816401850760 ) ) ;
#11963 = DIRECTION ( 'NONE',  ( -1.000000000000000000, 0.000000000000000000, 0.000000000000000000 ) ) ;
#11964 = DIRECTION ( 'NONE',  ( -1.000000000000000000, 0.000000000000000000, 0.000000000000000000 ) ) ;
#11965 = CARTESIAN_POINT ( 'NONE',  ( -3.229081750799087214, 8.212677051982280929, 10.74170107049143397 ) ) ;
#11966 = AXIS2_PLACEMENT_3D ( 'NONE', #50199, #55165, #10262 ) ;
#11967 = CARTESIAN_POINT ( 'NONE',  ( -22.65996813707689128, -2.607318832796680752, 4.069902221062763559 ) ) ;
#11968 = AXIS2_PLACEMENT_3D ( 'NONE', #52261, #13317, #57907 ) ;
#11969 = ORIENTED_EDGE ( 'NONE', *, *, #16528, .F. ) ;
#11970 = UNCERTAINTY_MEASURE_WITH_UNIT (LENGTH_MEASURE( 1.000000000000000082E-05 ), #60747, 'distance_accuracy_value', 'NONE');
#11971 = CARTESIAN_POINT ( 'NONE',  ( 0.2655924914740778187, 7.838010948425048419, 9.409507842006050282 ) ) ;
#11972 = CARTESIAN_POINT ( 'NONE',  ( 0.5572780756287527559, -5.905274004878251937, -10.83930267798922564 ) ) ;
#11973 = B_SPLINE_CURVE_WITH_KNOTS ( 'NONE', 3,
 ( #61450, #31218, #17235, #1298, #26881, #5971, #1627, #21901, #37509, #26227, #62434, #16896 ),
 .UNSPECIFIED., .F., .F.,
 ( 4, 2, 2, 2, 2, 4 ),
 ( 0.000000000000000000, 0.002493599491187762762, 0.004987198982375525523, 0.006233998727969406253, 0.007480798473563286116, 0.009974397964751049311 ),
 .UNSPECIFIED. ) ;
#11974 = ADVANCED_FACE ( 'NONE', ( #58563 ), #12989, .T. ) ;
#11975 = VERTEX_POINT ( 'NONE', #21674 ) ;
#11976 = EDGE_CURVE ( 'NONE', #40181, #55613, #41929, .T. ) ;
#11977 = VERTEX_POINT ( 'NONE', #59865 ) ;
#11978 = CARTESIAN_POINT ( 'NONE',  ( 36.00000000000000711, 12.68495603654573500, 1.286231064351171627 ) ) ;
#11979 = CARTESIAN_POINT ( 'NONE',  ( -27.09342121492585065, -1.671264186070199553, -1.607500752098762975 ) ) ;
#11980 = CARTESIAN_POINT ( 'NONE',  ( -35.00000000000000000, 0.000000000000000000, 0.000000000000000000 ) ) ;
#11981 = FACE_OUTER_BOUND ( 'NONE', #25147, .T. ) ;
#11982 = ORIENTED_EDGE ( 'NONE', *, *, #7833, .T. ) ;
#11983 = CIRCLE ( 'NONE', #16274, 2.899999999999995470 ) ;
#11984 = EDGE_CURVE ( 'NONE', #56228, #18427, #8902, .T. ) ;
#11985 = AXIS2_PLACEMENT_3D ( 'NONE', #55767, #55433, #40452 ) ;
#11986 = EDGE_LOOP ( 'NONE', ( #1417, #7354, #23623, #35565 ) ) ;
#11987 = ORIENTED_EDGE ( 'NONE', *, *, #59862, .F. ) ;
#11988 = CARTESIAN_POINT ( 'NONE',  ( 2.507146904658100972, 7.719969556433170510, 0.2163149345876847485 ) ) ;
#11989 = AXIS2_PLACEMENT_3D ( 'NONE', #849, #21115, #41391 ) ;
#11991 = VECTOR ( 'NONE', #41915, 1000.000000000000000 ) ;
#11990 = CYLINDRICAL_SURFACE ( 'NONE', #61880, 12.74999999999999822 ) ;
#11992 = ORIENTED_EDGE ( 'NONE', *, *, #33780, .T. ) ;
#11993 = DIRECTION ( 'NONE',  ( -1.000000000000000000, 0.000000000000000000, 0.000000000000000000 ) ) ;
#11994 = CARTESIAN_POINT ( 'NONE',  ( 1.000000000000000888, 4.472310526050849333, -6.020667617347339906 ) ) ;
#11995 = ORIENTED_EDGE ( 'NONE', *, *, #6724, .T. ) ;
#11996 = CARTESIAN_POINT ( 'NONE',  ( 0.2653519789438771315, 11.50012635727061117, -4.209148152332801374 ) ) ;
#11997 = DIRECTION ( 'NONE',  ( 1.000000000000000000, 0.000000000000000000, 0.000000000000000000 ) ) ;
#11998 = CARTESIAN_POINT ( 'NONE',  ( 23.97867415005905656, 2.287513683784789364, 11.78413097500964746 ) ) ;
#11999 = ORIENTED_EDGE ( 'NONE', *, *, #19251, .F. ) ;
#12000 = AXIS2_PLACEMENT_3D ( 'NONE', #3814, #44645, #65583 ) ;
#12001 = CARTESIAN_POINT ( 'NONE',  ( 37.00000000000000711, 4.705694406421931860E-17, -3.469127814946512892E-15 ) ) ;
#12002 = EDGE_CURVE ( 'NONE', #22893, #3903, #24991, .T. ) ;
#12003 = EDGE_LOOP ( 'NONE', ( #37948, #42584, #31771, #14442 ) ) ;
#12004 = DIRECTION ( 'NONE',  ( 0.000000000000000000, 1.000000000000000000, 0.000000000000000000 ) ) ;
#12005 = CIRCLE ( 'NONE', #20466, 5.000000000000000888 ) ;
#12006 = CARTESIAN_POINT ( 'NONE',  ( -18.54402015049394237, -5.053814502618243942, 12.52063007984827614 ) ) ;
#12007 = EDGE_CURVE ( 'NONE', #24100, #65334, #44881, .T. ) ;
#12008 = DIRECTION ( 'NONE',  ( 0.000000000000000000, -0.01356324068817991828, 0.9999080150203990547 ) ) ;
#12009 = AXIS2_PLACEMENT_3D ( 'NONE', #18872, #58129, #28504 ) ;
#12010 = CARTESIAN_POINT ( 'NONE',  ( -35.00000000000000000, 12.02534193257726791, -4.237174932027097718 ) ) ;
#12011 = CARTESIAN_POINT ( 'NONE',  ( -35.00000000000000000, -11.72397916322012890, 0.7214809346828189307 ) ) ;
#12012 = CARTESIAN_POINT ( 'NONE',  ( 8.623514385631457557, 3.166471940042038025, 11.57766326477777064 ) ) ;
#12013 = CARTESIAN_POINT ( 'NONE',  ( -27.10719052120871098, -1.714424047991075506, -1.622102031466694072 ) ) ;
#12014 = DIRECTION ( 'NONE',  ( 0.000000000000000000, 0.01356324068817998940, -0.9999080150203990547 ) ) ;
#12015 = ORIENTED_EDGE ( 'NONE', *, *, #53413, .T. ) ;
#12016 = DIRECTION ( 'NONE',  ( 0.000000000000000000, 0.000000000000000000, 1.000000000000000000 ) ) ;
#12017 = ORIENTED_EDGE ( 'NONE', *, *, #46388, .F. ) ;
#12018 = CARTESIAN_POINT ( 'NONE',  ( -22.71097035706202760, 2.118550233809425087, 4.510116093748266053 ) ) ;
#12019 = AXIS2_PLACEMENT_3D ( 'NONE', #38181, #28542, #43177 ) ;
#12020 = DIRECTION ( 'NONE',  ( -1.000000000000000000, -0.000000000000000000, 0.000000000000000000 ) ) ;
#12021 = ORIENTED_EDGE ( 'NONE', *, *, #52837, .T. ) ;
#12022 = CARTESIAN_POINT ( 'NONE',  ( 3.031336079629604718, 7.553623348802402049, 2.306006909710363040 ) ) ;
#12023 = CYLINDRICAL_SURFACE ( 'NONE', #25525, 7.499999999999988454 ) ;
#12024 = CARTESIAN_POINT ( 'NONE',  ( -37.00000000000000711, -11.61175578952785159, -1.771820996347277966 ) ) ;
#12025 = EDGE_CURVE ( 'NONE', #29943, #26384, #13630, .T. ) ;
#12026 = ORIENTED_EDGE ( 'NONE', *, *, #57047, .F. ) ;
#12027 = EDGE_LOOP ( 'NONE', ( #9600, #15000, #40646, #4014 ) ) ;
#12028 = CARTESIAN_POINT ( 'NONE',  ( 2.368238019615387824, -6.736275681109187730, -3.681632831800456973 ) ) ;
#12029 = EDGE_CURVE ( 'NONE', #50930, #25928, #14289, .T. ) ;
#12030 =( BOUNDED_SURFACE ( )  B_SPLINE_SURFACE ( 3, 1, ( 
 ( #32141, #37132 ),
 ( #51489, #606 ),
 ( #51798, #16855 ),
 ( #20866, #41134 ) ),
 .UNSPECIFIED., .F., .F., .F. ) 
 B_SPLINE_SURFACE_WITH_KNOTS ( ( 4, 4 ),
 ( 2, 2 ),
 ( 0.000000000000000000, 1.000000000000000000 ),
 ( 0.000000000000000000, 1.000000000000000000 ),
 .UNSPECIFIED. ) 
 GEOMETRIC_REPRESENTATION_ITEM ( )  RATIONAL_B_SPLINE_SURFACE ( (
 ( 1.000000000000000000, 1.000000000000000000),
 ( 0.9942764183789327692, 0.8450855930916585379),
 ( 0.9942764183789327692, 0.8450855930916585379),
 ( 1.000000000000000000, 1.000000000000000000) ) ) 
 REPRESENTATION_ITEM ( '' )  SURFACE ( )  );
#12031 = ORIENTED_EDGE ( 'NONE', *, *, #18484, .F. ) ;
#12032 = CYLINDRICAL_SURFACE ( 'NONE', #47651, 13.50000000000000178 ) ;
#12033 = DIRECTION ( 'NONE',  ( 1.000000000000000000, -0.000000000000000000, 0.000000000000000000 ) ) ;
#12034 = EDGE_CURVE ( 'NONE', #59522, #44220, #54556, .T. ) ;
#12035 = CARTESIAN_POINT ( 'NONE',  ( 35.00000000000000000, 5.246972444134017977, -10.99909370905159101 ) ) ;
#12036 = CARTESIAN_POINT ( 'NONE',  ( 0.9232058338315058954, 0.3773051331667984232, 12.46548196349786330 ) ) ;
#12037 = DIRECTION ( 'NONE',  ( 0.000000000000000000, 0.000000000000000000, 1.000000000000000000 ) ) ;
#12038 = ORIENTED_EDGE ( 'NONE', *, *, #20402, .T. ) ;
#12039 = CIRCLE ( 'NONE', #58781, 4.999999999999999112 ) ;
#12040 = FACE_OUTER_BOUND ( 'NONE', #53072, .T. ) ;
#12041 = AXIS2_PLACEMENT_3D ( 'NONE', #47712, #59023, #23772 ) ;
#12042 = CIRCLE ( 'NONE', #20551, 5.000000000000000888 ) ;
#12043 = EDGE_CURVE ( 'NONE', #64838, #37589, #57504, .T. ) ;
#12044 = CARTESIAN_POINT ( 'NONE',  ( -27.30975859563925212, -13.34112994997249579, -2.066478916269102406 ) ) ;
#12045 = CARTESIAN_POINT ( 'NONE',  ( -37.00000000000000711, -11.66664283989676321, -5.143145423404404504 ) ) ;
#12046 = CARTESIAN_POINT ( 'NONE',  ( 1.948354844646953188, -3.407825014329060043, 11.46941405766422051 ) ) ;
#12047 = LINE ( 'NONE', #52638, #21122 ) ;
#12048 = CARTESIAN_POINT ( 'NONE',  ( 37.00000000000000711, 7.379373053628868639, -10.39746860227893421 ) ) ;
#12049 = CARTESIAN_POINT ( 'NONE',  ( 2.305787727787084407, -5.756228004061490822, 5.047606869483037606 ) ) ;
#12050 = CARTESIAN_POINT ( 'NONE',  ( -22.29195009621226475, -2.682867222693498643, -2.585382421603447778 ) ) ;
#12051 = CIRCLE ( 'NONE', #21620, 12.75000000000000178 ) ;
#12052 = AXIS2_PLACEMENT_3D ( 'NONE', #25090, #59350, #29101 ) ;
#12053 = EDGE_LOOP ( 'NONE', ( #38949, #11624, #4817, #27281 ) ) ;
#12054 = CARTESIAN_POINT ( 'NONE',  ( 4.913901985660861449, -9.916373276759339106, 9.161512742702274892 ) ) ;
#12055 = EDGE_CURVE ( 'NONE', #12311, #61990, #51411, .T. ) ;
#12056 = ORIENTED_EDGE ( 'NONE', *, *, #3552, .F. ) ;
#12057 = LINE ( 'NONE', #42624, #8917 ) ;
#12058 = DIRECTION ( 'NONE',  ( -1.000000000000000000, 0.000000000000000000, 0.000000000000000000 ) ) ;
#12059 = VECTOR ( 'NONE', #23154, 1000.000000000000000 ) ;
#12060 = ORIENTED_EDGE ( 'NONE', *, *, #20942, .T. ) ;
#12061 = CARTESIAN_POINT ( 'NONE',  ( 35.00000000000000000, 4.705694406421931860E-17, -3.469127814946512892E-15 ) ) ;
#12062 = ORIENTED_EDGE ( 'NONE', *, *, #18707, .F. ) ;
#12063 = DIRECTION ( 'NONE',  ( -1.000000000000000000, 0.000000000000000000, 0.000000000000000000 ) ) ;
#12064 = ORIENTED_EDGE ( 'NONE', *, *, #58178, .F. ) ;
#12065 = ORIENTED_EDGE ( 'NONE', *, *, #61498, .F. ) ;
#12066 = CARTESIAN_POINT ( 'NONE',  ( -27.08417568107323703, -1.774279301226113548, 1.449568724721383539 ) ) ;
#12067 = AXIS2_PLACEMENT_3D ( 'NONE', #6371, #46933, #1394 ) ;
#12068 = VERTEX_POINT ( 'NONE', #48580 ) ;
#12069 = CARTESIAN_POINT ( 'NONE',  ( -27.09195336418143540, -10.57949983636788716, 5.663524655488941129 ) ) ;
#12070 = CARTESIAN_POINT ( 'NONE',  ( 1.109979610371582215, -11.59954799439117679, -4.732439402374714277 ) ) ;
#12071 = CARTESIAN_POINT ( 'NONE',  ( 35.00000000000000000, -12.74068829017554094, -0.4871980014161064743 ) ) ;
#12072 = CARTESIAN_POINT ( 'NONE',  ( 35.00000000000000000, 4.705694406421931860E-17, -3.469127814946512892E-15 ) ) ;
#12073 = ORIENTED_EDGE ( 'NONE', *, *, #49188, .T. ) ;
#12074 = CARTESIAN_POINT ( 'NONE',  ( 0.2648978790185602672, -7.769924372105269761, 9.465406350830582127 ) ) ;
#12075 = CARTESIAN_POINT ( 'NONE',  ( 11.12775972613914099, -27.03492176219597454, 13.41779706364883396 ) ) ;
#12076 = CARTESIAN_POINT ( 'NONE',  ( 2.653899356900501161, -7.767552767344323428, 0.2611590963048452396 ) ) ;
#12078 = ORIENTED_EDGE ( 'NONE', *, *, #40451, .T. ) ;
#12077 = DIRECTION ( 'NONE',  ( 0.000000000000000000, -0.07632122047557189648, 0.9970832820307033995 ) ) ;
#12079 = DIRECTION ( 'NONE',  ( -1.000000000000000000, -0.000000000000000000, 0.000000000000000000 ) ) ;
#12080 = EDGE_CURVE ( 'NONE', #55105, #25248, #20584, .T. ) ;
#12081 = ORIENTED_EDGE ( 'NONE', *, *, #24004, .F. ) ;
#12082 = AXIS2_PLACEMENT_3D ( 'NONE', #31763, #47423, #32093 ) ;
#12083 = CARTESIAN_POINT ( 'NONE',  ( 2.665405856346779512, 4.274976649834481002, 8.559192023451563713 ) ) ;
#12084 = CIRCLE ( 'NONE', #26954, 12.74999999999999822 ) ;
#12085 = ORIENTED_EDGE ( 'NONE', *, *, #49283, .T. ) ;
#12086 = CARTESIAN_POINT ( 'NONE',  ( 0.2676618633000485414, 9.484212776852446680, -7.748413788583108364 ) ) ;
#12087 = CARTESIAN_POINT ( 'NONE',  ( 2.241509619876137283, -4.877966158328267632, -5.872890204493071309 ) ) ;
#12088 = EDGE_CURVE ( 'NONE', #22962, #14666, #3577, .T. ) ;
#12090 = CARTESIAN_POINT ( 'NONE',  ( 0.4626703367443957271, -4.475905684073789637, 11.46957824750455934 ) ) ;
#12089 = CIRCLE ( 'NONE', #21651, 4.999999999999998224 ) ;
#12091 = VERTEX_POINT ( 'NONE', #39562 ) ;
#12092 = LINE ( 'NONE', #22393, #25949 ) ;
#12093 = CARTESIAN_POINT ( 'NONE',  ( 3.152665057735899001, -7.886634106564667235, -0.9030954876721221103 ) ) ;
#12094 = LINE ( 'NONE', #11755, #47960 ) ;
#12095 = ORIENTED_EDGE ( 'NONE', *, *, #50102, .T. ) ;
#12096 = ORIENTED_EDGE ( 'NONE', *, *, #41396, .T. ) ;
#12097 = CARTESIAN_POINT ( 'NONE',  ( 2.931247277082681180, 7.672001188570258812, 1.728824746592295902 ) ) ;
#12098 = VERTEX_POINT ( 'NONE', #48911 ) ;
#12099 = CIRCLE ( 'NONE', #49301, 5.000000000000000888 ) ;
#12100 = ORIENTED_EDGE ( 'NONE', *, *, #63412, .F. ) ;
#12101 = CARTESIAN_POINT ( 'NONE',  ( -36.00000000000000711, -10.12742074351902311, 7.745827850122975811 ) ) ;
#12102 = CARTESIAN_POINT ( 'NONE',  ( 5.515539859299206427, -0.002856745161749602371, -0.005336559634876431209 ) ) ;
#12103 = CARTESIAN_POINT ( 'NONE',  ( 2.350038591457964454, -8.861946706686103070, -5.855794476068694188 ) ) ;
#12104 = DIRECTION ( 'NONE',  ( -1.000000000000000000, 0.000000000000000000, -0.000000000000000000 ) ) ;
#12105 = B_SPLINE_CURVE_WITH_KNOTS ( 'NONE', 3,
 ( #4387, #4049, #60889, #34927, #15641, #60225, #25634, #55578, #14644, #4729, #20658, #50270, #40257, #44931, #29964, #45582, #61214, #39614, #44582 ),
 .UNSPECIFIED., .F., .F.,
 ( 4, 3, 3, 3, 3, 3, 4 ),
 ( 5.502793334042459344E-18, 2.825908398831507014E-05, 4.208813692484323650E-05, 5.591713746944412626E-05, 6.279584083232467632E-05, 9.105792820297537013E-05, 0.0001153131102488882644 ),
 .UNSPECIFIED. ) ;
#12106 = CARTESIAN_POINT ( 'NONE',  ( 0.2638984909335720941, -6.295352574288911818, -10.50550771760526381 ) ) ;
#12107 = ADVANCED_FACE ( 'NONE', ( #54865 ), #9288, .T. ) ;
#12108 = CIRCLE ( 'NONE', #453, 12.74999999999999822 ) ;
#12109 = DIRECTION ( 'NONE',  ( 0.000000000000000000, 0.9718671068226452103, -0.2355298848897551256 ) ) ;
#12110 = FACE_OUTER_BOUND ( 'NONE', #59932, .T. ) ;
#12111 = ORIENTED_EDGE ( 'NONE', *, *, #29388, .F. ) ;
#12112 = VECTOR ( 'NONE', #41446, 1000.000000000000000 ) ;
#12113 = DIRECTION ( 'NONE',  ( -1.000000000000000000, 0.000000000000000000, 0.000000000000000000 ) ) ;
#12114 = CARTESIAN_POINT ( 'NONE',  ( -22.30986928587821438, -3.138878161034336145, 2.105440358094961883 ) ) ;
#12115 = EDGE_CURVE ( 'NONE', #10957, #35285, #30249, .T. ) ;
#12116 = CARTESIAN_POINT ( 'NONE',  ( -22.27384469013076185, 0.3730095848193410446, 3.663183248998782116 ) ) ;
#12117 = CARTESIAN_POINT ( 'NONE',  ( 35.00000000000000000, -9.733281772932100395, 8.235637554476742395 ) ) ;
#12118 = AXIS2_PLACEMENT_3D ( 'NONE', #21352, #6733, #27008 ) ;
#12119 = CARTESIAN_POINT ( 'NONE',  ( 35.00000000000000000, 9.677500615117898164, -6.657191900728355094 ) ) ;
#12120 = CARTESIAN_POINT ( 'NONE',  ( 37.00000000000000711, 12.71517666308947980, -0.9416912585474888076 ) ) ;
#12121 = CARTESIAN_POINT ( 'NONE',  ( 9.376909970675686878, 1.710254508811689389, -11.87935414277131230 ) ) ;
#12122 = B_SPLINE_CURVE_WITH_KNOTS ( 'NONE', 3,
 ( #18980, #24954, #23646, #59879, #8341, #64829, #18338, #38603, #19309, #39242, #14610, #59539, #14300 ),
 .UNSPECIFIED., .F., .F.,
 ( 4, 3, 3, 3, 4 ),
 ( 3.127317220692750759E-18, 6.607593386745478183E-05, 0.0001321518677373528946, 0.0001982171734706228655, 0.0002642860854759485002 ),
 .UNSPECIFIED. ) ;
#12123 = VERTEX_POINT ( 'NONE', #40543 ) ;
#12124 = CARTESIAN_POINT ( 'NONE',  ( 37.00000000000000711, -9.908974237959688125, -6.307491713048997362 ) ) ;
#12125 = CIRCLE ( 'NONE', #44035, 25.00000000000000000 ) ;
#12126 = DIRECTION ( 'NONE',  ( 0.000000000000000000, 0.5987040770935676548, -0.8009703041134167423 ) ) ;
#12127 = CARTESIAN_POINT ( 'NONE',  ( -27.35552965826136429, -1.320216934008378473, -2.810569013793753346 ) ) ;
#12128 = AXIS2_PLACEMENT_3D ( 'NONE', #65043, #55406, #19836 ) ;
#12129 = DIRECTION ( 'NONE',  ( -1.000000000000000000, 0.000000000000000000, 0.000000000000000000 ) ) ;
#12130 = CARTESIAN_POINT ( 'NONE',  ( 9.105565894490755596, 3.302923352347424402, -13.09178073503522910 ) ) ;
#12131 = DIRECTION ( 'NONE',  ( -1.000000000000000000, 0.000000000000000000, 0.000000000000000000 ) ) ;
#12132 = ADVANCED_FACE ( 'NONE', ( #21241 ), #34876, .T. ) ;
#12133 = CIRCLE ( 'NONE', #45042, 5.000000000000000888 ) ;
#12134 = VERTEX_POINT ( 'NONE', #328 ) ;
#12135 = CYLINDRICAL_SURFACE ( 'NONE', #6804, 12.74999999999999822 ) ;
#12136 = DIRECTION ( 'NONE',  ( 1.000000000000000000, 0.000000000000000000, 0.000000000000000000 ) ) ;
#12137 = CARTESIAN_POINT ( 'NONE',  ( 0.2759803524722238000, 9.260954523383741588, 8.018167820447541061 ) ) ;
#12138 = DIRECTION ( 'NONE',  ( 0.000000000000000000, 0.000000000000000000, -1.000000000000000000 ) ) ;
#12139 = EDGE_LOOP ( 'NONE', ( #23301, #7768, #49176, #46433 ) ) ;
#12140 = EDGE_CURVE ( 'NONE', #1113, #43258, #4649, .T. ) ;
#12141 = CARTESIAN_POINT ( 'NONE',  ( 1.948354844646903672, -8.685970062895167487, 8.228891433297592428 ) ) ;
#12142 = DIRECTION ( 'NONE',  ( 0.000000000000000000, 0.1081190184239417817, -0.9941379571543595972 ) ) ;
#12143 = VECTOR ( 'NONE', #50339, 1000.000000000000000 ) ;
#12145 = VERTEX_POINT ( 'NONE', #24939 ) ;
#12144 = CARTESIAN_POINT ( 'NONE',  ( 0.2650492433740058718, -12.24562113162319399, 0.1101179680248548648 ) ) ;
#12146 = DIRECTION ( 'NONE',  ( -0.3939253465568944290, 0.4511294145502875996, -0.8008152550167518813 ) ) ;
#12147 = VECTOR ( 'NONE', #51880, 1000.000000000000000 ) ;
#12148 = ADVANCED_FACE ( 'NONE', ( #51542 ), #50862, .T. ) ;
#12149 = PLANE ( 'NONE',  #15990 ) ;
#12150 = ORIENTED_EDGE ( 'NONE', *, *, #50672, .F. ) ;
#12151 = CARTESIAN_POINT ( 'NONE',  ( 0.3401186441510218872, -9.562489599411579277, 7.690203051555989155 ) ) ;
#12152 = DIRECTION ( 'NONE',  ( 0.000000000000000000, 0.01356324068817998940, -0.9999080150203990547 ) ) ;
#12153 = DIRECTION ( 'NONE',  ( 1.000000000000000000, 0.000000000000000000, 0.000000000000000000 ) ) ;
#12154 = CARTESIAN_POINT ( 'NONE',  ( 2.000000000000001776, 0.2704997240206042930, -6.931223712253475000 ) ) ;
#12155 = CARTESIAN_POINT ( 'NONE',  ( -8.975844149139822647, 7.740763930099402224, -9.178461504936025861 ) ) ;
#12156 = AXIS2_PLACEMENT_3D ( 'NONE', #60695, #29439, #55043 ) ;
#12157 = CARTESIAN_POINT ( 'NONE',  ( 1.104777566491147667, 11.92547689818822576, 3.832109395972688848 ) ) ;
#12159 = EDGE_LOOP ( 'NONE', ( #43513, #4594, #20185, #50163, #30589, #2120 ) ) ;
#12158 = CARTESIAN_POINT ( 'NONE',  ( 16.78263030916553333, 10.48479066935627202, 5.836879698929882565 ) ) ;
#12160 = CARTESIAN_POINT ( 'NONE',  ( 1.634816307077735287, 5.013416918609651773, -11.67158647524072990 ) ) ;
#12161 = EDGE_CURVE ( 'NONE', #58976, #39860, #51874, .T. ) ;
#12162 = ORIENTED_EDGE ( 'NONE', *, *, #52488, .F. ) ;
#12163 = CARTESIAN_POINT ( 'NONE',  ( 23.95927305399629859, -3.715110391582095328, -11.41482587237507929 ) ) ;
#12164 = VERTEX_POINT ( 'NONE', #15276 ) ;
#12165 = DIRECTION ( 'NONE',  ( -1.000000000000000000, 0.000000000000000000, 0.000000000000000000 ) ) ;
#12166 = CARTESIAN_POINT ( 'NONE',  ( -34.00000000000000000, 11.99999999999999822, 0.000000000000000000 ) ) ;
#12167 = CARTESIAN_POINT ( 'NONE',  ( -4.023199085832738220, 9.887175217721903664, 6.815337405083463196 ) ) ;
#12168 = B_SPLINE_CURVE_WITH_KNOTS ( 'NONE', 3,
 ( #53858, #60141, #14561, #39193, #64462, #59823, #14256, #54835, #8300, #8618, #24563, #34839, #55145, #29868, #43525, #54177 ),
 .UNSPECIFIED., .F., .F.,
 ( 4, 3, 3, 3, 3, 4 ),
 ( 0.000000000000000000, 0.0003017745587525263854, 0.0006035491769808769931, 0.0009053241094668204765, 0.001207275924539398439, 0.001510325902531783112 ),
 .UNSPECIFIED. ) ;
#12169 = CARTESIAN_POINT ( 'NONE',  ( -36.99853283657032677, -2.301590494557429256, 20.84413141647363688 ) ) ;
#12170 = CARTESIAN_POINT ( 'NONE',  ( -27.08421860617808363, 0.8768262158915796078, -2.116856729767833123 ) ) ;
#12171 = VERTEX_POINT ( 'NONE', #45526 ) ;
#12172 = CARTESIAN_POINT ( 'NONE',  ( 5.515539859299206427, -0.005336559634876458097, 0.002856745161749549462 ) ) ;
#12173 = CARTESIAN_POINT ( 'NONE',  ( 35.00000000000000000, -3.916263239775270577, 11.07407352312216453 ) ) ;
#12174 = ORIENTED_EDGE ( 'NONE', *, *, #31265, .F. ) ;
#12175 = ORIENTED_EDGE ( 'NONE', *, *, #10650, .F. ) ;
#12176 = CARTESIAN_POINT ( 'NONE',  ( 2.941278708680199916, 6.138172921908581436, 0.1348063076487163725 ) ) ;
#12177 = CIRCLE ( 'NONE', #37674, 12.18649999999999878 ) ;
#12178 = VERTEX_POINT ( 'NONE', #51204 ) ;
#12179 = FACE_OUTER_BOUND ( 'NONE', #50121, .T. ) ;
#12180 = CARTESIAN_POINT ( 'NONE',  ( -22.46225619532221884, 3.586917175123544688, -2.255146441673786750 ) ) ;
#12181 = CARTESIAN_POINT ( 'NONE',  ( 12.51043786959929704, 0.3316631525046854212, 11.99656223984053760 ) ) ;
#12182 = CARTESIAN_POINT ( 'NONE',  ( 2.000000000000001776, 1.018311147294167274, 6.861346417234447159 ) ) ;
#12183 = B_SPLINE_CURVE_WITH_KNOTS ( 'NONE', 3,
 ( #51345, #6111, #1455, #41987, #27037, #11401, #36350, #61291, #22037, #56657, #31365, #26370, #5795, #15722, #472, #41324 ),
 .UNSPECIFIED., .F., .F.,
 ( 4, 3, 3, 3, 3, 4 ),
 ( 0.000000000000000000, 0.0002999043160757237339, 0.0005998071753050776903, 0.0008997092107374217093, 0.001204458948194628547, 0.001510329163474499270 ),
 .UNSPECIFIED. ) ;
#12184 = DIRECTION ( 'NONE',  ( -1.000000000000000000, 0.000000000000000000, 0.000000000000000000 ) ) ;
#12185 = CARTESIAN_POINT ( 'NONE',  ( 2.440552418640496768, -7.615619946579181843, 1.142369876085300273 ) ) ;
#12186 = CARTESIAN_POINT ( 'NONE',  ( 2.241352910868908754, 7.503490710578232914, 1.407733736974891681 ) ) ;
#12187 = EDGE_LOOP ( 'NONE', ( #31726, #21562, #31215, #56409 ) ) ;
#12188 = DIRECTION ( 'NONE',  ( 1.000000000000000000, 0.000000000000000000, 0.000000000000000000 ) ) ;
#12189 = ORIENTED_EDGE ( 'NONE', *, *, #56288, .F. ) ;
#12190 = PRODUCT_DEFINITION_SHAPE ( 'NONE', 'NONE',  #65810 ) ;
#12191 = CYLINDRICAL_SURFACE ( 'NONE', #44830, 13.50000000000000178 ) ;
#12192 = CARTESIAN_POINT ( 'NONE',  ( -35.04643116707788408, 0.01193867652720184691, -0.002453861112635541408 ) ) ;
#12193 = AXIS2_PLACEMENT_3D ( 'NONE', #23653, #13647, #33931 ) ;
#12194 = CARTESIAN_POINT ( 'NONE',  ( 2.261269890822073858, -3.940687015735691467, 6.546486799463097306 ) ) ;
#12195 = CARTESIAN_POINT ( 'NONE',  ( -27.01437459610461644, 13.31613970204373132, -2.220455681983952267 ) ) ;
#12196 = AXIS2_PLACEMENT_3D ( 'NONE', #56680, #50379, #4826 ) ;
#12197 = VERTEX_POINT ( 'NONE', #20607 ) ;
#12198 = EDGE_CURVE ( 'NONE', #45280, #167, #5989, .T. ) ;
#12199 = VERTEX_POINT ( 'NONE', #55851 ) ;
#12200 = DIRECTION ( 'NONE',  ( -1.000000000000000000, 0.000000000000000000, 0.000000000000000000 ) ) ;
#12201 = ORIENTED_EDGE ( 'NONE', *, *, #53760, .F. ) ;
#12202 = CARTESIAN_POINT ( 'NONE',  ( 0.2801149460245155876, 7.723514566794102087, -9.509848747524097590 ) ) ;
#12203 = CARTESIAN_POINT ( 'NONE',  ( 8.437200413559441614, 4.476360154859203355, 11.13383131558893346 ) ) ;
#12204 = CARTESIAN_POINT ( 'NONE',  ( 0.4613984246114878340, -9.610550265395797709, -7.694922453052239320 ) ) ;
#12205 = CARTESIAN_POINT ( 'NONE',  ( 3.152665057735933640, -5.461013642407022139, -5.761241965768077122 ) ) ;
#12206 = VERTEX_POINT ( 'NONE', #60836 ) ;
#12207 = DIRECTION ( 'NONE',  ( 0.000000000000000000, 0.2960891610144510966, 0.9551603052523478521 ) ) ;
#12208 = LINE ( 'NONE', #46478, #51274 ) ;
#12209 = CARTESIAN_POINT ( 'NONE',  ( -28.41827485489077532, 3.509237424706437292, -13.03592162821790801 ) ) ;
#12210 = CARTESIAN_POINT ( 'NONE',  ( -22.31328051695926007, 2.109671368890633669, 3.148362328073145200 ) ) ;
#12211 = AXIS2_PLACEMENT_3D ( 'NONE', #5433, #29686, #30365 ) ;
#12212 = EDGE_CURVE ( 'NONE', #10842, #19771, #26245, .T. ) ;
#12213 = CARTESIAN_POINT ( 'NONE',  ( 0.2869720083484346707, 6.306330337780659434, -10.50600528807140321 ) ) ;
#12214 = DIRECTION ( 'NONE',  ( 0.000000000000000000, 0.000000000000000000, 1.000000000000000000 ) ) ;
#12215 =( BOUNDED_CURVE ( )  B_SPLINE_CURVE ( 3, ( #52482, #54439, #64700, #34762 ),
 .UNSPECIFIED., .F., .F. ) 
 B_SPLINE_CURVE_WITH_KNOTS ( ( 4, 4 ),
 ( 4.045341626114011824, 4.054895942073102333 ),
 .UNSPECIFIED. ) 
 CURVE ( )  GEOMETRIC_REPRESENTATION_ITEM ( )  RATIONAL_B_SPLINE_CURVE ( ( 1.000000000000000000, 0.9999923929350129637, 0.9999923929350129637, 1.000000000000000000 ) ) 
 REPRESENTATION_ITEM ( '' )  );
#12216 = ADVANCED_FACE ( 'NONE', ( #14595 ), #46519, .T. ) ;
#12217 = EDGE_LOOP ( 'NONE', ( #30649, #30870, #60462, #10412 ) ) ;
#12218 = EDGE_CURVE ( 'NONE', #20405, #22815, #5654, .T. ) ;
#12219 = CARTESIAN_POINT ( 'NONE',  ( -14.32520573871325631, -34.50054679313745964, -8.085438606780256166 ) ) ;
#12220 = ORIENTED_EDGE ( 'NONE', *, *, #34931, .T. ) ;
#12221 = EDGE_CURVE ( 'NONE', #59141, #40799, #50315, .T. ) ;
#12222 = CARTESIAN_POINT ( 'NONE',  ( -6.726017918545671215, -1.195345798906086277, -13.44716762434733681 ) ) ;
#12223 = CARTESIAN_POINT ( 'NONE',  ( 37.00000000000000711, -4.946702696913249930, -11.13736569743272931 ) ) ;
#12224 = CARTESIAN_POINT ( 'NONE',  ( 0.2646305136544072623, 12.24595685781654630, 0.1321451301298244563 ) ) ;
#12225 =( GEOMETRIC_REPRESENTATION_CONTEXT ( 3 ) GLOBAL_UNCERTAINTY_ASSIGNED_CONTEXT ( ( #62502 ) ) GLOBAL_UNIT_ASSIGNED_CONTEXT ( ( #50461, #26163, #16174 ) ) REPRESENTATION_CONTEXT ( 'NONE', 'WORKASPACE' ) );
#12226 = FACE_OUTER_BOUND ( 'NONE', #41959, .T. ) ;
#12227 = CARTESIAN_POINT ( 'NONE',  ( 0.2648978790185619880, -11.46165506714231341, 4.312320170909196726 ) ) ;
#12228 = ORIENTED_EDGE ( 'NONE', *, *, #51005, .F. ) ;
#12230 = ORIENTED_EDGE ( 'NONE', *, *, #59724, .F. ) ;
#12229 = ADVANCED_FACE ( 'NONE', ( #25923 ), #56504, .T. ) ;
#12231 = DIRECTION ( 'NONE',  ( 0.000000000000000000, 0.000000000000000000, 1.000000000000000000 ) ) ;
#12232 = ORIENTED_EDGE ( 'NONE', *, *, #56078, .T. ) ;
#12233 = DIRECTION ( 'NONE',  ( -1.000000000000000000, 0.000000000000000000, 0.000000000000000000 ) ) ;
#12235 = AXIS2_PLACEMENT_3D ( 'NONE', #42202, #27580, #27261 ) ;
#12234 = DIRECTION ( 'NONE',  ( -1.000000000000000000, 0.000000000000000000, 0.000000000000000000 ) ) ;
#12236 = CARTESIAN_POINT ( 'NONE',  ( 35.00000000000000000, -10.43555801961471552, 5.391785509271064925 ) ) ;
#12237 = CARTESIAN_POINT ( 'NONE',  ( 2.241451721903216843, 0.06083185034806753988, -7.634225434981126490 ) ) ;
#12238 = CARTESIAN_POINT ( 'NONE',  ( 37.00000000000000711, 4.705694406421931860E-17, -3.469127814946512892E-15 ) ) ;
#12239 = EDGE_CURVE ( 'NONE', #42211, #11101, #11427, .T. ) ;
#12240 = CARTESIAN_POINT ( 'NONE',  ( 2.241311220309654129, 5.788190037953024003, 4.978033760028732324 ) ) ;
#12241 = PLANE ( 'NONE',  #5341 ) ;
#12242 = ORIENTED_EDGE ( 'NONE', *, *, #38292, .F. ) ;
#12243 = ORIENTED_EDGE ( 'NONE', *, *, #39840, .F. ) ;
#12244 = DIRECTION ( 'NONE',  ( 0.000000000000000000, -0.8835120444460271560, 0.4684084406997820471 ) ) ;
#12245 = ORIENTED_EDGE ( 'NONE', *, *, #22517, .T. ) ;
#12247 = CARTESIAN_POINT ( 'NONE',  ( -35.00000000000000000, 10.12742074351907462, -7.745827850122902092 ) ) ;
#12246 = AXIS2_PLACEMENT_3D ( 'NONE', #13162, #38762, #34422 ) ;
#12248 = CARTESIAN_POINT ( 'NONE',  ( 35.00000000000000000, -3.213188559034160452, 11.29812557209479706 ) ) ;
#12249 = EDGE_CURVE ( 'NONE', #63399, #22582, #10948, .T. ) ;
#12250 = CARTESIAN_POINT ( 'NONE',  ( -22.30527770659433173, -1.656864125491245066, 3.381761229713381667 ) ) ;
#12251 = ORIENTED_EDGE ( 'NONE', *, *, #32527, .F. ) ;
#12252 = CARTESIAN_POINT ( 'NONE',  ( -14.53304282576173279, -30.00000000000001066, -3.713578627762639250 ) ) ;
#12253 = CARTESIAN_POINT ( 'NONE',  ( 35.00000000000000000, -10.28547182238011715, -5.672855678558653914 ) ) ;
#12254 = ORIENTED_EDGE ( 'NONE', *, *, #20797, .F. ) ;
#12255 = ORIENTED_EDGE ( 'NONE', *, *, #31359, .F. ) ;
#12256 = CARTESIAN_POINT ( 'NONE',  ( 35.00000000000000000, 4.705694406421931860E-17, -3.469127814946512892E-15 ) ) ;
#12257 = ORIENTED_EDGE ( 'NONE', *, *, #7061, .T. ) ;
#12258 = ORIENTED_EDGE ( 'NONE', *, *, #3565, .T. ) ;
#12259 = CARTESIAN_POINT ( 'NONE',  ( 2.242418902651940993, 3.903399295463838126, 6.561482094363259243 ) ) ;
#12260 = ORIENTED_EDGE ( 'NONE', *, *, #37692, .F. ) ;
#12261 = ORIENTED_EDGE ( 'NONE', *, *, #16220, .F. ) ;
#12262 = CARTESIAN_POINT ( 'NONE',  ( -22.27709082389155171, -2.641652894015110054, 2.563977319272121580 ) ) ;
#12263 = CYLINDRICAL_SURFACE ( 'NONE', #36861, 6.936499999999988120 ) ;
#12264 = CIRCLE ( 'NONE', #38803, 12.18649999999999878 ) ;
#12265 = DIRECTION ( 'NONE',  ( -1.000000000000000000, -0.000000000000000000, 0.000000000000000000 ) ) ;
#12266 = CARTESIAN_POINT ( 'NONE',  ( 35.00000000000000000, -12.12087942037208776, 1.262958560998883595 ) ) ;
#12267 = FACE_OUTER_BOUND ( 'NONE', #33248, .T. ) ;
#12268 = LINE ( 'NONE', #37203, #2507 ) ;
#12269 = ORIENTED_EDGE ( 'NONE', *, *, #49502, .T. ) ;
#12270 = DIRECTION ( 'NONE',  ( -1.000000000000000000, 0.000000000000000000, 0.000000000000000000 ) ) ;
#12271 = CARTESIAN_POINT ( 'NONE',  ( 3.152665057734086229, 4.725420687650732532, 6.378477742800449768 ) ) ;
#12272 = CARTESIAN_POINT ( 'NONE',  ( 0.2655924914740778742, 0.04405032194303384191, 12.24627751708824341 ) ) ;
#12273 = CARTESIAN_POINT ( 'NONE',  ( 0.3675815128205912052, -2.391755495700685241, 12.04510820461658582 ) ) ;
#12274 = CARTESIAN_POINT ( 'NONE',  ( 2.000000000000001776, 0.000000000000000000, 0.000000000000000000 ) ) ;
#12275 = CARTESIAN_POINT ( 'NONE',  ( 0.2834382757448011270, -11.58108645293228633, -3.999440312567330569 ) ) ;
#12276 = EDGE_CURVE ( 'NONE', #57461, #17645, #33304, .T. ) ;
#12277 = VERTEX_POINT ( 'NONE', #42164 ) ;
#12278 = DIRECTION ( 'NONE',  ( -1.000000000000000000, 0.000000000000000000, 0.000000000000000000 ) ) ;
#12279 = VECTOR ( 'NONE', #62027, 1000.000000000000000 ) ;
#12280 = VERTEX_POINT ( 'NONE', #12560 ) ;
#12281 = CARTESIAN_POINT ( 'NONE',  ( 2.298277635560276089, 5.967558917212202552, -4.791911337974113394 ) ) ;
#12282 = DIRECTION ( 'NONE',  ( 1.000000000000000000, -0.000000000000000000, 0.000000000000000000 ) ) ;
#12283 = CARTESIAN_POINT ( 'NONE',  ( -35.00000000000000000, 0.000000000000000000, 0.000000000000000000 ) ) ;
#12284 = CARTESIAN_POINT ( 'NONE',  ( 25.00000000000000355, -30.00000000000000000, 1.530808498934191521E-15 ) ) ;
#12285 = VERTEX_POINT ( 'NONE', #1315 ) ;
#12286 = EDGE_CURVE ( 'NONE', #39344, #34948, #32514, .T. ) ;
#12287 = CARTESIAN_POINT ( 'NONE',  ( 37.00000000000000711, -11.73555825188272905, 4.983891302653699285 ) ) ;
#12288 = DIRECTION ( 'NONE',  ( 0.000000000000000000, 8.881784197001252323E-16, 1.000000000000000000 ) ) ;
#12289 = CARTESIAN_POINT ( 'NONE',  ( -19.02967556479643463, -13.50000000000023803, -2.066764320408402454E-13 ) ) ;
#12290 = CARTESIAN_POINT ( 'NONE',  ( -35.00000000000000000, 7.817610399097512541, 8.766823244862019138 ) ) ;
#12291 = AXIS2_PLACEMENT_3D ( 'NONE', #53333, #32677, #11436 ) ;
#12292 = ADVANCED_FACE ( 'NONE', ( #52519 ), #11454, .F. ) ;
#12293 = CARTESIAN_POINT ( 'NONE',  ( -22.59983133926798615, -2.378226455340827439, 3.996991822164148278 ) ) ;
#12294 = ORIENTED_EDGE ( 'NONE', *, *, #37073, .F. ) ;
#12295 = EDGE_CURVE ( 'NONE', #56700, #27528, #46081, .T. ) ;
#12296 = CARTESIAN_POINT ( 'NONE',  ( 1.719304012338701115, -5.690355757827699534, 11.38834240361771677 ) ) ;
#12297 = EDGE_CURVE ( 'NONE', #36193, #64644, #27882, .T. ) ;
#12298 = CARTESIAN_POINT ( 'NONE',  ( 2.263328370261528111, -3.943189046766291117, -6.545781832005235223 ) ) ;
#12299 = ORIENTED_EDGE ( 'NONE', *, *, #8566, .F. ) ;
#12300 = VERTEX_POINT ( 'NONE', #57832 ) ;
#12301 = CARTESIAN_POINT ( 'NONE',  ( 2.276905613633651626, -6.543460433228672990, 3.955794200962185592 ) ) ;
#12302 = CARTESIAN_POINT ( 'NONE',  ( 2.305787727787084407, -3.682701754025465846, -6.711944854845862451 ) ) ;
#12303 = CARTESIAN_POINT ( 'NONE',  ( -27.08935880048753120, -1.653090150966153526, -1.608762129670104235 ) ) ;
#12304 = CARTESIAN_POINT ( 'NONE',  ( 1.372161826076364388, -7.648244077827067500, 10.03232826862070759 ) ) ;
#12305 = EDGE_CURVE ( 'NONE', #266, #7420, #16917, .T. ) ;
#12306 = CARTESIAN_POINT ( 'NONE',  ( 2.305787727787083519, -6.711944854845849129, 3.682701754025489826 ) ) ;
#12307 = ORIENTED_EDGE ( 'NONE', *, *, #37969, .T. ) ;
#12308 = EDGE_CURVE ( 'NONE', #27547, #54995, #47131, .T. ) ;
#12310 = ORIENTED_EDGE ( 'NONE', *, *, #889, .F. ) ;
#12309 = B_SPLINE_CURVE_WITH_KNOTS ( 'NONE', 3,
 ( #47011, #1466, #62276, #32013, #52334, #58293, #43304, #43635, #57975, #63579, #3103, #28037, #63920, #53307, #2787, #43977, #12384, #27684, #19621 ),
 .UNSPECIFIED., .F., .F.,
 ( 4, 3, 3, 3, 3, 3, 4 ),
 ( 5.311484201212962216E-18, 2.825908398831288479E-05, 4.208813692483985515E-05, 5.591713746943959972E-05, 6.279584083232024464E-05, 9.105792820296832281E-05, 0.0001153131102488849034 ),
 .UNSPECIFIED. ) ;
#12311 = VERTEX_POINT ( 'NONE', #41857 ) ;
#12312 = DIRECTION ( 'NONE',  ( 0.000000000000000000, 0.8369827122275325104, 0.5472293298355300761 ) ) ;
#12313 = ADVANCED_FACE ( 'NONE', ( #53150 ), #22227, .T. ) ;
#12314 = CARTESIAN_POINT ( 'NONE',  ( 1.719304012338199517, 0.000000000000000000, 0.000000000000000000 ) ) ;
#12315 = ORIENTED_EDGE ( 'NONE', *, *, #27047, .T. ) ;
#12316 = AXIS2_PLACEMENT_3D ( 'NONE', #13086, #18746, #58663 ) ;
#12317 = DIRECTION ( 'NONE',  ( 0.000000000000000000, -0.01356324068817991828, 0.9999080150203990547 ) ) ;
#12318 = ADVANCED_FACE ( 'NONE', ( #17252 ), #37527, .T. ) ;
#12319 = CARTESIAN_POINT ( 'NONE',  ( 2.298277635560283194, -7.564013289873168233, 1.166137492762201022 ) ) ;
#12320 = ORIENTED_EDGE ( 'NONE', *, *, #16255, .F. ) ;
#12321 = AXIS2_PLACEMENT_3D ( 'NONE', #46007, #35991, #15069 ) ;
#12322 = CARTESIAN_POINT ( 'NONE',  ( 0.000000000000000000, -6.539067737394502089, 2.314222412769776138 ) ) ;
#12323 = B_SPLINE_CURVE_WITH_KNOTS ( 'NONE', 3,
 ( #56746, #41747, #31445, #6190, #26451, #46735, #21476, #42062, #62041, #57377, #16491, #16799, #36760, #32085, #57056, #52402 ),
 .UNSPECIFIED., .F., .F.,
 ( 4, 3, 3, 3, 3, 4 ),
 ( 3.270724739007979762E-15, 0.0002126834539179725146, 0.0004253519300366287925, 0.0006380165497224213767, 0.0007442707582428297443, 0.0009453531351416891940 ),
 .UNSPECIFIED. ) ;
#12324 = CARTESIAN_POINT ( 'NONE',  ( 2.241352910868908310, -2.689314586382304917, -7.145045428366603169 ) ) ;
#12325 = CARTESIAN_POINT ( 'NONE',  ( 2.245754705088788938, 7.136529175883056908, 2.715960966013291067 ) ) ;
#12326 = EDGE_LOOP ( 'NONE', ( #19273, #19333, #51960, #17542 ) ) ;
#12328 = EDGE_CURVE ( 'NONE', #42485, #21663, #16318, .T. ) ;
#12327 = EDGE_LOOP ( 'NONE', ( #64513, #40676, #57571, #30622 ) ) ;
#12329 = CARTESIAN_POINT ( 'NONE',  ( 2.241352910868908754, 2.532612177304442991, 7.202080440908749992 ) ) ;
#12330 = ORIENTED_EDGE ( 'NONE', *, *, #49325, .F. ) ;
#12331 = LINE ( 'NONE', #44233, #45525 ) ;
#12332 = ORIENTED_EDGE ( 'NONE', *, *, #61600, .F. ) ;
#12333 = CARTESIAN_POINT ( 'NONE',  ( 1.719304012341584365, 10.22720798541559439, -7.581471372738991299 ) ) ;
#12334 = CARTESIAN_POINT ( 'NONE',  ( 9.537768711902334218, -32.77116127932245604, -12.15562491791137134 ) ) ;
#12335 = CYLINDRICAL_SURFACE ( 'NONE', #44306, 5.000000000000000888 ) ;
#12336 = DIRECTION ( 'NONE',  ( 0.000000000000000000, -1.000000000000000000, 0.000000000000000000 ) ) ;
#12337 = CARTESIAN_POINT ( 'NONE',  ( 8.812247137149384457, 2.657441218557111906, 11.70499198588243850 ) ) ;
#12338 = CARTESIAN_POINT ( 'NONE',  ( 1.198791140420808699, 6.720248575444026429, -10.60778679489420284 ) ) ;
#12339 = DIRECTION ( 'NONE',  ( -1.000000000000000000, 0.000000000000000000, 0.000000000000000000 ) ) ;
#12340 = ORIENTED_EDGE ( 'NONE', *, *, #12295, .T. ) ;
#12341 = CARTESIAN_POINT ( 'NONE',  ( -35.00000000000000000, 0.000000000000000000, 0.000000000000000000 ) ) ;
#12342 = ORIENTED_EDGE ( 'NONE', *, *, #12955, .T. ) ;
#12343 = FACE_OUTER_BOUND ( 'NONE', #40947, .T. ) ;
#12344 = CARTESIAN_POINT ( 'NONE',  ( 2.241317068080787678, 6.656851426546641193, 3.737686401541526315 ) ) ;
#12345 = EDGE_LOOP ( 'NONE', ( #35920, #60567, #41456, #56165 ) ) ;
#12346 = CARTESIAN_POINT ( 'NONE',  ( 2.000000000000001776, -6.767909380267597363, -0.7805499053121327524 ) ) ;
#12347 = DIRECTION ( 'NONE',  ( -1.000000000000000000, 0.000000000000000000, -0.000000000000000000 ) ) ;
#12348 = CARTESIAN_POINT ( 'NONE',  ( 2.969415267404084791, -7.680649281077092105, 1.748187016698054652 ) ) ;
#12349 = ORIENTED_EDGE ( 'NONE', *, *, #36763, .F. ) ;
#12350 = ADVANCED_FACE ( 'NONE', ( #37854 ), #21592, .T. ) ;
#12351 = ORIENTED_EDGE ( 'NONE', *, *, #36235, .T. ) ;
#12352 = CARTESIAN_POINT ( 'NONE',  ( 3.152665057736261822, -7.102135024647099115, -3.546019893114602972 ) ) ;
#12353 = ORIENTED_EDGE ( 'NONE', *, *, #48623, .F. ) ;
#12354 = DIRECTION ( 'NONE',  ( -1.000000000000000000, 0.000000000000000000, 0.000000000000000000 ) ) ;
#12355 = DIRECTION ( 'NONE',  ( 0.000000000000000000, 0.000000000000000000, 1.000000000000000000 ) ) ;
#12356 = CARTESIAN_POINT ( 'NONE',  ( 0.000000000000000000, 0.000000000000000000, 0.000000000000000000 ) ) ;
#12357 = CARTESIAN_POINT ( 'NONE',  ( -19.41624570965199581, -4.334582023309537568, 11.19068518931768352 ) ) ;
#12358 = ORIENTED_EDGE ( 'NONE', *, *, #13420, .F. ) ;
#12359 = EDGE_CURVE ( 'NONE', #6959, #38911, #7816, .T. ) ;
#12360 = AXIS2_PLACEMENT_3D ( 'NONE', #59619, #14682, #20350 ) ;
#12361 = DIRECTION ( 'NONE',  ( -1.000000000000000000, 0.000000000000000000, 0.000000000000000000 ) ) ;
#12362 = CARTESIAN_POINT ( 'NONE',  ( 2.963017218115624019, -7.679262289252030804, -1.744728040076983788 ) ) ;
#12363 = CARTESIAN_POINT ( 'NONE',  ( -2.952869152607107139, -12.96714474214480717, 3.755417052241487585 ) ) ;
#12364 = CARTESIAN_POINT ( 'NONE',  ( 2.000000000000001776, -6.643843315911820646, 1.507714007300648307 ) ) ;
#12365 = DIRECTION ( 'NONE',  ( 0.000000000000000000, -0.6876994588534294239, 0.7259954919231249582 ) ) ;
#12366 = EDGE_CURVE ( 'NONE', #2801, #37153, #46850, .T. ) ;
#12367 = CYLINDRICAL_SURFACE ( 'NONE', #28817, 5.000000000000000888 ) ;
#12368 = CARTESIAN_POINT ( 'NONE',  ( 2.273267844204863053, -5.758000272829339572, 5.029122824445697582 ) ) ;
#12369 = CARTESIAN_POINT ( 'NONE',  ( 2.931247277082693614, 5.333206743525327198, -5.779735553870047227 ) ) ;
#12370 = VERTEX_POINT ( 'NONE', #11279 ) ;
#12371 = CARTESIAN_POINT ( 'NONE',  ( 2.241352910868908310, -4.970878533273800137, 5.794346703933830334 ) ) ;
#12372 = FACE_OUTER_BOUND ( 'NONE', #27192, .T. ) ;
#12373 = ORIENTED_EDGE ( 'NONE', *, *, #42927, .F. ) ;
#12374 = CARTESIAN_POINT ( 'NONE',  ( -22.30527770659433173, 3.757123197210718857, -0.2559941915621641306 ) ) ;
#12375 = DIRECTION ( 'NONE',  ( 1.000000000000000000, 0.000000000000000000, 0.000000000000000000 ) ) ;
#12376 = ORIENTED_EDGE ( 'NONE', *, *, #28603, .T. ) ;
#12377 = UNCERTAINTY_MEASURE_WITH_UNIT (LENGTH_MEASURE( 1.000000000000000082E-05 ), #22659, 'distance_accuracy_value', 'NONE');
#12378 = CARTESIAN_POINT ( 'NONE',  ( 2.241451721903215066, 4.953785420083490543, -5.809054012306810399 ) ) ;
#12379 = EDGE_LOOP ( 'NONE', ( #17395, #7469, #22139, #6567 ) ) ;
#12380 = CARTESIAN_POINT ( 'NONE',  ( 35.00000000000000000, 4.705694406421931860E-17, -3.469127814946512892E-15 ) ) ;
#12381 = ORIENTED_EDGE ( 'NONE', *, *, #5872, .T. ) ;
#12382 = ORIENTED_EDGE ( 'NONE', *, *, #61056, .T. ) ;
#12383 = EDGE_CURVE ( 'NONE', #19103, #14524, #57166, .T. ) ;
#12384 = CARTESIAN_POINT ( 'NONE',  ( 2.242418902651940549, -7.139616612143407259, 2.704708480794779657 ) ) ;
#12385 = VERTEX_POINT ( 'NONE', #62144 ) ;
#12386 = EDGE_CURVE ( 'NONE', #27171, #36886, #37580, .T. ) ;
#12387 = DIRECTION ( 'NONE',  ( 1.000000000000000000, 0.000000000000000000, 0.000000000000000000 ) ) ;
#12388 = CARTESIAN_POINT ( 'NONE',  ( 1.637652121266425231, 0.7383001981046479756, 13.48328331344350062 ) ) ;
#12389 = CARTESIAN_POINT ( 'NONE',  ( 32.00000000000000000, 1.230770033143089974E-14, 0.000000000000000000 ) ) ;
#12390 = DIRECTION ( 'NONE',  ( -1.000000000000000000, 0.000000000000000000, 0.000000000000000000 ) ) ;
#12391 = ORIENTED_EDGE ( 'NONE', *, *, #58580, .F. ) ;
#12392 = CARTESIAN_POINT ( 'NONE',  ( 2.889800649504073782, 1.129261637821690423, -6.016320774579795305 ) ) ;
#12393 = CARTESIAN_POINT ( 'NONE',  ( -22.39032720737627358, -3.916738514147019679, -0.9101257950221066650 ) ) ;
#12395 = ORIENTED_EDGE ( 'NONE', *, *, #62981, .F. ) ;
#12394 = DIRECTION ( 'NONE',  ( 0.000000000000000000, 0.01356324068817991481, -0.9999080150203990547 ) ) ;
#12396 = ADVANCED_FACE ( 'NONE', ( #8570 ), #49797, .T. ) ;
#12397 = LINE ( 'NONE', #27371, #6583 ) ;
#12398 = ORIENTED_EDGE ( 'NONE', *, *, #56528, .T. ) ;
#12399 = CARTESIAN_POINT ( 'NONE',  ( -37.00000000000000711, 3.805206332242643263, -12.16893194857546412 ) ) ;
#12400 = VERTEX_POINT ( 'NONE', #33831 ) ;
#12401 = CIRCLE ( 'NONE', #49603, 12.18650000000000055 ) ;
#12402 = FACE_OUTER_BOUND ( 'NONE', #17763, .T. ) ;
#12403 = DIRECTION ( 'NONE',  ( -1.000000000000000000, 0.000000000000000000, -0.000000000000000000 ) ) ;
#12404 = DIRECTION ( 'NONE',  ( -1.000000000000000000, 0.000000000000000000, 0.000000000000000000 ) ) ;
#12405 = EDGE_LOOP ( 'NONE', ( #31234, #7099, #38833, #12162 ) ) ;
#12406 = DIRECTION ( 'NONE',  ( 0.000000000000000000, 0.01356324068817998940, -0.9999080150203990547 ) ) ;
#12407 = AXIS2_PLACEMENT_3D ( 'NONE', #63838, #18320, #38587 ) ;
#12408 = DIRECTION ( 'NONE',  ( 0.000000000000000000, -0.9289767198167871998, -0.3701381553399247792 ) ) ;
#12409 = CARTESIAN_POINT ( 'NONE',  ( -22.27710395300133328, -3.549456197028680648, -0.9764373854729214708 ) ) ;
#12410 = ORIENTED_EDGE ( 'NONE', *, *, #47772, .F. ) ;
#12411 =( BOUNDED_CURVE ( )  B_SPLINE_CURVE ( 3, ( #43814, #22212, #64096, #18575 ),
 .UNSPECIFIED., .F., .F. ) 
 B_SPLINE_CURVE_WITH_KNOTS ( ( 4, 4 ),
 ( 4.494179741888913782, 4.524178010218698809 ),
 .UNSPECIFIED. ) 
 CURVE ( )  GEOMETRIC_REPRESENTATION_ITEM ( )  RATIONAL_B_SPLINE_CURVE ( ( 1.000000000000000000, 0.9999250100640160177, 0.9999250100640160177, 1.000000000000000000 ) ) 
 REPRESENTATION_ITEM ( '' )  );
#12412 = ORIENTED_EDGE ( 'NONE', *, *, #36734, .T. ) ;
#12413 = CARTESIAN_POINT ( 'NONE',  ( 0.2648321136542672871, 12.03456865502706208, 2.265911310221853991 ) ) ;
#12414 = VERTEX_POINT ( 'NONE', #19205 ) ;
#12415 = VERTEX_POINT ( 'NONE', #13866 ) ;
#12416 = CARTESIAN_POINT ( 'NONE',  ( 35.00000000000000000, 11.98254675519227952, -2.220215194441947482 ) ) ;
#12417 = CARTESIAN_POINT ( 'NONE',  ( -22.27704833740210333, 3.351945466913931693, 1.521679877253146351 ) ) ;
#12418 = CARTESIAN_POINT ( 'NONE',  ( 2.241526690369558761, -7.179945570618739836, -2.594870554108910543 ) ) ;
#12419 = CARTESIAN_POINT ( 'NONE',  ( 0.3675815128205912052, -12.13672785388549080, -1.872154644482208585 ) ) ;
#12420 = CYLINDRICAL_SURFACE ( 'NONE', #14626, 2.899999999999994582 ) ;
#12421 = CARTESIAN_POINT ( 'NONE',  ( 0.000000000000000000, -4.376687952327290354, -5.220963330856675633 ) ) ;
#12422 = EDGE_CURVE ( 'NONE', #55363, #23613, #17402, .T. ) ;
#12423 = DIRECTION ( 'NONE',  ( -1.000000000000000000, -1.836970198721029688E-16, 0.000000000000000000 ) ) ;
#12424 = EDGE_CURVE ( 'NONE', #23282, #48840, #64103, .T. ) ;
#12425 = ORIENTED_EDGE ( 'NONE', *, *, #6531, .F. ) ;
#12426 = LINE ( 'NONE', #36133, #25995 ) ;
#12427 = CYLINDRICAL_SURFACE ( 'NONE', #6309, 12.74999999999999822 ) ;
#12428 = EDGE_CURVE ( 'NONE', #64891, #61666, #35421, .T. ) ;
#12429 = B_SPLINE_CURVE_WITH_KNOTS ( 'NONE', 3,
 ( #48933, #9006, #47938, #42939, #7702, #2741, #22999, #58587, #13013, #33295, #53598, #8042, #28306, #48601, #38612, #3388, #58926, #13338, #23657 ),
 .UNSPECIFIED., .F., .F.,
 ( 4, 3, 3, 3, 3, 3, 4 ),
 ( 4.336808689942017736E-19, 2.831840207499681410E-05, 4.217266859840561197E-05, 5.602024318395812120E-05, 6.290810167968882650E-05, 9.120440630945197459E-05, 0.0001153103026479751004 ),
 .UNSPECIFIED. ) ;
#12430 = CARTESIAN_POINT ( 'NONE',  ( 2.280717697723841919, -4.794838658391056718, 5.957695241725387447 ) ) ;
#12431 = DIRECTION ( 'NONE',  ( 0.000000000000000000, 0.01356324068817998940, -0.9999080150203990547 ) ) ;
#12432 = CARTESIAN_POINT ( 'NONE',  ( 2.241352910868908310, 6.569501556381442953, 3.889181972941473386 ) ) ;
#12433 = DIRECTION ( 'NONE',  ( 1.000000000000000000, 0.000000000000000000, 0.000000000000000000 ) ) ;
#12434 = CARTESIAN_POINT ( 'NONE',  ( 8.937200413559445167, 4.247489200464594994, -11.22584895011355144 ) ) ;
#12435 = EDGE_CURVE ( 'NONE', #9473, #61317, #36026, .T. ) ;
#12437 = ORIENTED_EDGE ( 'NONE', *, *, #4717, .T. ) ;
#12436 = EDGE_CURVE ( 'NONE', #25992, #51508, #54589, .T. ) ;
#12438 = FACE_OUTER_BOUND ( 'NONE', #19316, .T. ) ;
#12439 = CARTESIAN_POINT ( 'NONE',  ( -35.00000000000000000, 0.000000000000000000, 0.000000000000000000 ) ) ;
#12440 = DIRECTION ( 'NONE',  ( -0.000000000000000000, -0.000000000000000000, -1.000000000000000000 ) ) ;
#12441 = CARTESIAN_POINT ( 'NONE',  ( 3.092491956585992074, -1.813286239165846636, -7.707758057368695681 ) ) ;
#12442 = AXIS2_PLACEMENT_3D ( 'NONE', #39160, #59455, #23904 ) ;
#12443 = EDGE_CURVE ( 'NONE', #60039, #21190, #59443, .T. ) ;
#12444 = B_SPLINE_CURVE_WITH_KNOTS ( 'NONE', 3,
 ( #29701, #2839, #35350, #30375, #25067, #30041, #465, #55659, #24739, #40678, #51335, #15407, #10095, #4468, #40332, #40014, #50991, #25717, #45017, #35676, #35003, #773, #50009, #50670, #65292, #61598 ),
 .UNSPECIFIED., .F., .F.,
 ( 4, 2, 2, 2, 2, 2, 2, 2, 2, 2, 2, 2, 4 ),
 ( 0.000000000000000000, 0.001405882151622312804, 0.002811764303244625608, 0.004217646454866938628, 0.005623528606489251215, 0.008435292909733880726, 0.01124705721297850763, 0.01265293936460081849, 0.01405882151622312760, 0.01687058581946774410, 0.01827646797109005322, 0.01968235012271236581, 0.02249411442595698057 ),
 .UNSPECIFIED. ) ;
#12445 = CIRCLE ( 'NONE', #49651, 12.18650000000000055 ) ;
#12446 = FACE_OUTER_BOUND ( 'NONE', #43003, .T. ) ;
#12447 = CARTESIAN_POINT ( 'NONE',  ( -26.94662368254203244, -12.23618042240103243, 5.703482483425735161 ) ) ;
#12448 = ORIENTED_EDGE ( 'NONE', *, *, #43979, .T. ) ;
#12449 = CARTESIAN_POINT ( 'NONE',  ( 2.177405672431146133, 8.129711416440880356, -7.702458780351681078 ) ) ;
#12450 = CARTESIAN_POINT ( 'NONE',  ( 0.9232058338315048962, -1.793035206307261875, -12.34162163148535463 ) ) ;
#12451 = CARTESIAN_POINT ( 'NONE',  ( 0.3218525148189844698, 9.236582760335979359, 8.069481661595380828 ) ) ;
#12452 = CARTESIAN_POINT ( 'NONE',  ( -22.27384469013076185, 3.663183248998794106, -0.3730095848193202279 ) ) ;
#12453 = VERTEX_POINT ( 'NONE', #58475 ) ;
#12454 = CARTESIAN_POINT ( 'NONE',  ( 0.000000000000000000, 244.9489742783177917, -24.99999999999999289 ) ) ;
#12455 = CARTESIAN_POINT ( 'NONE',  ( 2.000000000000001776, -1.225832621831797420, -6.827324998361596009 ) ) ;
#12456 = ORIENTED_EDGE ( 'NONE', *, *, #19154, .F. ) ;
#12457 = ORIENTED_EDGE ( 'NONE', *, *, #54665, .F. ) ;
#12458 = DIRECTION ( 'NONE',  ( -1.000000000000000000, 0.000000000000000000, 0.000000000000000000 ) ) ;
#12459 = EDGE_CURVE ( 'NONE', #53266, #9626, #14203, .T. ) ;
#12460 = LINE ( 'NONE', #38063, #29800 ) ;
#12461 = EDGE_LOOP ( 'NONE', ( #13686, #14662, #41948, #42061 ) ) ;
#12462 = EDGE_CURVE ( 'NONE', #39298, #55512, #62715, .T. ) ;
#12463 = CARTESIAN_POINT ( 'NONE',  ( 0.2648978790185584908, -9.465406350830660287, 7.769924372105172949 ) ) ;
#12464 = CARTESIAN_POINT ( 'NONE',  ( 1.719304012338199295, 11.67935079956398958, 5.066286238785226992 ) ) ;
#12465 = CARTESIAN_POINT ( 'NONE',  ( 2.241352910868909643, 7.532448145350525870, -1.243507963608017075 ) ) ;
#12466 = CARTESIAN_POINT ( 'NONE',  ( -4.049490757281464681, -11.39905423463014777, 7.243820352457140288 ) ) ;
#12467 = CARTESIAN_POINT ( 'NONE',  ( 2.844750968616139630, 3.626176236708114953, -6.946006365803918392 ) ) ;
#12468 = CARTESIAN_POINT ( 'NONE',  ( 37.00000000000000711, 5.300372733891642874, -11.59605747147788790 ) ) ;
#12470 = ORIENTED_EDGE ( 'NONE', *, *, #16294, .F. ) ;
#12469 = CARTESIAN_POINT ( 'NONE',  ( -37.00000000000000711, -1.903127969211109383, -11.59095880812010471 ) ) ;
#12471 = DIRECTION ( 'NONE',  ( -1.000000000000000000, 0.000000000000000000, 0.000000000000000000 ) ) ;
#12472 = EDGE_LOOP ( 'NONE', ( #11672, #39089, #55615, #18502 ) ) ;
#12473 = CARTESIAN_POINT ( 'NONE',  ( 22.88594695219327235, 3.421158645304719137, -11.50198563395279194 ) ) ;
#12474 = ORIENTED_EDGE ( 'NONE', *, *, #6986, .T. ) ;
#12475 = ORIENTED_EDGE ( 'NONE', *, *, #26458, .F. ) ;
#12476 = CONTEXT_DEPENDENT_SHAPE_REPRESENTATION ( #40875, #7996 ) ;
#12477 = CARTESIAN_POINT ( 'NONE',  ( 1.104777566491146112, -11.59867774809547569, 4.729982681549492085 ) ) ;
#12478 = CARTESIAN_POINT ( 'NONE',  ( -15.07969093506218883, -34.00054679313987549, 8.511206496389501552 ) ) ;
#12479 = AXIS2_PLACEMENT_3D ( 'NONE', #19474, #2884, #23141 ) ;
#12480 = CARTESIAN_POINT ( 'NONE',  ( -3.807799651111238859, 10.57930927450194503, 5.668006617322318696 ) ) ;
#12481 = CARTESIAN_POINT ( 'NONE',  ( -48.22764741571072022, -0.3553121838687482437, -6.242084797467388313 ) ) ;
#12482 = CARTESIAN_POINT ( 'NONE',  ( -27.08416813689867908, 0.7899859999124485554, -2.150738950797698834 ) ) ;
#12483 = ORIENTED_EDGE ( 'NONE', *, *, #4193, .F. ) ;
#12484 = AXIS2_PLACEMENT_3D ( 'NONE', #42422, #2575, #62717 ) ;
#12485 = CARTESIAN_POINT ( 'NONE',  ( 145.1370849898475797, 3.309064568108273190E-14, 0.000000000000000000 ) ) ;
#12486 = CARTESIAN_POINT ( 'NONE',  ( 3.780834652287974773, 8.352030633203074927, -10.60629927458383470 ) ) ;
#12488 = ORIENTED_EDGE ( 'NONE', *, *, #2691, .T. ) ;
#12487 = CARTESIAN_POINT ( 'NONE',  ( 1.547277799339151771, -12.12286970032358724, -3.695326562728837416 ) ) ;
#12489 = VERTEX_POINT ( 'NONE', #33527 ) ;
#12490 = CYLINDRICAL_SURFACE ( 'NONE', #24749, 12.18650000000000055 ) ;
#12491 = ORIENTED_EDGE ( 'NONE', *, *, #6524, .F. ) ;
#12492 = DIRECTION ( 'NONE',  ( 0.000000000000000000, -0.7617968321374946061, -0.6478160128811867313 ) ) ;
#12493 = AXIS2_PLACEMENT_3D ( 'NONE', #3873, #44391, #45074 ) ;
#12494 = CARTESIAN_POINT ( 'NONE',  ( 5.514970785353741078, -0.004233694591582968896, -0.002093325033903797351 ) ) ;
#12495 = CARTESIAN_POINT ( 'NONE',  ( -27.08704841010890974, 0.9786466045354205168, -2.081152044925704825 ) ) ;
#12496 = CARTESIAN_POINT ( 'NONE',  ( 1.937114397841935398, 3.531416430611461266, -12.33981801388254240 ) ) ;
#12497 = CARTESIAN_POINT ( 'NONE',  ( -29.41386513404535208, 0.9325270014138739016, 13.46939172307182275 ) ) ;
#12498 = CIRCLE ( 'NONE', #7191, 12.18649999999999878 ) ;
#12499 = CARTESIAN_POINT ( 'NONE',  ( -35.00000000000000000, 5.814360711498290257, 10.70999494708494559 ) ) ;
#12500 = EDGE_CURVE ( 'NONE', #22430, #40555, #64795, .T. ) ;
#12501 = ORIENTED_EDGE ( 'NONE', *, *, #59275, .T. ) ;
#12502 = CARTESIAN_POINT ( 'NONE',  ( 37.00000000000000711, 4.705694406421931860E-17, -3.469127814946512892E-15 ) ) ;
#12503 = EDGE_LOOP ( 'NONE', ( #37768, #53759, #35871, #46615 ) ) ;
#12504 = CARTESIAN_POINT ( 'NONE',  ( 0.2652384529303130623, -6.065769141714278945, 10.63836770010964194 ) ) ;
#12505 = CARTESIAN_POINT ( 'NONE',  ( -7.636043109944020024, -8.974902109404503392, -10.10026812394724338 ) ) ;
#12506 = CARTESIAN_POINT ( 'NONE',  ( 2.305787727787085295, -3.971363876084009537, 6.545285700970515208 ) ) ;
#12507 = LINE ( 'NONE', #58768, #22354 ) ;
#12508 = ORIENTED_EDGE ( 'NONE', *, *, #18758, .F. ) ;
#12509 = ORIENTED_EDGE ( 'NONE', *, *, #13852, .T. ) ;
#12510 = ADVANCED_FACE ( 'NONE', ( #29495 ), #22132, .F. ) ;
#12511 = DIRECTION ( 'NONE',  ( -1.000000000000000000, 0.000000000000000000, 0.000000000000000000 ) ) ;
#12512 = EDGE_LOOP ( 'NONE', ( #17971, #7537, #31637, #16524 ) ) ;
#12513 = LINE ( 'NONE', #26848, #25575 ) ;
#12514 = CARTESIAN_POINT ( 'NONE',  ( 37.00000000000000711, -5.644643009979139592, -10.30098186818248074 ) ) ;
#12515 = CARTESIAN_POINT ( 'NONE',  ( -27.09729107899852352, -2.094470452261897542, -1.021938248127332693 ) ) ;
#12516 = CARTESIAN_POINT ( 'NONE',  ( -35.05012975565874456, 0.01377677982611810216, -0.002073729464863237164 ) ) ;
#12517 = EDGE_LOOP ( 'NONE', ( #55732, #32418, #62125, #58295 ) ) ;
#12518 = CARTESIAN_POINT ( 'NONE',  ( 0.2650492594609250019, -6.027447650185294492, -10.66007682546623592 ) ) ;
#12519 = CARTESIAN_POINT ( 'NONE',  ( -22.28856623400852399, -2.585606290939616692, 2.668530796663832749 ) ) ;
#12520 = CARTESIAN_POINT ( 'NONE',  ( -28.80358531978833625, 2.755772354643147182, -13.22187685252809253 ) ) ;
#12521 = CARTESIAN_POINT ( 'NONE',  ( -44.83472798829954797, -0.9996270273486108637, 15.30615170800020763 ) ) ;
#12522 = AXIS2_PLACEMENT_3D ( 'NONE', #34177, #27899, #13881 ) ;
#12523 = CARTESIAN_POINT ( 'NONE',  ( 0.3053067050349157485, 6.328522421120416297, -10.49978800868453988 ) ) ;
#12524 = DIRECTION ( 'NONE',  ( 0.000000000000000000, 0.000000000000000000, 1.000000000000000000 ) ) ;
#12525 = AXIS2_PLACEMENT_3D ( 'NONE', #3218, #43419, #48765 ) ;
#12526 = ORIENTED_EDGE ( 'NONE', *, *, #42048, .F. ) ;
#12527 = CARTESIAN_POINT ( 'NONE',  ( -18.77295711560618940, -11.99999999999997513, -0.7162851318434579895 ) ) ;
#12528 = FACE_OUTER_BOUND ( 'NONE', #1637, .T. ) ;
#12529 = CARTESIAN_POINT ( 'NONE',  ( -12.75996857643550797, -29.16082758670667019, -4.038023594093941959 ) ) ;
#12530 = ORIENTED_EDGE ( 'NONE', *, *, #37814, .F. ) ;
#12531 = AXIS2_PLACEMENT_3D ( 'NONE', #17091, #57335, #61998 ) ;
#12532 = CARTESIAN_POINT ( 'NONE',  ( -17.32166409804204577, 3.211681732051251625, -13.11356909678292126 ) ) ;
#12533 = CARTESIAN_POINT ( 'NONE',  ( 34.38695973621796043, 25.00000000000000000, 3.530690241644829364 ) ) ;
#12534 = CARTESIAN_POINT ( 'NONE',  ( 2.177405672431842465, -10.89176600224772606, 2.605669267166142333 ) ) ;
#12535 = B_SPLINE_CURVE_WITH_KNOTS ( 'NONE', 3,
 ( #29712, #61608, #50019, #14735, #35014, #128, #55666, #20409, #35684, #9766, #40690, #51003, #5462, #475, #41011, #61293, #15724, #36000, #56300, #10749, #31036, #51348 ),
 .UNSPECIFIED., .F., .F.,
 ( 4, 3, 3, 3, 3, 3, 3, 4 ),
 ( 0.000000000000000000, 4.455945684386670302E-05, 6.636307477203838871E-05, 8.816671873158670684E-05, 0.0001099660380492599882, 0.0001317545563165301817, 0.0001762613022895049089, 0.0001867992666138357976 ),
 .UNSPECIFIED. ) ;
#12536 = CIRCLE ( 'NONE', #49734, 12.18649999999999878 ) ;
#12537 = CARTESIAN_POINT ( 'NONE',  ( 0.2648978790185619880, -1.996248716311710414, 12.08224454301447892 ) ) ;
#12538 = CYLINDRICAL_SURFACE ( 'NONE', #61736, 6.094511299047803199 ) ;
#12539 = EDGE_CURVE ( 'NONE', #49753, #63399, #54254, .T. ) ;
#12540 = ORIENTED_EDGE ( 'NONE', *, *, #36009, .T. ) ;
#12541 = ORIENTED_EDGE ( 'NONE', *, *, #36566, .F. ) ;
#12542 = CARTESIAN_POINT ( 'NONE',  ( -19.56743653832047158, -33.00000000000000000, -5.000000000000003553 ) ) ;
#12543 = EDGE_LOOP ( 'NONE', ( #34637, #6505, #63272, #45569 ) ) ;
#12544 = CARTESIAN_POINT ( 'NONE',  ( -27.08419797710328325, -2.268561579780436599, 0.3221715127607953644 ) ) ;
#12545 = CARTESIAN_POINT ( 'NONE',  ( 37.00000000000000711, 4.705694406421931860E-17, -3.469127814946512892E-15 ) ) ;
#12546 = CARTESIAN_POINT ( 'NONE',  ( 35.00000000000000000, -7.499679039483992504, 9.040300684349768190 ) ) ;
#12547 = CARTESIAN_POINT ( 'NONE',  ( 1.194176325881345813, 3.807610977967081922, -11.96454551582839798 ) ) ;
#12548 = CARTESIAN_POINT ( 'NONE',  ( 3.152665057736163678, 7.923639299009212600, -0.4801242025614006481 ) ) ;
#12549 = CARTESIAN_POINT ( 'NONE',  ( 2.262775599887398403, 5.761998514038564778, 5.019217486252278704 ) ) ;
#12550 = DIRECTION ( 'NONE',  ( -1.000000000000000000, -1.836970198721029688E-16, 0.000000000000000000 ) ) ;
#12551 = ORIENTED_EDGE ( 'NONE', *, *, #22512, .T. ) ;
#12552 = ORIENTED_EDGE ( 'NONE', *, *, #27463, .F. ) ;
#12553 = DIRECTION ( 'NONE',  ( -1.000000000000000000, 0.000000000000000000, 0.000000000000000000 ) ) ;
#12554 = ORIENTED_EDGE ( 'NONE', *, *, #32256, .T. ) ;
#12555 = CARTESIAN_POINT ( 'NONE',  ( 35.00000000000000000, 4.983891302653744582, 11.73555825188270596 ) ) ;
#12556 = EDGE_CURVE ( 'NONE', #6306, #21596, #35075, .T. ) ;
#12557 = VECTOR ( 'NONE', #14231, 1000.000000000000000 ) ;
#12558 = DIRECTION ( 'NONE',  ( 1.000000000000000000, 0.000000000000000000, 0.000000000000000000 ) ) ;
#12559 = ORIENTED_EDGE ( 'NONE', *, *, #56898, .F. ) ;
#12560 = CARTESIAN_POINT ( 'NONE',  ( -35.00000000000000000, -6.946017217729864690, -10.01317267707894310 ) ) ;
#12561 = CARTESIAN_POINT ( 'NONE',  ( -13.26547918569663054, -33.36007533429795302, -10.54465099870413880 ) ) ;
#12562 = AXIS2_PLACEMENT_3D ( 'NONE', #28619, #63526, #2390 ) ;
#12563 = CARTESIAN_POINT ( 'NONE',  ( 2.963017218115626239, -1.744728040076958919, 7.679262289252037910 ) ) ;
#12564 = ORIENTED_EDGE ( 'NONE', *, *, #35444, .F. ) ;
#12565 = VERTEX_POINT ( 'NONE', #61082 ) ;
#12566 = CARTESIAN_POINT ( 'NONE',  ( 0.000000000000000000, -1.734723475976807094E-15, 13.50000000000000178 ) ) ;
#12567 = ORIENTED_EDGE ( 'NONE', *, *, #53667, .T. ) ;
#12568 = ORIENTED_EDGE ( 'NONE', *, *, #52981, .T. ) ;
#12569 = LINE ( 'NONE', #62793, #21699 ) ;
#12570 = VERTEX_POINT ( 'NONE', #25170 ) ;
#12571 = ORIENTED_EDGE ( 'NONE', *, *, #51289, .F. ) ;
#12572 = DIRECTION ( 'NONE',  ( 0.000000000000000000, 0.01356324068817998940, -0.9999080150203989437 ) ) ;
#12574 = AXIS2_PLACEMENT_3D ( 'NONE', #44166, #29209, #49182 ) ;
#12573 = CARTESIAN_POINT ( 'NONE',  ( 35.00000000000000000, 11.07407352312218052, 3.916263239775223504 ) ) ;
#12575 = CYLINDRICAL_SURFACE ( 'NONE', #24636, 6.936499999999988120 ) ;
#12576 = DIRECTION ( 'NONE',  ( 0.000000000000000000, 0.000000000000000000, 1.000000000000000000 ) ) ;
#12577 = CARTESIAN_POINT ( 'NONE',  ( 5.514970785353741078, 0.003262412238248711249, 0.003415090918276149964 ) ) ;
#12578 = CARTESIAN_POINT ( 'NONE',  ( 0.2647959493198558945, 11.55693259385006222, 4.049980114636408501 ) ) ;
#12579 = AXIS2_PLACEMENT_3D ( 'NONE', #18417, #38994, #59617 ) ;
#12580 = ADVANCED_FACE ( 'NONE', ( #45135 ), #15513, .T. ) ;
#12581 = EDGE_LOOP ( 'NONE', ( #42223, #5775, #11189, #15269 ) ) ;
#12582 = CARTESIAN_POINT ( 'NONE',  ( 3.152665057734040488, 0.000000000000000000, 0.000000000000000000 ) ) ;
#12583 = CARTESIAN_POINT ( 'NONE',  ( -25.00000000000000355, -30.00000000000000000, 5.000000000000000888 ) ) ;
#12584 = VECTOR ( 'NONE', #10623, 1000.000000000000000 ) ;
#12585 = EDGE_CURVE ( 'NONE', #65358, #47259, #13865, .T. ) ;
#12586 = CARTESIAN_POINT ( 'NONE',  ( 35.00000000000000000, -11.78745411414841726, -3.093009498343884722 ) ) ;
#12587 = DIRECTION ( 'NONE',  ( 0.000000000000000000, -0.5155538571770288403, 0.8568571761675849441 ) ) ;
#12588 = CARTESIAN_POINT ( 'NONE',  ( 26.34661844826604593, 11.53221627053869369, 3.317828791472333005 ) ) ;
#12589 = CARTESIAN_POINT ( 'NONE',  ( 5.514970785353741078, -0.002796696073589895887, -0.003805873180274304147 ) ) ;
#12590 = CYLINDRICAL_SURFACE ( 'NONE', #34036, 4.999999999999998224 ) ;
#12591 = CARTESIAN_POINT ( 'NONE',  ( 0.3675815128205894289, -11.62724744438063063, -3.951233083390586209 ) ) ;
#12592 = CARTESIAN_POINT ( 'NONE',  ( 2.177405672431937500, -11.17876532285415792, 0.6747479782258832826 ) ) ;
#12593 = EDGE_LOOP ( 'NONE', ( #37640, #31270, #65769, #54892 ) ) ;
#12594 = ADVANCED_FACE ( 'NONE', ( #4912 ), #51461, .T. ) ;
#12595 = CARTESIAN_POINT ( 'NONE',  ( 2.507146904658097419, -7.180414359940930247, -2.843654641958959672 ) ) ;
#12596 =( BOUNDED_SURFACE ( )  B_SPLINE_SURFACE ( 3, 1, ( 
 ( #28384, #29051 ),
 ( #48680, #49360 ),
 ( #3138, #3806 ),
 ( #59636, #24369 ) ),
 .UNSPECIFIED., .F., .F., .F. ) 
 B_SPLINE_SURFACE_WITH_KNOTS ( ( 4, 4 ),
 ( 2, 2 ),
 ( 0.000000000000000000, 1.000000000000000000 ),
 ( 0.000000000000000000, 1.000000000000000000 ),
 .UNSPECIFIED. ) 
 GEOMETRIC_REPRESENTATION_ITEM ( )  RATIONAL_B_SPLINE_SURFACE ( (
 ( 1.000000000000000000, 1.000000000000000000),
 ( 0.9856612449720755231, 0.9999558406602322425),
 ( 0.9856612449720755231, 0.9999558406602322425),
 ( 1.000000000000000000, 1.000000000000000000) ) ) 
 REPRESENTATION_ITEM ( '' )  SURFACE ( )  );
#12597 = ORIENTED_EDGE ( 'NONE', *, *, #49560, .F. ) ;
#12598 = CARTESIAN_POINT ( 'NONE',  ( -11.40165637462999904, -7.508992741355383416, 9.360289953322597611 ) ) ;
#12599 = DIRECTION ( 'NONE',  ( 0.000000000000000000, -0.07632122047557185485, 0.9970832820307033995 ) ) ;
#12600 = CARTESIAN_POINT ( 'NONE',  ( 2.000000000000001776, 0.000000000000000000, 0.000000000000000000 ) ) ;
#12601 = CARTESIAN_POINT ( 'NONE',  ( -35.00000000000000000, 7.251710744571578715, 9.240395740215660680 ) ) ;
#12602 = CARTESIAN_POINT ( 'NONE',  ( 2.589278595512544356, 7.670769623692099692, 1.107986312493582925 ) ) ;
#12603 = EDGE_CURVE ( 'NONE', #59191, #39378, #31912, .T. ) ;
#12604 = ORIENTED_EDGE ( 'NONE', *, *, #818, .F. ) ;
#12605 = CARTESIAN_POINT ( 'NONE',  ( -35.00000000000000000, 8.551552972817082932, 8.052525312709914118 ) ) ;
#12606 = CARTESIAN_POINT ( 'NONE',  ( 2.297017764050091504, -3.682881532880131648, 6.708511771223863995 ) ) ;
#12607 = DIRECTION ( 'NONE',  ( -1.000000000000000000, 0.000000000000000000, 0.000000000000000000 ) ) ;
#12608 = CARTESIAN_POINT ( 'NONE',  ( 3.657075258460736222, -30.77912794045597522, -15.01778408663798814 ) ) ;
#12609 = CIRCLE ( 'NONE', #25342, 5.000000000000000000 ) ;
#12610 = ADVANCED_FACE ( 'NONE', ( #39813 ), #31152, .T. ) ;
#12611 = B_SPLINE_CURVE_WITH_KNOTS ( 'NONE', 3,
 ( #38927, #3038, #63848, #60842, #45221, #50551, #61170 ),
 .UNSPECIFIED., .F., .F.,
 ( 4, 3, 4 ),
 ( 6.914360523903184076E-15, 0.002398160485434806810, 0.005002426799384151676 ),
 .UNSPECIFIED. ) ;
#12612 = CARTESIAN_POINT ( 'NONE',  ( -4.984433189575353751, -1.083073623696801935, -13.45752292036589637 ) ) ;
#12613 = ORIENTED_EDGE ( 'NONE', *, *, #51398, .T. ) ;
#12614 = CIRCLE ( 'NONE', #29605, 2.899999999999994582 ) ;
#12615 = CARTESIAN_POINT ( 'NONE',  ( 2.655192694322927593, -4.290256727313598972, 8.589732161582016801 ) ) ;
#12616 = CARTESIAN_POINT ( 'NONE',  ( -35.00000000000000000, 0.000000000000000000, 0.000000000000000000 ) ) ;
#12617 = CARTESIAN_POINT ( 'NONE',  ( -37.00000000000000711, 4.946702696913171771, 11.13736569743276306 ) ) ;
#12618 = VECTOR ( 'NONE', #53302, 1000.000000000000000 ) ;
#12619 = VERTEX_POINT ( 'NONE', #40122 ) ;
#12620 = DIRECTION ( 'NONE',  ( -1.000000000000000000, 0.000000000000000000, 0.000000000000000000 ) ) ;
#12621 = AXIS2_PLACEMENT_3D ( 'NONE', #16708, #26694, #46004 ) ;
#12622 = ORIENTED_EDGE ( 'NONE', *, *, #19383, .T. ) ;
#12623 = CARTESIAN_POINT ( 'NONE',  ( 2.260457164927188511, -6.546788723198579518, 3.939659644572524488 ) ) ;
#12624 = LINE ( 'NONE', #58889, #41724 ) ;
#12625 = CYLINDRICAL_SURFACE ( 'NONE', #59798, 4.999999999999999112 ) ;
#12626 = DIRECTION ( 'NONE',  ( -1.000000000000000000, 0.000000000000000000, 0.000000000000000000 ) ) ;
#12627 = CARTESIAN_POINT ( 'NONE',  ( -22.71097035706202405, -0.4203397252017116448, 4.965150228107737540 ) ) ;
#12628 = ORIENTED_EDGE ( 'NONE', *, *, #27436, .T. ) ;
#12629 = ORIENTED_EDGE ( 'NONE', *, *, #19697, .F. ) ;
#12630 = VECTOR ( 'NONE', #38368, 1000.000000000000000 ) ;
#12631 = ORIENTED_EDGE ( 'NONE', *, *, #24987, .T. ) ;
#12632 = DIRECTION ( 'NONE',  ( 0.000000000000000000, 0.000000000000000000, 1.000000000000000000 ) ) ;
#12633 = ADVANCED_FACE ( 'NONE', ( #19549 ), #35474, .T. ) ;
#12634 = CARTESIAN_POINT ( 'NONE',  ( 0.000000000000000000, -2.562706407243680928, 6.312399813420318750 ) ) ;
#12635 = VERTEX_POINT ( 'NONE', #30163 ) ;
#12636 = CARTESIAN_POINT ( 'NONE',  ( 3.152665057734040488, 0.000000000000000000, 0.000000000000000000 ) ) ;
#12637 = CARTESIAN_POINT ( 'NONE',  ( -22.27704833740210333, -0.3581593033281198490, -3.663709865074131766 ) ) ;
#12638 = ORIENTED_EDGE ( 'NONE', *, *, #27389, .F. ) ;
#12639 = CARTESIAN_POINT ( 'NONE',  ( 2.305787727787084407, 0.1666591538753756929, -7.654065630109506024 ) ) ;
#12640 = CARTESIAN_POINT ( 'NONE',  ( 22.36482863261543486, -11.96441317219524514, -0.9234811557364158707 ) ) ;
#12641 = LINE ( 'NONE', #3367, #47342 ) ;
#12642 = ORIENTED_EDGE ( 'NONE', *, *, #33760, .F. ) ;
#12643 = EDGE_LOOP ( 'NONE', ( #42867, #46131, #398, #55193 ) ) ;
#12644 = CARTESIAN_POINT ( 'NONE',  ( -35.00000000000000000, -2.080187960898651767, 12.57916205664480458 ) ) ;
#12645 = ORIENTED_EDGE ( 'NONE', *, *, #58000, .T. ) ;
#12646 = DIRECTION ( 'NONE',  ( 0.000000000000000000, -0.01356324068817998940, 0.9999080150203990547 ) ) ;
#12647 = VERTEX_POINT ( 'NONE', #60415 ) ;
#12648 = CARTESIAN_POINT ( 'NONE',  ( 2.290907136833256530, 3.684064771923258874, 6.705538900522838297 ) ) ;
#12649 = CARTESIAN_POINT ( 'NONE',  ( 14.81924285005568898, -34.67057711548255128, -7.362581078982665339 ) ) ;
#12650 = DIRECTION ( 'NONE',  ( 0.000000000000000000, 0.000000000000000000, 1.000000000000000000 ) ) ;
#12652 = CARTESIAN_POINT ( 'NONE',  ( -22.27756824490284515, 3.555646273932183021, 0.9591204781039950333 ) ) ;
#12651 = AXIS2_PLACEMENT_3D ( 'NONE', #53411, #2878, #54396 ) ;
#12653 = EDGE_CURVE ( 'NONE', #48935, #4396, #23428, .T. ) ;
#12654 = CARTESIAN_POINT ( 'NONE',  ( 16.78263030916553333, 25.00000000000000000, 5.836879698929882565 ) ) ;
#12655 = CARTESIAN_POINT ( 'NONE',  ( -27.20102706715913143, -1.966718264078098910, -1.765193291701730338 ) ) ;
#12656 = CARTESIAN_POINT ( 'NONE',  ( 5.373297959932116896, -9.555382238011333129, -7.266535920493700118 ) ) ;
#12657 = EDGE_LOOP ( 'NONE', ( #26399, #30108, #45231, #62764 ) ) ;
#12658 = LINE ( 'NONE', #2048, #18409 ) ;
#12659 = ORIENTED_EDGE ( 'NONE', *, *, #37969, .F. ) ;
#12660 = AXIS2_PLACEMENT_3D ( 'NONE', #43584, #23989, #18353 ) ;
#12661 = CARTESIAN_POINT ( 'NONE',  ( 145.1370849898475797, 3.309064568108273190E-14, 0.000000000000000000 ) ) ;
#12662 = EDGE_CURVE ( 'NONE', #61808, #46276, #55100, .T. ) ;
#12663 = CARTESIAN_POINT ( 'NONE',  ( -37.00000000000000711, -8.352657516904613999, -8.258652103341526995 ) ) ;
#12664 = ADVANCED_FACE ( 'NONE', ( #50466 ), #65394, .F. ) ;
#12665 = ORIENTED_EDGE ( 'NONE', *, *, #43745, .F. ) ;
#12666 = CARTESIAN_POINT ( 'NONE',  ( -15.52273868740600626, 8.454822416089735171, 8.515633660947054651 ) ) ;
#12667 = CARTESIAN_POINT ( 'NONE',  ( 0.2767916011545393240, 6.288637995698108440, 10.51265105824864676 ) ) ;
#12668 = B_SPLINE_CURVE_WITH_KNOTS ( 'NONE', 3,
 ( #60608, #54966, #55288, #50974, #5423, #54670, #34986, #14395, #15045, #39337, #14069, #60280, #9089, #24374, #29371, #10385, #19072, #49665, #65580, #59639, #4105, #25694 ),
 .UNSPECIFIED., .F., .F.,
 ( 4, 3, 3, 3, 3, 3, 3, 4 ),
 ( 0.000000000000000000, 4.447697177976356439E-05, 6.624143997791323828E-05, 8.800576886944330051E-05, 0.0001097699864780905381, 0.0001315341395364381678, 0.0001760120188223285103, 0.0001867971373174725450 ),
 .UNSPECIFIED. ) ;
#12669 = CARTESIAN_POINT ( 'NONE',  ( 0.2653141334712555421, -9.409392642815692653, -7.837911425448877090 ) ) ;
#12670 = VERTEX_POINT ( 'NONE', #50133 ) ;
#12671 = ORIENTED_EDGE ( 'NONE', *, *, #3563, .T. ) ;
#12672 = ADVANCED_FACE ( 'NONE', ( #55438 ), #9875, .T. ) ;
#12673 = DIRECTION ( 'NONE',  ( 0.000000000000000000, 0.000000000000000000, 1.000000000000000000 ) ) ;
#12674 = VECTOR ( 'NONE', #61437, 1000.000000000000000 ) ;
#12675 = ORIENTED_EDGE ( 'NONE', *, *, #48029, .T. ) ;
#12676 = ADVANCED_FACE ( 'NONE', ( #56081 ), #28941, .F. ) ;
#12677 = CARTESIAN_POINT ( 'NONE',  ( 2.305787727787083519, -2.774453000917197265, 7.135468203929974607 ) ) ;
#12678 = CARTESIAN_POINT ( 'NONE',  ( 0.2646305136544072623, -9.465888453932908675, -7.770320294339273737 ) ) ;
#12679 = CARTESIAN_POINT ( 'NONE',  ( -2.894288433085122847, -12.68055345927033706, 4.644490739423512871 ) ) ;
#12680 = CARTESIAN_POINT ( 'NONE',  ( -7.393613020821582005, 5.386680228572950035, -10.72686196631679323 ) ) ;
#12681 = EDGE_LOOP ( 'NONE', ( #3911, #31941, #48349, #46666 ) ) ;
#12682 = VECTOR ( 'NONE', #16918, 1000.000000000000000 ) ;
#12683 = CARTESIAN_POINT ( 'NONE',  ( 0.3675815128205894289, -4.447030445008105737, -11.44679196252413789 ) ) ;
#12684 = EDGE_CURVE ( 'NONE', #60345, #12453, #31781, .T. ) ;
#12685 = EDGE_CURVE ( 'NONE', #25020, #32375, #1126, .T. ) ;
#12686 = CARTESIAN_POINT ( 'NONE',  ( 5.527856869237409931, -26.90719658711817530, -15.68471180892751171 ) ) ;
#12687 = B_SPLINE_CURVE_WITH_KNOTS ( 'NONE', 3,
 ( #315, #15261, #65460, #10588, #14906, #35541, #20900, #39878, #55507, #30867, #60158, #61149, #10265, #20594, #5295, #25565 ),
 .UNSPECIFIED., .F., .F.,
 ( 4, 3, 3, 3, 3, 4 ),
 ( 7.589415207398531038E-19, 0.0003017745587525230244, 0.0006035491769808683194, 0.0009053241094668093092, 0.001207275924541010865, 0.001510325902535037453 ),
 .UNSPECIFIED. ) ;
#12688 = ADVANCED_FACE ( 'NONE', ( #33685 ), #33018, .T. ) ;
#12689 = CARTESIAN_POINT ( 'NONE',  ( 21.94582960821244555, 13.05933372330677500, -3.441589981846832291 ) ) ;
#12690 = CARTESIAN_POINT ( 'NONE',  ( -27.08423805673873375, -0.6554626340706021237, 2.195702713475284895 ) ) ;
#12691 = CARTESIAN_POINT ( 'NONE',  ( 145.1370849898475797, 3.309064568108273190E-14, 0.000000000000000000 ) ) ;
#12692 = CARTESIAN_POINT ( 'NONE',  ( 6.211465341154163156, -9.377354143557047550, -7.490490949957647970 ) ) ;
#12693 = CARTESIAN_POINT ( 'NONE',  ( 2.835339799623992629, 5.281994181469073624, -5.783398714696503795 ) ) ;
#12694 = AXIS2_PLACEMENT_3D ( 'NONE', #43435, #43781, #29452 ) ;
#12695 = CIRCLE ( 'NONE', #16983, 4.999999999999999112 ) ;
#12696 = ORIENTED_EDGE ( 'NONE', *, *, #48047, .T. ) ;
#12697 = CARTESIAN_POINT ( 'NONE',  ( 12.49808451655605879, -9.686563543903927709, -7.085704797288028267 ) ) ;
#12698 = ORIENTED_EDGE ( 'NONE', *, *, #54178, .T. ) ;
#12699 = DIRECTION ( 'NONE',  ( 1.000000000000000000, 0.000000000000000000, 0.000000000000000000 ) ) ;
#12700 = AXIS2_PLACEMENT_3D ( 'NONE', #30819, #15851, #46154 ) ;
#12701 = CARTESIAN_POINT ( 'NONE',  ( -22.29115169517546136, 3.712980101756725659, -0.2790989024812895458 ) ) ;
#12702 = CARTESIAN_POINT ( 'NONE',  ( 2.241352910868909643, -7.532448145350499225, -1.243507963608171174 ) ) ;
#12703 = ORIENTED_EDGE ( 'NONE', *, *, #24729, .F. ) ;
#12704 = CARTESIAN_POINT ( 'NONE',  ( 2.241352910868908310, 4.970878533273838329, -5.794346703933798359 ) ) ;
#12705 = VERTEX_POINT ( 'NONE', #51773 ) ;
#12706 = CARTESIAN_POINT ( 'NONE',  ( -35.00000000000000000, -11.99999999999999289, 0.000000000000000000 ) ) ;
#12707 = ORIENTED_EDGE ( 'NONE', *, *, #47054, .F. ) ;
#12708 = ORIENTED_EDGE ( 'NONE', *, *, #58338, .F. ) ;
#12709 = CARTESIAN_POINT ( 'NONE',  ( 28.76862497509140226, -12.20680944158938175, 5.780333286781263347 ) ) ;
#12710 = AXIS2_PLACEMENT_3D ( 'NONE', #65226, #19695, #29975 ) ;
#12712 = EDGE_CURVE ( 'NONE', #10987, #22527, #45733, .T. ) ;
#12711 = CARTESIAN_POINT ( 'NONE',  ( 0.3278977287071234148, -12.03512402322222208, -2.374069413450269561 ) ) ;
#12713 = ADVANCED_FACE ( 'NONE', ( #23387 ), #48357, .T. ) ;
#12714 = ORIENTED_EDGE ( 'NONE', *, *, #16913, .T. ) ;
#12715 = DIRECTION ( 'NONE',  ( 0.000000000000000000, -0.7196168960969719919, -0.6943713148249714973 ) ) ;
#12716 = CARTESIAN_POINT ( 'NONE',  ( 2.990245332647783805, 8.465748356454174228, 0.5125330575219991802 ) ) ;
#12717 = VECTOR ( 'NONE', #20587, 1000.000000000000000 ) ;
#12718 = LINE ( 'NONE', #2451, #24834 ) ;
#12719 = CARTESIAN_POINT ( 'NONE',  ( 5.514970785353741078, 0.004588761610584827719, 0.001117786416802128355 ) ) ;
#12720 = ORIENTED_EDGE ( 'NONE', *, *, #38002, .F. ) ;
#12721 = CARTESIAN_POINT ( 'NONE',  ( -35.00000000000000000, -11.74226168163341022, -0.3025107581132430723 ) ) ;
#12722 = CARTESIAN_POINT ( 'NONE',  ( 12.30974346995382973, -29.30943841933768113, 5.552318955347200991 ) ) ;
#12723 = CARTESIAN_POINT ( 'NONE',  ( 0.9232058338315048962, -6.559496812049736114, 10.60677148422242411 ) ) ;
#12725 = ORIENTED_EDGE ( 'NONE', *, *, #7984, .T. ) ;
#12724 = LINE ( 'NONE', #37015, #21314 ) ;
#12726 = LINE ( 'NONE', #2112, #43682 ) ;
#12727 = VERTEX_POINT ( 'NONE', #41432 ) ;
#12728 = CARTESIAN_POINT ( 'NONE',  ( 0.2767916011545407673, -6.288637995698039163, -10.51265105824868762 ) ) ;
#12729 = ADVANCED_FACE ( 'NONE', ( #53330 ), #47116, .T. ) ;
#12730 = VECTOR ( 'NONE', #38846, 1000.000000000000000 ) ;
#12731 = ORIENTED_EDGE ( 'NONE', *, *, #32185, .F. ) ;
#12732 = CARTESIAN_POINT ( 'NONE',  ( 2.000000000000001776, -6.250523986464001425, 3.007653927006548766 ) ) ;
#12733 = CARTESIAN_POINT ( 'NONE',  ( 0.2717059086739025964, 4.023283916512583325, -11.56868249951477701 ) ) ;
#12734 = CARTESIAN_POINT ( 'NONE',  ( 0.3665391374699467075, 8.095513416941352958, -9.237363111276685856 ) ) ;
#12735 = DIRECTION ( 'NONE',  ( 0.000000000000000000, 0.9246979985058736418, 0.3807014730195186214 ) ) ;
#12736 = DIRECTION ( 'NONE',  ( 1.000000000000000000, 0.000000000000000000, 0.000000000000000000 ) ) ;
#12737 = ADVANCED_FACE ( 'NONE', ( #3125 ), #35716, .F. ) ;
#12738 = CARTESIAN_POINT ( 'NONE',  ( 2.941278708680199916, 6.138172921908580548, -0.1348063076487160949 ) ) ;
#12739 = CARTESIAN_POINT ( 'NONE',  ( -22.29195009621226475, -3.616122380634895439, -0.8975732442595631966 ) ) ;
#12740 = EDGE_LOOP ( 'NONE', ( #42636, #41582, #39293, #58772 ) ) ;
#12741 = VERTEX_POINT ( 'NONE', #38338 ) ;
#12742 = CARTESIAN_POINT ( 'NONE',  ( 2.000000000000001776, -5.450255447309714896, -4.087611905901492371 ) ) ;
#12743 = EDGE_LOOP ( 'NONE', ( #4857, #3287, #42976, #50402 ) ) ;
#12744 = EDGE_CURVE ( 'NONE', #27033, #7491, #18421, .T. ) ;
#12745 = EDGE_LOOP ( 'NONE', ( #36552, #52048, #46552, #48132 ) ) ;
#12746 = FACE_OUTER_BOUND ( 'NONE', #47587, .T. ) ;
#12747 = CARTESIAN_POINT ( 'NONE',  ( -35.00000000000000000, -2.185196060783795691, -11.54110654723651486 ) ) ;
#12748 = LINE ( 'NONE', #13733, #1191 ) ;
#12749 = CARTESIAN_POINT ( 'NONE',  ( 0.2915757698887260219, -10.50410115670273647, 6.312478057070419091 ) ) ;
#12750 = DIRECTION ( 'NONE',  ( -1.000000000000000000, -1.836970198721029688E-16, 0.000000000000000000 ) ) ;
#12751 = CARTESIAN_POINT ( 'NONE',  ( 2.241526690369556984, -7.521460607153588995, -1.308664175663846185 ) ) ;
#12752 = AXIS2_PLACEMENT_3D ( 'NONE', #64223, #13666, #38281 ) ;
#12753 = DIRECTION ( 'NONE',  ( -1.000000000000000000, 0.000000000000000000, 0.000000000000000000 ) ) ;
#12754 = ORIENTED_EDGE ( 'NONE', *, *, #60266, .T. ) ;
#12755 = EDGE_CURVE ( 'NONE', #18737, #51616, #3277, .T. ) ;
#12756 = CARTESIAN_POINT ( 'NONE',  ( -27.08423805673873375, -1.573803011992715106, -1.665498649074261373 ) ) ;
#12757 = DIRECTION ( 'NONE',  ( 0.000000000000000000, 0.000000000000000000, 1.000000000000000000 ) ) ;
#12758 = EDGE_CURVE ( 'NONE', #63698, #7920, #22374, .T. ) ;
#12759 = ADVANCED_FACE ( 'NONE', ( #26168 ), #7773, .T. ) ;
#12760 = CIRCLE ( 'NONE', #59490, 4.999999999999999112 ) ;
#12761 = CARTESIAN_POINT ( 'NONE',  ( 2.000000000000001776, 0.000000000000000000, 0.000000000000000000 ) ) ;
#12762 = LINE ( 'NONE', #33051, #383 ) ;
#12763 = ADVANCED_FACE ( 'NONE', ( #58660 ), #19155, .T. ) ;
#12764 = CIRCLE ( 'NONE', #14838, 12.74999999999999822 ) ;
#12765 = DIRECTION ( 'NONE',  ( -1.000000000000000000, 0.000000000000000000, 0.000000000000000000 ) ) ;
#12766 = ADVANCED_FACE ( 'NONE', ( #33367 ), #8102, .T. ) ;
#12767 = CARTESIAN_POINT ( 'NONE',  ( 0.3665391374699465965, 12.04754782681760794, -2.392238720110335226 ) ) ;
#12768 = ORIENTED_EDGE ( 'NONE', *, *, #30760, .F. ) ;
#12769 = FACE_OUTER_BOUND ( 'NONE', #23271, .T. ) ;
#12770 = CARTESIAN_POINT ( 'NONE',  ( 0.2833330754217402991, -1.928200609300391610, -12.09951353627562298 ) ) ;
#12771 = CARTESIAN_POINT ( 'NONE',  ( 0.9232058338315058954, -8.301689855530105078, -9.306586124266681637 ) ) ;
#12772 = CARTESIAN_POINT ( 'NONE',  ( -18.49080574448724690, -13.49999999999999822, -2.827202046691532642E-15 ) ) ;
#12773 = AXIS2_PLACEMENT_3D ( 'NONE', #56254, #51299, #18512 ) ;
#12774 = CARTESIAN_POINT ( 'NONE',  ( -27.35552965826137140, -0.2619431035391951434, 3.094132632038943065 ) ) ;
#12775 = CARTESIAN_POINT ( 'NONE',  ( 0.9232058338315058954, -6.559496812049588677, -10.60677148422251115 ) ) ;
#12776 = ORIENTED_EDGE ( 'NONE', *, *, #7668, .T. ) ;
#12777 = CARTESIAN_POINT ( 'NONE',  ( 37.00000000000000711, 10.28547182238015978, 5.672855678558568648 ) ) ;
#12778 = DIRECTION ( 'NONE',  ( 0.000000000000000000, -0.01356324068817998940, 0.9999080150203990547 ) ) ;
#12779 = DIRECTION ( 'NONE',  ( 1.000000000000000000, 0.000000000000000000, 0.000000000000000000 ) ) ;
#12780 = CARTESIAN_POINT ( 'NONE',  ( 1.194176325881340928, -12.44396189284383780, -1.672143286119688321 ) ) ;
#12781 = ORIENTED_EDGE ( 'NONE', *, *, #49324, .F. ) ;
#12782 = CARTESIAN_POINT ( 'NONE',  ( 0.3341166715381307939, 2.378838837789095439, 12.03629799686216195 ) ) ;
#12783 = CIRCLE ( 'NONE', #7471, 2.899999999999996803 ) ;
#12784 = DIRECTION ( 'NONE',  ( -1.000000000000000000, 0.000000000000000000, 0.000000000000000000 ) ) ;
#12785 = VERTEX_POINT ( 'NONE', #887 ) ;
#12786 = APPLICATION_CONTEXT ( 'automotive_design' ) ;
#12787 = B_SPLINE_CURVE_WITH_KNOTS ( 'NONE', 3,
 ( #10876, #60430, #35139, #30177, #35487, #35793, #31167, #60110, #10214, #25855, #46145, #65086 ),
 .UNSPECIFIED., .F., .F.,
 ( 4, 2, 2, 2, 2, 4 ),
 ( 0.002289549871878519133, 0.002934044320523027626, 0.003578538769167536118, 0.004867527666456550502, 0.006156516563745564885, 0.007445505461034578401 ),
 .UNSPECIFIED. ) ;
#12788 = ORIENTED_EDGE ( 'NONE', *, *, #37449, .F. ) ;
#12789 = CARTESIAN_POINT ( 'NONE',  ( -35.00000000000000000, 0.000000000000000000, 0.000000000000000000 ) ) ;
#12790 = CIRCLE ( 'NONE', #43553, 12.74999999999999822 ) ;
#12791 = ADVANCED_FACE ( 'NONE', ( #19392 ), #13581, .F. ) ;
#12792 = AXIS2_PLACEMENT_3D ( 'NONE', #47470, #52469, #22858 ) ;
#12793 = AXIS2_PLACEMENT_3D ( 'NONE', #53711, #8144, #28415 ) ;
#12794 = ORIENTED_EDGE ( 'NONE', *, *, #37716, .F. ) ;
#12795 = CARTESIAN_POINT ( 'NONE',  ( 35.00000000000000000, -10.75351884295723970, 4.725891942574862448 ) ) ;
#12796 = EDGE_CURVE ( 'NONE', #21512, #1348, #41447, .T. ) ;
#12797 = CARTESIAN_POINT ( 'NONE',  ( 5.516018279890452902, -0.0009545156522407517155, -0.006707902355169297580 ) ) ;
#12798 = DIRECTION ( 'NONE',  ( 0.000000000000000000, 0.000000000000000000, 1.000000000000000000 ) ) ;
#12799 = CARTESIAN_POINT ( 'NONE',  ( 2.288423627607478306, -7.560204962263194162, -1.169285315515855350 ) ) ;
#12800 =( BOUNDED_SURFACE ( )  B_SPLINE_SURFACE ( 3, 1, ( 
 ( #1620, #10921 ),
 ( #51824, #305 ),
 ( #46496, #20581 ),
 ( #36842, #47175 ) ),
 .UNSPECIFIED., .F., .F., .F. ) 
 B_SPLINE_SURFACE_WITH_KNOTS ( ( 4, 4 ),
 ( 2, 2 ),
 ( 0.000000000000000000, 1.000000000000000000 ),
 ( 0.000000000000000000, 1.000000000000000000 ),
 .UNSPECIFIED. ) 
 GEOMETRIC_REPRESENTATION_ITEM ( )  RATIONAL_B_SPLINE_SURFACE ( (
 ( 1.000000000000000000, 1.000000000000000000),
 ( 0.9932032654565553509, 0.8386279382598740284),
 ( 0.9932032654565553509, 0.8386279382598740284),
 ( 1.000000000000000000, 1.000000000000000000) ) ) 
 REPRESENTATION_ITEM ( '' )  SURFACE ( )  );
#12801 = DIRECTION ( 'NONE',  ( 0.000000000000000000, 0.000000000000000000, 1.000000000000000000 ) ) ;
#12802 = CARTESIAN_POINT ( 'NONE',  ( 0.3537226245948378867, 5.910416419900530904, 10.75912040401511049 ) ) ;
#12804 = EDGE_LOOP ( 'NONE', ( #53739, #1649, #22283, #17798 ) ) ;
#12803 = DIRECTION ( 'NONE',  ( 0.000000000000000000, -0.9651210252299767811, -0.2618041379715732586 ) ) ;
#12805 = CARTESIAN_POINT ( 'NONE',  ( -22.27709082389155171, 2.563977319272137567, 2.641652894015082520 ) ) ;
#12806 = ORIENTED_EDGE ( 'NONE', *, *, #41718, .T. ) ;
#12807 = DIRECTION ( 'NONE',  ( 0.000000000000000000, 0.000000000000000000, 1.000000000000000000 ) ) ;
#12808 = EDGE_LOOP ( 'NONE', ( #7001, #8985, #24915, #36943 ) ) ;
#12809 = EDGE_CURVE ( 'NONE', #27449, #429, #9375, .T. ) ;
#12810 = EDGE_LOOP ( 'NONE', ( #38304, #42430, #47866, #36379 ) ) ;
#12811 = PLANE ( 'NONE',  #40078 ) ;
#12812 = CIRCLE ( 'NONE', #61661, 12.74999999999999822 ) ;
#12813 = CARTESIAN_POINT ( 'NONE',  ( 4.225235259830817824, -26.75987402111029922, 15.91411249164822728 ) ) ;
#12814 = CARTESIAN_POINT ( 'NONE',  ( -25.13384719747249108, 8.062265727243834945, 10.83424663242000996 ) ) ;
#12815 = AXIS2_PLACEMENT_3D ( 'NONE', #8043, #22004, #28307 ) ;
#12816 = DIRECTION ( 'NONE',  ( 1.000000000000000000, 0.000000000000000000, 0.000000000000000000 ) ) ;
#12817 = CARTESIAN_POINT ( 'NONE',  ( -35.00000000000000000, 0.000000000000000000, 0.000000000000000000 ) ) ;
#12819 = ORIENTED_EDGE ( 'NONE', *, *, #31019, .F. ) ;
#12818 = VECTOR ( 'NONE', #21188, 1000.000000000000000 ) ;
#12820 = AXIS2_PLACEMENT_3D ( 'NONE', #16358, #2038, #21682 ) ;
#12821 = CARTESIAN_POINT ( 'NONE',  ( -26.14336630348346091, -10.67021403765777521, 5.492080489366163221 ) ) ;
#12822 = DIRECTION ( 'NONE',  ( 0.000000000000000000, -0.01356324068817991828, 0.9999080150203990547 ) ) ;
#12824 = EDGE_LOOP ( 'NONE', ( #46856, #31375, #19803, #10984 ) ) ;
#12823 = CARTESIAN_POINT ( 'NONE',  ( 0.8320506296491579912, -11.81055997318801332, -3.891425424503422992 ) ) ;
#12825 = ORIENTED_EDGE ( 'NONE', *, *, #28726, .T. ) ;
#12826 = AXIS2_PLACEMENT_3D ( 'NONE', #41454, #26840, #61414 ) ;
#12827 = FACE_OUTER_BOUND ( 'NONE', #14588, .T. ) ;
#12828 = EDGE_CURVE ( 'NONE', #32047, #10423, #18744, .T. ) ;
#12829 = EDGE_LOOP ( 'NONE', ( #15361, #42845, #37345, #20044 ) ) ;
#12830 = VECTOR ( 'NONE', #52199, 1000.000000000000000 ) ;
#12831 = CARTESIAN_POINT ( 'NONE',  ( 29.35982233226166471, -7.748204631658793140, 11.05532493772648550 ) ) ;
#12832 = CYLINDRICAL_SURFACE ( 'NONE', #40420, 2.899999999999994582 ) ;
#12833 = FACE_OUTER_BOUND ( 'NONE', #17005, .T. ) ;
#12834 = EDGE_CURVE ( 'NONE', #7231, #56666, #48943, .T. ) ;
#12835 = CARTESIAN_POINT ( 'NONE',  ( -27.20102706715913143, -2.512061365242607369, 0.8206313329275958246 ) ) ;
#12836 = CARTESIAN_POINT ( 'NONE',  ( 37.00000000000000711, 4.705694406421931860E-17, -3.469127814946512892E-15 ) ) ;
#12837 = CARTESIAN_POINT ( 'NONE',  ( -27.08704841010922593, -1.888108843319752150, 1.313007237774850289 ) ) ;
#12838 = CARTESIAN_POINT ( 'NONE',  ( -9.351388602708162523, 12.99278190472488248, -3.665735721005250358 ) ) ;
#12839 = AXIS2_PLACEMENT_3D ( 'NONE', #39657, #39977, #60587 ) ;
#12840 = ORIENTED_EDGE ( 'NONE', *, *, #26896, .F. ) ;
#12841 = CARTESIAN_POINT ( 'NONE',  ( -17.71314213125373627, 12.92974920937838768, 3.882255733911251117 ) ) ;
#12842 = VERTEX_POINT ( 'NONE', #8421 ) ;
#12843 = AXIS2_PLACEMENT_3D ( 'NONE', #45029, #40693, #65303 ) ;
#12844 = DIRECTION ( 'NONE',  ( -1.000000000000000000, -0.000000000000000000, -0.000000000000000000 ) ) ;
#12845 = DIRECTION ( 'NONE',  ( -1.000000000000000000, 0.000000000000000000, 0.000000000000000000 ) ) ;
#12846 = CARTESIAN_POINT ( 'NONE',  ( 0.2648978790185602672, -7.769924372105269761, 9.465406350830582127 ) ) ;
#12847 = ADVANCED_FACE ( 'NONE', ( #14378 ), #49967, .T. ) ;
#12848 = AXIS2_PLACEMENT_3D ( 'NONE', #59331, #29083, #39700 ) ;
#12849 = AXIS2_PLACEMENT_3D ( 'NONE', #4715, #51243, #16308 ) ;
#12850 = VERTEX_POINT ( 'NONE', #34650 ) ;
#12851 = CARTESIAN_POINT ( 'NONE',  ( 0.2646305136544072623, 11.46223899740600238, 4.312539723326168861 ) ) ;
#12852 = EDGE_CURVE ( 'NONE', #36872, #65779, #24356, .T. ) ;
#12853 = VERTEX_POINT ( 'NONE', #39318 ) ;
#12854 = VECTOR ( 'NONE', #22155, 999.9999999999998863 ) ;
#12855 = CARTESIAN_POINT ( 'NONE',  ( 0.3632410797595260199, 7.689504457927780479, -9.572936598843549305 ) ) ;
#12856 = CARTESIAN_POINT ( 'NONE',  ( 8.691781497961200031, 5.979943475656228635, 10.40578628523820015 ) ) ;
#12857 = EDGE_CURVE ( 'NONE', #37109, #27716, #25029, .T. ) ;
#12858 = CARTESIAN_POINT ( 'NONE',  ( 2.269879328256730666, 1.473193649116136372, 7.500604381673465326 ) ) ;
#12859 = DIRECTION ( 'NONE',  ( -1.000000000000000000, 0.000000000000000000, 0.000000000000000000 ) ) ;
#12860 = ORIENTED_EDGE ( 'NONE', *, *, #264, .F. ) ;
#12861 = DIRECTION ( 'NONE',  ( 1.000000000000000000, 0.000000000000000000, 0.000000000000000000 ) ) ;
#12862 = DIRECTION ( 'NONE',  ( -1.000000000000000000, 0.000000000000000000, 0.000000000000000000 ) ) ;
#12863 = DIRECTION ( 'NONE',  ( -0.000000000000000000, -1.000000000000000000, -0.000000000000000000 ) ) ;
#12864 = CARTESIAN_POINT ( 'NONE',  ( -36.06592381555557125, -2.436921198044748937, -22.43244911821614807 ) ) ;
#12865 = VECTOR ( 'NONE', #5039, 1000.000000000000000 ) ;
#12866 = VECTOR ( 'NONE', #59904, 1000.000000000000000 ) ;
#12867 = CARTESIAN_POINT ( 'NONE',  ( 2.241317068080782793, -0.09149433816010646425, -7.633845645378813494 ) ) ;
#12869 = AXIS2_PLACEMENT_3D ( 'NONE', #33017, #23066, #28371 ) ;
#12868 = B_SPLINE_CURVE_WITH_KNOTS ( 'NONE', 3,
 ( #8186, #58757, #32456, #43093, #63369, #17837, #37456, #59077 ),
 .UNSPECIFIED., .F., .F.,
 ( 4, 2, 2, 4 ),
 ( 0.01093700429183111326, 0.01319343274642247738, 0.01544986120101383975, 0.01996271811019656450 ),
 .UNSPECIFIED. ) ;
#12870 = CARTESIAN_POINT ( 'NONE',  ( 3.152665057734040488, 0.000000000000000000, 0.000000000000000000 ) ) ;
#12871 = ORIENTED_EDGE ( 'NONE', *, *, #47646, .T. ) ;
#12872 = DIRECTION ( 'NONE',  ( 1.000000000000000000, 0.000000000000000000, 0.000000000000000000 ) ) ;
#12873 = CARTESIAN_POINT ( 'NONE',  ( 29.73200328305864204, 9.106906332337908694, 10.00596268623472263 ) ) ;
#12874 = AXIS2_PLACEMENT_3D ( 'NONE', #48266, #43552, #12632 ) ;
#12875 = CARTESIAN_POINT ( 'NONE',  ( -10.50558643126015923, -29.12101583629321766, -8.365681325885642394 ) ) ;
#12876 = VERTEX_POINT ( 'NONE', #44621 ) ;
#12877 = CARTESIAN_POINT ( 'NONE',  ( -11.08084578044607582, -9.571663398071640572, -7.261247739973540227 ) ) ;
#12878 = CARTESIAN_POINT ( 'NONE',  ( 0.9296196016833688791, -8.327938962579976234, 9.278306863859505427 ) ) ;
#12879 = CARTESIAN_POINT ( 'NONE',  ( -28.66013792860432119, 0.4631296695479409919, 1.776574787184017179 ) ) ;
#12880 = VECTOR ( 'NONE', #52448, 1000.000000000000000 ) ;
#12881 = CARTESIAN_POINT ( 'NONE',  ( -29.59036887715360464, 2.131711947223947412, -13.33733930595583494 ) ) ;
#12882 = CARTESIAN_POINT ( 'NONE',  ( 0.2958664285830422402, -11.43993536884559425, 4.398464391600280798 ) ) ;
#12883 = ORIENTED_EDGE ( 'NONE', *, *, #15651, .F. ) ;
#12884 = DIRECTION ( 'NONE',  ( 1.000000000000000000, 0.000000000000000000, 0.000000000000000000 ) ) ;
#12885 = VERTEX_POINT ( 'NONE', #24697 ) ;
#12886 = AXIS2_PLACEMENT_3D ( 'NONE', #34807, #59454, #60109 ) ;
#12887 = EDGE_CURVE ( 'NONE', #23433, #38220, #39326, .T. ) ;
#12888 = CARTESIAN_POINT ( 'NONE',  ( 0.3665391374699464300, 10.76665847464320969, -5.911453292029489326 ) ) ;
#12889 = CARTESIAN_POINT ( 'NONE',  ( 2.440552418640498100, 7.301551120181799526, -2.447453236303752888 ) ) ;
#12890 = CARTESIAN_POINT ( 'NONE',  ( 2.350038591458110560, -8.533611140765442471, 6.324706260079973497 ) ) ;
#12891 = CARTESIAN_POINT ( 'NONE',  ( 2.241532322987418002, 0.01048837931145292675, -7.634455956583347636 ) ) ;
#12892 = FACE_OUTER_BOUND ( 'NONE', #44531, .T. ) ;
#12893 = CARTESIAN_POINT ( 'NONE',  ( 5.515539859299206427, 0.004759416711441679694, -0.003740028639278299410 ) ) ;
#12894 = DIRECTION ( 'NONE',  ( 1.000000000000000000, 0.000000000000000000, 0.000000000000000000 ) ) ;
#12895 = AXIS2_PLACEMENT_3D ( 'NONE', #22377, #57982, #17740 ) ;
#12896 = ORIENTED_EDGE ( 'NONE', *, *, #15643, .F. ) ;
#12897 = VECTOR ( 'NONE', #52652, 1000.000000000000000 ) ;
#12898 = VERTEX_POINT ( 'NONE', #24049 ) ;
#12899 = CARTESIAN_POINT ( 'NONE',  ( -37.00000000000000711, -3.645068577060105230, 11.16627499335654150 ) ) ;
#12900 = EDGE_LOOP ( 'NONE', ( #39816, #6766, #5375, #4354 ) ) ;
#12901 = B_SPLINE_CURVE_WITH_KNOTS ( 'NONE', 3,
 ( #58686, #53686, #18764, #54675, #14399, #45004, #33706 ),
 .UNSPECIFIED., .F., .F.,
 ( 4, 3, 4 ),
 ( 0.000000000000000000, 0.001700533616330578320, 0.005002426799374390387 ),
 .UNSPECIFIED. ) ;
#12902 = CARTESIAN_POINT ( 'NONE',  ( 2.000000000000001776, -0.08317740279924559776, -7.499538753794370294 ) ) ;
#12904 = CARTESIAN_POINT ( 'NONE',  ( 1.000000000000000888, 5.217815162096925086, -5.387430271863535403 ) ) ;
#12903 = AXIS2_PLACEMENT_3D ( 'NONE', #60634, #35356, #21042 ) ;
#12905 = CIRCLE ( 'NONE', #27751, 4.999999999999999112 ) ;
#12906 = DIRECTION ( 'NONE',  ( 0.9582930651793755139, -0.1254087680151165229, 0.2568015617827271724 ) ) ;
#12907 = ORIENTED_EDGE ( 'NONE', *, *, #60060, .F. ) ;
#12908 = CARTESIAN_POINT ( 'NONE',  ( -37.00000000000000711, 11.73808581813437968, -0.4353888892048790038 ) ) ;
#12909 = CARTESIAN_POINT ( 'NONE',  ( 2.899286259009683953, 1.713434346771327776, -7.664525129300146844 ) ) ;
#12910 = CARTESIAN_POINT ( 'NONE',  ( 37.00000000000000711, -1.791059740004337097, 12.05416472667166872 ) ) ;
#12911 = ORIENTED_EDGE ( 'NONE', *, *, #31598, .T. ) ;
#12912 = VERTEX_POINT ( 'NONE', #44001 ) ;
#12913 = LINE ( 'NONE', #33837, #51255 ) ;
#12914 = EDGE_CURVE ( 'NONE', #44234, #17999, #56315, .T. ) ;
#12915 = EDGE_LOOP ( 'NONE', ( #61458, #14171, #53661, #29563 ) ) ;
#12916 = CARTESIAN_POINT ( 'NONE',  ( 2.260457164927186291, 3.939659644572543584, 6.546788723198565307 ) ) ;
#12917 = VERTEX_POINT ( 'NONE', #49347 ) ;
#12918 = EDGE_LOOP ( 'NONE', ( #43931, #44348, #22885, #1513 ) ) ;
#12919 = VECTOR ( 'NONE', #64346, 1000.000000000000000 ) ;
#12920 = CARTESIAN_POINT ( 'NONE',  ( 34.00000000000000000, 11.99999999999999822, 0.000000000000000000 ) ) ;
#12921 = ADVANCED_FACE ( 'NONE', ( #3793 ), #44308, .T. ) ;
#12922 = DIRECTION ( 'NONE',  ( -0.2475719085175105416, 8.403603522408387294E-16, -0.9688695217174485563 ) ) ;
#12923 = AXIS2_PLACEMENT_3D ( 'NONE', #33499, #53790, #23190 ) ;
#12924 = FACE_OUTER_BOUND ( 'NONE', #19404, .T. ) ;
#12925 = DIRECTION ( 'NONE',  ( -1.000000000000000000, -0.000000000000000000, -0.000000000000000000 ) ) ;
#12926 = CARTESIAN_POINT ( 'NONE',  ( -35.00000000000000000, -3.213188559034318992, 11.29812557209475798 ) ) ;
#12927 = VECTOR ( 'NONE', #9829, 1000.000000000000000 ) ;
#12928 = LINE ( 'NONE', #8267, #44962 ) ;
#12929 = ORIENTED_EDGE ( 'NONE', *, *, #18267, .T. ) ;
#12930 = DIRECTION ( 'NONE',  ( -1.000000000000000000, 0.000000000000000000, -0.000000000000000000 ) ) ;
#12931 = CARTESIAN_POINT ( 'NONE',  ( 2.639814597422663667, 4.793557287999632877, 6.111633106000409654 ) ) ;
#12932 = CARTESIAN_POINT ( 'NONE',  ( 41.00000000000000711, -1.694065894508600678E-18, 1.500000000000000222 ) ) ;
#12933 = DIRECTION ( 'NONE',  ( -1.000000000000000000, 0.000000000000000000, 0.000000000000000000 ) ) ;
#12934 = CARTESIAN_POINT ( 'NONE',  ( 37.00000000000000711, -6.265926637539569910, -11.10408318471057676 ) ) ;
#12935 = CARTESIAN_POINT ( 'NONE',  ( 36.00000000000000711, -10.59380114696464581, 7.094637218249467914 ) ) ;
#12936 = CIRCLE ( 'NONE', #46923, 2.899999999999994582 ) ;
#12937 = CARTESIAN_POINT ( 'NONE',  ( 2.844750968616010400, -4.202329849280510565, -6.613363922490621327 ) ) ;
#12938 = DIRECTION ( 'NONE',  ( -1.000000000000000000, 0.000000000000000000, 0.000000000000000000 ) ) ;
#12939 = CARTESIAN_POINT ( 'NONE',  ( -37.00000000000000711, -8.830544224262881770, -9.196955404009390378 ) ) ;
#12940 = EDGE_CURVE ( 'NONE', #21973, #60604, #1176, .T. ) ;
#12941 = VERTEX_POINT ( 'NONE', #19724 ) ;
#12942 = DIRECTION ( 'NONE',  ( 0.000000000000000000, 0.000000000000000000, 1.000000000000000000 ) ) ;
#12943 = AXIS2_PLACEMENT_3D ( 'NONE', #44723, #39084, #4178 ) ;
#12944 = ORIENTED_EDGE ( 'NONE', *, *, #5, .F. ) ;
#12945 = DIRECTION ( 'NONE',  ( -1.000000000000000000, 0.000000000000000000, 0.000000000000000000 ) ) ;
#12946 = CARTESIAN_POINT ( 'NONE',  ( 2.305787727787085295, 5.970480882365287734, -4.792270232040832134 ) ) ;
#12947 = CARTESIAN_POINT ( 'NONE',  ( 37.00000000000000711, -11.37311665002365579, -2.936739658819832677 ) ) ;
#12948 = CARTESIAN_POINT ( 'NONE',  ( -35.04683013664716640, 0.0001018103929586065885, 0.01235741808121416756 ) ) ;
#12949 = CARTESIAN_POINT ( 'NONE',  ( 2.305787727787084407, 7.566723232958072032, 1.164987321564758371 ) ) ;
#12950 = ORIENTED_EDGE ( 'NONE', *, *, #45655, .T. ) ;
#12951 = DIRECTION ( 'NONE',  ( 1.000000000000000000, 0.000000000000000000, 0.000000000000000000 ) ) ;
#12952 = CARTESIAN_POINT ( 'NONE',  ( -35.00000000000000000, -11.30684963584386082, -4.545979934229532837 ) ) ;
#12953 = CARTESIAN_POINT ( 'NONE',  ( -18.76942114191558275, -13.50000000000000355, 0.6346529038414141510 ) ) ;
#12954 = CARTESIAN_POINT ( 'NONE',  ( 0.9207726606790023194, -30.53649492335445359, -15.30974548841835592 ) ) ;
#12955 = EDGE_CURVE ( 'NONE', #16089, #54132, #3332, .T. ) ;
#12956 = AXIS2_PLACEMENT_3D ( 'NONE', #63138, #52535, #7958 ) ;
#12957 = CARTESIAN_POINT ( 'NONE',  ( 35.00000000000000000, 8.295159312811978936, 8.927548052240801724 ) ) ;
#12958 = ORIENTED_EDGE ( 'NONE', *, *, #5488, .T. ) ;
#12959 = B_SPLINE_CURVE_WITH_KNOTS ( 'NONE', 3,
 ( #43617, #52952, #57960, #42970, #37662, #58624, #8069, #48323, #7384, #18384, #27666, #43287, #63247, #17717, #37975, #7739, #28660, #23350, #28024 ),
 .UNSPECIFIED., .F., .F.,
 ( 4, 3, 3, 3, 3, 3, 4 ),
 ( 5.421010862427522170E-20, 2.831840207499432383E-05, 4.217266859840160720E-05, 5.602024318395529550E-05, 6.290810167968680718E-05, 9.120440630944731252E-05, 0.0001153103026479744499 ),
 .UNSPECIFIED. ) ;
#12960 = CARTESIAN_POINT ( 'NONE',  ( 2.781367136451806665, -0.3081277311323283308, -7.808329083463450893 ) ) ;
#12961 = CARTESIAN_POINT ( 'NONE',  ( 2.000000000000001776, 5.814643797626986910, -3.550179297009520063 ) ) ;
#12962 = CARTESIAN_POINT ( 'NONE',  ( 36.00000000000000711, -7.094637218249427946, -10.59380114696467778 ) ) ;
#12963 = CIRCLE ( 'NONE', #45867, 4.999999999999999112 ) ;
#12964 = VECTOR ( 'NONE', #219, 1000.000000000000000 ) ;
#12965 = ORIENTED_EDGE ( 'NONE', *, *, #57118, .F. ) ;
#12967 = CARTESIAN_POINT ( 'NONE',  ( -9.824774371450907040, 12.26007224129469897, -5.655028462584398952 ) ) ;
#12966 = AXIS2_PLACEMENT_3D ( 'NONE', #55967, #50987, #10735 ) ;
#12969 = ORIENTED_EDGE ( 'NONE', *, *, #26792, .T. ) ;
#12968 = EDGE_CURVE ( 'NONE', #30390, #29592, #9648, .T. ) ;
#12970 = FACE_OUTER_BOUND ( 'NONE', #60912, .T. ) ;
#12971 = DIRECTION ( 'NONE',  ( -1.000000000000000000, -0.000000000000000000, 0.000000000000000000 ) ) ;
#12972 = CARTESIAN_POINT ( 'NONE',  ( 35.00000000000000000, 7.717887834988244045, -8.854740511458876639 ) ) ;
#12973 = DIRECTION ( 'NONE',  ( 1.000000000000000000, 0.000000000000000000, 0.000000000000000000 ) ) ;
#12974 = AXIS2_PLACEMENT_3D ( 'NONE', #20269, #55189, #34573 ) ;
#12975 = CARTESIAN_POINT ( 'NONE',  ( -22.27704833740210333, -2.142029987820955661, -2.993786163585799631 ) ) ;
#12976 = EDGE_CURVE ( 'NONE', #19103, #28220, #61671, .T. ) ;
#12977 = ORIENTED_EDGE ( 'NONE', *, *, #55676, .T. ) ;
#12978 = VERTEX_POINT ( 'NONE', #68 ) ;
#12979 = VERTEX_POINT ( 'NONE', #16006 ) ;
#12980 = DIRECTION ( 'NONE',  ( -1.000000000000000000, -0.000000000000000000, -0.000000000000000000 ) ) ;
#12981 = CARTESIAN_POINT ( 'NONE',  ( 3.152665057736111720, -7.281573230473792790, 3.161213418915395312 ) ) ;
#12983 = ADVANCED_FACE ( 'NONE', ( #1404 ), #55934, .T. ) ;
#12982 = B_SPLINE_CURVE_WITH_KNOTS ( 'NONE', 3,
 ( #15022, #66, #50310, #39316, #29349, #65557, #54651, #14045, #19388, #29998 ),
 .UNSPECIFIED., .F., .F.,
 ( 4, 2, 2, 2, 4 ),
 ( 3.469446951953614189E-18, 0.002586846717445558108, 0.003233558396806946768, 0.003880270076168335427, 0.005173693434891112747 ),
 .UNSPECIFIED. ) ;
#12984 = EDGE_LOOP ( 'NONE', ( #24887, #62933, #18845, #36420 ) ) ;
#12985 = DIRECTION ( 'NONE',  ( 0.000000000000000000, 0.01356324068817998940, -0.9999080150203990547 ) ) ;
#12986 = AXIS2_PLACEMENT_3D ( 'NONE', #19569, #60119, #14539 ) ;
#12987 = CARTESIAN_POINT ( 'NONE',  ( 2.258463476536646919, -7.546439757228810663, 1.192666169132608145 ) ) ;
#12988 = VERTEX_POINT ( 'NONE', #36292 ) ;
#12989 = CYLINDRICAL_SURFACE ( 'NONE', #12067, 5.225920239717171789 ) ;
#12990 = CARTESIAN_POINT ( 'NONE',  ( 2.266490820343225465, -2.750080098241469706, -7.130860233521876701 ) ) ;
#12991 = DIRECTION ( 'NONE',  ( 0.000000000000000000, -0.9847383929261598334, 0.1740410799127720121 ) ) ;
#12992 = EDGE_LOOP ( 'NONE', ( #39076, #48914, #24410, #722 ) ) ;
#12993 = ORIENTED_EDGE ( 'NONE', *, *, #35469, .F. ) ;
#12994 = CARTESIAN_POINT ( 'NONE',  ( 35.00000000000000000, -8.146229107149464355, -9.063649021438928699 ) ) ;
#12995 = EDGE_LOOP ( 'NONE', ( #28920, #51570, #10378, #10457 ) ) ;
#12996 = FACE_OUTER_BOUND ( 'NONE', #23597, .T. ) ;
#12997 = VERTEX_POINT ( 'NONE', #15672 ) ;
#12998 = AXIS2_PLACEMENT_3D ( 'NONE', #22645, #27285, #38234 ) ;
#12999 = FACE_OUTER_BOUND ( 'NONE', #44801, .T. ) ;
#13000 = DIRECTION ( 'NONE',  ( -1.000000000000000000, 0.000000000000000000, 0.000000000000000000 ) ) ;
#13001 = DIRECTION ( 'NONE',  ( -1.000000000000000000, 0.000000000000000000, 0.000000000000000000 ) ) ;
#13002 = AXIS2_PLACEMENT_3D ( 'NONE', #48547, #58523, #22950 ) ;
#13004 = CIRCLE ( 'NONE', #29983, 12.18650000000000055 ) ;
#13003 = CARTESIAN_POINT ( 'NONE',  ( -22.29770266787582500, 3.635870259503092949, 0.8895590726606663612 ) ) ;
#13005 = CARTESIAN_POINT ( 'NONE',  ( -10.00000000000000178, 0.000000000000000000, 0.000000000000000000 ) ) ;
#13006 = CARTESIAN_POINT ( 'NONE',  ( 0.4626703367445938464, -0.2831487465613948817, 12.30872794628576550 ) ) ;
#13007 = FACE_OUTER_BOUND ( 'NONE', #30849, .T. ) ;
#13009 = EDGE_LOOP ( 'NONE', ( #22397, #39701, #20987, #32851 ) ) ;
#13008 = B_SPLINE_CURVE_WITH_KNOTS ( 'NONE', 3,
 ( #61125, #15871, #15559, #30842, #25887, #46174, #51504, #620 ),
 .UNSPECIFIED., .F., .F.,
 ( 4, 2, 2, 4 ),
 ( 0.000000000000000000, 0.0003639104015150019687, 0.0007278208030300039374, 0.001455641606060009826 ),
 .UNSPECIFIED. ) ;
#13010 = CARTESIAN_POINT ( 'NONE',  ( 0.8320506296491574361, 10.95539209551947479, 5.883188144889816229 ) ) ;
#13011 =( BOUNDED_SURFACE ( )  B_SPLINE_SURFACE ( 3, 1, ( 
 ( #61610, #17312 ),
 ( #51006, #58202 ),
 ( #15726, #5799 ),
 ( #11095, #47898 ) ),
 .UNSPECIFIED., .F., .F., .F. ) 
 B_SPLINE_SURFACE_WITH_KNOTS ( ( 4, 4 ),
 ( 2, 2 ),
 ( 0.000000000000000000, 1.000000000000000000 ),
 ( 0.000000000000000000, 1.000000000000000000 ),
 .UNSPECIFIED. ) 
 GEOMETRIC_REPRESENTATION_ITEM ( )  RATIONAL_B_SPLINE_SURFACE ( (
 ( 1.000000000000000000, 1.000000000000000000),
 ( 0.9942764183789327692, 0.8450855930916580938),
 ( 0.9942764183789327692, 0.8450855930916580938),
 ( 1.000000000000000000, 1.000000000000000000) ) ) 
 REPRESENTATION_ITEM ( '' )  SURFACE ( )  );
#13012 = ORIENTED_EDGE ( 'NONE', *, *, #60060, .T. ) ;
#13013 = CARTESIAN_POINT ( 'NONE',  ( 2.255723233588951437, -2.736592204236698134, 7.132203433012278104 ) ) ;
#13014 = CARTESIAN_POINT ( 'NONE',  ( 5.516018279890452902, 0.004525000489649771626, 0.005042957932158598396 ) ) ;
#13015 = VERTEX_POINT ( 'NONE', #20352 ) ;
#13016 = CARTESIAN_POINT ( 'NONE',  ( -27.05874794189610455, 1.734723475976807094E-15, -8.673617379884035472E-15 ) ) ;
#13017 = DIRECTION ( 'NONE',  ( 0.000000000000000000, -0.01356324068817998940, 0.9999080150203990547 ) ) ;
#13018 = CARTESIAN_POINT ( 'NONE',  ( -22.30625920655495165, 2.750410778797892419, 2.610366806364663450 ) ) ;
#13019 =( GEOMETRIC_REPRESENTATION_CONTEXT ( 3 ) GLOBAL_UNCERTAINTY_ASSIGNED_CONTEXT ( ( #37671 ) ) GLOBAL_UNIT_ASSIGNED_CONTEXT ( ( #18881, #43817, #13858 ) ) REPRESENTATION_CONTEXT ( 'NONE', 'WORKASPACE' ) );
#13020 = ORIENTED_EDGE ( 'NONE', *, *, #62578, .T. ) ;
#13021 = VECTOR ( 'NONE', #17966, 1000.000000000000000 ) ;
#13022 = ORIENTED_EDGE ( 'NONE', *, *, #56697, .T. ) ;
#13023 = CARTESIAN_POINT ( 'NONE',  ( 35.00000000000000000, -3.614449339633571512, -11.17622378668005290 ) ) ;
#13024 = AXIS2_PLACEMENT_3D ( 'NONE', #16348, #26638, #406 ) ;
#13025 = ORIENTED_EDGE ( 'NONE', *, *, #22545, .T. ) ;
#13026 = CARTESIAN_POINT ( 'NONE',  ( -25.90770972894546276, -12.26982202440151681, 5.631397833353792848 ) ) ;
#13027 = LINE ( 'NONE', #28320, #60549 ) ;
#13028 = VECTOR ( 'NONE', #44798, 1000.000000000000000 ) ;
#13029 = CARTESIAN_POINT ( 'NONE',  ( 0.2646305136544072623, -9.296005949277173386, -7.972778379581646924 ) ) ;
#13030 = CARTESIAN_POINT ( 'NONE',  ( -37.00000000000000711, 12.60630747491665993, -1.908798535168240607 ) ) ;
#13031 = LINE ( 'NONE', #7055, #41657 ) ;
#13032 = ORIENTED_EDGE ( 'NONE', *, *, #15320, .F. ) ;
#13033 = FACE_OUTER_BOUND ( 'NONE', #2257, .T. ) ;
#13034 = EDGE_CURVE ( 'NONE', #19643, #6845, #63810, .T. ) ;
#13035 = AXIS2_PLACEMENT_3D ( 'NONE', #6129, #36698, #56995 ) ;
#13036 = CARTESIAN_POINT ( 'NONE',  ( -35.00000000000000000, 0.000000000000000000, 0.000000000000000000 ) ) ;
#13037 = DIRECTION ( 'NONE',  ( 1.000000000000000000, 0.000000000000000000, 0.000000000000000000 ) ) ;
#13038 = DIRECTION ( 'NONE',  ( -1.000000000000000000, 0.000000000000000000, 0.000000000000000000 ) ) ;
#13039 = CARTESIAN_POINT ( 'NONE',  ( 6.313836040153129936, -9.245614688376601720, -7.652703899474847304 ) ) ;
#13040 = DIRECTION ( 'NONE',  ( 0.000000000000000000, 0.01356324068817991828, -0.9999080150203990547 ) ) ;
#13041 = CIRCLE ( 'NONE', #51422, 5.000000000000000000 ) ;
#13042 = CIRCLE ( 'NONE', #56574, 4.999999999999999112 ) ;
#13043 = VECTOR ( 'NONE', #19824, 1000.000000000000114 ) ;
#13044 = EDGE_CURVE ( 'NONE', #56327, #53890, #51939, .T. ) ;
#13045 = ORIENTED_EDGE ( 'NONE', *, *, #40864, .F. ) ;
#13046 = CARTESIAN_POINT ( 'NONE',  ( 12.89197382821344107, -10.53456990936045656, -5.760929614845139213 ) ) ;
#13047 = ORIENTED_EDGE ( 'NONE', *, *, #17758, .F. ) ;
#13048 = DIRECTION ( 'NONE',  ( 0.000000000000000000, 0.000000000000000000, -1.000000000000000000 ) ) ;
#13049 = ADVANCED_FACE ( 'NONE', ( #56598 ), #4278, .F. ) ;
#13050 = CARTESIAN_POINT ( 'NONE',  ( 41.00000000000000711, 1.820029539775944174E-16, -1.500000000000000222 ) ) ;
#13051 = CARTESIAN_POINT ( 'NONE',  ( 0.3675815128205894289, 9.235491948680119023, -8.093875121225982738 ) ) ;
#13052 = ORIENTED_EDGE ( 'NONE', *, *, #3351, .F. ) ;
#13053 = CARTESIAN_POINT ( 'NONE',  ( 2.241536586108913820, 4.902521014023406565, -5.852386772940019632 ) ) ;
#13054 = EDGE_CURVE ( 'NONE', #39894, #53714, #27690, .T. ) ;
#13055 = ORIENTED_EDGE ( 'NONE', *, *, #43453, .F. ) ;
#13056 = VECTOR ( 'NONE', #7130, 1000.000000000000000 ) ;
#13057 = DIRECTION ( 'NONE',  ( 1.000000000000000000, 0.000000000000000000, 0.000000000000000000 ) ) ;
#13058 = ORIENTED_EDGE ( 'NONE', *, *, #54480, .F. ) ;
#13059 = ORIENTED_EDGE ( 'NONE', *, *, #64411, .F. ) ;
#13060 = FACE_OUTER_BOUND ( 'NONE', #30363, .T. ) ;
#13061 = VECTOR ( 'NONE', #59507, 1000.000000000000114 ) ;
#13062 = CARTESIAN_POINT ( 'NONE',  ( -22.31213670151049300, -3.398324501467297587, -1.669817926839923583 ) ) ;
#13063 = EDGE_CURVE ( 'NONE', #47012, #6868, #7522, .T. ) ;
#13064 = ORIENTED_EDGE ( 'NONE', *, *, #48523, .T. ) ;
#13065 = DIRECTION ( 'NONE',  ( 0.000000000000000000, 0.9718671068226450993, -0.2355298848897551256 ) ) ;
#13066 = CARTESIAN_POINT ( 'NONE',  ( 3.780834652287974773, 8.352030633203080257, 10.60629927458383115 ) ) ;
#13067 = LINE ( 'NONE', #2103, #16343 ) ;
#13068 = CARTESIAN_POINT ( 'NONE',  ( 17.82326783675071624, 8.603617134778573927, 8.377922036602647893 ) ) ;
#13069 = ORIENTED_EDGE ( 'NONE', *, *, #18400, .T. ) ;
#13070 = CARTESIAN_POINT ( 'NONE',  ( -15.27729454824424948, 5.151216734910788908, 25.00000000000000000 ) ) ;
#13071 = EDGE_CURVE ( 'NONE', #25930, #54896, #3457, .T. ) ;
#13072 = VECTOR ( 'NONE', #61910, 1000.000000000000000 ) ;
#13073 = CARTESIAN_POINT ( 'NONE',  ( 17.91771366450749525, -28.72671386922736758, 8.232269603669239544 ) ) ;
#13074 = CARTESIAN_POINT ( 'NONE',  ( 2.269879328256734219, -1.473193649116087078, -7.500604381673475984 ) ) ;
#13076 = VERTEX_POINT ( 'NONE', #25338 ) ;
#13075 = CARTESIAN_POINT ( 'NONE',  ( -24.43712776614061610, 9.284275035674196985, 7.605845515126569367 ) ) ;
#13077 = CARTESIAN_POINT ( 'NONE',  ( -35.00000000000000000, 12.74613886779085270, -0.3137578094507860738 ) ) ;
#13078 = ORIENTED_EDGE ( 'NONE', *, *, #60256, .F. ) ;
#13079 = DIRECTION ( 'NONE',  ( 1.000000000000000000, 0.000000000000000000, 0.000000000000000000 ) ) ;
#13080 = VERTEX_POINT ( 'NONE', #31628 ) ;
#13081 = DIRECTION ( 'NONE',  ( 1.000000000000000000, -0.000000000000000000, 0.000000000000000000 ) ) ;
#13082 = CARTESIAN_POINT ( 'NONE',  ( 3.152665057734040488, 0.000000000000000000, 0.000000000000000000 ) ) ;
#13083 = DIRECTION ( 'NONE',  ( 0.000000000000000000, 0.000000000000000000, 1.000000000000000000 ) ) ;
#13084 = CARTESIAN_POINT ( 'NONE',  ( 35.00000000000000000, 8.573591947375318156, -8.029056188533719052 ) ) ;
#13085 = CIRCLE ( 'NONE', #65089, 5.000000000000001776 ) ;
#13086 = CARTESIAN_POINT ( 'NONE',  ( 2.000000000000001776, -6.812627895098285258, -0.04423456934733380197 ) ) ;
#13087 = CARTESIAN_POINT ( 'NONE',  ( 2.000000000000001776, 6.643843315911821534, -1.507714007300717585 ) ) ;
#13088 = CARTESIAN_POINT ( 'NONE',  ( -22.27706089016750113, -3.548384797797525358, -0.9798385173596375619 ) ) ;
#13089 = EDGE_CURVE ( 'NONE', #38600, #52675, #46829, .T. ) ;
#13090 = ORIENTED_EDGE ( 'NONE', *, *, #35185, .T. ) ;
#13091 = CARTESIAN_POINT ( 'NONE',  ( 35.00000000000000000, 4.705694406421931860E-17, -3.469127814946512892E-15 ) ) ;
#13092 = ORIENTED_EDGE ( 'NONE', *, *, #3722, .F. ) ;
#13093 = EDGE_CURVE ( 'NONE', #41782, #18208, #26659, .T. ) ;
#13094 = ORIENTED_EDGE ( 'NONE', *, *, #35778, .T. ) ;
#13096 = AXIS2_PLACEMENT_3D ( 'NONE', #52177, #27218, #47510 ) ;
#13095 = CARTESIAN_POINT ( 'NONE',  ( 0.000000000000000000, -1.530946385938321219, -7.342084388195388556 ) ) ;
#13097 = CARTESIAN_POINT ( 'NONE',  ( 35.00000000000000000, 4.705694406421931860E-17, -3.469127814946512892E-15 ) ) ;
#13098 = DIRECTION ( 'NONE',  ( 0.000000000000000000, 0.01356324068817998940, -0.9999080150203989437 ) ) ;
#13099 = CARTESIAN_POINT ( 'NONE',  ( -22.28073302975500880, 0.9769664947681371281, 3.560599703067811816 ) ) ;
#13100 = LINE ( 'NONE', #28388, #8299 ) ;
#13101 = CARTESIAN_POINT ( 'NONE',  ( -35.00000000000000000, -1.591260454995328866, 12.08216339958900321 ) ) ;
#13102 = AXIS2_PLACEMENT_3D ( 'NONE', #12238, #32502, #27868 ) ;
#13103 = CARTESIAN_POINT ( 'NONE',  ( 1.104777566491143448, -11.07886329447272900, -5.844728374724383002 ) ) ;
#13104 = EDGE_LOOP ( 'NONE', ( #3976, #16122, #4237, #25353 ) ) ;
#13105 = CARTESIAN_POINT ( 'NONE',  ( 0.000000000000000000, 0.000000000000000000, 0.000000000000000000 ) ) ;
#13106 = AXIS2_PLACEMENT_3D ( 'NONE', #2407, #18359, #22686 ) ;
#13107 = CARTESIAN_POINT ( 'NONE',  ( -27.08417568107323703, -1.449568724721387092, -1.774279301226125760 ) ) ;
#13108 = CARTESIAN_POINT ( 'NONE',  ( -22.28506771379528573, 2.081613609299084011, 3.091577134491921619 ) ) ;
#13109 = AXIS2_PLACEMENT_3D ( 'NONE', #18488, #18135, #38407 ) ;
#13110 = EDGE_CURVE ( 'NONE', #24851, #49976, #14962, .T. ) ;
#13111 = DIRECTION ( 'NONE',  ( 0.000000000000000000, 0.7196168960969766548, 0.6943713148249667233 ) ) ;
#13112 = DIRECTION ( 'NONE',  ( 1.000000000000000000, 0.000000000000000000, 0.000000000000000000 ) ) ;
#13113 = CARTESIAN_POINT ( 'NONE',  ( 31.45682506574157244, -3.065323467461853024, -24.16565572891780889 ) ) ;
#13114 = CARTESIAN_POINT ( 'NONE',  ( 12.27732682522752583, 0.5231312807845712731, -11.98861953884736131 ) ) ;
#13115 = ORIENTED_EDGE ( 'NONE', *, *, #53199, .F. ) ;
#13116 = FACE_OUTER_BOUND ( 'NONE', #29597, .T. ) ;
#13117 = CARTESIAN_POINT ( 'NONE',  ( -36.00000000000000711, -11.80185301892984562, 4.824807283154076920 ) ) ;
#13118 = CARTESIAN_POINT ( 'NONE',  ( 35.00000000000000000, 4.705694406421931860E-17, -3.469127814946512892E-15 ) ) ;
#13119 = EDGE_CURVE ( 'NONE', #36445, #5130, #22424, .T. ) ;
#13120 = AXIS2_PLACEMENT_3D ( 'NONE', #7597, #48189, #16265 ) ;
#13121 = EDGE_CURVE ( 'NONE', #43985, #56943, #9771, .T. ) ;
#13122 = LINE ( 'NONE', #33406, #64916 ) ;
#13123 = CARTESIAN_POINT ( 'NONE',  ( 35.00000000000000000, 4.339012074899953220, -10.91536515067649660 ) ) ;
#13124 = VERTEX_POINT ( 'NONE', #52907 ) ;
#13125 = DIRECTION ( 'NONE',  ( 0.000000000000000000, 0.01356324068817998940, -0.9999080150203989437 ) ) ;
#13126 = CARTESIAN_POINT ( 'NONE',  ( 2.268878695252929845, -4.798796461778220390, -5.949442550447101574 ) ) ;
#13127 = DIRECTION ( 'NONE',  ( 1.000000000000000000, 0.000000000000000000, 0.000000000000000000 ) ) ;
#13128 = VERTEX_POINT ( 'NONE', #48592 ) ;
#13129 = CARTESIAN_POINT ( 'NONE',  ( -14.11589373245165469, 8.250315036047107142, -8.713914264323175729 ) ) ;
#13130 = CYLINDRICAL_SURFACE ( 'NONE', #9655, 4.999999999999999112 ) ;
#13131 = ADVANCED_FACE ( 'NONE', ( #31953 ), #57248, .T. ) ;
#13132 = ORIENTED_EDGE ( 'NONE', *, *, #2591, .F. ) ;
#13133 = VECTOR ( 'NONE', #35905, 1000.000000000000000 ) ;
#13134 = AXIS2_PLACEMENT_3D ( 'NONE', #2119, #42654, #43326 ) ;
#13135 = ORIENTED_EDGE ( 'NONE', *, *, #21369, .T. ) ;
#13136 = LINE ( 'NONE', #2854, #51178 ) ;
#13137 = AXIS2_PLACEMENT_3D ( 'NONE', #34124, #58791, #44420 ) ;
#13138 = B_SPLINE_CURVE_WITH_KNOTS ( 'NONE', 3,
 ( #38798, #59097, #33144, #63085, #17544, #37811, #22865, #28173, #50426, #50742, #8864, #50090 ),
 .UNSPECIFIED., .F., .F.,
 ( 4, 2, 2, 2, 2, 4 ),
 ( 2.096074351170153978E-17, 0.002188339370024745302, 0.004376678740049471522, 0.005470848425061835933, 0.006565018110074198610, 0.008753357480098915289 ),
 .UNSPECIFIED. ) ;
#13139 = ORIENTED_EDGE ( 'NONE', *, *, #13976, .T. ) ;
#13140 = CARTESIAN_POINT ( 'NONE',  ( -37.00000000000000711, 11.61175578952786047, 1.771820996347196697 ) ) ;
#13141 = DIRECTION ( 'NONE',  ( -1.000000000000000000, 0.000000000000000000, 0.000000000000000000 ) ) ;
#13142 = DIRECTION ( 'NONE',  ( -1.000000000000000000, 0.000000000000000000, 0.000000000000000000 ) ) ;
#13143 = CYLINDRICAL_SURFACE ( 'NONE', #18124, 5.000000000000000888 ) ;
#13144 = CARTESIAN_POINT ( 'NONE',  ( -27.22416769087903532, 9.103615227035337654, -7.837773337750173930 ) ) ;
#13145 = ADVANCED_FACE ( 'NONE', ( #62535 ), #17676, .T. ) ;
#13146 = AXIS2_PLACEMENT_3D ( 'NONE', #37215, #7287, #48226 ) ;
#13147 = DIRECTION ( 'NONE',  ( 0.000000000000000000, 0.8989688749565172277, 0.4380125133593943398 ) ) ;
#13149 = ORIENTED_EDGE ( 'NONE', *, *, #21369, .F. ) ;
#13148 = DIRECTION ( 'NONE',  ( -1.000000000000000000, 0.000000000000000000, -0.000000000000000000 ) ) ;
#13150 = DIRECTION ( 'NONE',  ( 0.000000000000000000, -0.9987865678893271815, 0.04924826701375693838 ) ) ;
#13151 = EDGE_CURVE ( 'NONE', #55517, #16276, #4366, .T. ) ;
#13152 = ORIENTED_EDGE ( 'NONE', *, *, #4902, .T. ) ;
#13153 = DIRECTION ( 'NONE',  ( 0.000000000000000000, -0.01356324068817998940, 0.9999080150203990547 ) ) ;
#13154 = VECTOR ( 'NONE', #20145, 1000.000000000000000 ) ;
#13155 = ORIENTED_EDGE ( 'NONE', *, *, #1761, .F. ) ;
#13156 = ORIENTED_EDGE ( 'NONE', *, *, #64756, .T. ) ;
#13157 = CARTESIAN_POINT ( 'NONE',  ( -18.12415734164024883, 6.857820005957854015, 11.63132115085990570 ) ) ;
#13158 = EDGE_CURVE ( 'NONE', #53510, #57274, #32708, .T. ) ;
#13159 = CARTESIAN_POINT ( 'NONE',  ( -2.647174210752905488, -26.63290002157760128, 16.10638009382239488 ) ) ;
#13160 = CARTESIAN_POINT ( 'NONE',  ( -25.43923780825302572, 12.11207825353047518, 5.970565962100374158 ) ) ;
#13161 = CARTESIAN_POINT ( 'NONE',  ( 36.00000000000000711, -8.235637554476713973, -9.733281772932135922 ) ) ;
#13162 = CARTESIAN_POINT ( 'NONE',  ( 0.000000000000000000, 5.450255447309811707, -4.087611905901392007 ) ) ;
#13163 = EDGE_CURVE ( 'NONE', #50412, #7150, #58576, .T. ) ;
#13164 = DIRECTION ( 'NONE',  ( 1.000000000000000000, -0.000000000000000000, -0.000000000000000000 ) ) ;
#13166 = VERTEX_POINT ( 'NONE', #33283 ) ;
#13165 = EDGE_CURVE ( 'NONE', #27716, #10498, #56111, .T. ) ;
#13167 = CARTESIAN_POINT ( 'NONE',  ( -22.27711653538342773, -0.4190680140413403088, -3.657713416444744237 ) ) ;
#13168 = CARTESIAN_POINT ( 'NONE',  ( 0.7400311444011711259, -3.907401494355001059, 11.77295732453933041 ) ) ;
#13169 = DIRECTION ( 'NONE',  ( -1.000000000000000000, 0.000000000000000000, 0.000000000000000000 ) ) ;
#13170 = AXIS2_PLACEMENT_3D ( 'NONE', #5590, #595, #35145 ) ;
#13171 = ORIENTED_EDGE ( 'NONE', *, *, #44204, .T. ) ;
#13172 = EDGE_CURVE ( 'NONE', #29748, #48808, #23484, .T. ) ;
#13173 = CARTESIAN_POINT ( 'NONE',  ( 2.941278708680199916, 5.248410529370268307, -3.185832147968391759 ) ) ;
#13174 = ORIENTED_EDGE ( 'NONE', *, *, #43987, .F. ) ;
#13175 = CARTESIAN_POINT ( 'NONE',  ( 2.257661810676419911, -7.499185766072598902, 1.459225434025957835 ) ) ;
#13176 = CARTESIAN_POINT ( 'NONE',  ( 0.3401186441510234970, -10.49699112323338213, -6.355596563012414713 ) ) ;
#13177 = CARTESIAN_POINT ( 'NONE',  ( 5.516018279890452902, -0.003580555109620837603, -0.005752102158673828673 ) ) ;
#13178 = CARTESIAN_POINT ( 'NONE',  ( -35.00000000000000000, 0.2661492558805056974, -12.18359334611896116 ) ) ;
#13179 = DIRECTION ( 'NONE',  ( -1.000000000000000000, -0.000000000000000000, 0.000000000000000000 ) ) ;
#13180 = CARTESIAN_POINT ( 'NONE',  ( 0.000000000000000000, 4.376687952327335651, 5.220963330856624118 ) ) ;
#13181 = CIRCLE ( 'NONE', #49326, 2.899999999999994582 ) ;
#13182 = DIRECTION ( 'NONE',  ( 0.000000000000000000, -0.8515178078024921993, 0.5243256840888473880 ) ) ;
#13183 = ORIENTED_EDGE ( 'NONE', *, *, #55933, .T. ) ;
#13184 = CARTESIAN_POINT ( 'NONE',  ( -10.00000000000000178, 0.000000000000000000, 0.000000000000000000 ) ) ;
#13185 = EDGE_LOOP ( 'NONE', ( #2812, #54877, #31444, #26570 ) ) ;
#13186 = CARTESIAN_POINT ( 'NONE',  ( -27.32343372485686217, 1.382463360572562028, 2.674948176236182640 ) ) ;
#13187 = AXIS2_PLACEMENT_3D ( 'NONE', #44436, #49146, #59421 ) ;
#13188 = CARTESIAN_POINT ( 'NONE',  ( 2.589278595513707870, 4.794929105510967737, -6.089088204449037534 ) ) ;
#13189 = CARTESIAN_POINT ( 'NONE',  ( 2.000000000000001776, -3.152010634611731366, 6.039758645301271933 ) ) ;
#13190 = EDGE_CURVE ( 'NONE', #61135, #42299, #64203, .T. ) ;
#13191 = ORIENTED_EDGE ( 'NONE', *, *, #39564, .T. ) ;
#13192 = LINE ( 'NONE', #9167, #54610 ) ;
#13193 = ORIENTED_EDGE ( 'NONE', *, *, #65060, .T. ) ;
#13194 = DIRECTION ( 'NONE',  ( -1.000000000000000000, 0.000000000000000000, 0.000000000000000000 ) ) ;
#13195 = DIRECTION ( 'NONE',  ( 1.000000000000000000, 0.000000000000000000, 0.000000000000000000 ) ) ;
#13196 = CARTESIAN_POINT ( 'NONE',  ( -35.00000000000000000, 8.830544224262945718, 9.196955404009328205 ) ) ;
#13197 = DIRECTION ( 'NONE',  ( 0.000000000000000000, 0.5987040770935676548, -0.8009703041134168533 ) ) ;
#13198 = ORIENTED_EDGE ( 'NONE', *, *, #27374, .T. ) ;
#13199 = AXIS2_PLACEMENT_3D ( 'NONE', #45322, #15050, #35662 ) ;
#13200 = DIRECTION ( 'NONE',  ( 1.000000000000000000, 0.000000000000000000, 0.000000000000000000 ) ) ;
#13201 = DIRECTION ( 'NONE',  ( 1.000000000000000000, 0.000000000000000000, 0.000000000000000000 ) ) ;
#13202 = EDGE_CURVE ( 'NONE', #14676, #43944, #28794, .T. ) ;
#13203 = CARTESIAN_POINT ( 'NONE',  ( -27.04788180060269553, 0.2724356095623531870, -3.218072544330549345 ) ) ;
#13204 = CARTESIAN_POINT ( 'NONE',  ( -35.00000000000000000, -2.216820770815165265, 11.53507381115582575 ) ) ;
#13205 = CARTESIAN_POINT ( 'NONE',  ( -27.08421723179412410, -0.5069555058557356775, -2.234476190936522499 ) ) ;
#13206 = CARTESIAN_POINT ( 'NONE',  ( 0.7400311444011745676, -4.574267895796777061, -11.53023780418230970 ) ) ;
#13207 =( BOUNDED_CURVE ( )  B_SPLINE_CURVE ( 3, ( #45399, #40749, #61037, #35074 ),
 .UNSPECIFIED., .F., .F. ) 
 B_SPLINE_CURVE_WITH_KNOTS ( ( 4, 4 ),
 ( 3.531674309133673528, 3.627469539221107375 ),
 .UNSPECIFIED. ) 
 CURVE ( )  GEOMETRIC_REPRESENTATION_ITEM ( )  RATIONAL_B_SPLINE_CURVE ( ( 1.000000000000000000, 0.9992354190151078175, 0.9992354190151078175, 1.000000000000000000 ) ) 
 REPRESENTATION_ITEM ( '' )  );
#13208 = ORIENTED_EDGE ( 'NONE', *, *, #23204, .T. ) ;
#13209 = CARTESIAN_POINT ( 'NONE',  ( -27.08421723179412055, 1.681635392574631460, -1.556274442127712820 ) ) ;
#13210 = CARTESIAN_POINT ( 'NONE',  ( 5.530133899448235191, -0.01594518557925637958, 0.001124651387254935967 ) ) ;
#13211 = CARTESIAN_POINT ( 'NONE',  ( -2.647174210752905488, -25.80125502049867947, -15.55106108913133767 ) ) ;
#13212 = ORIENTED_EDGE ( 'NONE', *, *, #18430, .F. ) ;
#13213 = CARTESIAN_POINT ( 'NONE',  ( 37.00000000000000711, 10.02106554660720050, 7.882940143791662635 ) ) ;
#13214 = CARTESIAN_POINT ( 'NONE',  ( 0.6511581176963219253, -8.205008037406710031, 9.263557799003001136 ) ) ;
#13215 = DIRECTION ( 'NONE',  ( 0.000000000000000000, -0.9651210252299767811, -0.2618041379715732586 ) ) ;
#13216 = EDGE_CURVE ( 'NONE', #63114, #1051, #62765, .T. ) ;
#13217 = DIRECTION ( 'NONE',  ( 0.000000000000000000, -0.01356324068817998940, 0.9999080150203990547 ) ) ;
#13218 = EDGE_CURVE ( 'NONE', #33743, #34466, #31962, .T. ) ;
#13219 = CARTESIAN_POINT ( 'NONE',  ( 0.3474126878361781801, -11.44231427242452881, 4.439989671676180194 ) ) ;
#13220 = ORIENTED_EDGE ( 'NONE', *, *, #47009, .F. ) ;
#13221 = CARTESIAN_POINT ( 'NONE',  ( 47.00000000000000711, 4.705694406421931860E-17, -3.469127814946512892E-15 ) ) ;
#13222 = ORIENTED_EDGE ( 'NONE', *, *, #3428, .T. ) ;
#13223 = CARTESIAN_POINT ( 'NONE',  ( 2.245754705088394587, -7.212684575686793664, 2.506725724682641765 ) ) ;
#13224 = DIRECTION ( 'NONE',  ( 0.000000000000000000, 0.9987865678893275145, -0.04924826701374940968 ) ) ;
#13225 = CARTESIAN_POINT ( 'NONE',  ( 2.770579946183332254, 7.437949029067727480, -2.384572752174010990 ) ) ;
#13226 = CARTESIAN_POINT ( 'NONE',  ( 2.556980015514275006, -4.795979673457624770, 6.074557383033025282 ) ) ;
#13227 = DIRECTION ( 'NONE',  ( 0.000000000000000000, 0.000000000000000000, -1.000000000000000000 ) ) ;
#13228 = DIRECTION ( 'NONE',  ( 0.000000000000000000, 0.9999080150203989437, 0.01356324068817649567 ) ) ;
#13229 = DIRECTION ( 'NONE',  ( -1.000000000000000000, 0.000000000000000000, -0.000000000000000000 ) ) ;
#13230 = CARTESIAN_POINT ( 'NONE',  ( 0.2646305136544065406, 7.770320294339174261, 9.465888453932986835 ) ) ;
#13231 = ORIENTED_EDGE ( 'NONE', *, *, #58494, .F. ) ;
#13232 = AXIS2_PLACEMENT_3D ( 'NONE', #27772, #48075, #2533 ) ;
#13233 = EDGE_LOOP ( 'NONE', ( #11361, #48491, #5622, #48455 ) ) ;
#13234 = LINE ( 'NONE', #15186, #45921 ) ;
#13235 = EDGE_LOOP ( 'NONE', ( #51989, #22687, #5207, #29399 ) ) ;
#13236 = EDGE_CURVE ( 'NONE', #61588, #29827, #39364, .T. ) ;
#13237 = FILL_AREA_STYLE ('',( #62779 ) ) ;
#13238 = ADVANCED_FACE ( 'NONE', ( #59221 ), #29926, .T. ) ;
#13239 = CARTESIAN_POINT ( 'NONE',  ( -35.00000000000000000, 12.14284015767850100, 1.030638227056609679 ) ) ;
#13240 = LINE ( 'NONE', #9208, #38536 ) ;
#13241 = EDGE_CURVE ( 'NONE', #54831, #32188, #28616, .T. ) ;
#13242 = CARTESIAN_POINT ( 'NONE',  ( -22.27786964138239867, -1.536369256421345142, 3.347945419004146661 ) ) ;
#13243 = VERTEX_POINT ( 'NONE', #24617 ) ;
#13244 = CARTESIAN_POINT ( 'NONE',  ( 0.3610902822527229383, 5.910495176556332275, -10.76187877352507094 ) ) ;
#13245 = AXIS2_PLACEMENT_3D ( 'NONE', #5029, #40248, #19674 ) ;
#13246 = CARTESIAN_POINT ( 'NONE',  ( 2.305787727787083519, 1.493241775258524084, -7.508843116234142911 ) ) ;
#13247 = CARTESIAN_POINT ( 'NONE',  ( -19.56743653832047158, -33.00000000000000000, 5.000000000000000888 ) ) ;
#13248 = ORIENTED_EDGE ( 'NONE', *, *, #65711, .T. ) ;
#13249 = VERTEX_POINT ( 'NONE', #8997 ) ;
#13250 = EDGE_CURVE ( 'NONE', #30538, #9776, #12122, .T. ) ;
#13251 = CARTESIAN_POINT ( 'NONE',  ( 34.00000000000000000, -11.99999999999997335, 0.000000000000000000 ) ) ;
#13253 = EDGE_LOOP ( 'NONE', ( #788, #39664, #9257, #30259 ) ) ;
#13252 = AXIS2_PLACEMENT_3D ( 'NONE', #24620, #15612, #44900 ) ;
#13254 = CARTESIAN_POINT ( 'NONE',  ( 0.9232058338315048962, 9.306586124266598148, 8.301689855530199225 ) ) ;
#13255 = ORIENTED_EDGE ( 'NONE', *, *, #53823, .F. ) ;
#13256 = ORIENTED_EDGE ( 'NONE', *, *, #34718, .F. ) ;
#13257 = CARTESIAN_POINT ( 'NONE',  ( 12.49336221634852429, 0.1658369216508863153, 13.50000000000000355 ) ) ;
#13258 = AXIS2_PLACEMENT_3D ( 'NONE', #43727, #3525, #29413 ) ;
#13259 = CARTESIAN_POINT ( 'NONE',  ( -27.09030469827931853, -1.608164674722575072, 1.657623467486013968 ) ) ;
#13260 = CARTESIAN_POINT ( 'NONE',  ( -35.00000000000000000, -0.4871980014162358152, 12.74068829017553739 ) ) ;
#13261 = DIRECTION ( 'NONE',  ( -1.000000000000000000, 0.000000000000000000, 0.000000000000000000 ) ) ;
#13262 = FACE_OUTER_BOUND ( 'NONE', #27646, .T. ) ;
#13263 = ADVANCED_FACE ( 'NONE', ( #9628 ), #58916, .T. ) ;
#13264 = DIRECTION ( 'NONE',  ( -1.000000000000000000, 0.000000000000000000, 0.000000000000000000 ) ) ;
#13265 = VERTEX_POINT ( 'NONE', #9300 ) ;
#13266 = DIRECTION ( 'NONE',  ( -1.000000000000000000, -0.000000000000000000, -0.000000000000000000 ) ) ;
#13267 = CARTESIAN_POINT ( 'NONE',  ( 2.990245332647872623, 1.974808303407790344, -8.248134185053331180 ) ) ;
#13268 = DIRECTION ( 'NONE',  ( 1.000000000000000000, 0.000000000000000000, -0.000000000000000000 ) ) ;
#13269 = CARTESIAN_POINT ( 'NONE',  ( 0.000000000000000000, 3.073484823194335025, 6.841322316745041654 ) ) ;
#13270 = CARTESIAN_POINT ( 'NONE',  ( -18.11422852383967452, 13.12233133686801345, 3.247147390179137449 ) ) ;
#13271 = CARTESIAN_POINT ( 'NONE',  ( 22.57855258442564761, -4.427776684447072952, 12.75322679295976691 ) ) ;
#13272 = CARTESIAN_POINT ( 'NONE',  ( -10.00000000000000178, 0.000000000000000000, 0.000000000000000000 ) ) ;
#13273 = CARTESIAN_POINT ( 'NONE',  ( -37.00000000000000711, 11.10408318471068689, -6.265926637539373623 ) ) ;
#13274 = CARTESIAN_POINT ( 'NONE',  ( 0.3675815128205894289, 5.910255304480445560, 10.76447900494942367 ) ) ;
#13275 = AXIS2_PLACEMENT_3D ( 'NONE', #46636, #32622, #1090 ) ;
#13276 = ORIENTED_EDGE ( 'NONE', *, *, #36988, .F. ) ;
#13277 = CARTESIAN_POINT ( 'NONE',  ( 3.152665057734127529, -7.281573230474269742, -3.161213418913537687 ) ) ;
#13278 = EDGE_CURVE ( 'NONE', #19899, #26297, #49892, .T. ) ;
#13279 = ORIENTED_EDGE ( 'NONE', *, *, #3641, .T. ) ;
#13280 = CARTESIAN_POINT ( 'NONE',  ( 0.3665391374699465965, 8.095513416941230389, 9.237363111276794214 ) ) ;
#13281 = CARTESIAN_POINT ( 'NONE',  ( 37.00000000000000711, 2.185196060784047045, 11.54110654723646157 ) ) ;
#13282 = CARTESIAN_POINT ( 'NONE',  ( 11.98523602762309537, -10.93063363335638272, -7.929333770360376121 ) ) ;
#13283 = CARTESIAN_POINT ( 'NONE',  ( 2.000000000000001776, 3.152010634611693174, 6.039758645301271933 ) ) ;
#13284 = CARTESIAN_POINT ( 'NONE',  ( 0.2646305136544065406, -4.312539723326059615, -11.46223899740604324 ) ) ;
#13285 = ORIENTED_EDGE ( 'NONE', *, *, #14244, .T. ) ;
#13286 = LINE ( 'NONE', #18929, #32112 ) ;
#13287 = ADVANCED_FACE ( 'NONE', ( #3378 ), #44896, .T. ) ;
#13288 = DIRECTION ( 'NONE',  ( -1.000000000000000000, 0.000000000000000000, -0.000000000000000000 ) ) ;
#13289 = CARTESIAN_POINT ( 'NONE',  ( 47.00000000000000711, 4.705694406421931860E-17, -3.469127814946512892E-15 ) ) ;
#13290 = CARTESIAN_POINT ( 'NONE',  ( 2.000000000000001776, -4.444115772890066651, -5.163689623839394116 ) ) ;
#13291 = EDGE_LOOP ( 'NONE', ( #58125, #44885, #28268, #48181 ) ) ;
#13292 = CARTESIAN_POINT ( 'NONE',  ( 2.491965175173673774, -0.2120508241296135687, -7.715025372670731407 ) ) ;
#13293 = CARTESIAN_POINT ( 'NONE',  ( 2.589278595512710002, 5.779442428606824222, -5.163950571302039272 ) ) ;
#13295 = ADVANCED_FACE ( 'NONE', ( #13643 ), #19645, .T. ) ;
#13294 = DIRECTION ( 'NONE',  ( 1.000000000000000000, 0.000000000000000000, 0.000000000000000000 ) ) ;
#13296 = EDGE_CURVE ( 'NONE', #22914, #1326, #21343, .T. ) ;
#13297 = EDGE_CURVE ( 'NONE', #50524, #21944, #20298, .T. ) ;
#13298 = ORIENTED_EDGE ( 'NONE', *, *, #51785, .T. ) ;
#13299 = ORIENTED_EDGE ( 'NONE', *, *, #4744, .T. ) ;
#13300 = CARTESIAN_POINT ( 'NONE',  ( -9.502271734863095176, 12.89234648065891875, -4.021717619241973907 ) ) ;
#13301 = ORIENTED_EDGE ( 'NONE', *, *, #51893, .F. ) ;
#13302 = CARTESIAN_POINT ( 'NONE',  ( -37.00000000000000711, -6.584150480049622445, 10.25474254703950905 ) ) ;
#13303 = DIRECTION ( 'NONE',  ( 0.000000000000000000, -0.3554799084908832896, -0.9346839223284592046 ) ) ;
#13304 = DIRECTION ( 'NONE',  ( 0.000000000000000000, 0.01356324068817992175, -0.9999080150203990547 ) ) ;
#13305 = CYLINDRICAL_SURFACE ( 'NONE', #29001, 12.18649999999999878 ) ;
#13306 = DIRECTION ( 'NONE',  ( 0.000000000000000000, 0.000000000000000000, -1.000000000000000000 ) ) ;
#13307 = EDGE_LOOP ( 'NONE', ( #30891, #47911, #37853, #34978 ) ) ;
#13308 = VERTEX_POINT ( 'NONE', #61823 ) ;
#13309 = ORIENTED_EDGE ( 'NONE', *, *, #37130, .F. ) ;
#13310 = FACE_OUTER_BOUND ( 'NONE', #24180, .T. ) ;
#13311 = EDGE_CURVE ( 'NONE', #32907, #12370, #124, .T. ) ;
#13312 = AXIS2_PLACEMENT_3D ( 'NONE', #25287, #24978, #14633 ) ;
#13313 = CARTESIAN_POINT ( 'NONE',  ( 2.941278708680199916, 4.048809123187997905, -4.615461433467216601 ) ) ;
#13314 = ORIENTED_EDGE ( 'NONE', *, *, #53865, .T. ) ;
#13315 = DIRECTION ( 'NONE',  ( 0.000000000000000000, 0.000000000000000000, 1.000000000000000000 ) ) ;
#13316 = EDGE_CURVE ( 'NONE', #42911, #18188, #56519, .T. ) ;
#13317 = DIRECTION ( 'NONE',  ( -1.000000000000000000, -1.836970198721029688E-16, 0.000000000000000000 ) ) ;
#13318 = EDGE_LOOP ( 'NONE', ( #35936, #58497, #13355, #22755 ) ) ;
#13319 = CARTESIAN_POINT ( 'NONE',  ( 2.241536586108912044, 6.608496983003842473, -3.822683724643396008 ) ) ;
#13320 = DIRECTION ( 'NONE',  ( -1.000000000000000000, 0.000000000000000000, 0.000000000000000000 ) ) ;
#13321 = CARTESIAN_POINT ( 'NONE',  ( 35.00000000000000000, -12.17626345777663310, 0.4993900848168664752 ) ) ;
#13322 = ORIENTED_EDGE ( 'NONE', *, *, #31629, .T. ) ;
#13323 = ORIENTED_EDGE ( 'NONE', *, *, #65504, .T. ) ;
#13324 = LINE ( 'NONE', #59531, #11873 ) ;
#13325 = ORIENTED_EDGE ( 'NONE', *, *, #8383, .F. ) ;
#13326 = DIRECTION ( 'NONE',  ( 0.000000000000000000, 0.4380125133593912312, -0.8989688749565187820 ) ) ;
#13327 = ORIENTED_EDGE ( 'NONE', *, *, #49502, .F. ) ;
#13328 = CARTESIAN_POINT ( 'NONE',  ( 0.2653141334712599830, -4.147025708564500590, 11.52266042163704718 ) ) ;
#13329 = DIRECTION ( 'NONE',  ( 0.000000000000000000, 0.01356324068817991828, -0.9999080150203990547 ) ) ;
#13330 = CARTESIAN_POINT ( 'NONE',  ( -19.56743653832047514, -28.99999999999999645, 5.000000000000000888 ) ) ;
#13331 = CARTESIAN_POINT ( 'NONE',  ( 37.00000000000000711, 12.14284015767851344, 1.030638227056429157 ) ) ;
#13332 = DIRECTION ( 'NONE',  ( 0.000000000000000000, -0.01356324068817998940, 0.9999080150203990547 ) ) ;
#13333 = CYLINDRICAL_SURFACE ( 'NONE', #35545, 5.000000000000000888 ) ;
#13334 = ORIENTED_EDGE ( 'NONE', *, *, #8018, .F. ) ;
#13335 = CARTESIAN_POINT ( 'NONE',  ( -36.00000000000000711, 4.237174932027226504, 12.02534193257722528 ) ) ;
#13336 = AXIS2_PLACEMENT_3D ( 'NONE', #44839, #65118, #14879 ) ;
#13337 = ORIENTED_EDGE ( 'NONE', *, *, #20413, .T. ) ;
#13338 = CARTESIAN_POINT ( 'NONE',  ( 2.298277635560275645, -2.772101951899011762, 7.133696409974386476 ) ) ;
#13339 = DIRECTION ( 'NONE',  ( -1.000000000000000000, 0.000000000000000000, -0.000000000000000000 ) ) ;
#13340 = ORIENTED_EDGE ( 'NONE', *, *, #22497, .T. ) ;
#13341 = CARTESIAN_POINT ( 'NONE',  ( -14.11589373245165469, 8.250315036047107142, 8.713914264323175729 ) ) ;
#13342 = CARTESIAN_POINT ( 'NONE',  ( 0.2739690278137235091, 6.282352088166262227, 10.51531306167489177 ) ) ;
#13343 = CARTESIAN_POINT ( 'NONE',  ( 0.2652384529303120075, -9.423437232855615520, -7.820949643217239178 ) ) ;
#13344 = CIRCLE ( 'NONE', #20749, 12.18650000000000055 ) ;
#13345 = EDGE_LOOP ( 'NONE', ( #52255, #51777, #36537, #13314 ) ) ;
#13346 = VERTEX_POINT ( 'NONE', #20621 ) ;
#13347 = DIRECTION ( 'NONE',  ( -0.000000000000000000, 1.000000000000000000, -0.000000000000000000 ) ) ;
#13348 = EDGE_CURVE ( 'NONE', #63832, #58967, #15608, .T. ) ;
#13349 = VERTEX_POINT ( 'NONE', #30571 ) ;
#13350 = CARTESIAN_POINT ( 'NONE',  ( -25.74809257979862309, -12.21955862071013676, 5.740220618591444612 ) ) ;
#13351 = CARTESIAN_POINT ( 'NONE',  ( -37.00000000000000711, 0.000000000000000000, 0.000000000000000000 ) ) ;
#13352 = CARTESIAN_POINT ( 'NONE',  ( 18.84867683979355846, 5.944105725974518251, 12.12095735156415088 ) ) ;
#13353 = CARTESIAN_POINT ( 'NONE',  ( -35.00000000000000000, 0.000000000000000000, 0.000000000000000000 ) ) ;
#13354 = DIRECTION ( 'NONE',  ( -1.000000000000000000, 0.000000000000000000, 0.000000000000000000 ) ) ;
#13355 = ORIENTED_EDGE ( 'NONE', *, *, #50683, .F. ) ;
#13356 = CARTESIAN_POINT ( 'NONE',  ( 2.241352910868908310, -1.407733736974815963, -7.503490710578247125 ) ) ;
#13357 = CONICAL_SURFACE ( 'NONE', #30360, 7.938172270156617749, 1.280189991382167047 ) ;
#13358 = EDGE_CURVE ( 'NONE', #49507, #36860, #35177, .T. ) ;
#13359 = CARTESIAN_POINT ( 'NONE',  ( -27.01437459610461644, -13.31613970204372421, -2.220455681983950935 ) ) ;
#13360 = CARTESIAN_POINT ( 'NONE',  ( 23.90122759429952026, 11.31311706520687288, -7.370651591097819200 ) ) ;
#13361 = LINE ( 'NONE', #18374, #47680 ) ;
#13362 = CARTESIAN_POINT ( 'NONE',  ( 35.00000000000000000, -12.15823808070322798, -0.8294751490778934366 ) ) ;
#13363 = CARTESIAN_POINT ( 'NONE',  ( 6.598188397287249707, -8.822549351475428736, -8.136977447280584030 ) ) ;
#13364 = CARTESIAN_POINT ( 'NONE',  ( -22.28415773361649954, -2.647149619609361793, -2.588610893123082235 ) ) ;
#13365 = VECTOR ( 'NONE', #11043, 1000.000000000000000 ) ;
#13366 = ORIENTED_EDGE ( 'NONE', *, *, #65726, .F. ) ;
#13367 = DIRECTION ( 'NONE',  ( -0.000000000000000000, -1.000000000000000000, -0.000000000000000000 ) ) ;
#13368 = CIRCLE ( 'NONE', #53783, 5.000000000000000888 ) ;
#13369 = ORIENTED_EDGE ( 'NONE', *, *, #889, .T. ) ;
#13370 = CARTESIAN_POINT ( 'NONE',  ( 0.3474126878361825654, 1.876013288000214274, -12.12932967384298522 ) ) ;
#13371 = DIRECTION ( 'NONE',  ( -0.9606638835031803270, 0.2674900627617600724, 0.07465901992591084113 ) ) ;
#13372 = DIRECTION ( 'NONE',  ( -1.000000000000000000, -0.000000000000000000, 0.000000000000000000 ) ) ;
#13373 = ORIENTED_EDGE ( 'NONE', *, *, #52480, .F. ) ;
#13374 = FACE_OUTER_BOUND ( 'NONE', #22044, .T. ) ;
#13375 = VERTEX_POINT ( 'NONE', #20278 ) ;
#13376 = ORIENTED_EDGE ( 'NONE', *, *, #27283, .F. ) ;
#13377 = ORIENTED_EDGE ( 'NONE', *, *, #1969, .T. ) ;
#13378 = B_SPLINE_CURVE_WITH_KNOTS ( 'NONE', 3,
 ( #1943, #62772, #28200, #2628, #22211, #27525, #47820, #42472, #42822, #17891, #63110, #48489, #17239, #22891, #8238, #55088, #18877, #29183, #18574 ),
 .UNSPECIFIED., .F., .F.,
 ( 4, 3, 3, 3, 3, 3, 4 ),
 ( 6.952433221959954168E-18, 2.825908398831159730E-05, 4.208813692483961120E-05, 5.591713746943971492E-05, 6.279584083232174897E-05, 9.105792820297123661E-05, 0.0001153131102488859469 ),
 .UNSPECIFIED. ) ;
#13379 = CYLINDRICAL_SURFACE ( 'NONE', #62057, 12.18650000000000055 ) ;
#13380 = CIRCLE ( 'NONE', #9109, 12.74999999999999822 ) ;
#13381 = CARTESIAN_POINT ( 'NONE',  ( -22.31099767395441091, -3.395517675085600651, -1.667781795950537216 ) ) ;
#13382 = ORIENTED_EDGE ( 'NONE', *, *, #21731, .T. ) ;
#13383 = CARTESIAN_POINT ( 'NONE',  ( 2.639814597422734721, 5.782006333156068045, 5.186391178752146836 ) ) ;
#13384 = DIRECTION ( 'NONE',  ( 0.000000000000000000, 0.9937233664769765662, -0.1118654143051580896 ) ) ;
#13385 = CARTESIAN_POINT ( 'NONE',  ( -35.00000000000000000, 4.018060380616562455, -11.50504120060938718 ) ) ;
#13386 = CARTESIAN_POINT ( 'NONE',  ( 19.21199004881496109, 2.638489798294652022, 11.74470497263192748 ) ) ;
#13387 = ORIENTED_EDGE ( 'NONE', *, *, #45974, .T. ) ;
#13388 =( BOUNDED_SURFACE ( )  B_SPLINE_SURFACE ( 3, 1, ( 
 ( #35802, #10223 ),
 ( #51139, #10887 ),
 ( #40824, #45155 ),
 ( #61103, #5251 ) ),
 .UNSPECIFIED., .F., .F., .F. ) 
 B_SPLINE_SURFACE_WITH_KNOTS ( ( 4, 4 ),
 ( 2, 2 ),
 ( 0.000000000000000000, 1.000000000000000000 ),
 ( 0.000000000000000000, 1.000000000000000000 ),
 .UNSPECIFIED. ) 
 GEOMETRIC_REPRESENTATION_ITEM ( )  RATIONAL_B_SPLINE_SURFACE ( (
 ( 1.000000000000000000, 1.000000000000000000),
 ( 0.6933888150995267674, 0.9895912004443193632),
 ( 0.6933888150995267674, 0.9895912004443193632),
 ( 1.000000000000000000, 1.000000000000000000) ) ) 
 REPRESENTATION_ITEM ( '' )  SURFACE ( )  );
#13389 = CARTESIAN_POINT ( 'NONE',  ( -35.00000000000000000, 6.547236723514155976, -9.752226076388824438 ) ) ;
#13390 = CARTESIAN_POINT ( 'NONE',  ( 12.19204271345157586, -29.31683997938378639, 5.830637565203388384 ) ) ;
#13391 = CARTESIAN_POINT ( 'NONE',  ( -29.60271627082680368, -3.677907232733512721, 11.42254165076253614 ) ) ;
#13393 = EDGE_LOOP ( 'NONE', ( #55361, #31866, #6143, #19865 ) ) ;
#13392 = DIRECTION ( 'NONE',  ( 0.000000000000000000, -0.8369827122275401710, -0.5472293298355184188 ) ) ;
#13394 = DIRECTION ( 'NONE',  ( -1.000000000000000000, -0.000000000000000000, -0.000000000000000000 ) ) ;
#13395 = VERTEX_POINT ( 'NONE', #41530 ) ;
#13397 = EDGE_CURVE ( 'NONE', #395, #37649, #30262, .T. ) ;
#13396 = DIRECTION ( 'NONE',  ( 0.000000000000000000, -0.01356324068817998940, 0.9999080150203990547 ) ) ;
#13398 = ORIENTED_EDGE ( 'NONE', *, *, #50647, .F. ) ;
#13399 = DIRECTION ( 'NONE',  ( 0.000000000000000000, -0.01356324068818000328, 0.9999080150203990547 ) ) ;
#13400 = CARTESIAN_POINT ( 'NONE',  ( -22.30625920655495165, 1.672644928563083333, -3.403091720605004866 ) ) ;
#13401 = CARTESIAN_POINT ( 'NONE',  ( 5.530133899448235191, 0.01293763278443438476, 0.009387834778845891709 ) ) ;
#13402 = DIRECTION ( 'NONE',  ( 0.000000000000000000, -0.3554799084908833451, -0.9346839223284592046 ) ) ;
#13403 = EDGE_CURVE ( 'NONE', #29231, #12206, #37325, .T. ) ;
#13404 = LINE ( 'NONE', #8758, #52695 ) ;
#13405 = FACE_OUTER_BOUND ( 'NONE', #33923, .T. ) ;
#13406 = DIRECTION ( 'NONE',  ( 0.000000000000000000, -0.01356324068817998940, 0.9999080150203990547 ) ) ;
#13407 = VERTEX_POINT ( 'NONE', #65485 ) ;
#13408 = CARTESIAN_POINT ( 'NONE',  ( 35.00000000000000000, 1.908798535168558352, 12.60630747491660664 ) ) ;
#13409 = EDGE_LOOP ( 'NONE', ( #30353, #61085, #23961, #55910 ) ) ;
#13410 = ORIENTED_EDGE ( 'NONE', *, *, #28389, .T. ) ;
#13411 = DIRECTION ( 'NONE',  ( -1.000000000000000000, 0.000000000000000000, 0.000000000000000000 ) ) ;
#13412 = CARTESIAN_POINT ( 'NONE',  ( -22.31099767395441091, 3.395517675085607756, 1.667781795950494583 ) ) ;
#13413 = CARTESIAN_POINT ( 'NONE',  ( 37.00000000000000711, -12.38385022362083987, -3.033604067594535714 ) ) ;
#13414 = CARTESIAN_POINT ( 'NONE',  ( 2.000000000000001776, -2.562706407243573459, -6.312399813420393357 ) ) ;
#13415 = CARTESIAN_POINT ( 'NONE',  ( 0.9232058338315058954, -10.98407661738924546, -5.905985151448264858 ) ) ;
#13416 = DIRECTION ( 'NONE',  ( -1.000000000000000000, 0.000000000000000000, -0.000000000000000000 ) ) ;
#13417 = EDGE_CURVE ( 'NONE', #35243, #29318, #46309, .T. ) ;
#13418 = CYLINDRICAL_SURFACE ( 'NONE', #52528, 13.50000000000000178 ) ;
#13419 = VECTOR ( 'NONE', #43961, 1000.000000000000000 ) ;
#13420 = EDGE_CURVE ( 'NONE', #54941, #35302, #10294, .T. ) ;
#13421 = EDGE_LOOP ( 'NONE', ( #36036, #8995, #2772, #62579 ) ) ;
#13422 = DIRECTION ( 'NONE',  ( -1.000000000000000000, 0.000000000000000000, -0.000000000000000000 ) ) ;
#13423 = CARTESIAN_POINT ( 'NONE',  ( 2.255723233588952326, -5.766109278028596741, -5.010912740808180388 ) ) ;
#13424 = ADVANCED_FACE ( 'NONE', ( #342 ), #56176, .F. ) ;
#13425 = CARTESIAN_POINT ( 'NONE',  ( -35.00000000000000000, 0.000000000000000000, 0.000000000000000000 ) ) ;
#13426 = CARTESIAN_POINT ( 'NONE',  ( 2.242418902651940549, -4.830735119000173938, 5.912154560271213555 ) ) ;
#13427 = CARTESIAN_POINT ( 'NONE',  ( 37.00000000000000711, -12.08151691381187298, 4.074242145636131518 ) ) ;
#13428 = EDGE_CURVE ( 'NONE', #41836, #17260, #5669, .T. ) ;
#13429 = CARTESIAN_POINT ( 'NONE',  ( 2.241537034860906719, -2.606707005150495249, -7.175668896091119464 ) ) ;
#13430 = EDGE_CURVE ( 'NONE', #22711, #21005, #2327, .T. ) ;
#13431 = CARTESIAN_POINT ( 'NONE',  ( -8.737571515103036646, -2.833124800313057801, 13.20164519060687347 ) ) ;
#13432 = VERTEX_POINT ( 'NONE', #55535 ) ;
#13433 = DIRECTION ( 'NONE',  ( -1.000000000000000000, 0.000000000000000000, 0.000000000000000000 ) ) ;
#13434 = CARTESIAN_POINT ( 'NONE',  ( 2.000000000000001776, 4.570217215903443986, -5.218059682435596258 ) ) ;
#13435 = CARTESIAN_POINT ( 'NONE',  ( -35.04643116707788408, 0.007621814750502498015, 0.009511118309123156589 ) ) ;
#13436 = EDGE_CURVE ( 'NONE', #61252, #10609, #16057, .T. ) ;
#13437 = DIRECTION ( 'NONE',  ( -1.000000000000000000, -0.000000000000000000, 0.000000000000000000 ) ) ;
#13438 = CARTESIAN_POINT ( 'NONE',  ( 1.000000000000000888, 6.253963800348250501, 4.139799123621038746 ) ) ;
#13439 = ORIENTED_EDGE ( 'NONE', *, *, #18793, .T. ) ;
#13440 = CARTESIAN_POINT ( 'NONE',  ( 5.516018279890452902, 0.006286471671802441874, 0.002527316374434314221 ) ) ;
#13441 = CARTESIAN_POINT ( 'NONE',  ( -9.806951085677328095, -9.949905073136244837, -6.721768133878152085 ) ) ;
#13442 = CARTESIAN_POINT ( 'NONE',  ( -18.01809167125681910, 3.277815084079592989, -11.54557337376306769 ) ) ;
#13443 = ORIENTED_EDGE ( 'NONE', *, *, #15551, .T. ) ;
#13444 = CARTESIAN_POINT ( 'NONE',  ( 24.82652845881425208, 10.42385221765396608, -8.578654028722157321 ) ) ;
#13445 = LINE ( 'NONE', #28746, #19212 ) ;
#13446 = ORIENTED_EDGE ( 'NONE', *, *, #41891, .T. ) ;
#13447 = ORIENTED_EDGE ( 'NONE', *, *, #62441, .F. ) ;
#13448 = AXIS2_PLACEMENT_3D ( 'NONE', #53247, #58577, #47286 ) ;
#13449 = CARTESIAN_POINT ( 'NONE',  ( 2.080613030138687147, 9.502643082083353612E-16, 7.580821595991582562 ) ) ;
#13450 = B_SPLINE_CURVE_WITH_KNOTS ( 'NONE', 3,
 ( #4750, #55918, #10349, #60568, #65542, #404, #59940 ),
 .UNSPECIFIED., .F., .F.,
 ( 4, 3, 4 ),
 ( 6.950728994019374331E-15, 0.002398160485434793366, 0.005002426799384073614 ),
 .UNSPECIFIED. ) ;
#13451 = VECTOR ( 'NONE', #14361, 1000.000000000000114 ) ;
#13452 = ORIENTED_EDGE ( 'NONE', *, *, #16777, .T. ) ;
#13453 = CARTESIAN_POINT ( 'NONE',  ( 1.020182472822747766, -12.22263240120535954, -2.608319446515142470 ) ) ;
#13454 = DIRECTION ( 'NONE',  ( -1.000000000000000000, 0.000000000000000000, 0.000000000000000000 ) ) ;
#13455 = DIRECTION ( 'NONE',  ( 0.000000000000000000, -0.8169148498130213154, 0.5767582926625057782 ) ) ;
#13456 = CARTESIAN_POINT ( 'NONE',  ( 5.516018279890452902, 0.006707902355169300182, -0.0009545156522407284051 ) ) ;
#13458 = VERTEX_POINT ( 'NONE', #10963 ) ;
#13457 = DIRECTION ( 'NONE',  ( 0.000000000000000000, -0.01356324068817991828, 0.9999080150203990547 ) ) ;
#13459 = FACE_OUTER_BOUND ( 'NONE', #27049, .T. ) ;
#13460 = ORIENTED_EDGE ( 'NONE', *, *, #14911, .F. ) ;
#13461 = DIRECTION ( 'NONE',  ( 1.000000000000000000, 0.000000000000000000, -0.000000000000000000 ) ) ;
#13462 = ORIENTED_EDGE ( 'NONE', *, *, #10269, .F. ) ;
#13463 = B_SPLINE_CURVE_WITH_KNOTS ( 'NONE', 3,
 ( #43197, #43520, #63801, #18284, #31902, #52227, #1686, #21952, #16955, #62490, #37221, #27259, #57537, #22262, #42526, #62827, #37574, #54830, #59173 ),
 .UNSPECIFIED., .F., .F.,
 ( 4, 3, 3, 3, 3, 3, 4 ),
 ( 4.336808689942017736E-19, 2.831840207499592302E-05, 4.217266859840494790E-05, 5.602024318395987625E-05, 6.290810167969022241E-05, 9.120440630944991460E-05, 0.0001153103026479746938 ),
 .UNSPECIFIED. ) ;
#13464 = EDGE_LOOP ( 'NONE', ( #63820, #20664, #36368, #65197 ) ) ;
#13465 = CARTESIAN_POINT ( 'NONE',  ( -36.00000000000000711, -12.74068829017553561, -0.4871980014162809458 ) ) ;
#13466 = CARTESIAN_POINT ( 'NONE',  ( -9.594501343355146261, -32.11802400029680626, 13.11109426626678953 ) ) ;
#13467 = LINE ( 'NONE', #18506, #56634 ) ;
#13468 = EDGE_CURVE ( 'NONE', #51219, #21179, #28730, .T. ) ;
#13469 = CARTESIAN_POINT ( 'NONE',  ( 2.000000000000001776, -2.480520636974233639, 6.345145617221206180 ) ) ;
#13470 = CARTESIAN_POINT ( 'NONE',  ( -37.00000000000000711, 0.000000000000000000, 0.000000000000000000 ) ) ;
#13471 = CARTESIAN_POINT ( 'NONE',  ( -27.08423805673873375, 0.6554626340706067866, -2.195702713475291112 ) ) ;
#13472 = ORIENTED_EDGE ( 'NONE', *, *, #60376, .T. ) ;
#13473 = CARTESIAN_POINT ( 'NONE',  ( 2.241352910868909643, -5.794346703933810794, -4.970878533273820565 ) ) ;
#13474 = DIRECTION ( 'NONE',  ( 1.000000000000000000, 0.000000000000000000, 0.000000000000000000 ) ) ;
#13475 = CARTESIAN_POINT ( 'NONE',  ( 37.00000000000000711, 4.705694406421931860E-17, -3.469127814946512892E-15 ) ) ;
#13476 = ORIENTED_EDGE ( 'NONE', *, *, #40675, .F. ) ;
#13477 = DIRECTION ( 'NONE',  ( 0.000000000000000000, -0.01356324068817999114, 0.9999080150203989437 ) ) ;
#13478 = ORIENTED_EDGE ( 'NONE', *, *, #30403, .T. ) ;
#13479 = CARTESIAN_POINT ( 'NONE',  ( 2.276905613633651182, -7.501802783089482674, 1.479235344773136784 ) ) ;
#13480 = CARTESIAN_POINT ( 'NONE',  ( 0.2833330754217370795, -10.50818856955514313, -6.300330022379329264 ) ) ;
#13481 = CARTESIAN_POINT ( 'NONE',  ( 0.3665391374699472626, 12.27992639892678284, -0.2638605131387596336 ) ) ;
#13482 = LINE ( 'NONE', #64667, #60259 ) ;
#13483 = CARTESIAN_POINT ( 'NONE',  ( -36.00000000000000711, -9.913596905230058098, -8.017674001891890612 ) ) ;
#13484 = CARTESIAN_POINT ( 'NONE',  ( -29.46184535117399150, 0.7194508147655768182, 13.48249488223129688 ) ) ;
#13485 = EDGE_CURVE ( 'NONE', #62894, #58300, #59653, .T. ) ;
#13486 = CARTESIAN_POINT ( 'NONE',  ( 2.241352910868908754, 3.889181972941541776, -6.569501556381402096 ) ) ;
#13487 = EDGE_LOOP ( 'NONE', ( #55194, #39584, #58210, #49716 ) ) ;
#13488 = EDGE_CURVE ( 'NONE', #20597, #239, #27091, .T. ) ;
#13489 = ORIENTED_EDGE ( 'NONE', *, *, #22545, .F. ) ;
#13490 = ADVANCED_FACE ( 'NONE', ( #1657, #21926 ), #42498, .F. ) ;
#13491 = CARTESIAN_POINT ( 'NONE',  ( 12.47628546223243617, 0.000000000000000000, 25.00000000000000000 ) ) ;
#13492 = CARTESIAN_POINT ( 'NONE',  ( 3.152665057735760445, 4.725420687649616092, -6.378477742801607953 ) ) ;
#13493 = VECTOR ( 'NONE', #8032, 1000.000000000000000 ) ;
#13494 = DIRECTION ( 'NONE',  ( -1.000000000000000000, 0.000000000000000000, 0.000000000000000000 ) ) ;
#13495 = B_SPLINE_CURVE_WITH_KNOTS ( 'NONE', 3,
 ( #55339, #10116, #64327, #44688 ),
 .UNSPECIFIED., .F., .F.,
 ( 4, 4 ),
 ( 0.007620068080905808769, 0.01192914805994312565 ),
 .UNSPECIFIED. ) ;
#13496 = DIRECTION ( 'NONE',  ( 1.000000000000000000, -0.000000000000000000, 0.000000000000000000 ) ) ;
#13497 = CARTESIAN_POINT ( 'NONE',  ( -35.00000000000000000, 0.000000000000000000, 0.000000000000000000 ) ) ;
#13498 = AXIS2_PLACEMENT_3D ( 'NONE', #33911, #30476, #54213 ) ;
#13499 = ADVANCED_FACE ( 'NONE', ( #42847 ), #63135, .T. ) ;
#13500 = CARTESIAN_POINT ( 'NONE',  ( 7.273419175973108608, -6.815651482458461530, -11.65514903918486311 ) ) ;
#13501 = EDGE_CURVE ( 'NONE', #17594, #35944, #4962, .T. ) ;
#13502 = DIRECTION ( 'NONE',  ( -1.000000000000000000, 0.000000000000000000, 0.000000000000000000 ) ) ;
#13503 = CARTESIAN_POINT ( 'NONE',  ( -35.00000000000000000, 9.217970097227725645, 7.971186206369506699 ) ) ;
#13504 = DIRECTION ( 'NONE',  ( 1.000000000000000000, -0.000000000000000000, 0.000000000000000000 ) ) ;
#13505 = EDGE_CURVE ( 'NONE', #54151, #24707, #58585, .T. ) ;
#13506 = EDGE_LOOP ( 'NONE', ( #42003, #47372, #22505, #2173 ) ) ;
#13507 = DIRECTION ( 'NONE',  ( -1.000000000000000000, -0.000000000000000000, 0.000000000000000000 ) ) ;
#13508 = CARTESIAN_POINT ( 'NONE',  ( 2.000000000000001776, -5.107597897712309098, -4.693343793638478978 ) ) ;
#13509 = DIRECTION ( 'NONE',  ( 1.000000000000000000, 0.000000000000000000, 0.000000000000000000 ) ) ;
#13510 = EDGE_CURVE ( 'NONE', #51925, #65451, #41552, .T. ) ;
#13511 = EDGE_CURVE ( 'NONE', #34813, #31213, #61723, .T. ) ;
#13512 = DIRECTION ( 'NONE',  ( 0.000000000000000000, 0.4198891015602590482, 0.9075754196709594490 ) ) ;
#13513 = CARTESIAN_POINT ( 'NONE',  ( 2.255723233588950549, -5.936060085173580525, 4.808373255828864323 ) ) ;
#13514 = ORIENTED_EDGE ( 'NONE', *, *, #49573, .T. ) ;
#13515 = DIRECTION ( 'NONE',  ( 0.000000000000000000, 0.01356324068817992175, -0.9999080150203990547 ) ) ;
#13516 = CARTESIAN_POINT ( 'NONE',  ( 5.536195898058073439, -0.007896796515810905470, 0.003145317580921124911 ) ) ;
#13518 = ADVANCED_FACE ( 'NONE', ( #48514 ), #6416, .F. ) ;
#13517 = CARTESIAN_POINT ( 'NONE',  ( -1.704253825401055966, -31.09323697348121129, -14.38225808330797584 ) ) ;
#13519 = EDGE_LOOP ( 'NONE', ( #17356, #2872, #17326, #23361 ) ) ;
#13520 = CARTESIAN_POINT ( 'NONE',  ( 0.4626703367445764159, -8.128802338754399059, 9.247028139127525748 ) ) ;
#13521 = B_SPLINE_CURVE_WITH_KNOTS ( 'NONE', 3,
 ( #44478, #59796, #18909, #65412, #39173, #54492, #19230, #29214, #59464, #38529, #59158, #45154, #23913 ),
 .UNSPECIFIED., .F., .F.,
 ( 4, 3, 3, 3, 4 ),
 ( 3.127317220692750759E-18, 6.607593386745536459E-05, 0.0001321518677373519188, 0.0001982171734706205887, 0.0002642860854759490966 ),
 .UNSPECIFIED. ) ;
#13522 = LINE ( 'NONE', #48477, #8417 ) ;
#13523 = DIRECTION ( 'NONE',  ( -1.000000000000000000, 0.000000000000000000, 0.000000000000000000 ) ) ;
#13524 = B_SPLINE_CURVE_WITH_KNOTS ( 'NONE', 3,
 ( #13799, #48757, #13176, #53748, #54733, #49735, #3554, #63366, #18519, #17833, #28455, #39411, #13480, #59377, #59072, #48440, #64665, #8183, #2889 ),
 .UNSPECIFIED., .F., .F.,
 ( 4, 3, 3, 3, 3, 3, 4 ),
 ( 9.407601696150301793E-18, 4.457896483015181383E-05, 6.639290541542492330E-05, 8.820687556479444300E-05, 0.0001100173248778943082, 0.0001545671401658154634, 0.0001830328308068594170 ),
 .UNSPECIFIED. ) ;
#13525 = DIRECTION ( 'NONE',  ( 0.000000000000000000, 0.04924826701374583615, 0.9987865678893277366 ) ) ;
#13526 = AXIS2_PLACEMENT_3D ( 'NONE', #24045, #23728, #43996 ) ;
#13527 = CARTESIAN_POINT ( 'NONE',  ( 37.00000000000000711, -5.015831474386232891, 10.62137734850272786 ) ) ;
#13528 = ORIENTED_EDGE ( 'NONE', *, *, #59174, .T. ) ;
#13529 = CARTESIAN_POINT ( 'NONE',  ( -22.46509356695199955, 0.8809186187926546507, -4.154553862421312083 ) ) ;
#13530 = CARTESIAN_POINT ( 'NONE',  ( -35.00000000000000000, 7.971186206369601734, -9.217970097227642157 ) ) ;
#13531 = AXIS2_PLACEMENT_3D ( 'NONE', #27903, #18907, #17611 ) ;
#13532 = CARTESIAN_POINT ( 'NONE',  ( 0.3057689695767493721, -9.538231270095055336, -7.702054583838566337 ) ) ;
#13533 = CARTESIAN_POINT ( 'NONE',  ( -36.00000000000000711, 1.738225594539995589, 12.63095688309029718 ) ) ;
#13534 = DIRECTION ( 'NONE',  ( -1.000000000000000000, 0.000000000000000000, 0.000000000000000000 ) ) ;
#13535 = CARTESIAN_POINT ( 'NONE',  ( 2.241451721903216399, -3.869794645251166010, 6.581017239736953073 ) ) ;
#13536 = DIRECTION ( 'NONE',  ( 1.000000000000000000, 0.000000000000000000, 0.000000000000000000 ) ) ;
#13537 = CARTESIAN_POINT ( 'NONE',  ( 5.516018279890452902, -0.006707902355169293243, 0.0009545156522407741585 ) ) ;
#13538 = VERTEX_POINT ( 'NONE', #49501 ) ;
#13539 = ORIENTED_EDGE ( 'NONE', *, *, #46824, .T. ) ;
#13540 = CARTESIAN_POINT ( 'NONE',  ( 2.034671305879985237, -8.030508024279507495, 8.476347594673388386 ) ) ;
#13541 = EDGE_LOOP ( 'NONE', ( #40958, #44770, #9537, #38428 ) ) ;
#13542 = VECTOR ( 'NONE', #55784, 1000.000000000000000 ) ;
#13543 =( NAMED_UNIT ( * ) SI_UNIT ( $, .STERADIAN. ) SOLID_ANGLE_UNIT ( ) );
#13544 = CARTESIAN_POINT ( 'NONE',  ( -35.00000000000000000, -11.56998259273174945, -3.827046518385204266 ) ) ;
#13545 = LINE ( 'NONE', #33524, #50231 ) ;
#13546 = EDGE_CURVE ( 'NONE', #64767, #56931, #33052, .T. ) ;
#13547 = CIRCLE ( 'NONE', #49557, 12.75000000000000178 ) ;
#13548 = CARTESIAN_POINT ( 'NONE',  ( -22.27704833740210333, -1.521679877253162116, 3.351945466913909488 ) ) ;
#13549 = ORIENTED_EDGE ( 'NONE', *, *, #6461, .T. ) ;
#13550 = CARTESIAN_POINT ( 'NONE',  ( 35.00000000000000000, 3.645068577060024850, -11.16627499335656815 ) ) ;
#13551 = CARTESIAN_POINT ( 'NONE',  ( 2.241352910868908754, 6.569501556381497132, -3.889181972941381460 ) ) ;
#13552 = FACE_OUTER_BOUND ( 'NONE', #26376, .T. ) ;
#13553 = ORIENTED_EDGE ( 'NONE', *, *, #27265, .F. ) ;
#13554 = VERTEX_POINT ( 'NONE', #18598 ) ;
#13555 = CARTESIAN_POINT ( 'NONE',  ( -35.00000000000000000, -12.42372387097880271, -2.865935305911757602 ) ) ;
#13556 = DIRECTION ( 'NONE',  ( -1.000000000000000000, 0.000000000000000000, 0.000000000000000000 ) ) ;
#13557 = ADVANCED_FACE ( 'NONE', ( #64428 ), #65085, .T. ) ;
#13558 = VERTEX_POINT ( 'NONE', #43490 ) ;
#13559 = ORIENTED_EDGE ( 'NONE', *, *, #37716, .T. ) ;
#13560 = CARTESIAN_POINT ( 'NONE',  ( -27.09125059358712306, -1.607567221344180952, 1.662156772100931157 ) ) ;
#13561 = CARTESIAN_POINT ( 'NONE',  ( 0.3654063281920738593, 10.50027211615256562, -6.366443614636578374 ) ) ;
#13562 = CARTESIAN_POINT ( 'NONE',  ( -37.00000000000000711, 6.036400161834567513, 10.07641281632180075 ) ) ;
#13563 = CYLINDRICAL_SURFACE ( 'NONE', #12574, 5.000000000000000888 ) ;
#13564 = EDGE_CURVE ( 'NONE', #63687, #30290, #64746, .T. ) ;
#13565 = CARTESIAN_POINT ( 'NONE',  ( 0.3675815128205894289, -10.76447900494936327, -5.910255304480558358 ) ) ;
#13566 = ORIENTED_EDGE ( 'NONE', *, *, #58206, .F. ) ;
#13567 = CARTESIAN_POINT ( 'NONE',  ( 2.253265082352432724, -1.452519439326509287, 7.498995607278134301 ) ) ;
#13568 = CARTESIAN_POINT ( 'NONE',  ( -17.31370294542102428, 7.098634700851768287, 9.677313122349437080 ) ) ;
#13569 = CARTESIAN_POINT ( 'NONE',  ( -20.73706235180480562, -13.15925562679262306, -3.065506255066365426 ) ) ;
#13570 = EDGE_CURVE ( 'NONE', #57717, #60184, #43291, .T. ) ;
#13571 = CARTESIAN_POINT ( 'NONE',  ( -35.04709527796842394, 0.001003525937978352878, -0.01232256164996822778 ) ) ;
#13572 = CARTESIAN_POINT ( 'NONE',  ( 2.305787727787084407, 1.164987321564833422, -7.566723232958059597 ) ) ;
#13573 = CYLINDRICAL_SURFACE ( 'NONE', #31826, 12.75000000000000178 ) ;
#13574 = DIRECTION ( 'NONE',  ( 0.000000000000000000, 0.000000000000000000, 1.000000000000000000 ) ) ;
#13575 = CARTESIAN_POINT ( 'NONE',  ( 0.2739690278137263402, -11.57167385487630362, -4.016979056590882280 ) ) ;
#13576 = CARTESIAN_POINT ( 'NONE',  ( -17.29244623348158783, 2.525873743887551814, 13.26159725786978960 ) ) ;
#13577 = CIRCLE ( 'NONE', #27396, 12.75000000000000178 ) ;
#13578 = VERTEX_POINT ( 'NONE', #44805 ) ;
#13579 = CARTESIAN_POINT ( 'NONE',  ( -35.00000000000000000, -6.547236723514086698, 9.752226076388870624 ) ) ;
#13580 = AXIS2_PLACEMENT_3D ( 'NONE', #63062, #37793, #22843 ) ;
#13581 =( BOUNDED_SURFACE ( )  B_SPLINE_SURFACE ( 3, 1, ( 
 ( #64274, #4769 ),
 ( #59958, #34004 ),
 ( #34339, #28694 ),
 ( #64578, #54946 ) ),
 .UNSPECIFIED., .F., .F., .F. ) 
 B_SPLINE_SURFACE_WITH_KNOTS ( ( 4, 4 ),
 ( 2, 2 ),
 ( 0.000000000000000000, 1.000000000000000000 ),
 ( 0.000000000000000000, 1.000000000000000000 ),
 .UNSPECIFIED. ) 
 GEOMETRIC_REPRESENTATION_ITEM ( )  RATIONAL_B_SPLINE_SURFACE ( (
 ( 1.000000000000000000, 1.000000000000000000),
 ( 0.6933888150995267674, 0.9895912004443193632),
 ( 0.6933888150995267674, 0.9895912004443193632),
 ( 1.000000000000000000, 1.000000000000000000) ) ) 
 REPRESENTATION_ITEM ( '' )  SURFACE ( )  );
#13582 = ORIENTED_EDGE ( 'NONE', *, *, #51358, .T. ) ;
#13583 = CARTESIAN_POINT ( 'NONE',  ( 37.00000000000000711, 2.865935305911624376, -12.42372387097883646 ) ) ;
#13584 = DIRECTION ( 'NONE',  ( -1.000000000000000000, 0.000000000000000000, 0.000000000000000000 ) ) ;
#13585 = CARTESIAN_POINT ( 'NONE',  ( 1.719304012338199517, 0.000000000000000000, 0.000000000000000000 ) ) ;
#13586 = AXIS2_PLACEMENT_3D ( 'NONE', #28380, #49355, #55283 ) ;
#13587 = CARTESIAN_POINT ( 'NONE',  ( 0.000000000000000000, -6.441884263200823746, -2.217201541069834914 ) ) ;
#13588 = DIRECTION ( 'NONE',  ( 1.000000000000000000, 0.000000000000000000, -0.000000000000000000 ) ) ;
#13589 = ORIENTED_EDGE ( 'NONE', *, *, #19448, .T. ) ;
#13590 = CARTESIAN_POINT ( 'NONE',  ( 35.00000000000000000, 2.497432891016841960, -11.47758908105695319 ) ) ;
#13591 = CARTESIAN_POINT ( 'NONE',  ( -35.04643116707788408, -0.009511118309140503824, 0.007621814750495559121 ) ) ;
#13592 = CARTESIAN_POINT ( 'NONE',  ( 9.376659010705683528, 2.637162270932692731, 11.70861080908859364 ) ) ;
#13593 = VECTOR ( 'NONE', #60949, 1000.000000000000000 ) ;
#13594 = CARTESIAN_POINT ( 'NONE',  ( -22.30861784526116054, 2.737516124790411176, 2.600591904828372325 ) ) ;
#13595 = B_SPLINE_CURVE_WITH_KNOTS ( 'NONE', 3,
 ( #12598, #2678, #33872, #32878, #7635, #63796 ),
 .UNSPECIFIED., .F., .F.,
 ( 4, 2, 4 ),
 ( 0.01068930494538425542, 0.01246789317672156866, 0.01424648140805888016 ),
 .UNSPECIFIED. ) ;
#13596 = ADVANCED_FACE ( 'NONE', ( #34504 ), #18252, .T. ) ;
#13597 = EDGE_CURVE ( 'NONE', #16004, #16830, #21385, .T. ) ;
#13598 = DIRECTION ( 'NONE',  ( 0.000000000000000000, 0.000000000000000000, -1.000000000000000000 ) ) ;
#13599 = ORIENTED_EDGE ( 'NONE', *, *, #54448, .T. ) ;
#13601 = EDGE_CURVE ( 'NONE', #9962, #31780, #20391, .T. ) ;
#13600 = CARTESIAN_POINT ( 'NONE',  ( 5.514624014163232779, 0.002789935220458047982, -0.003060352188290787166 ) ) ;
#13602 = ORIENTED_EDGE ( 'NONE', *, *, #49116, .F. ) ;
#13603 = DIRECTION ( 'NONE',  ( 0.000000000000000000, -0.01356324068817999114, 0.9999080150203989437 ) ) ;
#13604 = FACE_OUTER_BOUND ( 'NONE', #10207, .T. ) ;
#13605 = CARTESIAN_POINT ( 'NONE',  ( -37.25000000000000711, -1.694065894508600678E-18, 0.000000000000000000 ) ) ;
#13606 = DIRECTION ( 'NONE',  ( -1.000000000000000000, 0.000000000000000000, 0.000000000000000000 ) ) ;
#13607 = ORIENTED_EDGE ( 'NONE', *, *, #45275, .F. ) ;
#13608 = VERTEX_POINT ( 'NONE', #9224 ) ;
#13609 = CARTESIAN_POINT ( 'NONE',  ( -27.09569413923794912, 2.232620870184089057, -0.6513788562879346822 ) ) ;
#13610 = DIRECTION ( 'NONE',  ( -1.000000000000000000, 0.000000000000000000, 0.000000000000000000 ) ) ;
#13611 = CARTESIAN_POINT ( 'NONE',  ( 2.000000000000001776, 0.000000000000000000, 0.000000000000000000 ) ) ;
#13613 = CARTESIAN_POINT ( 'NONE',  ( 0.3610902822527237710, 9.234828023175207790, -8.091349661862537346 ) ) ;
#13612 = CIRCLE ( 'NONE', #3066, 12.18649999999999878 ) ;
#13614 = B_SPLINE_CURVE_WITH_KNOTS ( 'NONE', 3,
 ( #44795, #34165, #44458, #39815, #55440, #19208, #65076, #3627, #44154, #39151, #54474, #39481, #19551, #50469, #60102, #34798, #55103, #9532 ),
 .UNSPECIFIED., .F., .F.,
 ( 4, 2, 2, 2, 2, 2, 2, 2, 4 ),
 ( 0.000000000000000000, 0.001195117733165457262, 0.002390235466330913657, 0.003585353199496369835, 0.004780470932661826447, 0.005975588665827281758, 0.007170706398992739670, 0.008365824132158196716, 0.009560941865323654629 ),
 .UNSPECIFIED. ) ;
#13615 = DIRECTION ( 'NONE',  ( 0.000000000000000000, 0.000000000000000000, 1.000000000000000000 ) ) ;
#13616 = EDGE_LOOP ( 'NONE', ( #35772, #38314, #53222, #26450 ) ) ;
#13617 = ORIENTED_EDGE ( 'NONE', *, *, #33160, .F. ) ;
#13618 = ORIENTED_EDGE ( 'NONE', *, *, #56355, .T. ) ;
#13619 = FACE_OUTER_BOUND ( 'NONE', #31738, .T. ) ;
#13620 = B_SPLINE_CURVE_WITH_KNOTS ( 'NONE', 3,
 ( #36921, #52879, #36265, #57224, #11010, #26623 ),
 .UNSPECIFIED., .F., .F.,
 ( 4, 2, 4 ),
 ( 0.0002637379172192549199, 0.0009975831966643308908, 0.001731428476109406808 ),
 .UNSPECIFIED. ) ;
#13621 = DIRECTION ( 'NONE',  ( 0.000000000000000000, -0.01356324068817999114, 0.9999080150203989437 ) ) ;
#13622 = ADVANCED_FACE ( 'NONE', ( #3288 ), #4258, .T. ) ;
#13623 = ORIENTED_EDGE ( 'NONE', *, *, #52240, .T. ) ;
#13624 = DIRECTION ( 'NONE',  ( 0.000000000000000000, -0.01356324068817998940, 0.9999080150203990547 ) ) ;
#13625 = CARTESIAN_POINT ( 'NONE',  ( -22.27786964138239867, -0.3434379038477733959, -3.667590411552012597 ) ) ;
#13626 = EDGE_CURVE ( 'NONE', #41918, #52756, #38517, .T. ) ;
#13628 = VERTEX_POINT ( 'NONE', #43837 ) ;
#13627 = AXIS2_PLACEMENT_3D ( 'NONE', #42881, #52232, #47246 ) ;
#13629 = CIRCLE ( 'NONE', #10452, 12.18650000000000411 ) ;
#13630 = LINE ( 'NONE', #34568, #38621 ) ;
#13631 = CARTESIAN_POINT ( 'NONE',  ( 0.000000000000000000, -3.979254915827401540, 5.681598592373737766 ) ) ;
#13632 = DIRECTION ( 'NONE',  ( -1.000000000000000000, 0.000000000000000000, 0.000000000000000000 ) ) ;
#13633 = ORIENTED_EDGE ( 'NONE', *, *, #16749, .T. ) ;
#13634 = ORIENTED_EDGE ( 'NONE', *, *, #25589, .T. ) ;
#13635 = CARTESIAN_POINT ( 'NONE',  ( 2.941278708680199916, -0.9331242451665402449, 6.068329152486373168 ) ) ;
#13636 = VERTEX_POINT ( 'NONE', #64118 ) ;
#13637 = CARTESIAN_POINT ( 'NONE',  ( 0.000000000000000000, -6.253963800348261159, 4.139799123620986343 ) ) ;
#13638 = ORIENTED_EDGE ( 'NONE', *, *, #17962, .F. ) ;
#13639 = ADVANCED_FACE ( 'NONE', ( #25506 ), #27189, .F. ) ;
#13640 = VERTEX_POINT ( 'NONE', #56427 ) ;
#13641 = VECTOR ( 'NONE', #56440, 1000.000000000000000 ) ;
#13642 = CARTESIAN_POINT ( 'NONE',  ( 0.2651627923886317739, -4.271101819784433040, 11.47719387551885362 ) ) ;
#13643 = FACE_OUTER_BOUND ( 'NONE', #6056, .T. ) ;
#13644 = CARTESIAN_POINT ( 'NONE',  ( 2.941278708680199916, 5.248410529370224786, 3.185832147968465478 ) ) ;
#13645 = CARTESIAN_POINT ( 'NONE',  ( -22.28694879868232803, 3.597828382597545449, 0.9088670759107777553 ) ) ;
#13646 = CARTESIAN_POINT ( 'NONE',  ( 0.2648978790185593790, -6.237101853238620208, 10.53870023327861283 ) ) ;
#13647 = DIRECTION ( 'NONE',  ( 1.000000000000000000, 0.000000000000000000, 0.000000000000000000 ) ) ;
#13648 = ORIENTED_EDGE ( 'NONE', *, *, #33177, .T. ) ;
#13649 = FACE_OUTER_BOUND ( 'NONE', #50783, .T. ) ;
#13650 = ORIENTED_EDGE ( 'NONE', *, *, #56308, .F. ) ;
#13651 = CARTESIAN_POINT ( 'NONE',  ( -35.00000000000000000, 0.000000000000000000, 0.000000000000000000 ) ) ;
#13652 = DIRECTION ( 'NONE',  ( -1.000000000000000000, 0.000000000000000000, 0.000000000000000000 ) ) ;
#13653 = EDGE_CURVE ( 'NONE', #65068, #64141, #65404, .T. ) ;
#13654 = ORIENTED_EDGE ( 'NONE', *, *, #34916, .F. ) ;
#13655 = CARTESIAN_POINT ( 'NONE',  ( -14.65407954714387451, 8.414523573697247016, 8.555553591160615312 ) ) ;
#13656 = DIRECTION ( 'NONE',  ( 0.000000000000000000, -0.01356324068817998940, 0.9999080150203990547 ) ) ;
#13657 = DIRECTION ( 'NONE',  ( -1.000000000000000000, 0.000000000000000000, 0.000000000000000000 ) ) ;
#13658 = EDGE_CURVE ( 'NONE', #50699, #60788, #15007, .T. ) ;
#13659 = VERTEX_POINT ( 'NONE', #55448 ) ;
#13660 = VECTOR ( 'NONE', #19247, 1000.000000000000000 ) ;
#13661 = ORIENTED_EDGE ( 'NONE', *, *, #19704, .F. ) ;
#13662 = CARTESIAN_POINT ( 'NONE',  ( 37.00000000000000711, 4.705694406421931860E-17, -3.469127814946512892E-15 ) ) ;
#13663 = CIRCLE ( 'NONE', #21108, 12.75000000000000178 ) ;
#13664 = EDGE_LOOP ( 'NONE', ( #44791, #39688, #31526, #50056 ) ) ;
#13665 = CARTESIAN_POINT ( 'NONE',  ( -25.00000000000000355, -30.00000000000000000, -24.00000000000000000 ) ) ;
#13666 = DIRECTION ( 'NONE',  ( -1.000000000000000000, 0.000000000000000000, 0.000000000000000000 ) ) ;
#13667 = CARTESIAN_POINT ( 'NONE',  ( -29.61524753723641012, 2.148738662487795992, 13.35711602759049654 ) ) ;
#13668 = DIRECTION ( 'NONE',  ( 0.000000000000000000, -0.8696919319575129315, -0.4935949184179356242 ) ) ;
#13669 = CARTESIAN_POINT ( 'NONE',  ( 1.633930747251798099, -9.253127167384873175, 8.702439996574970138 ) ) ;
#13670 = APPLICATION_CONTEXT ( 'automotive_design' ) ;
#13671 = ORIENTED_EDGE ( 'NONE', *, *, #20961, .T. ) ;
#13672 = DIRECTION ( 'NONE',  ( 0.000000000000000000, -0.01356324068817999114, 0.9999080150203989437 ) ) ;
#13673 = CARTESIAN_POINT ( 'NONE',  ( 1.549075743844778419, 1.533250336942787007, 12.58108552526728019 ) ) ;
#13674 = EDGE_CURVE ( 'NONE', #11911, #56404, #23533, .T. ) ;
#13675 = AXIS2_PLACEMENT_3D ( 'NONE', #52654, #27352, #22364 ) ;
#13676 = EDGE_CURVE ( 'NONE', #10290, #11977, #10745, .T. ) ;
#13677 = VECTOR ( 'NONE', #40256, 1000.000000000000000 ) ;
#13678 = CARTESIAN_POINT ( 'NONE',  ( 0.3109076770649069621, -12.11383728282217476, -1.896437056876588256 ) ) ;
#13679 = CARTESIAN_POINT ( 'NONE',  ( 35.00000000000000000, 12.12087942037209842, -1.262958560998807656 ) ) ;
#13681 = AXIS2_PLACEMENT_3D ( 'NONE', #56096, #11855, #56437 ) ;
#13680 = CARTESIAN_POINT ( 'NONE',  ( 35.00000000000000000, 8.839356091080166067, 8.389074212634184846 ) ) ;
#13682 = CARTESIAN_POINT ( 'NONE',  ( 1.452237505248552996, 10.06489946308212957, -7.672309600508594229 ) ) ;
#13683 = CARTESIAN_POINT ( 'NONE',  ( 37.00000000000000711, 5.710938531231874116, 11.39945968423464784 ) ) ;
#13684 = CARTESIAN_POINT ( 'NONE',  ( -37.00000000000000711, 8.766823244862097297, -7.817610399097422835 ) ) ;
#13685 = CIRCLE ( 'NONE', #39180, 12.18649999999999878 ) ;
#13686 = ORIENTED_EDGE ( 'NONE', *, *, #39630, .F. ) ;
#13687 = DIRECTION ( 'NONE',  ( 0.000000000000000000, -0.04924826701373161142, -0.9987865678893286248 ) ) ;
#13688 = VERTEX_POINT ( 'NONE', #60427 ) ;
#13689 = CARTESIAN_POINT ( 'NONE',  ( -14.29135464769095520, 7.782112657557433089, -9.134479874907182051 ) ) ;
#13690 = CARTESIAN_POINT ( 'NONE',  ( -22.27720387087364884, -3.639274226782815536, 0.5572161790459860820 ) ) ;
#13691 = CYLINDRICAL_SURFACE ( 'NONE', #48096, 12.18649999999999878 ) ;
#13692 = CARTESIAN_POINT ( 'NONE',  ( 35.00000000000000000, -12.74921544981110699, 0.1414404973753423111 ) ) ;
#13693 = ORIENTED_EDGE ( 'NONE', *, *, #5635, .F. ) ;
#13694 = VERTEX_POINT ( 'NONE', #46449 ) ;
#13695 = VERTEX_POINT ( 'NONE', #50788 ) ;
#13696 = CARTESIAN_POINT ( 'NONE',  ( 0.3675815128205894289, -7.689697408877210094, -9.574637318042043432 ) ) ;
#13697 = CIRCLE ( 'NONE', #1006, 7.499999999999988454 ) ;
#13698 = ORIENTED_EDGE ( 'NONE', *, *, #42763, .F. ) ;
#13699 = CARTESIAN_POINT ( 'NONE',  ( 2.963017218115616913, 5.778072204777641829, 5.350609950027682693 ) ) ;
#13700 = CARTESIAN_POINT ( 'NONE',  ( 37.00000000000000711, -6.102719229070595830, 10.54834585426226390 ) ) ;
#13701 = CARTESIAN_POINT ( 'NONE',  ( 0.2801149460245113687, -9.257544930777214631, 8.024198546827449263 ) ) ;
#13702 = CARTESIAN_POINT ( 'NONE',  ( 2.000000000000001776, 4.376687952327335651, 5.220963330856624118 ) ) ;
#13703 = ADVANCED_FACE ( 'NONE', ( #35792 ), #21172, .T. ) ;
#13704 = EDGE_LOOP ( 'NONE', ( #39870, #610, #56310, #65479 ) ) ;
#13705 = CARTESIAN_POINT ( 'NONE',  ( -27.27855387000350262, -10.59660315834921107, 5.631341004100471892 ) ) ;
#13706 = AXIS2_PLACEMENT_3D ( 'NONE', #42512, #6973, #1002 ) ;
#13707 = CARTESIAN_POINT ( 'NONE',  ( 14.05446433506782533, -34.40329588773735736, 8.438602785652603799 ) ) ;
#13708 = CARTESIAN_POINT ( 'NONE',  ( 2.260457164927188511, -1.462935478981556514, -7.499412009325157946 ) ) ;
#13710 = EDGE_LOOP ( 'NONE', ( #58094, #29153, #36874, #1933 ) ) ;
#13709 = CARTESIAN_POINT ( 'NONE',  ( 11.74548640120467979, -8.775604215601116920, -8.184666801472349817 ) ) ;
#13711 = ORIENTED_EDGE ( 'NONE', *, *, #9196, .F. ) ;
#13712 = CARTESIAN_POINT ( 'NONE',  ( 0.2671309869109494417, -6.263183022891106511, -10.52409658627922440 ) ) ;
#13713 = ORIENTED_EDGE ( 'NONE', *, *, #27678, .F. ) ;
#13714 = CARTESIAN_POINT ( 'NONE',  ( 1.719304012338833676, 3.626341562670448493, 12.20344780066006152 ) ) ;
#13716 = DIRECTION ( 'NONE',  ( 1.000000000000000000, -0.000000000000000000, 0.000000000000000000 ) ) ;
#13715 = CIRCLE ( 'NONE', #59389, 12.18649999999999878 ) ;
#13717 = CIRCLE ( 'NONE', #39207, 4.999999999999999112 ) ;
#13718 = CARTESIAN_POINT ( 'NONE',  ( -35.00000000000000000, 10.80631716521666874, 4.603882218679588689 ) ) ;
#13719 = CARTESIAN_POINT ( 'NONE',  ( -11.40165637462999904, -7.508992741355383416, 9.360289953322597611 ) ) ;
#13720 = ADVANCED_FACE ( 'NONE', ( #61092 ), #24870, .T. ) ;
#13721 = CARTESIAN_POINT ( 'NONE',  ( 0.2653519890518174495, -11.50765826381080359, 4.188454465438642416 ) ) ;
#13722 = CARTESIAN_POINT ( 'NONE',  ( 35.00000000000000000, 11.78745411414844035, 3.093009498343795460 ) ) ;
#13723 = CARTESIAN_POINT ( 'NONE',  ( -37.00000000000000711, -7.251710744571512102, -9.240395740215712195 ) ) ;
#13724 = VECTOR ( 'NONE', #62418, 1000.000000000000000 ) ;
#13725 = VERTEX_POINT ( 'NONE', #5238 ) ;
#13726 = CARTESIAN_POINT ( 'NONE',  ( -4.989057617119008192, -0.9162120371760335003, 13.46887357958837406 ) ) ;
#13727 = VERTEX_POINT ( 'NONE', #25182 ) ;
#13728 = EDGE_CURVE ( 'NONE', #26571, #725, #45798, .T. ) ;
#13729 = VERTEX_POINT ( 'NONE', #40132 ) ;
#13730 = FACE_OUTER_BOUND ( 'NONE', #12992, .T. ) ;
#13731 = PLANE ( 'NONE',  #30483 ) ;
#13732 = AXIS2_PLACEMENT_3D ( 'NONE', #22652, #18327, #33272 ) ;
#13733 = CARTESIAN_POINT ( 'NONE',  ( 35.00000000000000000, -11.67026961469347768, -4.564151185897032725 ) ) ;
#13734 = CARTESIAN_POINT ( 'NONE',  ( -22.29677679919927868, 2.096973157017390843, 3.097220482903997318 ) ) ;
#13735 = CYLINDRICAL_SURFACE ( 'NONE', #51823, 12.74999999999999822 ) ;
#13736 = EDGE_CURVE ( 'NONE', #24592, #19340, #25552, .T. ) ;
#13737 = CARTESIAN_POINT ( 'NONE',  ( 0.3002738374340830907, 10.72659044316170984, -5.932527270856288837 ) ) ;
#13738 = CARTESIAN_POINT ( 'NONE',  ( 0.8320506296491593234, -10.95539209551942683, -5.883188144889889948 ) ) ;
#13739 = ORIENTED_EDGE ( 'NONE', *, *, #34777, .F. ) ;
#13740 = LINE ( 'NONE', #19078, #2085 ) ;
#13741 = CARTESIAN_POINT ( 'NONE',  ( 2.241311220309555097, -5.788190037953238942, -4.978033760028431232 ) ) ;
#13742 = CARTESIAN_POINT ( 'NONE',  ( -17.55122397361593656, -9.296840455340431575, 9.807752914019381763 ) ) ;
#13743 = ORIENTED_EDGE ( 'NONE', *, *, #43880, .T. ) ;
#13744 = EDGE_CURVE ( 'NONE', #5815, #40304, #20335, .T. ) ;
#13745 = CIRCLE ( 'NONE', #53062, 2.899999999999995026 ) ;
#13746 = CIRCLE ( 'NONE', #26527, 12.75000000000000178 ) ;
#13747 = CARTESIAN_POINT ( 'NONE',  ( 2.241352910868908310, -2.689314586382304917, -7.145045428366603169 ) ) ;
#13748 = CARTESIAN_POINT ( 'NONE',  ( -10.22406655687136023, -4.688833681473150605, 12.66448649920025993 ) ) ;
#13749 = ORIENTED_EDGE ( 'NONE', *, *, #32527, .T. ) ;
#13750 = CARTESIAN_POINT ( 'NONE',  ( 0.3665391374699467075, -3.952034409876221677, -11.62960183138731196 ) ) ;
#13751 = DIRECTION ( 'NONE',  ( 0.000000000000000000, -0.9635499925192201331, -0.2675283385292311911 ) ) ;
#13752 = FACE_OUTER_BOUND ( 'NONE', #11897, .T. ) ;
#13753 = AXIS2_PLACEMENT_3D ( 'NONE', #31927, #15649, #22282 ) ;
#13754 = EDGE_CURVE ( 'NONE', #266, #54167, #28838, .T. ) ;
#13755 = CARTESIAN_POINT ( 'NONE',  ( -25.86628395826706850, 5.139808748864376220, 10.84354029019568522 ) ) ;
#13756 = CARTESIAN_POINT ( 'NONE',  ( -35.00000000000000000, -8.352657516904613999, -8.258652103341526995 ) ) ;
#13757 = AXIS2_PLACEMENT_3D ( 'NONE', #24582, #50525, #29887 ) ;
#13758 =( BOUNDED_SURFACE ( )  B_SPLINE_SURFACE ( 3, 1, ( 
 ( #18951, #48892 ),
 ( #33254, #24253 ),
 ( #23619, #38907 ),
 ( #53562, #54540 ) ),
 .UNSPECIFIED., .F., .F., .F. ) 
 B_SPLINE_SURFACE_WITH_KNOTS ( ( 4, 4 ),
 ( 2, 2 ),
 ( 0.000000000000000000, 1.000000000000000000 ),
 ( 0.000000000000000000, 1.000000000000000000 ),
 .UNSPECIFIED. ) 
 GEOMETRIC_REPRESENTATION_ITEM ( )  RATIONAL_B_SPLINE_SURFACE ( (
 ( 1.000000000000000000, 1.000000000000000000),
 ( 0.6933888150995267674, 0.9895912004443193632),
 ( 0.6933888150995267674, 0.9895912004443193632),
 ( 1.000000000000000000, 1.000000000000000000) ) ) 
 REPRESENTATION_ITEM ( '' )  SURFACE ( )  );
#13759 = ORIENTED_EDGE ( 'NONE', *, *, #52998, .F. ) ;
#13760 = CARTESIAN_POINT ( 'NONE',  ( -9.830496058488753519, -10.61724537947942260, -5.608865105245247840 ) ) ;
#13761 = CARTESIAN_POINT ( 'NONE',  ( 1.000000000000000888, -1.530946385938321219, -7.342084388195388556 ) ) ;
#13762 = ORIENTED_EDGE ( 'NONE', *, *, #48526, .F. ) ;
#13763 = DIRECTION ( 'NONE',  ( 0.000000000000000000, 0.01356324068817992175, -0.9999080150203990547 ) ) ;
#13764 = CARTESIAN_POINT ( 'NONE',  ( -37.00000000000000711, -12.71517666308948691, 0.9416912585473986574 ) ) ;
#13765 = VERTEX_POINT ( 'NONE', #27467 ) ;
#13766 = AXIS2_PLACEMENT_3D ( 'NONE', #50864, #1317, #16267 ) ;
#13767 = VERTEX_POINT ( 'NONE', #36476 ) ;
#13768 = CARTESIAN_POINT ( 'NONE',  ( 35.00000000000000000, 11.02904044024202967, -4.041347439436060007 ) ) ;
#13769 = ORIENTED_EDGE ( 'NONE', *, *, #7929, .F. ) ;
#13770 = DIRECTION ( 'NONE',  ( -1.000000000000000000, 0.000000000000000000, -0.000000000000000000 ) ) ;
#13771 = CARTESIAN_POINT ( 'NONE',  ( 0.2648978790185584908, 6.237101853238694815, -10.53870023327857197 ) ) ;
#13772 = CARTESIAN_POINT ( 'NONE',  ( 0.2833330754217364689, -6.300330022379283079, 10.50818856955516090 ) ) ;
#13773 = LINE ( 'NONE', #34065, #8576 ) ;
#13774 = EDGE_CURVE ( 'NONE', #32833, #60184, #36628, .T. ) ;
#13775 = CARTESIAN_POINT ( 'NONE',  ( 35.00000000000000000, -7.376655759824808811, 9.700295462048739381 ) ) ;
#13777 = VERTEX_POINT ( 'NONE', #57097 ) ;
#13776 = CARTESIAN_POINT ( 'NONE',  ( 0.9296196016818646379, 7.691217109781894656, 9.812579935704260237 ) ) ;
#13778 = EDGE_CURVE ( 'NONE', #8079, #57809, #8679, .T. ) ;
#13779 = CARTESIAN_POINT ( 'NONE',  ( -35.00000000000000000, 11.61976888909158490, 3.827969819614504221 ) ) ;
#13780 = ORIENTED_EDGE ( 'NONE', *, *, #56771, .F. ) ;
#13781 = DIRECTION ( 'NONE',  ( -1.000000000000000000, -1.836970198721029688E-16, -0.000000000000000000 ) ) ;
#13782 = EDGE_LOOP ( 'NONE', ( #10141, #30381, #65082, #31714 ) ) ;
#13783 = ORIENTED_EDGE ( 'NONE', *, *, #13883, .T. ) ;
#13784 = CARTESIAN_POINT ( 'NONE',  ( -25.66858381519323018, 8.266157983362676376, 10.67702105760074183 ) ) ;
#13785 = CARTESIAN_POINT ( 'NONE',  ( -4.536586326003440028, -28.39263410566477930, 13.35746355086213555 ) ) ;
#13786 = DIRECTION ( 'NONE',  ( 1.000000000000000000, 0.000000000000000000, -0.000000000000000000 ) ) ;
#13787 = AXIS2_PLACEMENT_3D ( 'NONE', #48876, #37232, #22620 ) ;
#13788 = AXIS2_PLACEMENT_3D ( 'NONE', #62395, #52460, #65016 ) ;
#13789 = EDGE_CURVE ( 'NONE', #25348, #65337, #34140, .T. ) ;
#13790 = CARTESIAN_POINT ( 'NONE',  ( 2.941278708680199916, 1.972702289976003165, 5.814102272488595347 ) ) ;
#13791 = CARTESIAN_POINT ( 'NONE',  ( 3.459614771489464946, -11.09853614738469396, -4.563167253695070258 ) ) ;
#13792 = LINE ( 'NONE', #44380, #35155 ) ;
#13793 = ORIENTED_EDGE ( 'NONE', *, *, #4514, .T. ) ;
#13794 = EDGE_LOOP ( 'NONE', ( #43085, #43749, #31786, #10449 ) ) ;
#13795 = CARTESIAN_POINT ( 'NONE',  ( 1.452237505248552996, 1.611965288198731194, 12.55261342181975870 ) ) ;
#13796 = LINE ( 'NONE', #15375, #62948 ) ;
#13797 = ORIENTED_EDGE ( 'NONE', *, *, #34242, .T. ) ;
#13798 = CARTESIAN_POINT ( 'NONE',  ( 2.241506898688419458, -1.286963596520043440, 7.525229609709739087 ) ) ;
#13799 = CARTESIAN_POINT ( 'NONE',  ( 0.3675815128205912052, -10.50067073900647330, -6.367184624550275451 ) ) ;
#13800 = DIRECTION ( 'NONE',  ( 1.000000000000000000, 0.000000000000000000, 0.000000000000000000 ) ) ;
#13802 = CIRCLE ( 'NONE', #41426, 5.000000000000001776 ) ;
#13801 = CARTESIAN_POINT ( 'NONE',  ( 35.00000000000000000, -5.273331777780263074, 10.49591321039685887 ) ) ;
#13803 = CARTESIAN_POINT ( 'NONE',  ( 37.00000000000000711, 2.497432891016841960, -11.47758908105695319 ) ) ;
#13804 = EDGE_CURVE ( 'NONE', #21959, #63611, #5512, .T. ) ;
#13805 = CARTESIAN_POINT ( 'NONE',  ( 2.251139882113959878, 3.925854078924309043, -6.551456272498855427 ) ) ;
#13806 = CIRCLE ( 'NONE', #59491, 5.000000000000000888 ) ;
#13807 = ORIENTED_EDGE ( 'NONE', *, *, #20024, .T. ) ;
#13808 = ORIENTED_EDGE ( 'NONE', *, *, #134, .T. ) ;
#13809 = DIRECTION ( 'NONE',  ( 0.000000000000000000, -0.01356324068817998940, 0.9999080150203990547 ) ) ;
#13810 = CYLINDRICAL_SURFACE ( 'NONE', #28713, 4.999999999999999112 ) ;
#13811 = CIRCLE ( 'NONE', #20234, 12.75000000000000178 ) ;
#13812 = DIRECTION ( 'NONE',  ( 0.000000000000000000, 0.000000000000000000, 1.000000000000000000 ) ) ;
#13813 = ORIENTED_EDGE ( 'NONE', *, *, #15629, .F. ) ;
#13814 = CARTESIAN_POINT ( 'NONE',  ( -28.13819771402047820, 11.82670130915983719, -6.517207649538970138 ) ) ;
#13815 = CIRCLE ( 'NONE', #12895, 4.999999999999999112 ) ;
#13816 = DIRECTION ( 'NONE',  ( 0.000000000000000000, -0.01356324068817998940, 0.9999080150203990547 ) ) ;
#13817 = DIRECTION ( 'NONE',  ( -1.000000000000000000, -1.836970198721029688E-16, 0.000000000000000000 ) ) ;
#13818 = CARTESIAN_POINT ( 'NONE',  ( -27.08954555554413801, -2.082904663687656921, -0.9924303381791110823 ) ) ;
#13819 = DIRECTION ( 'NONE',  ( 0.000000000000000000, 0.01356324068817992175, -0.9999080150203990547 ) ) ;
#13820 = ORIENTED_EDGE ( 'NONE', *, *, #8664, .F. ) ;
#13821 = DIRECTION ( 'NONE',  ( 0.000000000000000000, 0.000000000000000000, 1.000000000000000000 ) ) ;
#13822 = CARTESIAN_POINT ( 'NONE',  ( -22.29770266787582500, -2.588315884842648185, 2.703976473263648206 ) ) ;
#13823 = FACE_OUTER_BOUND ( 'NONE', #17350, .T. ) ;
#13824 = EDGE_CURVE ( 'NONE', #44305, #16743, #58080, .T. ) ;
#13825 = AXIS2_PLACEMENT_3D ( 'NONE', #13351, #53927, #60531 ) ;
#13826 = AXIS2_PLACEMENT_3D ( 'NONE', #59892, #24969, #18688 ) ;
#13827 = AXIS2_PLACEMENT_3D ( 'NONE', #45194, #35197, #55502 ) ;
#13828 = DIRECTION ( 'NONE',  ( -0.000000000000000000, -0.000000000000000000, -1.000000000000000000 ) ) ;
#13829 = CARTESIAN_POINT ( 'NONE',  ( -28.15365128295566421, -11.30992368511472890, -4.022759283342765002 ) ) ;
#13830 = EDGE_LOOP ( 'NONE', ( #25668, #42877, #16349, #17233 ) ) ;
#13831 = DIRECTION ( 'NONE',  ( 1.000000000000000000, 0.000000000000000000, -0.000000000000000000 ) ) ;
#13832 = CARTESIAN_POINT ( 'NONE',  ( 0.2655924914740778187, 2.083162675473614112, 12.06787830249865756 ) ) ;
#13833 = CARTESIAN_POINT ( 'NONE',  ( 4.699914177767785084, -28.11199977926868598, -11.88398404624164506 ) ) ;
#13834 = ORIENTED_EDGE ( 'NONE', *, *, #48962, .T. ) ;
#13835 = CARTESIAN_POINT ( 'NONE',  ( -18.06443652845103642, 4.738606707596126455, -12.64292522309443001 ) ) ;
#13836 = DIRECTION ( 'NONE',  ( 1.000000000000000000, 0.000000000000000000, 0.000000000000000000 ) ) ;
#13837 = CARTESIAN_POINT ( 'NONE',  ( -15.27729454824424948, 5.151216734910788908, 25.00000000000000000 ) ) ;
#13838 = CARTESIAN_POINT ( 'NONE',  ( -35.00000000000000000, 4.309077947445652867, 10.92721691015457708 ) ) ;
#13839 = CARTESIAN_POINT ( 'NONE',  ( -7.489022030332961322, -8.034049540753116503, -10.84914964302385521 ) ) ;
#13840 = AXIS2_PLACEMENT_3D ( 'NONE', #20758, #55685, #56999 ) ;
#13841 = EDGE_CURVE ( 'NONE', #44679, #43286, #56416, .T. ) ;
#13842 = CARTESIAN_POINT ( 'NONE',  ( 35.00000000000000000, 5.300372733891642874, -11.59605747147788435 ) ) ;
#13843 = ORIENTED_EDGE ( 'NONE', *, *, #2350, .F. ) ;
#13844 = VECTOR ( 'NONE', #26841, 1000.000000000000000 ) ;
#13845 = CARTESIAN_POINT ( 'NONE',  ( -22.39032720737625937, 0.9101257950221148807, -3.916738514147017902 ) ) ;
#13846 = CIRCLE ( 'NONE', #38303, 6.936499999999987232 ) ;
#13847 = DIRECTION ( 'NONE',  ( -1.000000000000000000, 0.000000000000000000, 0.000000000000000000 ) ) ;
#13848 = CARTESIAN_POINT ( 'NONE',  ( 37.00000000000000711, 11.66953048682399441, -3.511814412392164186 ) ) ;
#13849 = LINE ( 'NONE', #53481, #53298 ) ;
#13850 = CARTESIAN_POINT ( 'NONE',  ( 2.253265082352434945, 7.543541742286983265, -1.199885753716548598 ) ) ;
#13851 = DIRECTION ( 'NONE',  ( 1.000000000000000000, 0.000000000000000000, -0.000000000000000000 ) ) ;
#13852 = EDGE_CURVE ( 'NONE', #817, #61894, #40377, .T. ) ;
#13853 = CIRCLE ( 'NONE', #1169, 6.936499999999989008 ) ;
#13854 = CARTESIAN_POINT ( 'NONE',  ( -24.42101984568203932, 3.522366633939687741, 2.451666775035081791 ) ) ;
#13855 = ORIENTED_EDGE ( 'NONE', *, *, #54500, .T. ) ;
#13856 = EDGE_CURVE ( 'NONE', #28250, #4710, #19260, .T. ) ;
#13857 = EDGE_LOOP ( 'NONE', ( #39044, #9398 ) ) ;
#13858 =( NAMED_UNIT ( * ) SI_UNIT ( $, .STERADIAN. ) SOLID_ANGLE_UNIT ( ) );
#13859 = CIRCLE ( 'NONE', #62706, 5.000000000000000000 ) ;
#13860 = ORIENTED_EDGE ( 'NONE', *, *, #16439, .T. ) ;
#13861 = CARTESIAN_POINT ( 'NONE',  ( 37.00000000000000711, -11.47758908105696207, -2.497432891016804657 ) ) ;
#13862 = EDGE_CURVE ( 'NONE', #23300, #27429, #7574, .T. ) ;
#13863 = CYLINDRICAL_SURFACE ( 'NONE', #38358, 4.999999999999998224 ) ;
#13864 = ORIENTED_EDGE ( 'NONE', *, *, #3907, .F. ) ;
#13866 = CARTESIAN_POINT ( 'NONE',  ( -22.23402523511428086, -7.703719777548943412E-30, -3.000000000000009326 ) ) ;
#13865 = CIRCLE ( 'NONE', #18116, 6.936499999999989896 ) ;
#13868 = EDGE_CURVE ( 'NONE', #8648, #57089, #63054, .T. ) ;
#13867 = CARTESIAN_POINT ( 'NONE',  ( 2.256373768223947085, -5.011614056002601458, -5.765785888498891509 ) ) ;
#13869 = VERTEX_POINT ( 'NONE', #31792 ) ;
#13870 = ORIENTED_EDGE ( 'NONE', *, *, #53889, .T. ) ;
#13871 = DIRECTION ( 'NONE',  ( -1.000000000000000000, 0.000000000000000000, 0.000000000000000000 ) ) ;
#13872 = CIRCLE ( 'NONE', #30816, 4.999999999999999112 ) ;
#13873 = LINE ( 'NONE', #48837, #35432 ) ;
#13874 = ORIENTED_EDGE ( 'NONE', *, *, #33005, .T. ) ;
#13875 = ORIENTED_EDGE ( 'NONE', *, *, #32557, .F. ) ;
#13876 = CARTESIAN_POINT ( 'NONE',  ( -35.00000000000000000, 11.73808581813437968, -0.4353888892048790038 ) ) ;
#13877 = CYLINDRICAL_SURFACE ( 'NONE', #9263, 12.18649999999999878 ) ;
#13878 = AXIS2_PLACEMENT_3D ( 'NONE', #54018, #18778, #23427 ) ;
#13879 = DIRECTION ( 'NONE',  ( 1.000000000000000000, 0.000000000000000000, 0.000000000000000000 ) ) ;
#13880 = DIRECTION ( 'NONE',  ( 1.000000000000000000, 0.000000000000000000, -0.000000000000000000 ) ) ;
#13881 = DIRECTION ( 'NONE',  ( 0.000000000000000000, -0.01356324068817991828, 0.9999080150203990547 ) ) ;
#13882 = AXIS2_PLACEMENT_3D ( 'NONE', #15176, #35456, #55755 ) ;
#13883 = EDGE_CURVE ( 'NONE', #44716, #54679, #27809, .T. ) ;
#13884 = DIRECTION ( 'NONE',  ( -0.3939253465568944290, -0.009718094113426823527, -0.9190910618577645685 ) ) ;
#13885 = VERTEX_POINT ( 'NONE', #2567 ) ;
#13886 = LINE ( 'NONE', #60116, #42336 ) ;
#13887 = AXIS2_PLACEMENT_3D ( 'NONE', #21097, #31414, #47690 ) ;
#13888 = CARTESIAN_POINT ( 'NONE',  ( -16.50484331857675002, 7.681086090980186576, 9.219792269895048520 ) ) ;
#13889 = EDGE_CURVE ( 'NONE', #4651, #52994, #11521, .T. ) ;
#13890 = CARTESIAN_POINT ( 'NONE',  ( -20.33691237604007540, -13.28109756591637947, -2.496095192331454715 ) ) ;
#13891 = DIRECTION ( 'NONE',  ( 0.000000000000000000, 0.9999080150203989437, 0.01356324068818348313 ) ) ;
#13892 = B_SPLINE_CURVE_WITH_KNOTS ( 'NONE', 3,
 ( #52615, #7039, #53256, #7703, #17688, #48602, #2052, #2742, #42256, #22316, #42586, #62888, #32609, #17353, #57930, #43581, #23000, #12344, #3056 ),
 .UNSPECIFIED., .F., .F.,
 ( 4, 3, 3, 3, 3, 3, 4 ),
 ( 8.641030098560686409E-18, 2.825908398991792413E-05, 4.208813692702779546E-05, 5.591713747221096955E-05, 6.279584083537769477E-05, 9.105792820727356767E-05, 0.0001153131102486933926 ),
 .UNSPECIFIED. ) ;
#13893 = CARTESIAN_POINT ( 'NONE',  ( 26.76876439064266222, 11.45740883406175570, 3.577846890752803155 ) ) ;
#13894 = CARTESIAN_POINT ( 'NONE',  ( 37.00000000000000711, -8.235637554476713973, -9.733281772932137699 ) ) ;
#13895 = CYLINDRICAL_SURFACE ( 'NONE', #5547, 12.18649999999999878 ) ;
#13896 = CARTESIAN_POINT ( 'NONE',  ( -35.00000000000000000, -5.015831474386382105, 10.62137734850266391 ) ) ;
#13897 = CARTESIAN_POINT ( 'NONE',  ( 1.198791140417499124, 5.826488554586223501, 11.12379938352617081 ) ) ;
#13898 = AXIS2_PLACEMENT_3D ( 'NONE', #9528, #65708, #25168 ) ;
#13899 = CIRCLE ( 'NONE', #107, 5.000000000000000000 ) ;
#13900 = ORIENTED_EDGE ( 'NONE', *, *, #57346, .T. ) ;
#13901 = CARTESIAN_POINT ( 'NONE',  ( 37.00000000000000711, -12.70128625845191728, 1.113475361586618195 ) ) ;
#13902 = AXIS2_PLACEMENT_3D ( 'NONE', #42601, #37647, #57943 ) ;
#13903 = EDGE_LOOP ( 'NONE', ( #15745, #18905, #24981, #28900 ) ) ;
#13904 = CARTESIAN_POINT ( 'NONE',  ( 2.665405856346775959, 7.981834391067746282, 5.274989403260939902 ) ) ;
#13905 = CARTESIAN_POINT ( 'NONE',  ( -22.27945548916780183, -3.673577025288764730, 0.3299677273100650732 ) ) ;
#13906 = EDGE_CURVE ( 'NONE', #35917, #1946, #26825, .T. ) ;
#13907 = AXIS2_PLACEMENT_3D ( 'NONE', #56443, #41132, #42110 ) ;
#13908 = CARTESIAN_POINT ( 'NONE',  ( -10.71762586082606639, -9.042033845899357658, 10.03605433748208853 ) ) ;
#13909 = DIRECTION ( 'NONE',  ( 0.000000000000000000, -1.000000000000000000, 0.000000000000000000 ) ) ;
#13910 = VERTEX_POINT ( 'NONE', #64358 ) ;
#13911 = LINE ( 'NONE', #60138, #45136 ) ;
#13913 = AXIS2_PLACEMENT_3D ( 'NONE', #2569, #2222, #17180 ) ;
#13912 = CARTESIAN_POINT ( 'NONE',  ( -35.04582288351658548, -0.01196488372923644808, 0.004274985098070607434 ) ) ;
#13914 = CARTESIAN_POINT ( 'NONE',  ( 8.937200413559443390, 4.476360154859203355, 11.13383131558893346 ) ) ;
#13915 = CARTESIAN_POINT ( 'NONE',  ( -22.28284753389937123, 2.640101649307557974, 2.590196335759697543 ) ) ;
#13916 = ADVANCED_FACE ( 'NONE', ( #49736 ), #53428, .T. ) ;
#13917 = ADVANCED_FACE ( 'NONE', ( #12833 ), #3871, .T. ) ;
#13918 = CARTESIAN_POINT ( 'NONE',  ( 35.00000000000000000, 10.43555801961475282, -5.391785509271000087 ) ) ;
#13919 = ORIENTED_EDGE ( 'NONE', *, *, #56106, .T. ) ;
#13920 = DIRECTION ( 'NONE',  ( -1.000000000000000000, 0.000000000000000000, 0.000000000000000000 ) ) ;
#13921 = VERTEX_POINT ( 'NONE', #23825 ) ;
#13922 = AXIS2_PLACEMENT_3D ( 'NONE', #60314, #54997, #19102 ) ;
#13923 = CARTESIAN_POINT ( 'NONE',  ( -35.00000000000000000, -7.094637218249277844, -10.59380114696477726 ) ) ;
#13924 = CARTESIAN_POINT ( 'NONE',  ( -16.48166895389392650, -34.42998396492343716, 6.120168360282491449 ) ) ;
#13925 = EDGE_CURVE ( 'NONE', #28701, #34574, #34431, .T. ) ;
#13926 = CARTESIAN_POINT ( 'NONE',  ( 2.000000000000001776, 4.604744433234674972, 5.919993978425482695 ) ) ;
#13927 = CARTESIAN_POINT ( 'NONE',  ( 6.633584127423891807, -5.026838569920903055, 12.53474721772208511 ) ) ;
#13928 = VECTOR ( 'NONE', #47628, 1000.000000000000000 ) ;
#13929 = AXIS2_PLACEMENT_3D ( 'NONE', #57710, #46728, #62033 ) ;
#13930 = EDGE_CURVE ( 'NONE', #12898, #14666, #1278, .T. ) ;
#13931 = EDGE_LOOP ( 'NONE', ( #23076, #61260, #46859, #56038 ) ) ;
#13932 = ORIENTED_EDGE ( 'NONE', *, *, #28499, .F. ) ;
#13933 = CYLINDRICAL_SURFACE ( 'NONE', #41385, 5.000000000000000888 ) ;
#13934 = DIRECTION ( 'NONE',  ( -0.1699641022377680333, 0.000000000000000000, 0.9854502544271371844 ) ) ;
#13935 = CARTESIAN_POINT ( 'NONE',  ( 2.241352910868908310, -5.901537464758421336, -4.843133558968188979 ) ) ;
#13936 = CARTESIAN_POINT ( 'NONE',  ( 0.3002738374340830907, 12.25576345519757915, 0.2255758963751899049 ) ) ;
#13937 = CARTESIAN_POINT ( 'NONE',  ( 0.3057689695767515370, 9.241339546505193070, -8.055876362038247862 ) ) ;
#13938 = CYLINDRICAL_SURFACE ( 'NONE', #56249, 4.500030059823568074 ) ;
#13939 = ORIENTED_EDGE ( 'NONE', *, *, #65051, .T. ) ;
#13940 = ADVANCED_FACE ( 'NONE', ( #63690 ), #33460, .F. ) ;
#13941 = B_SPLINE_CURVE_WITH_KNOTS ( 'NONE', 3,
 ( #48619, #8055, #59566, #28643, #29610, #14326, #49919, #24307, #34606, #18020, #3071, #23334, #44572, #43597, #18367, #38628 ),
 .UNSPECIFIED., .F., .F.,
 ( 4, 2, 2, 2, 2, 2, 2, 4 ),
 ( 4.091337135425211056E-18, 0.001225059573319686778, 0.001837589359979528107, 0.002450119146639369219, 0.003675178719959051876, 0.004900238293278734968, 0.007350357439918100283, 0.009800476586557464731 ),
 .UNSPECIFIED. ) ;
#13942 = ORIENTED_EDGE ( 'NONE', *, *, #43442, .F. ) ;
#13943 = ORIENTED_EDGE ( 'NONE', *, *, #25974, .T. ) ;
#13944 = LINE ( 'NONE', #7320, #41543 ) ;
#13945 = VECTOR ( 'NONE', #39741, 1000.000000000000000 ) ;
#13946 = AXIS2_PLACEMENT_3D ( 'NONE', #35990, #10737, #41652 ) ;
#13947 = CARTESIAN_POINT ( 'NONE',  ( 145.1370849898475797, 3.309064568108273190E-14, 0.000000000000000000 ) ) ;
#13948 = ORIENTED_EDGE ( 'NONE', *, *, #25264, .T. ) ;
#13949 = CARTESIAN_POINT ( 'NONE',  ( 2.241352910868908310, -3.744764251556946366, -6.652881166698550786 ) ) ;
#13950 = VECTOR ( 'NONE', #2993, 1000.000000000000000 ) ;
#13951 = DIRECTION ( 'NONE',  ( 0.000000000000000000, 0.01356324068817998940, -0.9999080150203990547 ) ) ;
#13952 = VERTEX_POINT ( 'NONE', #33116 ) ;
#13953 = SHAPE_REPRESENTATION ( 'motion translator_ISO - Spur gear 0.25M 58T 20PA 2FW ---S58B6H18L3.0N', ( #24966 ), #29232 ) ;
#13954 = CARTESIAN_POINT ( 'NONE',  ( -25.42680463514451716, 2.219378695194094142, -3.188632951113930414 ) ) ;
#13956 = ADVANCED_FACE ( 'NONE', ( #44390 ), #43756, .T. ) ;
#13955 = FACE_OUTER_BOUND ( 'NONE', #56809, .T. ) ;
#13957 = DIRECTION ( 'NONE',  ( 0.000000000000000000, 0.8276889981568877896, 0.5611870653623862726 ) ) ;
#13958 = ORIENTED_EDGE ( 'NONE', *, *, #42702, .F. ) ;
#13959 = AXIS2_PLACEMENT_3D ( 'NONE', #50700, #5146, #25412 ) ;
#13960 = VERTEX_POINT ( 'NONE', #24132 ) ;
#13961 = CARTESIAN_POINT ( 'NONE',  ( 2.249013661412228693, 2.498855301843084131, 7.216565855998264389 ) ) ;
#13963 = ORIENTED_EDGE ( 'NONE', *, *, #42910, .F. ) ;
#13962 = EDGE_CURVE ( 'NONE', #56170, #15952, #57573, .T. ) ;
#13964 = DIRECTION ( 'NONE',  ( 0.000000000000000000, -0.6745969609292717939, -0.7381862504171902151 ) ) ;
#13965 = ORIENTED_EDGE ( 'NONE', *, *, #31100, .T. ) ;
#13966 = AXIS2_PLACEMENT_3D ( 'NONE', #26423, #46704, #1164 ) ;
#13967 = ORIENTED_EDGE ( 'NONE', *, *, #20806, .F. ) ;
#13969 = ADVANCED_FACE ( 'NONE', ( #9155 ), #64036, .T. ) ;
#13968 = ORIENTED_EDGE ( 'NONE', *, *, #16861, .T. ) ;
#13970 = DIRECTION ( 'NONE',  ( 0.000000000000000000, -1.000000000000000000, 0.000000000000000000 ) ) ;
#13971 = CARTESIAN_POINT ( 'NONE',  ( -1.846890694251213771, -30.59587057577444824, -15.23951446459097170 ) ) ;
#13972 = CARTESIAN_POINT ( 'NONE',  ( 2.000000000000001776, 3.073484823194439386, -6.841322316745028331 ) ) ;
#13973 = CARTESIAN_POINT ( 'NONE',  ( 2.241352910868908754, -7.202080440908725123, -2.532612177304514933 ) ) ;
#13974 = LINE ( 'NONE', #53593, #49399 ) ;
#13975 = ORIENTED_EDGE ( 'NONE', *, *, #48450, .T. ) ;
#13976 = EDGE_CURVE ( 'NONE', #13694, #47279, #64666, .T. ) ;
#13977 = CARTESIAN_POINT ( 'NONE',  ( 1.104777566491145002, 11.07886329447276808, 5.844728374724304842 ) ) ;
#13978 = AXIS2_PLACEMENT_3D ( 'NONE', #2220, #6227, #16840 ) ;
#13979 = ORIENTED_EDGE ( 'NONE', *, *, #9915, .T. ) ;
#13980 =( BOUNDED_SURFACE ( )  B_SPLINE_SURFACE ( 3, 1, ( 
 ( #27846, #11325 ),
 ( #53785, #53116 ),
 ( #33152, #17871 ),
 ( #7558, #32807 ) ),
 .UNSPECIFIED., .F., .F., .F. ) 
 B_SPLINE_SURFACE_WITH_KNOTS ( ( 4, 4 ),
 ( 2, 2 ),
 ( 0.000000000000000000, 1.000000000000000000 ),
 ( 0.000000000000000000, 1.000000000000000000 ),
 .UNSPECIFIED. ) 
 GEOMETRIC_REPRESENTATION_ITEM ( )  RATIONAL_B_SPLINE_SURFACE ( (
 ( 1.000000000000000000, 1.000000000000000000),
 ( 0.9257577194822556033, 0.9980522942447415113),
 ( 0.9257577194822556033, 0.9980522942447415113),
 ( 1.000000000000000000, 1.000000000000000000) ) ) 
 REPRESENTATION_ITEM ( '' )  SURFACE ( )  );
#13981 = DIRECTION ( 'NONE',  ( 0.000000000000000000, -0.01356324068817998940, 0.9999080150203990547 ) ) ;
#13982 = CARTESIAN_POINT ( 'NONE',  ( -37.00000000000000711, 6.711949091238296639, -10.84030624090599559 ) ) ;
#13983 = ADVANCED_FACE ( 'NONE', ( #7870 ), #42508, .F. ) ;
#13984 = AXIS2_PLACEMENT_3D ( 'NONE', #17724, #47644, #42978 ) ;
#13985 = VERTEX_POINT ( 'NONE', #2890 ) ;
#13986 = CARTESIAN_POINT ( 'NONE',  ( 0.3537226245948357772, -10.75912040401513359, 5.910416419900492713 ) ) ;
#13987 = DIRECTION ( 'NONE',  ( 1.000000000000000000, 0.000000000000000000, 0.000000000000000000 ) ) ;
#13988 = CARTESIAN_POINT ( 'NONE',  ( -35.00000000000000000, 0.000000000000000000, 0.000000000000000000 ) ) ;
#13989 = VERTEX_POINT ( 'NONE', #59711 ) ;
#13990 = CIRCLE ( 'NONE', #192, 12.74999999999999822 ) ;
#13991 = VECTOR ( 'NONE', #31958, 1000.000000000000000 ) ;
#13992 = CIRCLE ( 'NONE', #30986, 4.999999999999999112 ) ;
#13993 = ORIENTED_EDGE ( 'NONE', *, *, #9032, .T. ) ;
#13994 = DIRECTION ( 'NONE',  ( -0.000000000000000000, -0.000000000000000000, -1.000000000000000000 ) ) ;
#13995 = ORIENTED_EDGE ( 'NONE', *, *, #41941, .T. ) ;
#13996 = CARTESIAN_POINT ( 'NONE',  ( -25.06355223964699874, -11.89192422770156021, 6.391943611169346617 ) ) ;
#13997 = LINE ( 'NONE', #65199, #47853 ) ;
#13998 = CARTESIAN_POINT ( 'NONE',  ( -30.15699386792130454, -0.5151376480018481363, 13.49760124941971462 ) ) ;
#13999 = CARTESIAN_POINT ( 'NONE',  ( -37.00000000000000711, 7.094637218249358668, 10.59380114696472752 ) ) ;
#14000 = CARTESIAN_POINT ( 'NONE',  ( 0.7400311444011713480, -9.270387619166385207, 8.241979373543633969 ) ) ;
#14001 = VERTEX_POINT ( 'NONE', #18520 ) ;
#14002 = CARTESIAN_POINT ( 'NONE',  ( -22.70624764888619751, -4.501516772829869950, -2.702761586319173404 ) ) ;
#14003 = CARTESIAN_POINT ( 'NONE',  ( 1.020182472822224851, 1.729367949134763771, 12.37761526492745112 ) ) ;
#14004 = AXIS2_PLACEMENT_3D ( 'NONE', #60827, #51533, #21232 ) ;
#14005 = AXIS2_PLACEMENT_3D ( 'NONE', #36839, #41159, #57139 ) ;
#14006 = EDGE_CURVE ( 'NONE', #27622, #28103, #23149, .T. ) ;
#14007 = AXIS2_PLACEMENT_3D ( 'NONE', #39355, #59655, #20068 ) ;
#14008 = CARTESIAN_POINT ( 'NONE',  ( -13.38666790241063964, -28.49056413965659473, -12.64716857254873617 ) ) ;
#14009 = CARTESIAN_POINT ( 'NONE',  ( 2.573738926104375047, -5.156412073069320812, 5.779258037546994409 ) ) ;
#14010 = CYLINDRICAL_SURFACE ( 'NONE', #45817, 13.50000000000000178 ) ;
#14011 = CARTESIAN_POINT ( 'NONE',  ( 7.292875064767452287, -5.787367871520388007, -10.52247668536931435 ) ) ;
#14012 = DIRECTION ( 'NONE',  ( -1.000000000000000000, 0.000000000000000000, 0.000000000000000000 ) ) ;
#14013 = VECTOR ( 'NONE', #49025, 1000.000000000000000 ) ;
#14014 = EDGE_CURVE ( 'NONE', #61621, #29328, #7633, .T. ) ;
#14015 = ORIENTED_EDGE ( 'NONE', *, *, #59667, .F. ) ;
#14016 = CARTESIAN_POINT ( 'NONE',  ( 37.00000000000000711, 9.896810808925392777, -7.110831038798317572 ) ) ;
#14017 = CIRCLE ( 'NONE', #32058, 12.74999999999999822 ) ;
#14018 = VERTEX_POINT ( 'NONE', #28788 ) ;
#14019 = DIRECTION ( 'NONE',  ( -0.000000000000000000, -1.000000000000000000, -0.000000000000000000 ) ) ;
#14020 = CARTESIAN_POINT ( 'NONE',  ( 2.770579946183332254, -7.437949029067708828, 2.384572752174059396 ) ) ;
#14021 = CARTESIAN_POINT ( 'NONE',  ( -27.01437459610461644, 11.79277645698183363, -2.220455681983952267 ) ) ;
#14022 = ORIENTED_EDGE ( 'NONE', *, *, #15545, .F. ) ;
#14023 = ADVANCED_FACE ( 'NONE', ( #29131 ), #49432, .T. ) ;
#14024 = AXIS2_PLACEMENT_3D ( 'NONE', #49627, #44954, #12801 ) ;
#14025 = EDGE_LOOP ( 'NONE', ( #29638, #15265, #14888, #23306 ) ) ;
#14026 = ORIENTED_EDGE ( 'NONE', *, *, #31777, .F. ) ;
#14027 = CARTESIAN_POINT ( 'NONE',  ( 0.2657645697724678180, -7.755260067564094584, -9.477802844074121325 ) ) ;
#14028 = EDGE_CURVE ( 'NONE', #26931, #2058, #33454, .T. ) ;
#14029 = AXIS2_PLACEMENT_3D ( 'NONE', #43717, #24098, #44358 ) ;
#14030 = VERTEX_POINT ( 'NONE', #45717 ) ;
#14031 = CARTESIAN_POINT ( 'NONE',  ( -22.27716857039623477, -2.496432241075901892, -2.705892286796406587 ) ) ;
#14032 = CYLINDRICAL_SURFACE ( 'NONE', #64433, 13.50000000000000178 ) ;
#14033 = CARTESIAN_POINT ( 'NONE',  ( 0.2956976708475456683, 10.50256636126827203, 6.317697191869677376 ) ) ;
#14034 = DIRECTION ( 'NONE',  ( 0.000000000000000000, -0.9796553971857721033, -0.2006870767258996657 ) ) ;
#14035 = VERTEX_POINT ( 'NONE', #20781 ) ;
#14036 = LINE ( 'NONE', #34638, #25512 ) ;
#14037 = CARTESIAN_POINT ( 'NONE',  ( -7.454036404616594780, -28.85515183291198227, -12.27947133142141212 ) ) ;
#14038 = CARTESIAN_POINT ( 'NONE',  ( 2.259025283528087957, -1.461109758650511070, -7.499281868334255918 ) ) ;
#14040 = VERTEX_POINT ( 'NONE', #41053 ) ;
#14039 = CARTESIAN_POINT ( 'NONE',  ( 5.536195898058073439, 0.008323005098841094671, -0.001726268814999541799 ) ) ;
#14041 = DIRECTION ( 'NONE',  ( -1.000000000000000000, 0.000000000000000000, 0.000000000000000000 ) ) ;
#14042 = ORIENTED_EDGE ( 'NONE', *, *, #1384, .F. ) ;
#14043 = CARTESIAN_POINT ( 'NONE',  ( 0.2872850955227773118, -6.306790329742856471, -10.50585060073186483 ) ) ;
#14044 = ORIENTED_EDGE ( 'NONE', *, *, #42347, .T. ) ;
#14045 = CARTESIAN_POINT ( 'NONE',  ( -29.65824816215590687, -0.5562943748163905466, -11.99470473606822907 ) ) ;
#14046 = AXIS2_PLACEMENT_3D ( 'NONE', #56768, #11190, #7492 ) ;
#14047 = CARTESIAN_POINT ( 'NONE',  ( 0.3164563675027628475, 3.967501530099240448, -11.60369811966058862 ) ) ;
#14048 = EDGE_CURVE ( 'NONE', #19224, #35366, #39513, .T. ) ;
#14049 = DIRECTION ( 'NONE',  ( -1.000000000000000000, 0.000000000000000000, 0.000000000000000000 ) ) ;
#14050 = DIRECTION ( 'NONE',  ( -1.000000000000000000, 0.000000000000000000, 0.000000000000000000 ) ) ;
#14051 = AXIS2_PLACEMENT_3D ( 'NONE', #19997, #24999, #50603 ) ;
#14052 = CARTESIAN_POINT ( 'NONE',  ( 0.2653519991613838003, -11.51519138201633474, 4.167757449530376412 ) ) ;
#14053 = DIRECTION ( 'NONE',  ( 0.000000000000000000, -0.01356324068817998940, 0.9999080150203990547 ) ) ;
#14054 = CARTESIAN_POINT ( 'NONE',  ( 0.2911222467163541716, -3.989243506922266924, -11.58731125337564016 ) ) ;
#14056 = ORIENTED_EDGE ( 'NONE', *, *, #22214, .F. ) ;
#14055 = CARTESIAN_POINT ( 'NONE',  ( -37.00000000000000711, 8.854740511458851770, 7.717887834988275131 ) ) ;
#14057 = ADVANCED_FACE ( 'NONE', ( #55369 ), #9467, .T. ) ;
#14058 = AXIS2_PLACEMENT_3D ( 'NONE', #27611, #32584, #17328 ) ;
#14059 = ORIENTED_EDGE ( 'NONE', *, *, #65582, .F. ) ;
#14060 = CARTESIAN_POINT ( 'NONE',  ( 0.000000000000000000, 0.000000000000000000, 0.000000000000000000 ) ) ;
#14061 = ORIENTED_EDGE ( 'NONE', *, *, #58838, .T. ) ;
#14062 = CIRCLE ( 'NONE', #43831, 4.999999999999999112 ) ;
#14063 = EDGE_CURVE ( 'NONE', #50365, #7766, #45334, .T. ) ;
#14064 = VERTEX_POINT ( 'NONE', #60042 ) ;
#14065 = CYLINDRICAL_SURFACE ( 'NONE', #2004, 12.74999999999999822 ) ;
#14066 = CARTESIAN_POINT ( 'NONE',  ( 0.3665391374699472626, 10.76665847464312620, 5.911453292029639428 ) ) ;
#14067 = CARTESIAN_POINT ( 'NONE',  ( 32.00000000000000000, 1.230770033143089974E-14, 0.000000000000000000 ) ) ;
#14068 = CARTESIAN_POINT ( 'NONE',  ( 0.2671309869109479429, -10.52409658627921019, 6.263183022891143814 ) ) ;
#14069 = CARTESIAN_POINT ( 'NONE',  ( -22.28776923226071460, 1.601293944844132122, -3.350304995653732743 ) ) ;
#14070 = DIRECTION ( 'NONE',  ( 0.000000000000000000, -0.01356324068817998940, 0.9999080150203990547 ) ) ;
#14071 = EDGE_CURVE ( 'NONE', #29408, #16453, #47977, .T. ) ;
#14072 = CARTESIAN_POINT ( 'NONE',  ( 1.633930747252547055, -11.34237452761363585, -5.718685543473386090 ) ) ;
#14073 = VECTOR ( 'NONE', #13268, 1000.000000000000000 ) ;
#14074 = ORIENTED_EDGE ( 'NONE', *, *, #59555, .F. ) ;
#14075 = PLANE ( 'NONE',  #57298 ) ;
#14076 = DIRECTION ( 'NONE',  ( 0.000000000000000000, 0.01356324068817998940, -0.9999080150203989437 ) ) ;
#14077 = CARTESIAN_POINT ( 'NONE',  ( 0.000000000000000000, -7.387287142779332960, -1.295372019972250710 ) ) ;
#14078 = EDGE_LOOP ( 'NONE', ( #47435, #39265, #5826, #26596, #14015, #29916 ) ) ;
#14079 = VECTOR ( 'NONE', #19360, 1000.000000000000000 ) ;
#14080 = CIRCLE ( 'NONE', #20454, 12.18650000000000055 ) ;
#14081 = B_SPLINE_CURVE_WITH_KNOTS ( 'NONE', 3,
 ( #51448, #26157, #41418, #11185, #5560, #30783, #46428, #40444, #60741, #15183 ),
 .UNSPECIFIED., .F., .F.,
 ( 4, 3, 3, 4 ),
 ( 1.939479807224432123E-18, 6.607638129004473975E-05, 9.911389841680488377E-05, 0.0001667630577588610102 ),
 .UNSPECIFIED. ) ;
#14082 = AXIS2_PLACEMENT_3D ( 'NONE', #6911, #31509, #41819 ) ;
#14083 = AXIS2_PLACEMENT_3D ( 'NONE', #21045, #36351, #11092 ) ;
#14084 = ADVANCED_FACE ( 'NONE', ( #11767 ), #40792, .F. ) ;
#14085 = CARTESIAN_POINT ( 'NONE',  ( 2.241528039335008327, -2.596349773934832683, -7.179411278563578414 ) ) ;
#14086 = LINE ( 'NONE', #49678, #32043 ) ;
#14087 = ORIENTED_EDGE ( 'NONE', *, *, #37919, .T. ) ;
#14088 = CARTESIAN_POINT ( 'NONE',  ( -22.27706485742869091, 2.625261754997705310, -2.580541389029900934 ) ) ;
#14089 = DIRECTION ( 'NONE',  ( -1.000000000000000000, 0.000000000000000000, 0.000000000000000000 ) ) ;
#14090 = CARTESIAN_POINT ( 'NONE',  ( -35.00000000000000000, 0.000000000000000000, 0.000000000000000000 ) ) ;
#14091 = VECTOR ( 'NONE', #11152, 1000.000000000000000 ) ;
#14092 = CIRCLE ( 'NONE', #11966, 12.74999999999999822 ) ;
#14093 = CARTESIAN_POINT ( 'NONE',  ( -18.04458733766117362, 25.00000000000000000, 3.916728392552376370 ) ) ;
#14094 = LINE ( 'NONE', #24399, #63817 ) ;
#14095 = VERTEX_POINT ( 'NONE', #1159 ) ;
#14096 = DIRECTION ( 'NONE',  ( -1.000000000000000000, 0.000000000000000000, -0.000000000000000000 ) ) ;
#14097 = CARTESIAN_POINT ( 'NONE',  ( 0.2706063244538030044, -12.09107863371559155, 1.954041462022380049 ) ) ;
#14098 = AXIS2_PLACEMENT_3D ( 'NONE', #64030, #53423, #48436 ) ;
#14099 = CYLINDRICAL_SURFACE ( 'NONE', #18058, 5.000000000000000888 ) ;
#14100 = ORIENTED_EDGE ( 'NONE', *, *, #5551, .T. ) ;
#14101 = DIRECTION ( 'NONE',  ( -0.8405098440481674205, 0.000000000000000000, -0.5417962735734949131 ) ) ;
#14102 = DIRECTION ( 'NONE',  ( 0.000000000000000000, -0.01356324068817998940, 0.9999080150203990547 ) ) ;
#14103 = VERTEX_POINT ( 'NONE', #16766 ) ;
#14104 = EDGE_CURVE ( 'NONE', #7512, #42983, #4461, .T. ) ;
#14105 = ORIENTED_EDGE ( 'NONE', *, *, #11337, .T. ) ;
#14106 = CARTESIAN_POINT ( 'NONE',  ( -22.70624764888619751, 0.7939291279022951953, -5.190207123845785198 ) ) ;
#14107 = EDGE_CURVE ( 'NONE', #50541, #13558, #25711, .T. ) ;
#14108 = ORIENTED_EDGE ( 'NONE', *, *, #17215, .T. ) ;
#14109 = DIRECTION ( 'NONE',  ( -1.000000000000000000, 0.000000000000000000, 0.000000000000000000 ) ) ;
#14110 = CARTESIAN_POINT ( 'NONE',  ( 0.3160775863651047457, -6.338373607799261400, 10.49803827792120714 ) ) ;
#14111 = CARTESIAN_POINT ( 'NONE',  ( 2.305787727787084851, -7.566723232958062262, -1.164987321564809886 ) ) ;
#14112 = CARTESIAN_POINT ( 'NONE',  ( 1.937114397841932290, -7.538912286488274717, -10.38782037574624262 ) ) ;
#14114 = ORIENTED_EDGE ( 'NONE', *, *, #39350, .F. ) ;
#14113 = CARTESIAN_POINT ( 'NONE',  ( 2.241506898688418570, -7.634383346098566392, 0.03933068055388246748 ) ) ;
#14115 = DIRECTION ( 'NONE',  ( 0.000000000000000000, -0.9635499925192201331, -0.2675283385292311911 ) ) ;
#14116 = VERTEX_POINT ( 'NONE', #52030 ) ;
#14117 = AXIS2_PLACEMENT_3D ( 'NONE', #25313, #55246, #14993 ) ;
#14118 = CYLINDRICAL_SURFACE ( 'NONE', #49762, 4.999999999999999112 ) ;
#14119 = ORIENTED_EDGE ( 'NONE', *, *, #47441, .T. ) ;
#14120 = VECTOR ( 'NONE', #14202, 1000.000000000000000 ) ;
#14121 = EDGE_LOOP ( 'NONE', ( #11397, #64964, #27280, #64348 ) ) ;
#14122 = CARTESIAN_POINT ( 'NONE',  ( -24.80569231367726246, 10.34937607735212772, 8.670028611839507349 ) ) ;
#14123 = CARTESIAN_POINT ( 'NONE',  ( -14.91771861688918399, -28.90354855594946315, 11.53870211789912759 ) ) ;
#14124 = EDGE_CURVE ( 'NONE', #21349, #36463, #62976, .T. ) ;
#14126 = CARTESIAN_POINT ( 'NONE',  ( -26.79516877879233050, 12.45549024775193736, 5.207329862939345411 ) ) ;
#14125 = AXIS2_PLACEMENT_3D ( 'NONE', #8136, #3499, #27416 ) ;
#14127 = AXIS2_PLACEMENT_3D ( 'NONE', #11980, #12626, #31603 ) ;
#14128 = CARTESIAN_POINT ( 'NONE',  ( 24.36182730707165689, -0.005113602571830759905, 12.00528096431153280 ) ) ;
#14129 = CARTESIAN_POINT ( 'NONE',  ( 5.516018279890452902, 0.004525000489649935558, -0.005042957932159086720 ) ) ;
#14130 = DIRECTION ( 'NONE',  ( 0.000000000000000000, -0.2149704402110114432, -0.9766205557100894330 ) ) ;
#14131 = ORIENTED_EDGE ( 'NONE', *, *, #35056, .T. ) ;
#14132 = VERTEX_POINT ( 'NONE', #12419 ) ;
#14133 = DIRECTION ( 'NONE',  ( 0.000000000000000000, -0.8989688749565111214, -0.4380125133594070519 ) ) ;
#14134 = ORIENTED_EDGE ( 'NONE', *, *, #54277, .F. ) ;
#14135 = AXIS2_PLACEMENT_3D ( 'NONE', #63169, #22266, #7989 ) ;
#14136 = CARTESIAN_POINT ( 'NONE',  ( 35.00000000000000000, -7.474872387601069867, -9.060822531526026680 ) ) ;
#14137 = CARTESIAN_POINT ( 'NONE',  ( 2.655192694323660341, -8.010337395399627525, 5.293797899976080856 ) ) ;
#14138 = DIRECTION ( 'NONE',  ( 1.000000000000000000, 0.000000000000000000, 0.000000000000000000 ) ) ;
#14139 = CARTESIAN_POINT ( 'NONE',  ( -27.35552965826136429, -2.810569013793742688, 1.320216934008381804 ) ) ;
#14140 = EDGE_CURVE ( 'NONE', #22570, #5722, #64944, .T. ) ;
#14141 = CIRCLE ( 'NONE', #42811, 12.18650000000000055 ) ;
#14142 = CARTESIAN_POINT ( 'NONE',  ( 1.719304012338398469, 8.755325027793414705, 9.242227816402090568 ) ) ;
#14143 = CARTESIAN_POINT ( 'NONE',  ( 2.903928887688295379, 0.9983813550132488723, -8.712847781149726245 ) ) ;
#14144 = VERTEX_POINT ( 'NONE', #47049 ) ;
#14145 = CIRCLE ( 'NONE', #55607, 5.000000000000000888 ) ;
#14146 = VERTEX_POINT ( 'NONE', #46382 ) ;
#14147 = CIRCLE ( 'NONE', #54525, 2.899999999999995470 ) ;
#14148 = DIRECTION ( 'NONE',  ( -1.000000000000000000, -0.000000000000000000, 0.000000000000000000 ) ) ;
#14149 = CARTESIAN_POINT ( 'NONE',  ( 35.00000000000000000, 11.65150730582934635, 1.488153103997001514 ) ) ;
#14150 = CYLINDRICAL_SURFACE ( 'NONE', #21318, 12.18650000000000055 ) ;
#14151 = ORIENTED_EDGE ( 'NONE', *, *, #15337, .F. ) ;
#14152 = CIRCLE ( 'NONE', #18423, 4.999999999999999112 ) ;
#14153 = CARTESIAN_POINT ( 'NONE',  ( 5.520433897694421610, -0.007082458259338479320, 0.01329351892498011924 ) ) ;
#14154 = EDGE_CURVE ( 'NONE', #32398, #28276, #828, .T. ) ;
#14155 =( BOUNDED_CURVE ( )  B_SPLINE_CURVE ( 3, ( #621, #14885, #35821, #55819 ),
 .UNSPECIFIED., .F., .F. ) 
 B_SPLINE_CURVE_WITH_KNOTS ( ( 4, 4 ),
 ( 2.725141476405820384, 2.750767380661962136 ),
 .UNSPECIFIED. ) 
 CURVE ( )  GEOMETRIC_REPRESENTATION_ITEM ( )  RATIONAL_B_SPLINE_CURVE ( ( 1.000000000000000000, 0.9999452768345937770, 0.9999452768345937770, 1.000000000000000000 ) ) 
 REPRESENTATION_ITEM ( '' )  );
#14156 = CARTESIAN_POINT ( 'NONE',  ( -5.394281107717450396, -1.427634444718381079, -11.91478059761895558 ) ) ;
#14157 = CARTESIAN_POINT ( 'NONE',  ( 145.1370849898475797, 3.309064568108273190E-14, 0.000000000000000000 ) ) ;
#14158 = CARTESIAN_POINT ( 'NONE',  ( -27.08421723179412410, -2.188590898430375908, -0.6782017488087925816 ) ) ;
#14159 = ADVANCED_FACE ( 'NONE', ( #46702 ), #27394, .T. ) ;
#14160 = CARTESIAN_POINT ( 'NONE',  ( -2.532614230583022152, -11.30437021680553222, 4.026315189028233377 ) ) ;
#14161 = ORIENTED_EDGE ( 'NONE', *, *, #34060, .F. ) ;
#14162 = AXIS2_PLACEMENT_3D ( 'NONE', #52704, #7802, #12431 ) ;
#14163 = CARTESIAN_POINT ( 'NONE',  ( -21.04906020170784942, 11.41231286973902925, -3.710994071045396137 ) ) ;
#14164 = DIRECTION ( 'NONE',  ( -1.000000000000000000, 0.000000000000000000, 0.000000000000000000 ) ) ;
#14165 = CIRCLE ( 'NONE', #28008, 5.000000000000000888 ) ;
#14166 = DIRECTION ( 'NONE',  ( 0.000000000000000000, 0.01356324068817992522, -0.9999080150203990547 ) ) ;
#14167 = AXIS2_PLACEMENT_3D ( 'NONE', #38968, #24012, #28996 ) ;
#14168 = EDGE_CURVE ( 'NONE', #50541, #4916, #57684, .T. ) ;
#14169 = CARTESIAN_POINT ( 'NONE',  ( 2.844750968615770148, -3.626176236708136713, 6.946006365803760296 ) ) ;
#14170 = CARTESIAN_POINT ( 'NONE',  ( 0.3675815128205894289, -4.447030445008105737, -11.44679196252413789 ) ) ;
#14171 = ORIENTED_EDGE ( 'NONE', *, *, #65639, .F. ) ;
#14172 = CARTESIAN_POINT ( 'NONE',  ( 1.000000000000000888, -3.224464355699781848, -6.771471746882029130 ) ) ;
#14173 = CARTESIAN_POINT ( 'NONE',  ( 2.835339799623878054, 6.612744557053422234, 4.197472173747671675 ) ) ;
#14174 = VECTOR ( 'NONE', #36141, 1000.000000000000000 ) ;
#14175 = CARTESIAN_POINT ( 'NONE',  ( 8.295782569430503628, -26.46630966554524278, -14.48708413691750074 ) ) ;
#14176 = EDGE_LOOP ( 'NONE', ( #38171, #53730, #61482, #31810 ) ) ;
#14177 = CARTESIAN_POINT ( 'NONE',  ( 0.9296196016823387032, -6.590257778216964901, 10.58347995892855842 ) ) ;
#14178 = CARTESIAN_POINT ( 'NONE',  ( -28.21837939661944006, -12.11352702982830642, -5.967125770076286528 ) ) ;
#14179 = DIRECTION ( 'NONE',  ( 0.000000000000000000, 0.000000000000000000, 1.000000000000000000 ) ) ;
#14180 = ADVANCED_FACE ( 'NONE', ( #21784 ), #32690, .T. ) ;
#14181 = AXIS2_PLACEMENT_3D ( 'NONE', #20481, #36070, #40762 ) ;
#14182 = CYLINDRICAL_SURFACE ( 'NONE', #59390, 12.75000000000000178 ) ;
#14183 = FACE_OUTER_BOUND ( 'NONE', #32408, .T. ) ;
#14184 = AXIS2_PLACEMENT_3D ( 'NONE', #5813, #6126, #62281 ) ;
#14185 = CARTESIAN_POINT ( 'NONE',  ( 1.719304012342639965, 12.38166659047149487, -2.961219984262613458 ) ) ;
#14186 = ORIENTED_EDGE ( 'NONE', *, *, #29761, .T. ) ;
#14187 = CARTESIAN_POINT ( 'NONE',  ( 2.241352910868909643, -6.569501556381414531, -3.889181972941518683 ) ) ;
#14188 = CARTESIAN_POINT ( 'NONE',  ( -8.018618887729799027, 9.418346547213671371, -9.692888119526816837 ) ) ;
#14190 = VECTOR ( 'NONE', #4073, 1000.000000000000000 ) ;
#14189 = CARTESIAN_POINT ( 'NONE',  ( 37.00000000000000711, 4.705694406421931860E-17, -3.469127814946512892E-15 ) ) ;
#14191 = CARTESIAN_POINT ( 'NONE',  ( 2.969415267405017822, -4.760005747566342649, 6.276215141898974892 ) ) ;
#14192 = CARTESIAN_POINT ( 'NONE',  ( 2.255723233588951882, 7.544965460065586882, -1.196143347838635407 ) ) ;
#14193 = CARTESIAN_POINT ( 'NONE',  ( 35.00000000000000000, 4.705694406421931860E-17, -3.469127814946512892E-15 ) ) ;
#14194 = VECTOR ( 'NONE', #60113, 1000.000000000000114 ) ;
#14195 = CARTESIAN_POINT ( 'NONE',  ( -25.42680463514451716, 3.188632951113952174, 2.219378695194055062 ) ) ;
#14196 = CARTESIAN_POINT ( 'NONE',  ( 2.242418902651536428, 1.227462051875141569, -7.535443599794351854 ) ) ;
#14197 = VERTEX_POINT ( 'NONE', #61659 ) ;
#14198 = ORIENTED_EDGE ( 'NONE', *, *, #18298, .F. ) ;
#14199 = CARTESIAN_POINT ( 'NONE',  ( -17.65540486153495792, -7.075472138365880070, -9.696984679443399813 ) ) ;
#14200 = VERTEX_POINT ( 'NONE', #16115 ) ;
#14201 =( NAMED_UNIT ( * ) PLANE_ANGLE_UNIT ( ) SI_UNIT ( $, .RADIAN. ) );
#14202 = DIRECTION ( 'NONE',  ( -1.000000000000000000, -0.000000000000000000, 0.000000000000000000 ) ) ;
#14203 = CIRCLE ( 'NONE', #14901, 12.75000000000000178 ) ;
#14204 = CARTESIAN_POINT ( 'NONE',  ( 1.452237505248552996, 3.767214359061125784, 12.08199618361514460 ) ) ;
#14205 = ORIENTED_EDGE ( 'NONE', *, *, #39194, .F. ) ;
#14206 = CARTESIAN_POINT ( 'NONE',  ( 0.3632410797595245211, 5.910360611678975751, -10.76277061791634360 ) ) ;
#14207 = DIRECTION ( 'NONE',  ( 0.000000000000000000, -0.8660254037844380415, -0.5000000000000009992 ) ) ;
#14208 = CARTESIAN_POINT ( 'NONE',  ( 2.244591118396919605, -4.989853642776339804, -5.779440292195060280 ) ) ;
#14209 = ORIENTED_EDGE ( 'NONE', *, *, #33503, .T. ) ;
#14210 = VERTEX_POINT ( 'NONE', #32382 ) ;
#14211 = CARTESIAN_POINT ( 'NONE',  ( 2.260457164927185847, -7.226149053012470347, -2.482766715766981935 ) ) ;
#14213 = DIRECTION ( 'NONE',  ( -1.000000000000000000, 0.000000000000000000, 0.000000000000000000 ) ) ;
#14212 = CIRCLE ( 'NONE', #51417, 12.18650000000000055 ) ;
#14214 = EDGE_CURVE ( 'NONE', #8323, #64016, #36279, .T. ) ;
#14215 = AXIS2_PLACEMENT_3D ( 'NONE', #53822, #24521, #28863 ) ;
#14216 = ORIENTED_EDGE ( 'NONE', *, *, #45552, .F. ) ;
#14217 = CARTESIAN_POINT ( 'NONE',  ( 35.00000000000000000, -11.24036214326524608, -6.018036132182126963 ) ) ;
#14218 = ORIENTED_EDGE ( 'NONE', *, *, #28541, .T. ) ;
#14219 = DIRECTION ( 'NONE',  ( -1.000000000000000000, 0.000000000000000000, 0.000000000000000000 ) ) ;
#14220 = CARTESIAN_POINT ( 'NONE',  ( -27.09342121492660382, -1.607500752098860231, 1.671264186073233571 ) ) ;
#14221 = AXIS2_PLACEMENT_3D ( 'NONE', #1193, #41744, #13125 ) ;
#14222 = EDGE_CURVE ( 'NONE', #26347, #46169, #54063, .T. ) ;
#14223 = DIRECTION ( 'NONE',  ( 0.000000000000000000, 0.000000000000000000, 1.000000000000000000 ) ) ;
#14224 = LINE ( 'NONE', #29835, #16805 ) ;
#14225 = LINE ( 'NONE', #9230, #7864 ) ;
#14226 = EDGE_LOOP ( 'NONE', ( #26244, #42440, #40519, #12351 ) ) ;
#14227 = CARTESIAN_POINT ( 'NONE',  ( 2.260457164927187179, 7.639515169785715543, -0.1384509728649304106 ) ) ;
#14228 = CARTESIAN_POINT ( 'NONE',  ( 35.00000000000000000, -11.59095880812006385, 1.903127969211307224 ) ) ;
#14229 = DIRECTION ( 'NONE',  ( -1.000000000000000000, 0.000000000000000000, 0.000000000000000000 ) ) ;
#14230 = CYLINDRICAL_SURFACE ( 'NONE', #51921, 4.999999999999999112 ) ;
#14231 = DIRECTION ( 'NONE',  ( 1.000000000000000000, -0.000000000000000000, -0.000000000000000000 ) ) ;
#14232 = CIRCLE ( 'NONE', #22758, 4.999999999999999112 ) ;
#14233 = CARTESIAN_POINT ( 'NONE',  ( -27.08639648637162622, 1.614109828501636201, -1.635407781268143124 ) ) ;
#14234 = CARTESIAN_POINT ( 'NONE',  ( -27.35552965826135008, 3.094132632038936404, 0.2619431035391969198 ) ) ;
#14235 = LINE ( 'NONE', #19574, #27032 ) ;
#14236 = B_SPLINE_CURVE_WITH_KNOTS ( 'NONE', 3,
 ( #21272, #31264, #62174, #41217, #61194, #15940, #16626, #35892, #56189, #56538, #47228, #51235, #10982, #51568, #62480, #6017 ),
 .UNSPECIFIED., .F., .F.,
 ( 4, 3, 3, 3, 3, 4 ),
 ( 0.000000000000000000, 0.0002176109881720252439, 0.0004352086762394603413, 0.0006528017811446877247, 0.0007615147961451705421, 0.0009453342004947429180 ),
 .UNSPECIFIED. ) ;
#14237 = DIRECTION ( 'NONE',  ( -1.000000000000000000, 0.000000000000000000, 0.000000000000000000 ) ) ;
#14238 = AXIS2_PLACEMENT_3D ( 'NONE', #63265, #37996, #1788 ) ;
#14239 = EDGE_CURVE ( 'NONE', #20746, #25736, #4008, .T. ) ;
#14240 = ORIENTED_EDGE ( 'NONE', *, *, #37079, .F. ) ;
#14241 = CARTESIAN_POINT ( 'NONE',  ( 0.3675815128205894289, 0.2638082659428422350, 12.27743992903066328 ) ) ;
#14242 = EDGE_CURVE ( 'NONE', #61726, #14742, #64594, .T. ) ;
#14243 = ORIENTED_EDGE ( 'NONE', *, *, #43041, .F. ) ;
#14244 = EDGE_CURVE ( 'NONE', #125, #14997, #58625, .T. ) ;
#14245 = DIRECTION ( 'NONE',  ( 0.000000000000000000, -0.01356324068817991828, 0.9999080150203990547 ) ) ;
#14246 = CARTESIAN_POINT ( 'NONE',  ( 2.255723233588948773, -7.499053486174012129, -1.456523090672685816 ) ) ;
#14247 = CIRCLE ( 'NONE', #12156, 2.214855479030549468 ) ;
#14248 = CARTESIAN_POINT ( 'NONE',  ( 2.241537034860906275, -4.910958050585477963, 5.845308934728764783 ) ) ;
#14249 = CARTESIAN_POINT ( 'NONE',  ( -37.00000000000000711, 0.000000000000000000, 0.000000000000000000 ) ) ;
#14250 = EDGE_CURVE ( 'NONE', #33968, #32845, #46063, .T. ) ;
#14251 = CARTESIAN_POINT ( 'NONE',  ( 2.000000000000001776, 0.4804830611970061227, 6.919838746524539452 ) ) ;
#14252 = ORIENTED_EDGE ( 'NONE', *, *, #17190, .F. ) ;
#14253 = CARTESIAN_POINT ( 'NONE',  ( -27.16408673750833103, 8.649729821182791767, -8.318274995791208326 ) ) ;
#14254 = LINE ( 'NONE', #10241, #243 ) ;
#14255 = DIRECTION ( 'NONE',  ( -1.000000000000000000, -0.000000000000000000, 0.000000000000000000 ) ) ;
#14256 = CARTESIAN_POINT ( 'NONE',  ( 0.9232167919969133107, 2.570564963838149364, 12.19756235544080525 ) ) ;
#14257 = ADVANCED_FACE ( 'NONE', ( #8770 ), #47583, .F. ) ;
#14258 = LINE ( 'NONE', #34841, #22335 ) ;
#14259 = ORIENTED_EDGE ( 'NONE', *, *, #13172, .T. ) ;
#14260 = EDGE_CURVE ( 'NONE', #5091, #10987, #42677, .T. ) ;
#14261 = DIRECTION ( 'NONE',  ( 1.000000000000000000, 0.000000000000000000, 0.000000000000000000 ) ) ;
#14262 = ORIENTED_EDGE ( 'NONE', *, *, #50149, .T. ) ;
#14263 = CARTESIAN_POINT ( 'NONE',  ( 0.2915757698887299632, -0.2147157799033968251, -12.25305747416128099 ) ) ;
#14264 = CARTESIAN_POINT ( 'NONE',  ( -36.00000000000000711, -6.018036132182241538, 11.24036214326518390 ) ) ;
#14265 = CIRCLE ( 'NONE', #43995, 7.938172270156617749 ) ;
#14266 = AXIS2_PLACEMENT_3D ( 'NONE', #4214, #45417, #25148 ) ;
#14267 = DIRECTION ( 'NONE',  ( 1.000000000000000000, -0.000000000000000000, 0.000000000000000000 ) ) ;
#14268 = DIRECTION ( 'NONE',  ( 0.000000000000000000, -0.9970832820307030664, -0.07632122047557567124 ) ) ;
#14269 = EDGE_LOOP ( 'NONE', ( #17456, #21591, #45881, #686 ) ) ;
#14270 = ORIENTED_EDGE ( 'NONE', *, *, #15999, .F. ) ;
#14272 = EDGE_CURVE ( 'NONE', #59596, #25928, #14017, .T. ) ;
#14271 = CARTESIAN_POINT ( 'NONE',  ( -15.69195845145067736, -33.00000000000000000, -4.009712365929965827 ) ) ;
#14273 = CARTESIAN_POINT ( 'NONE',  ( 35.00000000000000000, 4.705694406421931860E-17, -3.469127814946512892E-15 ) ) ;
#14274 = CARTESIAN_POINT ( 'NONE',  ( 5.515188684475870851, -0.003709313826049772961, 0.003857086913166378472 ) ) ;
#14275 = CYLINDRICAL_SURFACE ( 'NONE', #51172, 6.094511299047803199 ) ;
#14276 = CARTESIAN_POINT ( 'NONE',  ( 2.941278708680199916, 3.185832147968446826, 5.248410529370236333 ) ) ;
#14277 = CARTESIAN_POINT ( 'NONE',  ( 0.3223008802179246901, 9.236652594547246409, -8.069628056118025583 ) ) ;
#14278 = CARTESIAN_POINT ( 'NONE',  ( 2.000000000000001776, 0.000000000000000000, 0.000000000000000000 ) ) ;
#14279 = CARTESIAN_POINT ( 'NONE',  ( 1.000000000000000888, -5.662015959325143122, -4.918493191654053298 ) ) ;
#14280 = ORIENTED_EDGE ( 'NONE', *, *, #24164, .F. ) ;
#14281 = ORIENTED_EDGE ( 'NONE', *, *, #10794, .T. ) ;
#14282 = ORIENTED_EDGE ( 'NONE', *, *, #1807, .F. ) ;
#14283 = DIRECTION ( 'NONE',  ( 1.000000000000000000, 0.000000000000000000, 0.000000000000000000 ) ) ;
#14284 = CIRCLE ( 'NONE', #22800, 12.18650000000000233 ) ;
#14285 = PLANE ( 'NONE',  #32110 ) ;
#14286 = VERTEX_POINT ( 'NONE', #29369 ) ;
#14287 = CARTESIAN_POINT ( 'NONE',  ( -4.806344283790351390, -7.508992741355383416, 25.00000000000000000 ) ) ;
#14288 = VERTEX_POINT ( 'NONE', #11303 ) ;
#14289 = LINE ( 'NONE', #39891, #34382 ) ;
#14290 = LINE ( 'NONE', #15279, #33956 ) ;
#14291 = CARTESIAN_POINT ( 'NONE',  ( 3.152665057736013132, 7.281573230473836311, -3.161213418915250095 ) ) ;
#14292 = VERTEX_POINT ( 'NONE', #10977 ) ;
#14293 = ORIENTED_EDGE ( 'NONE', *, *, #25264, .F. ) ;
#14294 = DIRECTION ( 'NONE',  ( 0.000000000000000000, -0.01356324068817998940, 0.9999080150203990547 ) ) ;
#14295 = ORIENTED_EDGE ( 'NONE', *, *, #24301, .F. ) ;
#14296 = CARTESIAN_POINT ( 'NONE',  ( -37.00000000000000711, 0.000000000000000000, 0.000000000000000000 ) ) ;
#14297 = ORIENTED_EDGE ( 'NONE', *, *, #33691, .F. ) ;
#14298 = EDGE_LOOP ( 'NONE', ( #43207, #30554, #50458, #26483 ) ) ;
#14299 = ORIENTED_EDGE ( 'NONE', *, *, #44678, .F. ) ;
#14300 = CARTESIAN_POINT ( 'NONE',  ( 0.2648978790185602672, 11.55204314799263798, 4.063980959785085112 ) ) ;
#14301 = DIRECTION ( 'NONE',  ( -1.000000000000000000, 0.000000000000000000, 0.000000000000000000 ) ) ;
#14302 = EDGE_CURVE ( 'NONE', #12134, #47920, #55596, .T. ) ;
#14303 = VECTOR ( 'NONE', #37380, 1000.000000000000000 ) ;
#14304 = CARTESIAN_POINT ( 'NONE',  ( 0.000000000000000000, -4.962980376314023445, -4.846014654777856201 ) ) ;
#14305 = CARTESIAN_POINT ( 'NONE',  ( 0.6511581176963763262, -0.3309006379877175164, 12.37037447926123868 ) ) ;
#14306 = EDGE_LOOP ( 'NONE', ( #60231, #6402, #27430, #18965 ) ) ;
#14307 = CARTESIAN_POINT ( 'NONE',  ( 2.276198483117257698, -7.130755363255148360, -2.759333101207220196 ) ) ;
#14308 = VERTEX_POINT ( 'NONE', #10625 ) ;
#14309 = ADVANCED_FACE ( 'NONE', ( #29678 ), #4104, .T. ) ;
#14310 = DIRECTION ( 'NONE',  ( -0.000000000000000000, -0.000000000000000000, -1.000000000000000000 ) ) ;
#14311 = CYLINDRICAL_SURFACE ( 'NONE', #27726, 5.000000000000000888 ) ;
#14312 = CIRCLE ( 'NONE', #52559, 4.999999999999999112 ) ;
#14313 = ORIENTED_EDGE ( 'NONE', *, *, #47247, .T. ) ;
#14314 = CARTESIAN_POINT ( 'NONE',  ( 1.109979610372471059, 9.898186741523009147, -7.679283534372109976 ) ) ;
#14315 = FACE_OUTER_BOUND ( 'NONE', #47675, .T. ) ;
#14316 = LINE ( 'NONE', #35246, #25958 ) ;
#14317 = ORIENTED_EDGE ( 'NONE', *, *, #24848, .T. ) ;
#14318 = EDGE_CURVE ( 'NONE', #56626, #15788, #3429, .T. ) ;
#14319 = EDGE_LOOP ( 'NONE', ( #36363, #58750, #19588, #6197 ) ) ;
#14320 = CARTESIAN_POINT ( 'NONE',  ( 1.104777566491138563, 6.672212870706200505, 10.60111489796736350 ) ) ;
#14321 = ORIENTED_EDGE ( 'NONE', *, *, #62553, .F. ) ;
#14322 = EDGE_CURVE ( 'NONE', #51071, #24932, #36893, .T. ) ;
#14323 = CYLINDRICAL_SURFACE ( 'NONE', #37003, 6.511478057721953761 ) ;
#14324 = DIRECTION ( 'NONE',  ( 0.000000000000000000, -0.01356324068817998940, 0.9999080150203990547 ) ) ;
#14325 = DIRECTION ( 'NONE',  ( -1.000000000000000000, 0.000000000000000000, 0.000000000000000000 ) ) ;
#14326 = CARTESIAN_POINT ( 'NONE',  ( -3.311295734053511630, 10.53467347881536398, 5.749784130745220878 ) ) ;
#14327 = EDGE_CURVE ( 'NONE', #49219, #34799, #41601, .T. ) ;
#14328 = CARTESIAN_POINT ( 'NONE',  ( 13.37455928674113714, 10.48515777575467744, -5.840559289581060298 ) ) ;
#14329 = AXIS2_PLACEMENT_3D ( 'NONE', #30267, #15297, #5007 ) ;
#14330 = EDGE_LOOP ( 'NONE', ( #2930, #33113, #65798, #7941 ) ) ;
#14331 = DIRECTION ( 'NONE',  ( 1.000000000000000000, -0.000000000000000000, 0.000000000000000000 ) ) ;
#14332 = CARTESIAN_POINT ( 'NONE',  ( 0.000000000000000000, -4.472310526050796931, 6.020667617347345235 ) ) ;
#14333 = VECTOR ( 'NONE', #56998, 1000.000000000000000 ) ;
#14334 = CARTESIAN_POINT ( 'NONE',  ( 0.2801149460245161427, -12.09752788490056119, -1.933835447580753319 ) ) ;
#14335 = EDGE_CURVE ( 'NONE', #29968, #48838, #60736, .T. ) ;
#14336 = CARTESIAN_POINT ( 'NONE',  ( 2.931247277082683844, -5.333206743525275684, 5.779735553870076536 ) ) ;
#14337 = EDGE_CURVE ( 'NONE', #12300, #50867, #229, .T. ) ;
#14338 = DIRECTION ( 'NONE',  ( 0.000000000000000000, -0.01356324068817992175, 0.9999080150203990547 ) ) ;
#14339 = DIRECTION ( 'NONE',  ( 0.000000000000000000, -0.2355298848897586506, -0.9718671068226442111 ) ) ;
#14340 = CARTESIAN_POINT ( 'NONE',  ( 0.000000000000000000, 0.000000000000000000, 0.000000000000000000 ) ) ;
#14341 = B_SPLINE_CURVE_WITH_KNOTS ( 'NONE', 3,
 ( #3129, #27074, #17086, #33370, #57332, #53670, #18080, #12739, #2123, #22749, #58665, #63951, #57998, #32042, #53334, #7778, #47367, #43662, #52360, #12409, #13088, #62963 ),
 .UNSPECIFIED., .F., .F.,
 ( 4, 3, 3, 3, 3, 3, 3, 4 ),
 ( 1.560799312097622405E-17, 4.455945684386779400E-05, 6.636307477204042159E-05, 8.816671873158962063E-05, 0.0001099660380492628749, 0.0001317545563165329193, 0.0001762613022895090831, 0.0001867992666138409204 ),
 .UNSPECIFIED. ) ;
#14342 = EDGE_CURVE ( 'NONE', #53268, #14064, #18321, .T. ) ;
#14343 = ORIENTED_EDGE ( 'NONE', *, *, #45442, .F. ) ;
#14344 = DIRECTION ( 'NONE',  ( 1.000000000000000000, 0.000000000000000000, 0.000000000000000000 ) ) ;
#14345 = ADVANCED_FACE ( 'NONE', ( #31261 ), #6014, .T. ) ;
#14346 =( BOUNDED_SURFACE ( )  B_SPLINE_SURFACE ( 3, 1, ( 
 ( #26993, #26014 ),
 ( #11357, #21993 ),
 ( #46947, #52607 ),
 ( #36948, #2042 ) ),
 .UNSPECIFIED., .F., .F., .F. ) 
 B_SPLINE_SURFACE_WITH_KNOTS ( ( 4, 4 ),
 ( 2, 2 ),
 ( 0.000000000000000000, 1.000000000000000000 ),
 ( 0.000000000000000000, 1.000000000000000000 ),
 .UNSPECIFIED. ) 
 GEOMETRIC_REPRESENTATION_ITEM ( )  RATIONAL_B_SPLINE_SURFACE ( (
 ( 1.000000000000000000, 1.000000000000000000),
 ( 0.9942764183789327692, 0.8450855930916585379),
 ( 0.9942764183789327692, 0.8450855930916585379),
 ( 1.000000000000000000, 1.000000000000000000) ) ) 
 REPRESENTATION_ITEM ( '' )  SURFACE ( )  );
#14347 = ORIENTED_EDGE ( 'NONE', *, *, #10300, .T. ) ;
#14348 = CARTESIAN_POINT ( 'NONE',  ( 3.152665057734119536, 1.848755561852129858, -7.719888720907784219 ) ) ;
#14349 = CYLINDRICAL_SURFACE ( 'NONE', #14117, 4.000000000000000000 ) ;
#14350 = CYLINDRICAL_SURFACE ( 'NONE', #16229, 4.094603870727468120 ) ;
#14351 = ADVANCED_FACE ( 'NONE', ( #1000 ), #61835, .F. ) ;
#14352 = DIRECTION ( 'NONE',  ( 0.000000000000000000, -6.879075853011489629E-15, 1.000000000000000000 ) ) ;
#14353 = ORIENTED_EDGE ( 'NONE', *, *, #8923, .T. ) ;
#14354 = AXIS2_PLACEMENT_3D ( 'NONE', #51111, #881, #21153 ) ;
#14355 = ORIENTED_EDGE ( 'NONE', *, *, #63485, .F. ) ;
#14356 = ORIENTED_EDGE ( 'NONE', *, *, #53163, .T. ) ;
#14357 = CARTESIAN_POINT ( 'NONE',  ( 2.963017218115628904, 3.051711603120633498, -7.259628195185902300 ) ) ;
#14358 = DIRECTION ( 'NONE',  ( -1.000000000000000000, -0.000000000000000000, -0.000000000000000000 ) ) ;
#14359 = VERTEX_POINT ( 'NONE', #44638 ) ;
#14360 = DIRECTION ( 'NONE',  ( 0.000000000000000000, -0.7196168960969868689, -0.6943713148249562872 ) ) ;
#14361 = DIRECTION ( 'NONE',  ( 0.3865475372811021937, 0.01937500237529058214, -0.9220659470476461061 ) ) ;
#14362 = CARTESIAN_POINT ( 'NONE',  ( 0.3654063281920728601, -9.235228056823977738, 8.093076148786007451 ) ) ;
#14363 = DIRECTION ( 'NONE',  ( -1.000000000000000000, 0.000000000000000000, -0.000000000000000000 ) ) ;
#14364 = EDGE_LOOP ( 'NONE', ( #792, #23636, #44107, #62001 ) ) ;
#14365 = CIRCLE ( 'NONE', #35588, 12.18649999999999878 ) ;
#14366 = LINE ( 'NONE', #49635, #29874 ) ;
#14367 = CARTESIAN_POINT ( 'NONE',  ( 3.194234995343557149, -28.25772741625902640, -13.63608895904094531 ) ) ;
#14368 = CARTESIAN_POINT ( 'NONE',  ( 2.305787727787083519, 7.135468203929983488, 2.774453000917173284 ) ) ;
#14370 = ORIENTED_EDGE ( 'NONE', *, *, #47928, .T. ) ;
#14369 = DIRECTION ( 'NONE',  ( 0.000000000000000000, 0.01356324068817998940, -0.9999080150203990547 ) ) ;
#14371 = CARTESIAN_POINT ( 'NONE',  ( 5.515539859299206427, -0.005751553894234964250, 0.001886660928063870184 ) ) ;
#14372 = ORIENTED_EDGE ( 'NONE', *, *, #26109, .F. ) ;
#14373 = CARTESIAN_POINT ( 'NONE',  ( 0.3109076770649054633, -6.333869442011710760, -10.49874397806412141 ) ) ;
#14374 = ORIENTED_EDGE ( 'NONE', *, *, #45732, .T. ) ;
#14375 = CARTESIAN_POINT ( 'NONE',  ( 2.000000000000001776, 3.152010634611693174, 6.039758645301271933 ) ) ;
#14376 = CARTESIAN_POINT ( 'NONE',  ( 2.941278708680199916, 5.721889327162181793, -2.226055275041733506 ) ) ;
#14377 = VECTOR ( 'NONE', #63844, 1000.000000000000000 ) ;
#14378 = FACE_OUTER_BOUND ( 'NONE', #45594, .T. ) ;
#14379 = DIRECTION ( 'NONE',  ( 0.000000000000000000, -0.9847383929261599445, 0.1740410799127720953 ) ) ;
#14380 = ADVANCED_FACE ( 'NONE', ( #41544 ), #64928, .T. ) ;
#14381 = CARTESIAN_POINT ( 'NONE',  ( -37.00000000000000711, 0.000000000000000000, 0.000000000000000000 ) ) ;
#14382 = CARTESIAN_POINT ( 'NONE',  ( -27.10719052120871098, -0.1538293304135310291, -2.355164825213519109 ) ) ;
#14383 = CARTESIAN_POINT ( 'NONE',  ( 0.2676618633000454883, -4.037335446657164262, -11.56235835488944197 ) ) ;
#14385 = ORIENTED_EDGE ( 'NONE', *, *, #25836, .T. ) ;
#14384 = CARTESIAN_POINT ( 'NONE',  ( 0.2648978790185602672, -0.1321385342561549048, -12.24533305150758267 ) ) ;
#14386 = ORIENTED_EDGE ( 'NONE', *, *, #4648, .F. ) ;
#14387 = CARTESIAN_POINT ( 'NONE',  ( 13.21690730856285434, -12.92645890715633250, -3.899147611715625850 ) ) ;
#14388 = ORIENTED_EDGE ( 'NONE', *, *, #34731, .T. ) ;
#14389 = ORIENTED_EDGE ( 'NONE', *, *, #22013, .T. ) ;
#14390 = EDGE_CURVE ( 'NONE', #60024, #41622, #21618, .T. ) ;
#14391 = CARTESIAN_POINT ( 'NONE',  ( 0.5547464869798243159, 1.842327806480310137, -12.20441397277154572 ) ) ;
#14392 = CARTESIAN_POINT ( 'NONE',  ( -27.08423923533013422, 0.2759775751762021390, 2.274768056034770058 ) ) ;
#14393 = FACE_OUTER_BOUND ( 'NONE', #55912, .T. ) ;
#14394 = DIRECTION ( 'NONE',  ( 0.000000000000000000, 0.01356324068817998940, -0.9999080150203990547 ) ) ;
#14395 = CARTESIAN_POINT ( 'NONE',  ( -22.28350523959501217, 1.580062893038993499, -3.346230442873227684 ) ) ;
#14396 = CARTESIAN_POINT ( 'NONE',  ( 2.297017764049619437, 7.246120070222534792, 2.462009443075805493 ) ) ;
#14397 = CARTESIAN_POINT ( 'NONE',  ( 1.459561108993787659, -11.25243317554921063, -5.767168887069020755 ) ) ;
#14398 = EDGE_LOOP ( 'NONE', ( #5319, #35576, #20039, #37696 ) ) ;
#14399 = CARTESIAN_POINT ( 'NONE',  ( 2.350038591457826342, -7.710465783964407294, -7.305692696276328668 ) ) ;
#14400 = CARTESIAN_POINT ( 'NONE',  ( -37.00000000000000711, 3.645068577060182946, -11.16627499335651130 ) ) ;
#14401 = DIRECTION ( 'NONE',  ( -1.000000000000000000, 0.000000000000000000, 0.000000000000000000 ) ) ;
#14402 = ADVANCED_FACE ( 'NONE', ( #52208 ), #27564, .T. ) ;
#14403 = ORIENTED_EDGE ( 'NONE', *, *, #33201, .T. ) ;
#14404 = AXIS2_PLACEMENT_3D ( 'NONE', #21461, #16785, #2155 ) ;
#14405 = CARTESIAN_POINT ( 'NONE',  ( 43.79915462856099850, -1.187172983101278056, -16.56021102286108970 ) ) ;
#14406 = CARTESIAN_POINT ( 'NONE',  ( -10.90165637463000614, -7.508992741355389633, -11.21895841913464764 ) ) ;
#14407 = CARTESIAN_POINT ( 'NONE',  ( -37.00000000000000711, 0.000000000000000000, 0.000000000000000000 ) ) ;
#14408 = EDGE_LOOP ( 'NONE', ( #30431, #23452, #63766, #33907 ) ) ;
#14409 = LINE ( 'NONE', #25379, #48968 ) ;
#14410 = CARTESIAN_POINT ( 'NONE',  ( 0.3665391374699472626, -11.44911061034389732, 4.447929964102808498 ) ) ;
#14411 = DIRECTION ( 'NONE',  ( -0.3939253465568942625, 0.7103112711423451575, 0.5833358547425114837 ) ) ;
#14412 = B_SPLINE_CURVE_WITH_KNOTS ( 'NONE', 3,
 ( #21278, #42522, #41554, #62821, #37568, #16307, #36584 ),
 .UNSPECIFIED., .F., .F.,
 ( 4, 3, 4 ),
 ( 4.926993459890410048E-15, 0.002398160485434636807, 0.005002426799381711787 ),
 .UNSPECIFIED. ) ;
#14413 = EDGE_CURVE ( 'NONE', #38595, #6117, #43182, .T. ) ;
#14414 = AXIS2_PLACEMENT_3D ( 'NONE', #43011, #16448, #12408 ) ;
#14415 = EDGE_CURVE ( 'NONE', #16341, #11407, #16941, .T. ) ;
#14416 = DIRECTION ( 'NONE',  ( 0.000000000000000000, 0.01356324068817991828, -0.9999080150203990547 ) ) ;
#14417 = DIRECTION ( 'NONE',  ( 1.000000000000000000, -0.000000000000000000, -0.000000000000000000 ) ) ;
#14418 = ORIENTED_EDGE ( 'NONE', *, *, #15174, .F. ) ;
#14419 = DIRECTION ( 'NONE',  ( 0.000000000000000000, 0.01356324068817991828, -0.9999080150203990547 ) ) ;
#14420 = CARTESIAN_POINT ( 'NONE',  ( -22.27709082389155171, 3.541295940224340022, 1.005749854561671652 ) ) ;
#14421 = FACE_OUTER_BOUND ( 'NONE', #62794, .T. ) ;
#14422 = VERTEX_POINT ( 'NONE', #28233 ) ;
#14423 = ADVANCED_FACE ( 'NONE', ( #58500 ), #8776, .T. ) ;
#14424 = CARTESIAN_POINT ( 'NONE',  ( 9.751598139935644838, 1.285911471645831528, 13.44024205703445851 ) ) ;
#14425 = FACE_OUTER_BOUND ( 'NONE', #27055, .T. ) ;
#14426 = ORIENTED_EDGE ( 'NONE', *, *, #61850, .F. ) ;
#14427 = ORIENTED_EDGE ( 'NONE', *, *, #21982, .T. ) ;
#14428 = EDGE_LOOP ( 'NONE', ( #46046, #7699, #64238, #55860 ) ) ;
#14429 = CARTESIAN_POINT ( 'NONE',  ( -22.51237073810381517, -0.2145858836692187410, -4.418556976583602136 ) ) ;
#14430 = VERTEX_POINT ( 'NONE', #37877 ) ;
#14431 = DIRECTION ( 'NONE',  ( 0.000000000000000000, -0.01356324068817998940, 0.9999080150203990547 ) ) ;
#14432 = DIRECTION ( 'NONE',  ( -1.000000000000000000, 0.000000000000000000, 0.000000000000000000 ) ) ;
#14433 = CARTESIAN_POINT ( 'NONE',  ( 0.3053067050349123623, -6.328522421120339914, 10.49978800868458961 ) ) ;
#14434 = DIRECTION ( 'NONE',  ( 1.000000000000000000, 0.000000000000000000, 0.000000000000000000 ) ) ;
#14435 = CARTESIAN_POINT ( 'NONE',  ( -11.25859294448574666, -33.36858074101470351, 11.10377723166772768 ) ) ;
#14437 = ORIENTED_EDGE ( 'NONE', *, *, #5187, .T. ) ;
#14436 = CARTESIAN_POINT ( 'NONE',  ( 2.241352910868908310, -7.633946224498473043, -0.08337961031712197435 ) ) ;
#14438 = DIRECTION ( 'NONE',  ( 0.000000000000000000, 0.8696919319575201479, 0.4935949184179230786 ) ) ;
#14439 = VERTEX_POINT ( 'NONE', #6655 ) ;
#14440 = DIRECTION ( 'NONE',  ( -1.000000000000000000, 0.000000000000000000, 0.000000000000000000 ) ) ;
#14441 = ORIENTED_EDGE ( 'NONE', *, *, #64378, .F. ) ;
#14442 = ORIENTED_EDGE ( 'NONE', *, *, #4830, .F. ) ;
#14443 = CARTESIAN_POINT ( 'NONE',  ( -25.00000000000000355, -30.00000000000000000, -24.00000000000000000 ) ) ;
#14444 = CARTESIAN_POINT ( 'NONE',  ( 16.45277491483706456, -34.41570230176820644, 6.124363151459176535 ) ) ;
#14445 = DIRECTION ( 'NONE',  ( -1.000000000000000000, 0.000000000000000000, 0.000000000000000000 ) ) ;
#14446 = EDGE_CURVE ( 'NONE', #58655, #30420, #57859, .T. ) ;
#14447 = DIRECTION ( 'NONE',  ( 0.000000000000000000, -0.01356324068817998940, 0.9999080150203990547 ) ) ;
#14448 = DIRECTION ( 'NONE',  ( 1.000000000000000000, 0.000000000000000000, 0.000000000000000000 ) ) ;
#14449 = CARTESIAN_POINT ( 'NONE',  ( 2.241352910868910531, 5.901537464758454199, 4.843133558968147234 ) ) ;
#14450 = EDGE_LOOP ( 'NONE', ( #62956, #15305, #10299, #50207 ) ) ;
#14451 = ADVANCED_FACE ( 'NONE', ( #32864 ), #65426, .F. ) ;
#14452 = VECTOR ( 'NONE', #32710, 1000.000000000000114 ) ;
#14453 = EDGE_LOOP ( 'NONE', ( #34253, #63201, #39961, #53814 ) ) ;
#14454 = FACE_OUTER_BOUND ( 'NONE', #21714, .T. ) ;
#14455 = ORIENTED_EDGE ( 'NONE', *, *, #39540, .F. ) ;
#14456 = ORIENTED_EDGE ( 'NONE', *, *, #60256, .T. ) ;
#14457 = EDGE_CURVE ( 'NONE', #45219, #55881, #17614, .T. ) ;
#14458 = CARTESIAN_POINT ( 'NONE',  ( -35.00000000000000000, 4.074242145636004508, 12.08151691381191739 ) ) ;
#14459 = CARTESIAN_POINT ( 'NONE',  ( -22.27719381268171261, 0.9730858478814007340, -3.550654232855434689 ) ) ;
#14460 = B_SPLINE_CURVE_WITH_KNOTS ( 'NONE', 3,
 ( #47023, #33357, #11740, #22058, #7094, #1794, #42315, #2798, #58651, #17067, #28047, #13075, #52346, #62951, #27059, #1478, #27369, #47664, #53655, #22734, #57985, #16742, #26728, #42997 ),
 .UNSPECIFIED., .F., .F.,
 ( 4, 2, 2, 2, 2, 2, 2, 2, 2, 2, 2, 4 ),
 ( 0.000000000000000000, 0.0006693376636140126916, 0.001338675327228025383, 0.002008012990842038183, 0.002677350654456050767, 0.004016025981684075499, 0.004685363645298088950, 0.005354701308912100666, 0.006024038972526111514, 0.006693376636140124097, 0.008032051963368149264, 0.01070940261782419439 ),
 .UNSPECIFIED. ) ;
#14461 = CARTESIAN_POINT ( 'NONE',  ( 17.52955304423989347, 7.823381130471544154, 9.114384484749823656 ) ) ;
#14462 = CARTESIAN_POINT ( 'NONE',  ( 37.00000000000000711, -1.771820996347075017, 11.61175578952787113 ) ) ;
#14463 = CARTESIAN_POINT ( 'NONE',  ( 2.406456491626523420, 7.176027849159630989, 7.573451137021355528 ) ) ;
#14464 = CARTESIAN_POINT ( 'NONE',  ( 27.57023587884935978, -12.80946526384611239, 4.265168728770441398 ) ) ;
#14465 = ORIENTED_EDGE ( 'NONE', *, *, #31502, .T. ) ;
#14466 = VERTEX_POINT ( 'NONE', #62477 ) ;
#14467 = EDGE_CURVE ( 'NONE', #45445, #35395, #48076, .T. ) ;
#14468 = DIRECTION ( 'NONE',  ( 0.000000000000000000, 0.000000000000000000, 1.000000000000000000 ) ) ;
#14469 = EDGE_CURVE ( 'NONE', #18816, #43792, #34130, .T. ) ;
#14470 = CYLINDRICAL_SURFACE ( 'NONE', #56283, 12.18650000000000055 ) ;
#14471 = DIRECTION ( 'NONE',  ( 1.000000000000000000, 0.000000000000000000, 0.000000000000000000 ) ) ;
#14472 = EDGE_CURVE ( 'NONE', #11505, #18081, #34243, .T. ) ;
#14473 = CARTESIAN_POINT ( 'NONE',  ( -35.00000000000000000, -4.309077947445573820, -10.92721691015460550 ) ) ;
#14474 = CARTESIAN_POINT ( 'NONE',  ( 1.719304012339867516, -12.38166659046446938, 2.961219984258617544 ) ) ;
#14475 = DIRECTION ( 'NONE',  ( 0.000000000000000000, 0.01356324068818000848, -0.9999080150203990547 ) ) ;
#14476 = FACE_OUTER_BOUND ( 'NONE', #63131, .T. ) ;
#14477 = CARTESIAN_POINT ( 'NONE',  ( 2.305787727787084407, -5.047606869483016290, -5.756228004061508585 ) ) ;
#14478 = ORIENTED_EDGE ( 'NONE', *, *, #7429, .F. ) ;
#14479 = CARTESIAN_POINT ( 'NONE',  ( 2.000000000000001776, 0.000000000000000000, 0.000000000000000000 ) ) ;
#14480 = DIRECTION ( 'NONE',  ( 1.000000000000000000, 0.000000000000000000, 0.000000000000000000 ) ) ;
#14481 = CARTESIAN_POINT ( 'NONE',  ( 35.00000000000000000, -11.01837265713068525, 6.415447294506815723 ) ) ;
#14482 = AXIS2_PLACEMENT_3D ( 'NONE', #5079, #56252, #10366 ) ;
#14483 = EDGE_CURVE ( 'NONE', #62155, #45280, #2420, .T. ) ;
#14484 = AXIS2_PLACEMENT_3D ( 'NONE', #24033, #50616, #49329 ) ;
#14485 = ADVANCED_FACE ( 'NONE', ( #64131 ), #43847, .T. ) ;
#14486 = CARTESIAN_POINT ( 'NONE',  ( 2.899286259009686617, -6.616268644969667712, -4.231523595108555469 ) ) ;
#14487 = CARTESIAN_POINT ( 'NONE',  ( -18.04458733766117362, -12.91933584589293282, 3.916728392552376370 ) ) ;
#14488 = VERTEX_POINT ( 'NONE', #8272 ) ;
#14489 = CARTESIAN_POINT ( 'NONE',  ( 2.241352910868908310, 7.633946224498473931, -0.08337961031706911386 ) ) ;
#14490 = CARTESIAN_POINT ( 'NONE',  ( 2.573738926104320424, 6.586859681822653911, 4.074516960797377685 ) ) ;
#14491 = CARTESIAN_POINT ( 'NONE',  ( 1.717027338329501829, -31.08339181399450979, -14.39386062070807171 ) ) ;
#14492 = ORIENTED_EDGE ( 'NONE', *, *, #27322, .F. ) ;
#14493 = CARTESIAN_POINT ( 'NONE',  ( 1.020182472821653974, -6.631405022219332146, 10.59341968305508708 ) ) ;
#14494 = CARTESIAN_POINT ( 'NONE',  ( 2.000000000000001776, -5.860254403322033845, 3.474373880649773039 ) ) ;
#14495 = DIRECTION ( 'NONE',  ( 1.000000000000000000, 0.000000000000000000, 0.000000000000000000 ) ) ;
#14496 = DIRECTION ( 'NONE',  ( -1.000000000000000000, -0.000000000000000000, -0.000000000000000000 ) ) ;
#14497 = CARTESIAN_POINT ( 'NONE',  ( 2.406456491625218685, 9.571062220824229527, -4.152987573057118631 ) ) ;
#14498 = B_SPLINE_CURVE_WITH_KNOTS ( 'NONE', 3,
 ( #41846, #10937, #57482, #47188, #52167, #46200, #645, #51840, #61457, #15902, #5976, #62135, #36855, #57155, #1633, #27526 ),
 .UNSPECIFIED., .F., .F.,
 ( 4, 3, 3, 3, 3, 4 ),
 ( 0.000000000000000000, 0.0002999043160757539290, 0.0005998071753051414413, 0.0008997092107375177696, 0.001204458948197544834, 0.001510329163480266142 ),
 .UNSPECIFIED. ) ;
#14499 = CARTESIAN_POINT ( 'NONE',  ( 0.3675815128205894289, 1.872154644482084684, 12.13672785388550679 ) ) ;
#14500 = ORIENTED_EDGE ( 'NONE', *, *, #61374, .F. ) ;
#14501 = CARTESIAN_POINT ( 'NONE',  ( 47.00000000000000711, 4.705694406421931860E-17, -3.469127814946512892E-15 ) ) ;
#14502 = CARTESIAN_POINT ( 'NONE',  ( -27.10128162969832744, 1.304299867634929999, 1.945744751330081179 ) ) ;
#14503 = DIRECTION ( 'NONE',  ( -1.000000000000000000, 0.000000000000000000, 0.000000000000000000 ) ) ;
#14504 = CARTESIAN_POINT ( 'NONE',  ( 1.020182472824197495, -1.729367949134086979, -12.37761526492820785 ) ) ;
#14505 = CARTESIAN_POINT ( 'NONE',  ( 2.276198483117262583, 7.555081843354708226, -1.175725118478776920 ) ) ;
#14506 = DIRECTION ( 'NONE',  ( -1.000000000000000000, 0.000000000000000000, 0.000000000000000000 ) ) ;
#14507 = CARTESIAN_POINT ( 'NONE',  ( -37.00000000000000711, 0.000000000000000000, 0.000000000000000000 ) ) ;
#14508 = CARTESIAN_POINT ( 'NONE',  ( 2.280717697722506099, 1.173604464352448806, -7.556934756534813502 ) ) ;
#14509 = ORIENTED_EDGE ( 'NONE', *, *, #12386, .T. ) ;
#14510 = EDGE_LOOP ( 'NONE', ( #19040, #50043, #55455, #57184 ) ) ;
#14511 = DIRECTION ( 'NONE',  ( -1.000000000000000000, 0.000000000000000000, 0.000000000000000000 ) ) ;
#14512 = ORIENTED_EDGE ( 'NONE', *, *, #37244, .F. ) ;
#14513 = DIRECTION ( 'NONE',  ( -1.000000000000000000, 0.000000000000000000, -0.000000000000000000 ) ) ;
#14514 = FACE_OUTER_BOUND ( 'NONE', #58902, .T. ) ;
#14515 = VERTEX_POINT ( 'NONE', #34184 ) ;
#14516 = CARTESIAN_POINT ( 'NONE',  ( 35.00000000000000000, -11.91791701451267826, -2.544412758415803388 ) ) ;
#14517 = EDGE_CURVE ( 'NONE', #3037, #38770, #8929, .T. ) ;
#14518 = CARTESIAN_POINT ( 'NONE',  ( 12.70977043081474989, 11.35156634708707379, -3.911303883136926896 ) ) ;
#14519 = CIRCLE ( 'NONE', #5020, 12.74999999999999822 ) ;
#14520 = CARTESIAN_POINT ( 'NONE',  ( 2.242418902652064006, -4.983487297756227896, -5.783980263415513079 ) ) ;
#14521 = ORIENTED_EDGE ( 'NONE', *, *, #60296, .T. ) ;
#14522 = EDGE_LOOP ( 'NONE', ( #17230, #23640, #55225, #43418 ) ) ;
#14523 = CARTESIAN_POINT ( 'NONE',  ( 2.705197763288548884, 0.2797837188787443141, -7.783989928191459740 ) ) ;
#14524 = VERTEX_POINT ( 'NONE', #38864 ) ;
#14525 = AXIS2_PLACEMENT_3D ( 'NONE', #42848, #22241, #53164 ) ;
#14526 = CARTESIAN_POINT ( 'NONE',  ( -27.10307689719060065, 0.5470785519252523432, -2.283215755731191177 ) ) ;
#14527 = ORIENTED_EDGE ( 'NONE', *, *, #9491, .F. ) ;
#14528 = DIRECTION ( 'NONE',  ( -1.000000000000000000, -0.000000000000000000, 0.000000000000000000 ) ) ;
#14529 = CARTESIAN_POINT ( 'NONE',  ( 2.266490820343225465, 7.130860233521887359, -2.750080098241445725 ) ) ;
#14531 = EDGE_CURVE ( 'NONE', #21703, #57924, #49189, .T. ) ;
#14530 = CARTESIAN_POINT ( 'NONE',  ( 2.373367633546869193, -3.994744114396135526, 6.557448619657627376 ) ) ;
#14532 = CARTESIAN_POINT ( 'NONE',  ( 2.000000000000001776, 4.976357229393922665, -4.652926418895522609 ) ) ;
#14533 = AXIS2_PLACEMENT_3D ( 'NONE', #12636, #52591, #13315 ) ;
#14534 = DIRECTION ( 'NONE',  ( 0.000000000000000000, 0.01356324068817998940, -0.9999080150203990547 ) ) ;
#14535 = VERTEX_POINT ( 'NONE', #64438 ) ;
#14536 =( BOUNDED_SURFACE ( )  B_SPLINE_SURFACE ( 3, 1, ( 
 ( #39648, #3454 ),
 ( #28363, #3783 ),
 ( #24688, #18412 ),
 ( #14039, #48659 ) ),
 .UNSPECIFIED., .F., .F., .F. ) 
 B_SPLINE_SURFACE_WITH_KNOTS ( ( 4, 4 ),
 ( 2, 2 ),
 ( 0.000000000000000000, 1.000000000000000000 ),
 ( 0.000000000000000000, 1.000000000000000000 ),
 .UNSPECIFIED. ) 
 GEOMETRIC_REPRESENTATION_ITEM ( )  RATIONAL_B_SPLINE_SURFACE ( (
 ( 1.000000000000000000, 1.000000000000000000),
 ( 0.6933888150995267674, 0.9895912004443193632),
 ( 0.6933888150995267674, 0.9895912004443193632),
 ( 1.000000000000000000, 1.000000000000000000) ) ) 
 REPRESENTATION_ITEM ( '' )  SURFACE ( )  );
#14537 = CARTESIAN_POINT ( 'NONE',  ( 1.634816307076173425, -12.16351623921533331, 3.661851000130821099 ) ) ;
#14538 = CARTESIAN_POINT ( 'NONE',  ( 1.719304012341412724, 2.961219984259706450, -12.38166659046466300 ) ) ;
#14539 = DIRECTION ( 'NONE',  ( 0.000000000000000000, 0.1387779952735747890, -0.9903235168508558450 ) ) ;
#14540 = EDGE_CURVE ( 'NONE', #36604, #33098, #57954, .T. ) ;
#14541 = CARTESIAN_POINT ( 'NONE',  ( -22.28506771379528573, -3.091577134491930057, 2.081613609299069800 ) ) ;
#14542 = DIRECTION ( 'NONE',  ( 1.000000000000000000, 0.000000000000000000, 0.000000000000000000 ) ) ;
#14543 = CARTESIAN_POINT ( 'NONE',  ( 23.57283587138365988, 1.992978007930514606, 13.35506794274939857 ) ) ;
#14544 = CARTESIAN_POINT ( 'NONE',  ( -27.20102706715912788, 2.585824624629304402, 0.5453431011644924720 ) ) ;
#14545 = CARTESIAN_POINT ( 'NONE',  ( 37.00000000000000711, -8.830544224263011444, -9.196955404009264257 ) ) ;
#14546 = DIRECTION ( 'NONE',  ( 0.000000000000000000, 0.9999080150203990547, 0.01356324068817645230 ) ) ;
#14547 = EDGE_CURVE ( 'NONE', #43973, #56447, #13521, .T. ) ;
#14548 = EDGE_CURVE ( 'NONE', #14197, #4304, #42858, .T. ) ;
#14549 = ORIENTED_EDGE ( 'NONE', *, *, #25978, .T. ) ;
#14550 = CARTESIAN_POINT ( 'NONE',  ( -18.58686583997218378, 5.151216734910788908, -10.83812558286602012 ) ) ;
#14551 = VERTEX_POINT ( 'NONE', #3951 ) ;
#14552 = CARTESIAN_POINT ( 'NONE',  ( -3.518363822661491280, -9.894611242992905176, 6.801870020365760716 ) ) ;
#14553 = CARTESIAN_POINT ( 'NONE',  ( 0.000000000000000000, 6.164400007374783108, 2.900694413976516728 ) ) ;
#14554 = CARTESIAN_POINT ( 'NONE',  ( 1.719304012338836563, -2.961219984258077087, 12.38166659046417095 ) ) ;
#14555 = DIRECTION ( 'NONE',  ( 0.000000000000000000, 0.000000000000000000, -1.000000000000000000 ) ) ;
#14556 = CARTESIAN_POINT ( 'NONE',  ( 2.844750968616409637, 5.286885609675039177, 5.783165144077036857 ) ) ;
#14557 = ORIENTED_EDGE ( 'NONE', *, *, #57749, .T. ) ;
#14558 = CARTESIAN_POINT ( 'NONE',  ( -11.34824676872795379, -8.373158424984243453, -10.59295273223004585 ) ) ;
#14559 = CARTESIAN_POINT ( 'NONE',  ( 2.000000000000001776, -4.472310526050796931, 6.020667617347345235 ) ) ;
#14560 = CARTESIAN_POINT ( 'NONE',  ( -27.09252613521594455, 2.086468883257836193, 1.005681546875630383 ) ) ;
#14561 = CARTESIAN_POINT ( 'NONE',  ( 0.5547464869798239828, 2.442933571354971356, 12.09851097165510403 ) ) ;
#14562 = B_SPLINE_CURVE_WITH_KNOTS ( 'NONE', 3,
 ( #5962, #56829, #46185, #17881, #7568, #11891, #12881, #27855, #48161, #62427 ),
 .UNSPECIFIED., .F., .F.,
 ( 4, 2, 2, 2, 4 ),
 ( 0.002391677032556851785, 0.003742148321009147044, 0.005092619609461442737, 0.006443090897913736695, 0.007793562186366032388 ),
 .UNSPECIFIED. ) ;
#14563 = EDGE_CURVE ( 'NONE', #50060, #42450, #57624, .T. ) ;
#14564 = CARTESIAN_POINT ( 'NONE',  ( 37.00000000000000711, -4.545979934229326780, 11.30684963584393543 ) ) ;
#14565 = ORIENTED_EDGE ( 'NONE', *, *, #55887, .T. ) ;
#14566 = CARTESIAN_POINT ( 'NONE',  ( 0.2646305136544072623, -6.237419468587151350, 10.53923716745245009 ) ) ;
#14567 = VERTEX_POINT ( 'NONE', #28880 ) ;
#14568 = CARTESIAN_POINT ( 'NONE',  ( 0.3109076770649031873, -0.2359198520040302893, -12.25911371383827841 ) ) ;
#14569 = DIRECTION ( 'NONE',  ( 0.000000000000000000, 0.8515178078024849828, -0.5243256840888592674 ) ) ;
#14570 = CIRCLE ( 'NONE', #37986, 2.899999999999993694 ) ;
#14571 = CARTESIAN_POINT ( 'NONE',  ( 2.827825597296805604, 6.207590800588465463, -6.550135365664023546 ) ) ;
#14572 = CARTESIAN_POINT ( 'NONE',  ( 20.00005080000000035, 5.400000000000000355, 1.000000000000000000 ) ) ;
#14573 = EDGE_CURVE ( 'NONE', #21425, #56181, #53350, .T. ) ;
#14574 = ORIENTED_EDGE ( 'NONE', *, *, #19970, .T. ) ;
#14575 = CIRCLE ( 'NONE', #29448, 12.75000000000000178 ) ;
#14576 = ORIENTED_EDGE ( 'NONE', *, *, #8657, .F. ) ;
#14577 = DIRECTION ( 'NONE',  ( 0.000000000000000000, 0.000000000000000000, 1.000000000000000000 ) ) ;
#14578 = ORIENTED_EDGE ( 'NONE', *, *, #55095, .T. ) ;
#14579 = CARTESIAN_POINT ( 'NONE',  ( 2.406456491626467020, 5.751891873090721141, 8.704497555691622424 ) ) ;
#14580 = CARTESIAN_POINT ( 'NONE',  ( -37.00000000000000711, -10.80631716521663854, -4.603882218679666849 ) ) ;
#14581 = CARTESIAN_POINT ( 'NONE',  ( 2.000000000000001776, -5.450255447309714896, -4.087611905901492371 ) ) ;
#14582 = CARTESIAN_POINT ( 'NONE',  ( -37.00000000000000711, 8.295159312811854591, 8.927548052240926069 ) ) ;
#14583 = CARTESIAN_POINT ( 'NONE',  ( -10.90165637463000614, -7.508992741355389633, -11.21895841913464764 ) ) ;
#14584 = PLANE ( 'NONE',  #31794 ) ;
#14585 = VERTEX_POINT ( 'NONE', #65096 ) ;
#14587 = ORIENTED_EDGE ( 'NONE', *, *, #18549, .F. ) ;
#14586 = CARTESIAN_POINT ( 'NONE',  ( -22.31328051695926007, 0.2528478350594092761, 3.781397440874584071 ) ) ;
#14588 = EDGE_LOOP ( 'NONE', ( #65282, #15086, #33836, #59808 ) ) ;
#14589 = B_SPLINE_CURVE_WITH_KNOTS ( 'NONE', 3,
 ( #33143, #42441, #37144, #58106, #63391, #23171, #47158, #57448, #37482, #7211, #17859, #32152, #27181, #57790, #47793, #52475, #47475, #27836, #2247, #52136, #42788, #63084 ),
 .UNSPECIFIED., .F., .F.,
 ( 4, 3, 3, 3, 3, 3, 3, 4 ),
 ( 1.318988870012550679E-18, 4.449119708436826640E-05, 6.626296329540441862E-05, 8.803456484962596642E-05, 0.0001098060367612799996, 0.0001315774408628507465, 0.0001760698110411156123, 0.0001829697163287818842 ),
 .UNSPECIFIED. ) ;
#14590 = CARTESIAN_POINT ( 'NONE',  ( -37.00000000000000711, 5.865551165831237590, -11.32068061209289134 ) ) ;
#14591 = DIRECTION ( 'NONE',  ( 1.000000000000000000, -0.000000000000000000, -0.000000000000000000 ) ) ;
#14592 = VERTEX_POINT ( 'NONE', #9234 ) ;
#14593 = FACE_OUTER_BOUND ( 'NONE', #26034, .T. ) ;
#14594 = ORIENTED_EDGE ( 'NONE', *, *, #8449, .T. ) ;
#14595 = FACE_OUTER_BOUND ( 'NONE', #28513, .T. ) ;
#14596 = EDGE_CURVE ( 'NONE', #42404, #43631, #56527, .T. ) ;
#14597 = CARTESIAN_POINT ( 'NONE',  ( 6.022218414405385190, -8.808464729627129230, -10.23561391756376260 ) ) ;
#14598 = EDGE_CURVE ( 'NONE', #45277, #22627, #43790, .T. ) ;
#14599 = DIRECTION ( 'NONE',  ( -1.000000000000000000, 0.000000000000000000, 0.000000000000000000 ) ) ;
#14600 = CARTESIAN_POINT ( 'NONE',  ( 1.719304012340731269, -10.22720798541492826, -7.581471372739399861 ) ) ;
#14601 = ORIENTED_EDGE ( 'NONE', *, *, #13163, .F. ) ;
#14602 = ORIENTED_EDGE ( 'NONE', *, *, #38518, .T. ) ;
#14603 = DIRECTION ( 'NONE',  ( 0.000000000000000000, -0.9985334138511243740, 0.05413890858540761075 ) ) ;
#14604 = EDGE_CURVE ( 'NONE', #52645, #34279, #23630, .T. ) ;
#14605 = ORIENTED_EDGE ( 'NONE', *, *, #64698, .F. ) ;
#14606 = CARTESIAN_POINT ( 'NONE',  ( 1.719304012339881282, -12.20344780066076318, 3.626341562669963992 ) ) ;
#14607 = VERTEX_POINT ( 'NONE', #34816 ) ;
#14608 = ORIENTED_EDGE ( 'NONE', *, *, #53276, .F. ) ;
#14609 = VERTEX_POINT ( 'NONE', #55123 ) ;
#14610 = CARTESIAN_POINT ( 'NONE',  ( 0.2651627682582904932, 11.53745347823616285, 4.105539787731750323 ) ) ;
#14611 = CARTESIAN_POINT ( 'NONE',  ( -17.05023968204110929, -34.50000000000000000, -4.356789313881321846 ) ) ;
#14613 = EDGE_CURVE ( 'NONE', #797, #58290, #56566, .T. ) ;
#14612 = CARTESIAN_POINT ( 'NONE',  ( -27.04788180060268843, 2.923150379392654763, -1.373100113388769694 ) ) ;
#14614 = DIRECTION ( 'NONE',  ( -1.000000000000000000, -0.000000000000000000, 0.000000000000000000 ) ) ;
#14615 = ORIENTED_EDGE ( 'NONE', *, *, #2001, .T. ) ;
#14616 = CARTESIAN_POINT ( 'NONE',  ( 1.547277799337432702, 11.29700934613254404, 5.744300480442556811 ) ) ;
#14617 = AXIS2_PLACEMENT_3D ( 'NONE', #16072, #31682, #47650 ) ;
#14618 = ORIENTED_EDGE ( 'NONE', *, *, #29881, .F. ) ;
#14619 = CARTESIAN_POINT ( 'NONE',  ( -35.00000000000000000, 0.000000000000000000, 0.000000000000000000 ) ) ;
#14620 = CARTESIAN_POINT ( 'NONE',  ( -18.01437271360181924, -9.050680068142952450, -10.02063192642447298 ) ) ;
#14621 = ADVANCED_FACE ( 'NONE', ( #10885 ), #909, .T. ) ;
#14622 = ORIENTED_EDGE ( 'NONE', *, *, #61613, .T. ) ;
#14623 = CARTESIAN_POINT ( 'NONE',  ( -27.40895923133352596, 11.32254584181078449, -7.372712543863383594 ) ) ;
#14624 = DIRECTION ( 'NONE',  ( 0.000000000000000000, -0.01356324068817998940, 0.9999080150203990547 ) ) ;
#14625 = DIRECTION ( 'NONE',  ( 0.000000000000000000, -0.01356324068817998940, 0.9999080150203990547 ) ) ;
#14626 = AXIS2_PLACEMENT_3D ( 'NONE', #28711, #2486, #58332 ) ;
#14627 = VERTEX_POINT ( 'NONE', #5250 ) ;
#14628 = CARTESIAN_POINT ( 'NONE',  ( -18.58686583997218378, 5.151216734910788908, 25.00000000000000000 ) ) ;
#14629 = EDGE_CURVE ( 'NONE', #40447, #24291, #54438, .T. ) ;
#14630 = ORIENTED_EDGE ( 'NONE', *, *, #27020, .F. ) ;
#14631 = CARTESIAN_POINT ( 'NONE',  ( -24.80504806300548637, -8.637991458312614057, 10.38113301303026326 ) ) ;
#14632 = CARTESIAN_POINT ( 'NONE',  ( 0.7400311444011733464, 9.726551103566812628, 7.698344902199123041 ) ) ;
#14633 = DIRECTION ( 'NONE',  ( 0.000000000000000000, -0.01356324068817998940, 0.9999080150203990547 ) ) ;
#14634 = CARTESIAN_POINT ( 'NONE',  ( 3.152665057735448251, 0.9030954876725900693, -7.886634106564547331 ) ) ;
#14635 = DIRECTION ( 'NONE',  ( 0.000000000000000000, 0.1387779952735818667, -0.9903235168508549569 ) ) ;
#14636 = VERTEX_POINT ( 'NONE', #55792 ) ;
#14637 = CARTESIAN_POINT ( 'NONE',  ( 35.00000000000000000, 11.53507381115583108, 2.216820770815121744 ) ) ;
#14638 = CARTESIAN_POINT ( 'NONE',  ( 0.5547464869798223175, 5.905377260991372168, -10.83828453080459120 ) ) ;
#14639 = FACE_OUTER_BOUND ( 'NONE', #50299, .T. ) ;
#14640 = DIRECTION ( 'NONE',  ( 1.000000000000000000, 0.000000000000000000, 0.000000000000000000 ) ) ;
#14641 = B_SPLINE_CURVE_WITH_KNOTS ( 'NONE', 3,
 ( #56970, #27031, #118, #31358, #35677, #20398, #5453 ),
 .UNSPECIFIED., .F., .F.,
 ( 4, 3, 4 ),
 ( 0.000000000000000000, 0.001700533616330539505, 0.005002426799371278293 ),
 .UNSPECIFIED. ) ;
#14642 = CARTESIAN_POINT ( 'NONE',  ( 3.152665057735807075, 3.546019893115007537, -7.102135024646828221 ) ) ;
#14643 = CARTESIAN_POINT ( 'NONE',  ( 3.152665057734113319, -5.461013642405577073, 5.761241965769066553 ) ) ;
#14644 = CARTESIAN_POINT ( 'NONE',  ( 2.263328370261525890, -5.944174889971089115, -4.802372801874562391 ) ) ;
#14645 = CYLINDRICAL_SURFACE ( 'NONE', #18762, 12.18650000000000055 ) ;
#14646 = DIRECTION ( 'NONE',  ( -1.000000000000000000, 0.000000000000000000, 0.000000000000000000 ) ) ;
#14647 = AXIS2_PLACEMENT_3D ( 'NONE', #6315, #37547, #26578 ) ;
#14648 = ADVANCED_FACE ( 'NONE', ( #20541 ), #15534, .F. ) ;
#14649 = ORIENTED_EDGE ( 'NONE', *, *, #35354, .F. ) ;
#14650 = CARTESIAN_POINT ( 'NONE',  ( -30.09644976052020482, -2.995659101710075767, 11.64721265447471943 ) ) ;
#14651 = AXIS2_PLACEMENT_3D ( 'NONE', #374, #41566, #55573 ) ;
#14652 = CIRCLE ( 'NONE', #59314, 12.18649999999999878 ) ;
#14653 = VERTEX_POINT ( 'NONE', #4928 ) ;
#14654 = FACE_OUTER_BOUND ( 'NONE', #6370, .T. ) ;
#14655 = DIRECTION ( 'NONE',  ( 1.000000000000000000, 0.000000000000000000, 0.000000000000000000 ) ) ;
#14656 = LINE ( 'NONE', #8074, #10912 ) ;
#14657 = VECTOR ( 'NONE', #51708, 1000.000000000000000 ) ;
#14658 = DIRECTION ( 'NONE',  ( 0.000000000000000000, -0.4380125133594037767, 0.8989688749565126757 ) ) ;
#14659 = ORIENTED_EDGE ( 'NONE', *, *, #20332, .F. ) ;
#14660 = EDGE_LOOP ( 'NONE', ( #3616, #56767, #52327, #58323 ) ) ;
#14661 = AXIS2_PLACEMENT_3D ( 'NONE', #59159, #53840, #29216 ) ;
#14662 = ORIENTED_EDGE ( 'NONE', *, *, #2718, .F. ) ;
#14663 = CARTESIAN_POINT ( 'NONE',  ( 2.507146904658100972, 2.843654641958985430, -7.180414359940920477 ) ) ;
#14664 = CARTESIAN_POINT ( 'NONE',  ( 2.589278595513593739, 3.664724287895330335, -6.829211973730652474 ) ) ;
#14665 = ADVANCED_FACE ( 'NONE', ( #65731 ), #56797, .T. ) ;
#14666 = VERTEX_POINT ( 'NONE', #20201 ) ;
#14667 = DIRECTION ( 'NONE',  ( 1.000000000000000000, 0.000000000000000000, 0.000000000000000000 ) ) ;
#14668 = FACE_OUTER_BOUND ( 'NONE', #37161, .T. ) ;
#14669 = CARTESIAN_POINT ( 'NONE',  ( -19.02967556479643463, -13.50000000000023803, -2.066764320408402454E-13 ) ) ;
#14670 = ORIENTED_EDGE ( 'NONE', *, *, #16909, .F. ) ;
#14671 = DIRECTION ( 'NONE',  ( 1.000000000000000000, 0.000000000000000000, 0.000000000000000000 ) ) ;
#14672 = EDGE_CURVE ( 'NONE', #25281, #43014, #32094, .T. ) ;
#14673 = CARTESIAN_POINT ( 'NONE',  ( -13.72965000697286264, -28.58137455677893612, -12.42479717943305140 ) ) ;
#14674 = DIRECTION ( 'NONE',  ( 0.000000000000000000, 0.01356324068817992175, -0.9999080150203990547 ) ) ;
#14676 = VERTEX_POINT ( 'NONE', #50797 ) ;
#14675 = CARTESIAN_POINT ( 'NONE',  ( 12.10998784662220729, -8.443435280036764468, -8.526922110106905706 ) ) ;
#14677 = CARTESIAN_POINT ( 'NONE',  ( -35.00000000000000000, 12.49688848680887965, -2.527899948230500460 ) ) ;
#14678 = EDGE_CURVE ( 'NONE', #18084, #52024, #8837, .T. ) ;
#14679 = ORIENTED_EDGE ( 'NONE', *, *, #38418, .T. ) ;
#14680 = CARTESIAN_POINT ( 'NONE',  ( 2.889800649504073782, 5.267262008933712991, -3.118861721612510518 ) ) ;
#14681 = ORIENTED_EDGE ( 'NONE', *, *, #54073, .T. ) ;
#14682 = DIRECTION ( 'NONE',  ( -1.000000000000000000, 0.000000000000000000, 0.000000000000000000 ) ) ;
#14683 = CARTESIAN_POINT ( 'NONE',  ( 0.2648978790185619880, 9.465406350830608773, 7.769924372105235122 ) ) ;
#14684 = DIRECTION ( 'NONE',  ( -1.000000000000000000, 0.000000000000000000, -0.000000000000000000 ) ) ;
#14685 = CARTESIAN_POINT ( 'NONE',  ( 2.000000000000001776, -5.457833520448623688, -4.281014542496604847 ) ) ;
#14686 = CARTESIAN_POINT ( 'NONE',  ( -22.27722019117890540, 0.6494988092404053726, 3.623917154020592335 ) ) ;
#14687 = CARTESIAN_POINT ( 'NONE',  ( 0.2648978790185602672, -12.24533305150758267, 0.1321385342561976484 ) ) ;
#14689 = EDGE_CURVE ( 'NONE', #17729, #8204, #50165, .T. ) ;
#14688 = DIRECTION ( 'NONE',  ( 0.000000000000000000, 0.9999080150203989437, 0.01356324068817649567 ) ) ;
#14690 = CARTESIAN_POINT ( 'NONE',  ( -27.09048036756591671, -0.1785511875142926919, -2.303144499688040803 ) ) ;
#14691 = DIRECTION ( 'NONE',  ( -1.000000000000000000, 0.000000000000000000, 0.000000000000000000 ) ) ;
#14693 = ORIENTED_EDGE ( 'NONE', *, *, #52853, .F. ) ;
#14692 = CARTESIAN_POINT ( 'NONE',  ( -35.00000000000000000, -3.287724142101498437, 11.73463472867575064 ) ) ;
#14694 = VERTEX_POINT ( 'NONE', #20859 ) ;
#14695 = CARTESIAN_POINT ( 'NONE',  ( 13.33811086919980582, -12.02507490806326906, -6.151199329268367322 ) ) ;
#14696 = ORIENTED_EDGE ( 'NONE', *, *, #20519, .F. ) ;
#14697 = EDGE_CURVE ( 'NONE', #16833, #1585, #15849, .T. ) ;
#14698 = ORIENTED_EDGE ( 'NONE', *, *, #9278, .F. ) ;
#14699 = CARTESIAN_POINT ( 'NONE',  ( 0.2834382757447995171, 8.029794915379554254, 9.254160138068977304 ) ) ;
#14700 = CARTESIAN_POINT ( 'NONE',  ( 37.00000000000000711, 4.705694406421931860E-17, -3.469127814946512892E-15 ) ) ;
#14701 = CARTESIAN_POINT ( 'NONE',  ( 22.88594695219327235, -4.822122601967141264, 10.98850006195556261 ) ) ;
#14702 = EDGE_CURVE ( 'NONE', #20748, #60151, #822, .T. ) ;
#14703 = CARTESIAN_POINT ( 'NONE',  ( 35.00000000000000000, 4.705694406421931860E-17, -3.469127814946512892E-15 ) ) ;
#14704 = VECTOR ( 'NONE', #42418, 1000.000000000000000 ) ;
#14705 = CARTESIAN_POINT ( 'NONE',  ( 2.259025283526328920, 7.225123487441466708, 2.484282765460346543 ) ) ;
#14706 = CARTESIAN_POINT ( 'NONE',  ( -27.08429572838383947, 0.5764601019426045525, 2.217805374070519253 ) ) ;
#14707 = EDGE_CURVE ( 'NONE', #64752, #52828, #22847, .T. ) ;
#14708 = CIRCLE ( 'NONE', #27488, 5.000000000000000000 ) ;
#14709 = AXIS2_PLACEMENT_3D ( 'NONE', #45050, #55689, #45367 ) ;
#14710 = ORIENTED_EDGE ( 'NONE', *, *, #46809, .T. ) ;
#14711 = CARTESIAN_POINT ( 'NONE',  ( 2.573738926104369718, -6.081632213771414719, 4.796056562246151955 ) ) ;
#14712 = ADVANCED_FACE ( 'NONE', ( #21531 ), #12191, .T. ) ;
#14713 = CYLINDRICAL_SURFACE ( 'NONE', #38760, 7.499999999999988454 ) ;
#14714 = AXIS2_PLACEMENT_3D ( 'NONE', #47297, #1075, #42585 ) ;
#14715 = CARTESIAN_POINT ( 'NONE',  ( -19.47984447937493613, -3.750539801530005768, 12.96855624952674724 ) ) ;
#14716 = ORIENTED_EDGE ( 'NONE', *, *, #25004, .F. ) ;
#14717 = CIRCLE ( 'NONE', #14661, 4.999999999999999112 ) ;
#14718 =( BOUNDED_CURVE ( )  B_SPLINE_CURVE ( 3, ( #48917, #23638, #43913, #43565 ),
 .UNSPECIFIED., .F., .F. ) 
 B_SPLINE_CURVE_WITH_KNOTS ( ( 4, 4 ),
 ( 3.768125045480501978, 3.806565460767492581 ),
 .UNSPECIFIED. ) 
 CURVE ( )  GEOMETRIC_REPRESENTATION_ITEM ( )  RATIONAL_B_SPLINE_CURVE ( ( 1.000000000000000000, 0.9998768649967908484, 0.9998768649967908484, 1.000000000000000000 ) ) 
 REPRESENTATION_ITEM ( '' )  );
#14719 = CARTESIAN_POINT ( 'NONE',  ( 47.77550903397572313, -0.4437794964968695410, 10.34167951973068966 ) ) ;
#14720 = DIRECTION ( 'NONE',  ( 0.000000000000000000, -0.2960891610144378849, -0.9551603052523519599 ) ) ;
#14721 = FACE_OUTER_BOUND ( 'NONE', #63724, .T. ) ;
#14722 = ORIENTED_EDGE ( 'NONE', *, *, #34, .T. ) ;
#14723 = CARTESIAN_POINT ( 'NONE',  ( 2.241311220309555097, 6.657499176698838284, -3.736531646286193276 ) ) ;
#14724 = DIRECTION ( 'NONE',  ( 0.000000000000000000, 0.000000000000000000, 1.000000000000000000 ) ) ;
#14725 = DIRECTION ( 'NONE',  ( 0.000000000000000000, 0.01356324068817998940, -0.9999080150203989437 ) ) ;
#14726 = ADVANCED_FACE ( 'NONE', ( #52114 ), #22168, .T. ) ;
#14727 = EDGE_CURVE ( 'NONE', #58914, #325, #16162, .T. ) ;
#14728 = CIRCLE ( 'NONE', #51941, 5.000000000000000888 ) ;
#14729 = CARTESIAN_POINT ( 'NONE',  ( -37.00000000000000711, 11.65554240571059275, -1.456211999474221086 ) ) ;
#14730 = DIRECTION ( 'NONE',  ( 0.000000000000000000, -0.01356324068817998940, 0.9999080150203990547 ) ) ;
#14731 = ORIENTED_EDGE ( 'NONE', *, *, #64087, .F. ) ;
#14732 = VECTOR ( 'NONE', #56346, 1000.000000000000000 ) ;
#14733 = CARTESIAN_POINT ( 'NONE',  ( -37.00000000000000711, 2.143131898507868297E-16, 1.750000000000000000 ) ) ;
#14734 = CARTESIAN_POINT ( 'NONE',  ( -9.387807931906369419, -8.620866317596876272, -8.357905562734071481 ) ) ;
#14735 = CARTESIAN_POINT ( 'NONE',  ( -22.29978294495153790, 3.598607126810735579, -1.052446240539692601 ) ) ;
#14736 = ORIENTED_EDGE ( 'NONE', *, *, #59154, .T. ) ;
#14737 = CARTESIAN_POINT ( 'NONE',  ( -35.00000000000000000, -1.039216533672986387, 11.70009620280411333 ) ) ;
#14738 = CYLINDRICAL_SURFACE ( 'NONE', #28797, 12.18649999999999878 ) ;
#14739 = ORIENTED_EDGE ( 'NONE', *, *, #23408, .T. ) ;
#14740 = EDGE_CURVE ( 'NONE', #41139, #56080, #16850, .T. ) ;
#14741 = VERTEX_POINT ( 'NONE', #6568 ) ;
#14742 = VERTEX_POINT ( 'NONE', #26836 ) ;
#14743 = AXIS2_PLACEMENT_3D ( 'NONE', #11765, #36400, #57339 ) ;
#14744 = CIRCLE ( 'NONE', #51957, 12.75000000000000178 ) ;
#14745 = EDGE_CURVE ( 'NONE', #53954, #64447, #15114, .T. ) ;
#14746 = ORIENTED_EDGE ( 'NONE', *, *, #56534, .T. ) ;
#14747 = CARTESIAN_POINT ( 'NONE',  ( -35.00000000000000000, 12.18632975068353019, 0.06441628369840693424 ) ) ;
#14748 = LINE ( 'NONE', #9127, #55901 ) ;
#14749 = VECTOR ( 'NONE', #62840, 1000.000000000000114 ) ;
#14750 = DIRECTION ( 'NONE',  ( 0.000000000000000000, -0.01356324068817998940, 0.9999080150203990547 ) ) ;
#14751 = CARTESIAN_POINT ( 'NONE',  ( 0.2653141617321020385, 4.229807441322468442, -11.49253039221378003 ) ) ;
#14752 = CARTESIAN_POINT ( 'NONE',  ( -8.761386526127953545, -26.55543068763903491, 14.32493309394703829 ) ) ;
#14753 = CARTESIAN_POINT ( 'NONE',  ( 24.89813668873049934, -0.9220755465451354604, -13.46995378289207856 ) ) ;
#14755 = VERTEX_POINT ( 'NONE', #41796 ) ;
#14754 = CARTESIAN_POINT ( 'NONE',  ( 1.634816307074677955, 7.601181930721248925, 10.17753964889715235 ) ) ;
#14756 = CYLINDRICAL_SURFACE ( 'NONE', #30954, 12.74999999999999822 ) ;
#14757 = ADVANCED_FACE ( 'NONE', ( #42424 ), #37125, .T. ) ;
#14758 = VERTEX_POINT ( 'NONE', #62392 ) ;
#14759 = VERTEX_POINT ( 'NONE', #57426 ) ;
#14760 = CIRCLE ( 'NONE', #5205, 7.580821595991582562 ) ;
#14761 = EDGE_LOOP ( 'NONE', ( #46192, #48304, #29337, #24691, #28025, #45171, #15252, #51935, #61347, #25500, #1877, #8662, #5342, #28111, #35561, #25902, #2708, #46365, #22507, #20006, #40569, #27039, #13855, #61926, #22606, #37326, #61120, #27770, #5966, #15391, #26276, #30557, #57608, #34496, #18721, #59474, #19731, #51278, #56618, #4099, #30385, #56676, #5664, #18140, #35146, #50716, #29657, #28392, #1707, #30057, #62207, #17054, #29197, #22317, #27279, #55779, #25558, #17830, #52601, #11552, #27359, #38717, #23893, #56233, #27447, #17747, #39532, #22613, #24693, #48718, #52329, #6294, #33414, #1007, #58673, #15041, #9625, #38526, #53139, #58113, #44409, #62349, #29838, #40498, #26679, #29971, #37588, #56237, #55284, #37223, #30755, #17093, #37531, #43530, #61325, #36647, #13654, #8720, #62344, #32461, #64660, #30216, #8761, #24256, #58923, #5677, #41666, #18312, #7953, #43067, #54547, #53567 ) ) ;
#14762 = CARTESIAN_POINT ( 'NONE',  ( -22.29382655386184453, -0.8947172055470686836, 3.622626291186073821 ) ) ;
#14763 = CARTESIAN_POINT ( 'NONE',  ( 17.91771366450749525, -29.71233038866033382, 8.402389056494223851 ) ) ;
#14764 = CARTESIAN_POINT ( 'NONE',  ( 3.100650473569754872, 7.866294126167277412, -0.9283202922944042701 ) ) ;
#14765 = DIRECTION ( 'NONE',  ( 1.000000000000000000, 0.000000000000000000, 0.000000000000000000 ) ) ;
#14766 = DIRECTION ( 'NONE',  ( 1.000000000000000000, -0.000000000000000000, -0.000000000000000000 ) ) ;
#14767 = ORIENTED_EDGE ( 'NONE', *, *, #32039, .F. ) ;
#14768 = ORIENTED_EDGE ( 'NONE', *, *, #2894, .F. ) ;
#14769 = CYLINDRICAL_SURFACE ( 'NONE', #60299, 12.74999999999999822 ) ;
#14770 = ORIENTED_EDGE ( 'NONE', *, *, #44399, .T. ) ;
#14771 = EDGE_CURVE ( 'NONE', #28779, #11257, #16542, .T. ) ;
#14772 = EDGE_CURVE ( 'NONE', #27274, #44068, #47136, .T. ) ;
#14773 = ORIENTED_EDGE ( 'NONE', *, *, #10742, .T. ) ;
#14774 = CARTESIAN_POINT ( 'NONE',  ( 0.9232058338315058954, -3.908895078357600639, 11.84276737136199209 ) ) ;
#14775 = CARTESIAN_POINT ( 'NONE',  ( -22.29195009621226475, 0.8975732442595634186, -3.616122380634906541 ) ) ;
#14776 = CARTESIAN_POINT ( 'NONE',  ( 18.20196009002823345, 5.188642410960312645, 10.83342377252405164 ) ) ;
#14777 = EDGE_CURVE ( 'NONE', #49417, #1896, #39687, .T. ) ;
#14778 = CARTESIAN_POINT ( 'NONE',  ( -22.27711351828769892, 1.028167152775530724, -3.534923377568743419 ) ) ;
#14779 = CARTESIAN_POINT ( 'NONE',  ( 1.948354844647019579, 8.228891433294911906, 8.685970062892966581 ) ) ;
#14780 = CIRCLE ( 'NONE', #2079, 12.74999999999999822 ) ;
#14781 = ADVANCED_FACE ( 'NONE', ( #5817 ), #47019, .T. ) ;
#14782 = FACE_OUTER_BOUND ( 'NONE', #48600, .T. ) ;
#14783 = ORIENTED_EDGE ( 'NONE', *, *, #16713, .F. ) ;
#14784 = CIRCLE ( 'NONE', #27522, 5.000000000000001776 ) ;
#14785 = VERTEX_POINT ( 'NONE', #31690 ) ;
#14786 = EDGE_CURVE ( 'NONE', #35230, #10928, #44878, .T. ) ;
#14787 = CARTESIAN_POINT ( 'NONE',  ( 2.000000000000001776, 0.4129979343797385294, 6.800241778083691457 ) ) ;
#14788 = CARTESIAN_POINT ( 'NONE',  ( 2.259025283528083516, 7.499281868334258583, -1.461109758650477541 ) ) ;
#14789 = CYLINDRICAL_SURFACE ( 'NONE', #61665, 7.499999999999988454 ) ;
#14790 = AXIS2_PLACEMENT_3D ( 'NONE', #36085, #51436, #41406 ) ;
#14791 = DIRECTION ( 'NONE',  ( 0.000000000000000000, 0.8276889981568920085, -0.5611870653623802774 ) ) ;
#14792 = DIRECTION ( 'NONE',  ( 1.000000000000000000, 0.000000000000000000, 0.000000000000000000 ) ) ;
#14793 = AXIS2_PLACEMENT_3D ( 'NONE', #30692, #40024, #24750 ) ;
#14794 = CARTESIAN_POINT ( 'NONE',  ( -7.761246313398307173, -2.161858718264055401, -11.80499000202248894 ) ) ;
#14795 = CARTESIAN_POINT ( 'NONE',  ( 1.000000000000000888, -6.253963800348222968, -4.139799123621093813 ) ) ;
#14796 = CARTESIAN_POINT ( 'NONE',  ( -37.00000000000000711, 0.000000000000000000, 0.000000000000000000 ) ) ;
#14797 = VERTEX_POINT ( 'NONE', #30397 ) ;
#14798 = CARTESIAN_POINT ( 'NONE',  ( 0.2653141334712558197, 10.62748186152497176, 6.084912053827373768 ) ) ;
#14799 = CARTESIAN_POINT ( 'NONE',  ( 37.00000000000000711, 12.16632754454236398, -0.7008968033239244555 ) ) ;
#14800 = FACE_OUTER_BOUND ( 'NONE', #10802, .T. ) ;
#14801 = AXIS2_PLACEMENT_3D ( 'NONE', #35219, #4991, #55522 ) ;
#14802 = EDGE_CURVE ( 'NONE', #21790, #2995, #56405, .T. ) ;
#14803 = CARTESIAN_POINT ( 'NONE',  ( -0.4370662499957438385, -31.03649492335514992, -14.44372008463312795 ) ) ;
#14804 = EDGE_CURVE ( 'NONE', #31156, #47008, #58721, .T. ) ;
#14805 = DIRECTION ( 'NONE',  ( -1.000000000000000000, 0.000000000000000000, -0.000000000000000000 ) ) ;
#14806 = ORIENTED_EDGE ( 'NONE', *, *, #22409, .T. ) ;
#14807 = LINE ( 'NONE', #19515, #55644 ) ;
#14808 = CARTESIAN_POINT ( 'NONE',  ( 5.516018279890452902, 0.004525000489649771626, 0.005042957932158598396 ) ) ;
#14809 = CARTESIAN_POINT ( 'NONE',  ( 10.57252189908326301, -33.12087690403964046, -11.56547414815872088 ) ) ;
#14810 = EDGE_LOOP ( 'NONE', ( #42926, #11438, #5955, #34561 ) ) ;
#14811 = CARTESIAN_POINT ( 'NONE',  ( 1.109979610369611347, -6.674783385104200661, 10.60154531817194368 ) ) ;
#14812 = DIRECTION ( 'NONE',  ( 0.000000000000000000, 0.01356324068817998940, -0.9999080150203990547 ) ) ;
#14813 = CARTESIAN_POINT ( 'NONE',  ( 0.2655924914740778187, -12.24627751708824341, -0.04405032194315980365 ) ) ;
#14814 = EDGE_CURVE ( 'NONE', #12988, #21262, #51365, .T. ) ;
#14816 = ORIENTED_EDGE ( 'NONE', *, *, #23504, .F. ) ;
#14815 = CARTESIAN_POINT ( 'NONE',  ( 0.2648321136542693410, -7.979621084888171900, 9.289286523730396539 ) ) ;
#14817 = CARTESIAN_POINT ( 'NONE',  ( 0.000000000000000000, 3.795144977083718008, -6.468916029978776017 ) ) ;
#14818 = CIRCLE ( 'NONE', #29739, 2.899999999999996803 ) ;
#14819 = VECTOR ( 'NONE', #26503, 1000.000000000000000 ) ;
#14820 = DIRECTION ( 'NONE',  ( 0.000000000000000000, 0.01356324068817998940, -0.9999080150203990547 ) ) ;
#14821 = ORIENTED_EDGE ( 'NONE', *, *, #28810, .T. ) ;
#14822 = DIRECTION ( 'NONE',  ( 0.000000000000000000, -0.9246979985058680906, -0.3807014730195321661 ) ) ;
#14823 = CARTESIAN_POINT ( 'NONE',  ( -35.00000000000000000, -12.31350058095525668, 3.307597835713200762 ) ) ;
#14824 = DIRECTION ( 'NONE',  ( 0.000000000000000000, 0.000000000000000000, 1.000000000000000000 ) ) ;
#14825 = CARTESIAN_POINT ( 'NONE',  ( -35.00000000000000000, -10.91072401419407001, -5.428340790341820821 ) ) ;
#14827 = CARTESIAN_POINT ( 'NONE',  ( -35.04709527796842394, -0.005220632201001842998, -0.01120703303053409428 ) ) ;
#14826 = CIRCLE ( 'NONE', #46708, 2.899999999999995026 ) ;
#14828 = CARTESIAN_POINT ( 'NONE',  ( 35.00000000000000000, 0.3025107581131208367, -11.74226168163341555 ) ) ;
#14829 = DIRECTION ( 'NONE',  ( 1.000000000000000000, -0.000000000000000000, 0.000000000000000000 ) ) ;
#14830 = EDGE_CURVE ( 'NONE', #5000, #47037, #26080, .T. ) ;
#14831 = ORIENTED_EDGE ( 'NONE', *, *, #17708, .F. ) ;
#14832 = DIRECTION ( 'NONE',  ( 1.000000000000000000, -0.000000000000000000, 0.000000000000000000 ) ) ;
#14833 = ORIENTED_EDGE ( 'NONE', *, *, #9479, .F. ) ;
#14834 = EDGE_CURVE ( 'NONE', #29699, #25796, #61871, .T. ) ;
#14835 = AXIS2_PLACEMENT_3D ( 'NONE', #62439, #6287, #46837 ) ;
#14836 = CARTESIAN_POINT ( 'NONE',  ( 0.3401186441510198888, 11.44115600261391386, 4.436257390736866313 ) ) ;
#14837 = CARTESIAN_POINT ( 'NONE',  ( -22.27706485742869091, -3.563814065926672381, 0.9221835209182321913 ) ) ;
#14839 = ORIENTED_EDGE ( 'NONE', *, *, #56669, .F. ) ;
#14838 = AXIS2_PLACEMENT_3D ( 'NONE', #43805, #19842, #14820 ) ;
#14840 = CARTESIAN_POINT ( 'NONE',  ( -32.16141091265169649, 25.00000000000000000, 5.384978440493686236 ) ) ;
#14841 = DIRECTION ( 'NONE',  ( 1.000000000000000000, 0.000000000000000000, 0.000000000000000000 ) ) ;
#14842 = CYLINDRICAL_SURFACE ( 'NONE', #10643, 4.999999999999999112 ) ;
#14843 = ORIENTED_EDGE ( 'NONE', *, *, #5304, .F. ) ;
#14844 = ORIENTED_EDGE ( 'NONE', *, *, #26557, .F. ) ;
#14845 = CARTESIAN_POINT ( 'NONE',  ( -2.532614230583022152, 25.00000000000000000, 4.026315189028233377 ) ) ;
#14846 = ORIENTED_EDGE ( 'NONE', *, *, #54746, .F. ) ;
#14847 = CIRCLE ( 'NONE', #52053, 7.499999999999988454 ) ;
#14848 = CARTESIAN_POINT ( 'NONE',  ( 0.3665391374699465965, 4.447929964102846689, 11.44911061034387956 ) ) ;
#14849 = ORIENTED_EDGE ( 'NONE', *, *, #38568, .T. ) ;
#14850 = CARTESIAN_POINT ( 'NONE',  ( -27.09861164373156939, 2.328930759213688528, -0.1603819633258264654 ) ) ;
#14851 = ADVANCED_FACE ( 'NONE', ( #55682 ), #11078, .F. ) ;
#14852 = CARTESIAN_POINT ( 'NONE',  ( 2.276905613633651626, 7.130967020394731293, -2.759436818562420068 ) ) ;
#14853 = CARTESIAN_POINT ( 'NONE',  ( 2.994568964204202821, -4.283796412555518351, 6.620406464816379177 ) ) ;
#14854 = CARTESIAN_POINT ( 'NONE',  ( 26.08439714455133185, 25.00000000000000000, 3.743551691817327942 ) ) ;
#14855 = ADVANCED_FACE ( 'NONE', ( #16082 ), #60996, .F. ) ;
#14856 = CARTESIAN_POINT ( 'NONE',  ( 0.3610902822527155553, 11.62472836966323442, 3.951920836718759489 ) ) ;
#14857 = ORIENTED_EDGE ( 'NONE', *, *, #6729, .T. ) ;
#14858 = CARTESIAN_POINT ( 'NONE',  ( 1.287602823386778228, -12.00540336274477049, 3.781900355162060468 ) ) ;
#14859 = EDGE_CURVE ( 'NONE', #2844, #28276, #41704, .T. ) ;
#14860 = DIRECTION ( 'NONE',  ( -1.000000000000000000, 0.000000000000000000, 0.000000000000000000 ) ) ;
#14861 = DIRECTION ( 'NONE',  ( -1.000000000000000000, 0.000000000000000000, 0.000000000000000000 ) ) ;
#14862 = CARTESIAN_POINT ( 'NONE',  ( 35.00000000000000000, 11.30684963584395675, 4.545979934229284147 ) ) ;
#14863 = DIRECTION ( 'NONE',  ( -1.000000000000000000, 0.000000000000000000, 0.000000000000000000 ) ) ;
#14864 = CARTESIAN_POINT ( 'NONE',  ( 37.00000000000000711, 11.78977382767499549, -4.245927698352105928 ) ) ;
#14865 = CARTESIAN_POINT ( 'NONE',  ( -35.00000000000000000, 0.000000000000000000, 0.000000000000000000 ) ) ;
#14866 = CARTESIAN_POINT ( 'NONE',  ( 2.889800649504073782, 3.002151847318916822, 5.334644486274205732 ) ) ;
#14867 = CIRCLE ( 'NONE', #55239, 5.000000000000000888 ) ;
#14869 = ORIENTED_EDGE ( 'NONE', *, *, #7803, .T. ) ;
#14868 = VECTOR ( 'NONE', #15689, 1000.000000000000000 ) ;
#14870 = AXIS2_PLACEMENT_3D ( 'NONE', #60002, #9424, #13763 ) ;
#14871 = CARTESIAN_POINT ( 'NONE',  ( 0.2739690278137263402, 0.1830199730327409235, 12.24770428423990687 ) ) ;
#14872 = VERTEX_POINT ( 'NONE', #15430 ) ;
#14873 = DIRECTION ( 'NONE',  ( 0.000000000000000000, -0.4698238015817428059, -0.8827602140260282226 ) ) ;
#14874 = CARTESIAN_POINT ( 'NONE',  ( -22.28350523959500862, -3.687952016964556545, 0.3047406164877147772 ) ) ;
#14875 = DIRECTION ( 'NONE',  ( -1.000000000000000000, -0.000000000000000000, 0.000000000000000000 ) ) ;
#14876 = DIRECTION ( 'NONE',  ( 0.000000000000000000, 0.000000000000000000, 1.000000000000000000 ) ) ;
#14877 = CARTESIAN_POINT ( 'NONE',  ( 2.259025283527873906, 2.484282765458685649, -7.225123487442588477 ) ) ;
#14878 = EDGE_LOOP ( 'NONE', ( #1105, #6841, #11501, #24933 ) ) ;
#14879 = DIRECTION ( 'NONE',  ( 0.000000000000000000, -0.7381862504171877726, 0.6745969609292743474 ) ) ;
#14880 = CARTESIAN_POINT ( 'NONE',  ( 2.556980015513303783, 2.429125721802597226, -7.348538402679253956 ) ) ;
#14881 = DIRECTION ( 'NONE',  ( 0.000000000000000000, 0.01356324068817998940, -0.9999080150203990547 ) ) ;
#14882 = PLANE ( 'NONE',  #61421 ) ;
#14883 = VECTOR ( 'NONE', #3115, 1000.000000000000000 ) ;
#14884 = TOROIDAL_SURFACE ( 'NONE', #52088, 20.19615242270663558, 3.000000000000000000 ) ;
#14885 = CARTESIAN_POINT ( 'NONE',  ( 29.20115507325780868, -4.760464791327672529, 11.01582872674790892 ) ) ;
#14886 = ADVANCED_FACE ( 'NONE', ( #36370 ), #11421, .F. ) ;
#14887 = DIRECTION ( 'NONE',  ( 0.3939253465568944290, -0.009718094113445955792, 0.9190910618577643465 ) ) ;
#14888 = ORIENTED_EDGE ( 'NONE', *, *, #59857, .F. ) ;
#14889 = CARTESIAN_POINT ( 'NONE',  ( -27.08850691366518504, -0.5697889027520377514, 2.232573186529265730 ) ) ;
#14890 = ORIENTED_EDGE ( 'NONE', *, *, #40699, .F. ) ;
#14891 = CARTESIAN_POINT ( 'NONE',  ( 2.000000000000001776, 6.586971819220337032, 3.586335490831404460 ) ) ;
#14892 = CARTESIAN_POINT ( 'NONE',  ( -23.18047892478188743, -4.338318103648297175, 2.037851053449315941 ) ) ;
#14893 = AXIS2_PLACEMENT_3D ( 'NONE', #47290, #1729, #27302 ) ;
#14894 = B_SPLINE_CURVE_WITH_KNOTS ( 'NONE', 3,
 ( #61481, #45885, #1324, #21599, #35868, #12823, #40893, #984, #53070, #7507, #336, #51215, #56862, #12487, #53419, #58399 ),
 .UNSPECIFIED., .F., .F.,
 ( 4, 3, 3, 3, 3, 4 ),
 ( 6.505213034913026604E-19, 0.0003017745587525245423, 0.0006035491769808726563, 0.0009053241094668157060, 0.001207275924540510614, 0.001510325902534028712 ),
 .UNSPECIFIED. ) ;
#14895 = FACE_OUTER_BOUND ( 'NONE', #36781, .T. ) ;
#14896 = FACE_OUTER_BOUND ( 'NONE', #61294, .T. ) ;
#14897 = VERTEX_POINT ( 'NONE', #490 ) ;
#14898 = VERTEX_POINT ( 'NONE', #31385 ) ;
#14899 = DIRECTION ( 'NONE',  ( 0.000000000000000000, 0.000000000000000000, 1.000000000000000000 ) ) ;
#14900 = VERTEX_POINT ( 'NONE', #5479 ) ;
#14901 = AXIS2_PLACEMENT_3D ( 'NONE', #18587, #59137, #54795 ) ;
#14902 = CARTESIAN_POINT ( 'NONE',  ( 35.00000000000000000, 10.91072401419418014, 5.428340790341585453 ) ) ;
#14903 = CARTESIAN_POINT ( 'NONE',  ( -35.00000000000000000, 1.171570255487447643, 11.68758509253248867 ) ) ;
#14904 = CARTESIAN_POINT ( 'NONE',  ( -22.27711351828769892, -3.534923377568741198, -1.028167152775526283 ) ) ;
#14905 = CARTESIAN_POINT ( 'NONE',  ( -27.08416974970326763, 0.4041872645907068629, 2.255186831366090772 ) ) ;
#14906 = CARTESIAN_POINT ( 'NONE',  ( 0.7400311444011685724, 9.270387619166440274, -8.241979373543562915 ) ) ;
#14907 = CARTESIAN_POINT ( 'NONE',  ( -16.98800322446194855, 2.922502605998049674, 11.63868456991315625 ) ) ;
#14908 = DIRECTION ( 'NONE',  ( -0.9790892447477997917, -0.2034311943119418153, 0.000000000000000000 ) ) ;
#14909 = VERTEX_POINT ( 'NONE', #51687 ) ;
#14910 = AXIS2_PLACEMENT_3D ( 'NONE', #61707, #11183, #52075 ) ;
#14911 = EDGE_CURVE ( 'NONE', #2752, #8369, #24722, .T. ) ;
#14912 =( REPRESENTATION_RELATIONSHIP ('NONE','NONE', #63658, #13953 ) REPRESENTATION_RELATIONSHIP_WITH_TRANSFORMATION ( #37434 )SHAPE_REPRESENTATION_RELATIONSHIP( ) );
#14914 = ORIENTED_EDGE ( 'NONE', *, *, #11070, .F. ) ;
#14913 = CARTESIAN_POINT ( 'NONE',  ( -8.891032880924177206, -11.36194426013948444, -3.860857758255646921 ) ) ;
#14915 = VERTEX_POINT ( 'NONE', #6446 ) ;
#14916 = CARTESIAN_POINT ( 'NONE',  ( 0.7400311444011702378, -2.502569705372887920, -12.14938086789864791 ) ) ;
#14917 = EDGE_CURVE ( 'NONE', #35302, #32743, #3187, .T. ) ;
#14919 = CARTESIAN_POINT ( 'NONE',  ( 2.350038591457882298, 9.502240128959392962, -4.746773736939736921 ) ) ;
#14918 = CONICAL_SURFACE ( 'NONE', #12848, 12.73084802173761787, 0.3217505529694027477 ) ;
#14920 =( GEOMETRIC_REPRESENTATION_CONTEXT ( 3 ) GLOBAL_UNCERTAINTY_ASSIGNED_CONTEXT ( ( #17723 ) ) GLOBAL_UNIT_ASSIGNED_CONTEXT ( ( #56197, #20644, #6023 ) ) REPRESENTATION_CONTEXT ( 'NONE', 'WORKASPACE' ) );
#14921 = AXIS2_PLACEMENT_3D ( 'NONE', #26796, #47424, #2183 ) ;
#14922 = ORIENTED_EDGE ( 'NONE', *, *, #46727, .F. ) ;
#14923 = CARTESIAN_POINT ( 'NONE',  ( -22.31328051695926007, -1.076152733467184985, -3.633840107626963967 ) ) ;
#14924 = EDGE_LOOP ( 'NONE', ( #18348, #45193, #44553, #39138 ) ) ;
#14925 = CARTESIAN_POINT ( 'NONE',  ( -2.812214508280797887, -11.36735472963161087, 3.846083643116571693 ) ) ;
#14926 =( BOUNDED_CURVE ( )  B_SPLINE_CURVE ( 3, ( #25492, #59776, #45783, #24513 ),
 .UNSPECIFIED., .F., .F. ) 
 B_SPLINE_CURVE_WITH_KNOTS ( ( 4, 4 ),
 ( 2.345489028160348877, 2.374682635079008008 ),
 .UNSPECIFIED. ) 
 CURVE ( )  GEOMETRIC_REPRESENTATION_ITEM ( )  RATIONAL_B_SPLINE_CURVE ( ( 1.000000000000000000, 0.9999289790372866138, 0.9999289790372866138, 1.000000000000000000 ) ) 
 REPRESENTATION_ITEM ( '' )  );
#14927 = CARTESIAN_POINT ( 'NONE',  ( 5.530133899448235191, -0.006998616117863498513, -0.01437126147332041734 ) ) ;
#14928 = DIRECTION ( 'NONE',  ( 1.000000000000000000, 0.000000000000000000, -0.000000000000000000 ) ) ;
#14929 = CARTESIAN_POINT ( 'NONE',  ( -27.09833916700227263, -2.268067253344212553, -0.5492787772350189446 ) ) ;
#14930 = EDGE_LOOP ( 'NONE', ( #26889, #8349, #62035, #48732 ) ) ;
#14931 = ORIENTED_EDGE ( 'NONE', *, *, #2146, .T. ) ;
#14932 = DIRECTION ( 'NONE',  ( -1.000000000000000000, 0.000000000000000000, 0.000000000000000000 ) ) ;
#14933 = ORIENTED_EDGE ( 'NONE', *, *, #2267, .T. ) ;
#14934 = CARTESIAN_POINT ( 'NONE',  ( -22.00000000000000711, -20.00000000000000000, 2.449293598294706907E-15 ) ) ;
#14935 = ORIENTED_EDGE ( 'NONE', *, *, #9051, .F. ) ;
#14936 = ORIENTED_EDGE ( 'NONE', *, *, #50923, .F. ) ;
#14937 = ORIENTED_EDGE ( 'NONE', *, *, #33773, .F. ) ;
#14938 = CIRCLE ( 'NONE', #57453, 12.75000000000000178 ) ;
#14939 = CARTESIAN_POINT ( 'NONE',  ( -21.23983773598477498, -7.447593303288433830, 25.00000000000000000 ) ) ;
#14940 = EDGE_CURVE ( 'NONE', #37122, #20190, #47039, .T. ) ;
#14941 = CARTESIAN_POINT ( 'NONE',  ( -2.496508956744591501, -25.79293017570256552, 15.56347233531499086 ) ) ;
#14942 = AXIS2_PLACEMENT_3D ( 'NONE', #33401, #38718, #8790 ) ;
#14943 = DIRECTION ( 'NONE',  ( 0.000000000000000000, 1.000000000000000000, 0.000000000000000000 ) ) ;
#14944 = CARTESIAN_POINT ( 'NONE',  ( 22.61491127797214062, 25.00000000000000000, 9.376349503825034404 ) ) ;
#14945 = DIRECTION ( 'NONE',  ( 0.000000000000000000, 0.000000000000000000, -1.000000000000000000 ) ) ;
#14946 = VERTEX_POINT ( 'NONE', #27693 ) ;
#14947 = AXIS2_PLACEMENT_3D ( 'NONE', #2759, #40745, #61035 ) ;
#14948 = PLANE ( 'NONE',  #23766 ) ;
#14949 = CIRCLE ( 'NONE', #52144, 12.74999999999999822 ) ;
#14950 = ORIENTED_EDGE ( 'NONE', *, *, #62828, .T. ) ;
#14951 = CARTESIAN_POINT ( 'NONE',  ( 37.00000000000000711, 3.827046518385079032, -11.56998259273179386 ) ) ;
#14952 = CARTESIAN_POINT ( 'NONE',  ( -37.00000000000000711, 0.000000000000000000, 0.000000000000000000 ) ) ;
#14953 = AXIS2_PLACEMENT_3D ( 'NONE', #48657, #7407, #17741 ) ;
#14954 = ORIENTED_EDGE ( 'NONE', *, *, #2419, .T. ) ;
#14955 = DIRECTION ( 'NONE',  ( 1.000000000000000000, 0.000000000000000000, 0.000000000000000000 ) ) ;
#14956 = CARTESIAN_POINT ( 'NONE',  ( 2.000000000000001776, -4.915517050588423587, 4.717154614762070430 ) ) ;
#14957 = CIRCLE ( 'NONE', #31950, 6.936499999999989008 ) ;
#14958 = PLANE ( 'NONE',  #17452 ) ;
#14959 = EDGE_CURVE ( 'NONE', #59854, #39489, #18371, .T. ) ;
#14960 = ORIENTED_EDGE ( 'NONE', *, *, #20580, .T. ) ;
#14961 = CARTESIAN_POINT ( 'NONE',  ( 37.00000000000000711, 8.624332853796058629, -9.390600770288022758 ) ) ;
#14962 = CIRCLE ( 'NONE', #30923, 2.899999999999995026 ) ;
#14963 = ORIENTED_EDGE ( 'NONE', *, *, #63632, .T. ) ;
#14964 = LINE ( 'NONE', #15947, #38102 ) ;
#14965 = CARTESIAN_POINT ( 'NONE',  ( 1.014383007554952032, 9.851867765302182889, 7.686901933424183042 ) ) ;
#14966 = CARTESIAN_POINT ( 'NONE',  ( 1.000000000000000888, 0.08317740279942427428, -7.499538753794372070 ) ) ;
#14968 = CIRCLE ( 'NONE', #52169, 12.74999999999999822 ) ;
#14967 = CARTESIAN_POINT ( 'NONE',  ( 2.556980015513417914, 4.067895092073379182, 6.584367695372176144 ) ) ;
#14969 = CARTESIAN_POINT ( 'NONE',  ( 12.95271867950812528, 9.518344588336780987, -7.319468597748340244 ) ) ;
#14970 = ORIENTED_EDGE ( 'NONE', *, *, #17308, .F. ) ;
#14971 = LINE ( 'NONE', #9658, #21798 ) ;
#14972 = CARTESIAN_POINT ( 'NONE',  ( 1.104777566491140783, 5.844728374724420306, -11.07886329447270235 ) ) ;
#14973 = CYLINDRICAL_SURFACE ( 'NONE', #53425, 5.000000000000000888 ) ;
#14974 = CARTESIAN_POINT ( 'NONE',  ( 3.152665057734040488, 0.000000000000000000, 0.000000000000000000 ) ) ;
#14975 = AXIS2_PLACEMENT_3D ( 'NONE', #2517, #22788, #48057 ) ;
#14976 = AXIS2_PLACEMENT_3D ( 'NONE', #46001, #40009, #457 ) ;
#14977 = AXIS2_PLACEMENT_3D ( 'NONE', #15709, #31024, #6418 ) ;
#14978 = ADVANCED_FACE ( 'NONE', ( #7091 ), #42004, .F. ) ;
#14979 = FACE_OUTER_BOUND ( 'NONE', #40892, .T. ) ;
#14980 = DIRECTION ( 'NONE',  ( -1.000000000000000000, 0.000000000000000000, 0.000000000000000000 ) ) ;
#14981 = EDGE_CURVE ( 'NONE', #25930, #54875, #62284, .T. ) ;
#14982 = CARTESIAN_POINT ( 'NONE',  ( -35.04582288351658548, -0.002280196168880422626, 0.01249938581187134620 ) ) ;
#14983 = DIRECTION ( 'NONE',  ( -1.000000000000000000, 0.000000000000000000, -0.000000000000000000 ) ) ;
#14984 = DIRECTION ( 'NONE',  ( 0.000000000000000000, 0.000000000000000000, 1.000000000000000000 ) ) ;
#14985 = VECTOR ( 'NONE', #53738, 1000.000000000000000 ) ;
#14986 = AXIS2_PLACEMENT_3D ( 'NONE', #6682, #21961, #26293 ) ;
#14987 = EDGE_CURVE ( 'NONE', #61588, #22166, #13815, .T. ) ;
#14988 = VERTEX_POINT ( 'NONE', #16738 ) ;
#14989 = CARTESIAN_POINT ( 'NONE',  ( -27.09252613521643127, -1.304094283668831400, -1.914180209342516426 ) ) ;
#14990 = VECTOR ( 'NONE', #43110, 1000.000000000000114 ) ;
#14991 = ORIENTED_EDGE ( 'NONE', *, *, #40687, .T. ) ;
#14992 = CARTESIAN_POINT ( 'NONE',  ( 2.000000000000001776, 6.997684042076903310, 2.698595569414223849 ) ) ;
#14993 = DIRECTION ( 'NONE',  ( 0.000000000000000000, 0.000000000000000000, 1.000000000000000000 ) ) ;
#14994 = DIRECTION ( 'NONE',  ( 0.000000000000000000, 0.6876994588534194319, 0.7259954919231345061 ) ) ;
#14995 = AXIS2_PLACEMENT_3D ( 'NONE', #43992, #3117, #18068 ) ;
#14996 = CARTESIAN_POINT ( 'NONE',  ( 0.3040950598368144520, -0.2511348647276499535, 12.25911170648142878 ) ) ;
#14997 = VERTEX_POINT ( 'NONE', #48345 ) ;
#14998 = EDGE_CURVE ( 'NONE', #23816, #61226, #47221, .T. ) ;
#14999 = AXIS2_PLACEMENT_3D ( 'NONE', #49812, #8919, #15205 ) ;
#15000 = ORIENTED_EDGE ( 'NONE', *, *, #50812, .F. ) ;
#15001 = VERTEX_POINT ( 'NONE', #52342 ) ;
#15002 = CARTESIAN_POINT ( 'NONE',  ( 2.899286259009689282, 3.018334250363182925, -7.250549018622912456 ) ) ;
#15003 = DIRECTION ( 'NONE',  ( 0.3865475372811021382, 0.8598319252293097348, 0.3335716741247277684 ) ) ;
#15004 = ORIENTED_EDGE ( 'NONE', *, *, #41731, .F. ) ;
#15005 =( NAMED_UNIT ( * ) PLANE_ANGLE_UNIT ( ) SI_UNIT ( $, .RADIAN. ) );
#15006 = CARTESIAN_POINT ( 'NONE',  ( -35.00000000000000000, -1.903127969211109383, -11.59095880812010471 ) ) ;
#15007 = CIRCLE ( 'NONE', #52218, 12.18650000000000233 ) ;
#15008 = CARTESIAN_POINT ( 'NONE',  ( 2.827825597296804272, -8.965636292765729820, 1.027532345921656765 ) ) ;
#15009 = ORIENTED_EDGE ( 'NONE', *, *, #17943, .T. ) ;
#15010 = CARTESIAN_POINT ( 'NONE',  ( -22.29290468048228036, 0.2747050847461964262, 3.718584170466863181 ) ) ;
#15011 = CARTESIAN_POINT ( 'NONE',  ( -9.594501343354149725, -32.11802400029404936, -13.11109426626555319 ) ) ;
#15012 = CARTESIAN_POINT ( 'NONE',  ( 5.516018279890452902, 0.005976902763918716562, 0.003191189039764460479 ) ) ;
#15014 = VERTEX_POINT ( 'NONE', #32662 ) ;
#15013 = DIRECTION ( 'NONE',  ( -1.000000000000000000, -0.000000000000000000, -0.000000000000000000 ) ) ;
#15015 = AXIS2_PLACEMENT_3D ( 'NONE', #25272, #61189, #15304 ) ;
#15017 = AXIS2_PLACEMENT_3D ( 'NONE', #11096, #47337, #46660 ) ;
#15016 = DIRECTION ( 'NONE',  ( -1.000000000000000000, -0.000000000000000000, 0.000000000000000000 ) ) ;
#15018 = ORIENTED_EDGE ( 'NONE', *, *, #26511, .F. ) ;
#15019 = CARTESIAN_POINT ( 'NONE',  ( 0.3632410797595255758, -6.365652464380835873, -10.49990774419908490 ) ) ;
#15020 = B_SPLINE_CURVE_WITH_KNOTS ( 'NONE', 3,
 ( #59916, #39279, #59576, #29311, #14009, #54611, #9033, #24316, #44581, #64867, #14336, #9332, #65212, #55233, #39938, #14643 ),
 .UNSPECIFIED., .F., .F.,
 ( 4, 3, 3, 3, 3, 4 ),
 ( 0.000000000000000000, 0.0002176109881720223165, 0.0004352086762394594198, 0.0006528017811446865321, 0.0007615147961451690243, 0.0009453342004947184150 ),
 .UNSPECIFIED. ) ;
#15021 = ORIENTED_EDGE ( 'NONE', *, *, #20628, .F. ) ;
#15022 = CARTESIAN_POINT ( 'NONE',  ( -28.41827485489077532, 3.509237424706437292, -11.47541949982828413 ) ) ;
#15023 = B_SPLINE_CURVE_WITH_KNOTS ( 'NONE', 3,
 ( #3273, #37849, #63429, #28516, #53810, #23884, #18884, #64412, #43472, #44148, #48184, #2638, #63751, #23211, #17898, #48497, #2948, #48823, #22899, #43821, #64101, #18232 ),
 .UNSPECIFIED., .F., .F.,
 ( 4, 3, 3, 3, 3, 3, 3, 4 ),
 ( 6.774311733015938998E-18, 4.455945684386482600E-05, 6.636307477203528518E-05, 8.816671873158391502E-05, 0.0001099660380492575894, 0.0001317545563165268478, 0.0001762613022895026863, 0.0001867992666138357976 ),
 .UNSPECIFIED. ) ;
#15024 = LINE ( 'NONE', #4767, #40438 ) ;
#15025 = DIRECTION ( 'NONE',  ( 1.000000000000000000, 0.000000000000000000, 0.000000000000000000 ) ) ;
#15026 = CARTESIAN_POINT ( 'NONE',  ( 1.633930747252548388, -6.963441708414224607, -10.62371422070959781 ) ) ;
#15027 = DIRECTION ( 'NONE',  ( -1.000000000000000000, 0.000000000000000000, 0.000000000000000000 ) ) ;
#15028 = AXIS2_PLACEMENT_3D ( 'NONE', #36170, #36523, #5964 ) ;
#15029 = VECTOR ( 'NONE', #51945, 1000.000000000000000 ) ;
#15031 = AXIS2_PLACEMENT_3D ( 'NONE', #34043, #29082, #49388 ) ;
#15030 = DIRECTION ( 'NONE',  ( 1.000000000000000000, 0.000000000000000000, 0.000000000000000000 ) ) ;
#15032 = CARTESIAN_POINT ( 'NONE',  ( 2.242418902651940549, 5.783980263416092171, -4.983487297755500478 ) ) ;
#15033 = CARTESIAN_POINT ( 'NONE',  ( -27.08430418657511751, -0.2231435303617161081, -2.280643121250633509 ) ) ;
#15034 = CARTESIAN_POINT ( 'NONE',  ( 0.2648978790185593790, -4.063980959784970537, -11.55204314799267884 ) ) ;
#15036 = EDGE_LOOP ( 'NONE', ( #3928, #22278, #3281, #19029 ) ) ;
#15035 = CARTESIAN_POINT ( 'NONE',  ( 5.978762125391987148, -9.660146724424269138, 9.437723523674879544 ) ) ;
#15037 = CARTESIAN_POINT ( 'NONE',  ( -35.04709527796842394, 0.007030359780627049027, -0.01016988845958279042 ) ) ;
#15038 = ORIENTED_EDGE ( 'NONE', *, *, #17706, .T. ) ;
#15039 = CARTESIAN_POINT ( 'NONE',  ( 13.31844906986379939, -12.79504830355194578, -4.310850366937079237 ) ) ;
#15040 = ORIENTED_EDGE ( 'NONE', *, *, #33257, .T. ) ;
#15041 = ORIENTED_EDGE ( 'NONE', *, *, #2939, .T. ) ;
#15042 = CARTESIAN_POINT ( 'NONE',  ( 0.7400311444011692386, -12.39937114182725253, 0.3548322008126636451 ) ) ;
#15043 = LINE ( 'NONE', #54332, #63374 ) ;
#15044 = CARTESIAN_POINT ( 'NONE',  ( -27.08850691366480490, -2.218359546717756814, 0.6228349286848108290 ) ) ;
#15046 = CIRCLE ( 'NONE', #4487, 15.00000000000000000 ) ;
#15045 = CARTESIAN_POINT ( 'NONE',  ( -22.28482751661422867, 1.587261331312507240, -3.347211412506322148 ) ) ;
#15047 = ADVANCED_FACE ( 'NONE', ( #6782 ), #2106, .T. ) ;
#15048 = AXIS2_PLACEMENT_3D ( 'NONE', #6600, #30854, #61779 ) ;
#15049 = CARTESIAN_POINT ( 'NONE',  ( 37.00000000000000711, -11.60979404548631777, 3.704519465651427534 ) ) ;
#15050 = DIRECTION ( 'NONE',  ( -1.000000000000000000, -0.000000000000000000, -0.000000000000000000 ) ) ;
#15051 = AXIS2_PLACEMENT_3D ( 'NONE', #48781, #23846, #54430 ) ;
#15052 = ORIENTED_EDGE ( 'NONE', *, *, #58682, .F. ) ;
#15053 = DIRECTION ( 'NONE',  ( 0.000000000000000000, 0.7621620551276377942, -0.6473862847818260269 ) ) ;
#15054 = VECTOR ( 'NONE', #21986, 1000.000000000000000 ) ;
#15055 = CYLINDRICAL_SURFACE ( 'NONE', #3758, 12.74999999999999822 ) ;
#15056 = CARTESIAN_POINT ( 'NONE',  ( 0.7446945582509254535, 12.15064199164585546, 2.504154979875858000 ) ) ;
#15057 = ORIENTED_EDGE ( 'NONE', *, *, #27094, .T. ) ;
#15058 = VECTOR ( 'NONE', #62631, 1000.000000000000000 ) ;
#15059 = B_SPLINE_CURVE_WITH_KNOTS ( 'NONE', 3,
 ( #50063, #24792, #40061, #15458, #56019, #60350, #65652, #40386, #30736, #20780 ),
 .UNSPECIFIED., .F., .F.,
 ( 4, 3, 3, 4 ),
 ( 1.517883041479706208E-18, 6.607638129004506501E-05, 9.911389841680592731E-05, 0.0001667630577588618504 ),
 .UNSPECIFIED. ) ;
#15060 = ADVANCED_FACE ( 'NONE', ( #33004 ), #18063, .T. ) ;
#15061 = VECTOR ( 'NONE', #43411, 1000.000000000000000 ) ;
#15062 = CARTESIAN_POINT ( 'NONE',  ( -29.43980975494970309, -3.641506875706030488, 11.43413432115373318 ) ) ;
#15063 = ADVANCED_FACE ( 'NONE', ( #7405 ), #37998, .T. ) ;
#15064 = CARTESIAN_POINT ( 'NONE',  ( -10.85292393035418002, -8.302656004634402009, -10.64777333369827694 ) ) ;
#15065 = CARTESIAN_POINT ( 'NONE',  ( 29.03457606387295087, 25.00000000000000000, 10.97436308512422265 ) ) ;
#15066 = EDGE_CURVE ( 'NONE', #61002, #36996, #28681, .T. ) ;
#15067 = ORIENTED_EDGE ( 'NONE', *, *, #9295, .T. ) ;
#15068 = CARTESIAN_POINT ( 'NONE',  ( 2.255723233588952770, 6.680843247642368254, -3.704537245404970314 ) ) ;
#15069 = DIRECTION ( 'NONE',  ( 0.000000000000000000, -0.01356324068817999114, 0.9999080150203989437 ) ) ;
#15070 = DIRECTION ( 'NONE',  ( 0.000000000000000000, 0.4380125133593974485, -0.8989688749565157844 ) ) ;
#15071 = AXIS2_PLACEMENT_3D ( 'NONE', #37414, #2529, #58043 ) ;
#15072 = AXIS2_PLACEMENT_3D ( 'NONE', #34805, #5582, #25852 ) ;
#15073 = AXIS2_PLACEMENT_3D ( 'NONE', #8936, #43188, #2324 ) ;
#15074 = EDGE_CURVE ( 'NONE', #34975, #48767, #17171, .T. ) ;
#15075 = DIRECTION ( 'NONE',  ( 1.000000000000000000, 0.000000000000000000, 0.000000000000000000 ) ) ;
#15076 = DIRECTION ( 'NONE',  ( -1.000000000000000000, 0.000000000000000000, 0.000000000000000000 ) ) ;
#15077 = VERTEX_POINT ( 'NONE', #48994 ) ;
#15078 = DIRECTION ( 'NONE',  ( 1.000000000000000000, 0.000000000000000000, 0.000000000000000000 ) ) ;
#15079 = EDGE_CURVE ( 'NONE', #22351, #14567, #18226, .T. ) ;
#15080 = CARTESIAN_POINT ( 'NONE',  ( -22.27722022243424149, 3.470949075637794312, 1.227876413014556078 ) ) ;
#15081 = CARTESIAN_POINT ( 'NONE',  ( 35.00000000000000000, 6.917234959366825642, -9.493370459201726064 ) ) ;
#15082 = ORIENTED_EDGE ( 'NONE', *, *, #47164, .T. ) ;
#15083 = LINE ( 'NONE', #49694, #28714 ) ;
#15084 = CARTESIAN_POINT ( 'NONE',  ( -35.00000000000000000, 0.000000000000000000, 0.000000000000000000 ) ) ;
#15085 = ORIENTED_EDGE ( 'NONE', *, *, #7755, .F. ) ;
#15086 = ORIENTED_EDGE ( 'NONE', *, *, #41142, .F. ) ;
#15087 = VERTEX_POINT ( 'NONE', #19041 ) ;
#15088 = CIRCLE ( 'NONE', #49064, 12.18649999999999878 ) ;
#15089 = VERTEX_POINT ( 'NONE', #59282 ) ;
#15090 = EDGE_CURVE ( 'NONE', #63404, #3635, #47982, .T. ) ;
#15091 = DIRECTION ( 'NONE',  ( 0.000000000000000000, -0.01356324068817998940, 0.9999080150203990547 ) ) ;
#15092 = CYLINDRICAL_SURFACE ( 'NONE', #15544, 6.183183579532408380 ) ;
#15093 = CARTESIAN_POINT ( 'NONE',  ( 0.2869720083484325057, -6.306330337780580386, 10.50600528807145118 ) ) ;
#15094 = CARTESIAN_POINT ( 'NONE',  ( -22.65996813707688062, -2.220979297960720800, -4.292955455498900896 ) ) ;
#15095 = DIRECTION ( 'NONE',  ( 0.000000000000000000, -0.8515178078024924213, 0.5243256840888473880 ) ) ;
#15096 = AXIS2_PLACEMENT_3D ( 'NONE', #50624, #15360, #35633 ) ;
#15098 = EDGE_CURVE ( 'NONE', #36353, #29968, #54196, .T. ) ;
#15097 = CARTESIAN_POINT ( 'NONE',  ( -11.75561129372955094, -29.30098385689712970, 6.671426272442088745 ) ) ;
#15099 = CARTESIAN_POINT ( 'NONE',  ( 24.19622822648017646, 1.946907465358852951, -13.36368882268028635 ) ) ;
#15101 = ORIENTED_EDGE ( 'NONE', *, *, #11894, .F. ) ;
#15100 = CARTESIAN_POINT ( 'NONE',  ( 35.00000000000000000, 3.827046518385079032, -11.56998259273179386 ) ) ;
#15102 = FACE_OUTER_BOUND ( 'NONE', #46734, .T. ) ;
#15103 = ORIENTED_EDGE ( 'NONE', *, *, #42335, .T. ) ;
#15104 = DIRECTION ( 'NONE',  ( 1.000000000000000000, 0.000000000000000000, 0.000000000000000000 ) ) ;
#15105 = ORIENTED_EDGE ( 'NONE', *, *, #48826, .T. ) ;
#15106 = ORIENTED_EDGE ( 'NONE', *, *, #60444, .T. ) ;
#15107 = CARTESIAN_POINT ( 'NONE',  ( 0.3002738374340929162, 9.533456882268753318, -7.705051734330175428 ) ) ;
#15108 = CARTESIAN_POINT ( 'NONE',  ( 9.349182579143541005, -29.24123260035452176, 11.20990699596516293 ) ) ;
#15109 = CARTESIAN_POINT ( 'NONE',  ( -27.45775109278351067, 25.00000000000000000, -1.989333891161980894 ) ) ;
#15110 = CARTESIAN_POINT ( 'NONE',  ( 2.770579946183334918, 7.739026583264748460, -1.056759439485493335 ) ) ;
#15111 = CYLINDRICAL_SURFACE ( 'NONE', #40964, 6.936499999999988120 ) ;
#15112 = LINE ( 'NONE', #45376, #60672 ) ;
#15113 = ORIENTED_EDGE ( 'NONE', *, *, #22945, .F. ) ;
#15114 = CIRCLE ( 'NONE', #60785, 12.18650000000000055 ) ;
#15115 = ORIENTED_EDGE ( 'NONE', *, *, #15204, .T. ) ;
#15116 = LINE ( 'NONE', #168, #57137 ) ;
#15117 = ORIENTED_EDGE ( 'NONE', *, *, #40473, .F. ) ;
#15118 = ORIENTED_EDGE ( 'NONE', *, *, #1523, .F. ) ;
#15120 = CIRCLE ( 'NONE', #4562, 2.899999999999995026 ) ;
#15119 = DIRECTION ( 'NONE',  ( -1.000000000000000000, 0.000000000000000000, -0.000000000000000000 ) ) ;
#15121 = LINE ( 'NONE', #33845, #56477 ) ;
#15122 = CARTESIAN_POINT ( 'NONE',  ( -22.28415773361650309, 0.9182279841530148756, -3.586804264761557004 ) ) ;
#15123 = CARTESIAN_POINT ( 'NONE',  ( 18.48387936547513277, 3.702729101149824675, 11.42676336058183217 ) ) ;
#15124 = CARTESIAN_POINT ( 'NONE',  ( 2.241352910868908310, 7.633946224498473931, 0.08337961031706864201 ) ) ;
#15125 = AXIS2_PLACEMENT_3D ( 'NONE', #63888, #33312, #37306 ) ;
#15126 = EDGE_CURVE ( 'NONE', #17960, #12171, #52224, .T. ) ;
#15127 = DIRECTION ( 'NONE',  ( -1.000000000000000000, 0.000000000000000000, 0.000000000000000000 ) ) ;
#15128 = VECTOR ( 'NONE', #15342, 1000.000000000000114 ) ;
#15129 = CARTESIAN_POINT ( 'NONE',  ( -32.00000000000000000, -15.00000000000000000, 0.000000000000000000 ) ) ;
#15130 = ORIENTED_EDGE ( 'NONE', *, *, #26646, .T. ) ;
#15131 =( BOUNDED_SURFACE ( )  B_SPLINE_SURFACE ( 3, 1, ( 
 ( #58457, #49147 ),
 ( #53478, #3913 ),
 ( #23534, #43460 ),
 ( #18870, #18569 ) ),
 .UNSPECIFIED., .F., .F., .F. ) 
 B_SPLINE_SURFACE_WITH_KNOTS ( ( 4, 4 ),
 ( 2, 2 ),
 ( 0.000000000000000000, 1.000000000000000000 ),
 ( 0.000000000000000000, 1.000000000000000000 ),
 .UNSPECIFIED. ) 
 GEOMETRIC_REPRESENTATION_ITEM ( )  RATIONAL_B_SPLINE_SURFACE ( (
 ( 1.000000000000000000, 1.000000000000000000),
 ( 0.6933888150995267674, 0.9895912004443193632),
 ( 0.6933888150995267674, 0.9895912004443193632),
 ( 1.000000000000000000, 1.000000000000000000) ) ) 
 REPRESENTATION_ITEM ( '' )  SURFACE ( )  );
#15132 = ORIENTED_EDGE ( 'NONE', *, *, #39087, .F. ) ;
#15133 = LINE ( 'NONE', #10153, #54049 ) ;
#15134 = FILL_AREA_STYLE_COLOUR ( '', #41459 ) ;
#15135 = ADVANCED_FACE ( 'NONE', ( #38673 ), #58978, .T. ) ;
#15136 = CARTESIAN_POINT ( 'NONE',  ( 37.00000000000000711, -10.43555801961471552, 5.391785509271064925 ) ) ;
#15137 = DIRECTION ( 'NONE',  ( 0.000000000000000000, -0.1740410799127686259, -0.9847383929261604996 ) ) ;
#15138 = EDGE_CURVE ( 'NONE', #62542, #46560, #14036, .T. ) ;
#15139 = CARTESIAN_POINT ( 'NONE',  ( -35.00000000000000000, 9.240395740215735287, -7.251710744571480127 ) ) ;
#15140 = CIRCLE ( 'NONE', #48058, 12.74999999999999822 ) ;
#15141 = CARTESIAN_POINT ( 'NONE',  ( 24.19857423850153566, 0.7091544454727191082, -13.48603582285567271 ) ) ;
#15142 = DIRECTION ( 'NONE',  ( -1.000000000000000000, -0.000000000000000000, 0.000000000000000000 ) ) ;
#15143 = CIRCLE ( 'NONE', #27887, 5.000000000000000000 ) ;
#15144 = CARTESIAN_POINT ( 'NONE',  ( 2.717984159219211104, 6.148373979318834337, 4.788867404453586829 ) ) ;
#15145 = EDGE_CURVE ( 'NONE', #797, #33730, #58590, .T. ) ;
#15146 = ORIENTED_EDGE ( 'NONE', *, *, #4608, .T. ) ;
#15147 = CARTESIAN_POINT ( 'NONE',  ( 2.000000000000001776, -4.409940824963369366, -5.354199675985328533 ) ) ;
#15148 = CARTESIAN_POINT ( 'NONE',  ( 37.00000000000000711, 10.39746860227901060, 7.379373053628750512 ) ) ;
#15149 = CARTESIAN_POINT ( 'NONE',  ( -18.25006854224444908, -9.443202773001939221, 7.404452808139724063 ) ) ;
#15150 = B_SPLINE_CURVE_WITH_KNOTS ( 'NONE', 3,
 ( #41249, #11652, #15973, #1035, #21305, #52246, #6687, #31293, #16972, #17313, #57894, #37246, #26958 ),
 .UNSPECIFIED., .F., .F.,
 ( 4, 3, 3, 3, 4 ),
 ( 2.602085213965210642E-18, 6.607593386745474117E-05, 0.0001321518677373518646, 0.0001982171734706210224, 0.0002642860854759482834 ),
 .UNSPECIFIED. ) ;
#15151 = CARTESIAN_POINT ( 'NONE',  ( -14.08345347784036328, -34.41374607521908757, -8.401505689976490387 ) ) ;
#15152 = FACE_OUTER_BOUND ( 'NONE', #63189, .T. ) ;
#15153 = ORIENTED_EDGE ( 'NONE', *, *, #23759, .F. ) ;
#15154 = DIRECTION ( 'NONE',  ( -1.000000000000000000, -0.000000000000000000, -0.000000000000000000 ) ) ;
#15155 = CARTESIAN_POINT ( 'NONE',  ( 2.507146904658057451, 6.577532285019759506, 4.047319006787481577 ) ) ;
#15156 = EDGE_CURVE ( 'NONE', #24950, #36705, #53999, .T. ) ;
#15157 = CARTESIAN_POINT ( 'NONE',  ( 19.43600575278776788, -28.99999999999999289, -5.424900065531946147 ) ) ;
#15158 = ORIENTED_EDGE ( 'NONE', *, *, #58934, .F. ) ;
#15159 = CARTESIAN_POINT ( 'NONE',  ( -35.00000000000000000, 0.000000000000000000, 0.000000000000000000 ) ) ;
#15160 = DIRECTION ( 'NONE',  ( -1.000000000000000000, 0.000000000000000000, 0.000000000000000000 ) ) ;
#15161 = CARTESIAN_POINT ( 'NONE',  ( 17.27839441901508621, -10.52068335315807524, 5.771933972472480967 ) ) ;
#15162 = EDGE_CURVE ( 'NONE', #27103, #8013, #6550, .T. ) ;
#15163 = AXIS2_PLACEMENT_3D ( 'NONE', #43140, #33171, #42149 ) ;
#15164 = AXIS2_PLACEMENT_3D ( 'NONE', #13861, #34156, #54469 ) ;
#15166 = EDGE_LOOP ( 'NONE', ( #37111, #44033, #47519, #36067 ) ) ;
#15165 = CARTESIAN_POINT ( 'NONE',  ( 0.000000000000000000, 7.414200355365252015, 1.131208685655162638 ) ) ;
#15167 = CARTESIAN_POINT ( 'NONE',  ( -27.09833916700227618, 2.268067253344194345, 0.5492787772349813080 ) ) ;
#15168 = EDGE_CURVE ( 'NONE', #31395, #1816, #14366, .T. ) ;
#15169 = VECTOR ( 'NONE', #11554, 1000.000000000000227 ) ;
#15170 = VECTOR ( 'NONE', #61223, 1000.000000000000000 ) ;
#15171 = CARTESIAN_POINT ( 'NONE',  ( -35.00000000000000000, -11.29812557209474733, -3.213188559034363401 ) ) ;
#15172 = EDGE_CURVE ( 'NONE', #10704, #39168, #18733, .T. ) ;
#15173 = ORIENTED_EDGE ( 'NONE', *, *, #30872, .T. ) ;
#15174 = EDGE_CURVE ( 'NONE', #37272, #29699, #38378, .T. ) ;
#15175 = CARTESIAN_POINT ( 'NONE',  ( 0.3675815128205912052, 7.689697408877274931, 9.574637318041988365 ) ) ;
#15176 = CARTESIAN_POINT ( 'NONE',  ( 37.00000000000000711, 11.73808581813437080, -0.4353888892050498116 ) ) ;
#15177 = CARTESIAN_POINT ( 'NONE',  ( -14.11589373245165469, 8.250315036047107142, -10.68561190601526256 ) ) ;
#15178 = DIRECTION ( 'NONE',  ( 0.000000000000000000, 0.9987865678893277366, -0.04924826701374931254 ) ) ;
#15179 = CARTESIAN_POINT ( 'NONE',  ( 0.2956976708475453908, -11.44006538352183533, -4.397965666276546060 ) ) ;
#15180 = B_SPLINE_CURVE_WITH_KNOTS ( 'NONE', 3,
 ( #65299, #9421, #34387, #64962, #63991, #50018, #14734, #59030, #49056, #13441, #54364, #13760, #3834, #8800, #35013, #64625 ),
 .UNSPECIFIED., .F., .F.,
 ( 4, 2, 2, 2, 2, 2, 2, 4 ),
 ( 4.249187360970369464E-18, 0.002558063192038479913, 0.003837094788057715533, 0.005116126384076951153, 0.006395157980096183303, 0.007674189576115417188, 0.008953221172134649339, 0.01023225276815388322 ),
 .UNSPECIFIED. ) ;
#15181 = CIRCLE ( 'NONE', #6750, 5.000000000000000000 ) ;
#15182 = EDGE_CURVE ( 'NONE', #49437, #5514, #27, .T. ) ;
#15183 = CARTESIAN_POINT ( 'NONE',  ( 2.241352910868908754, 2.689314586382447914, -7.145045428366549878 ) ) ;
#15184 = CARTESIAN_POINT ( 'NONE',  ( 47.00000000000000711, 4.705694406421931860E-17, -3.469127814946512892E-15 ) ) ;
#15185 = ORIENTED_EDGE ( 'NONE', *, *, #51663, .T. ) ;
#15186 = CARTESIAN_POINT ( 'NONE',  ( 1.000000000000000888, 7.248432822490286753, -1.926193556692960440 ) ) ;
#15187 = CIRCLE ( 'NONE', #23704, 5.000000000000000888 ) ;
#15188 = ORIENTED_EDGE ( 'NONE', *, *, #51041, .T. ) ;
#15189 = CARTESIAN_POINT ( 'NONE',  ( 1.000000000000000888, 5.769711778877324448, 4.791703871138532023 ) ) ;
#15190 = CARTESIAN_POINT ( 'NONE',  ( 0.2956976708475421711, 11.44006538352186020, 4.397965666276463459 ) ) ;
#15191 = CYLINDRICAL_SURFACE ( 'NONE', #31932, 12.74999999999999822 ) ;
#15192 = VERTEX_POINT ( 'NONE', #8404 ) ;
#15193 = DIRECTION ( 'NONE',  ( -1.000000000000000000, 0.000000000000000000, -0.000000000000000000 ) ) ;
#15194 = DIRECTION ( 'NONE',  ( 0.000000000000000000, 0.000000000000000000, 1.000000000000000000 ) ) ;
#15195 = FACE_BOUND ( 'NONE', #29578, .T. ) ;
#15196 = ORIENTED_EDGE ( 'NONE', *, *, #45596, .F. ) ;
#15197 = AXIS2_PLACEMENT_3D ( 'NONE', #58076, #7511, #5755 ) ;
#15198 = ORIENTED_EDGE ( 'NONE', *, *, #63346, .T. ) ;
#15199 = CARTESIAN_POINT ( 'NONE',  ( 0.3675815128205912052, -12.27743992903065973, -0.2638082659429707988 ) ) ;
#15200 = ORIENTED_EDGE ( 'NONE', *, *, #55033, .F. ) ;
#15201 = DIRECTION ( 'NONE',  ( -1.000000000000000000, 0.000000000000000000, 0.000000000000000000 ) ) ;
#15202 = CARTESIAN_POINT ( 'NONE',  ( 5.516018279890452902, 0.004180585980734530596, -0.005331956019561480582 ) ) ;
#15203 = CARTESIAN_POINT ( 'NONE',  ( 2.280717697723838366, 7.131299706077064648, -2.762096098144267042 ) ) ;
#15204 = EDGE_CURVE ( 'NONE', #14946, #4245, #60699, .T. ) ;
#15205 = DIRECTION ( 'NONE',  ( 0.000000000000000000, 0.000000000000000000, 1.000000000000000000 ) ) ;
#15206 = CARTESIAN_POINT ( 'NONE',  ( -14.23194138997495273, 7.940651831586622578, 10.91941811743712876 ) ) ;
#15207 = CARTESIAN_POINT ( 'NONE',  ( 37.00000000000000711, -12.15823808070322798, -0.8294751490778934366 ) ) ;
#15208 = EDGE_LOOP ( 'NONE', ( #17630, #30352, #2260, #32898 ) ) ;
#15209 = CARTESIAN_POINT ( 'NONE',  ( 2.276198483117261695, -1.479169956994117241, 7.501576331167729705 ) ) ;
#15210 = CARTESIAN_POINT ( 'NONE',  ( 21.98520202802499668, 11.37898758322522852, -3.828589025987038319 ) ) ;
#15211 = CARTESIAN_POINT ( 'NONE',  ( 3.152665057735716037, -2.258875078500806044, 7.609997527621833235 ) ) ;
#15212 = CARTESIAN_POINT ( 'NONE',  ( 11.03672806164797215, 13.39240040767147555, -1.705299592209642556 ) ) ;
#15213 = CARTESIAN_POINT ( 'NONE',  ( -10.48620311856347875, -9.720786832536937538, 25.00000000000000000 ) ) ;
#15214 = LINE ( 'NONE', #45812, #39354 ) ;
#15215 = CARTESIAN_POINT ( 'NONE',  ( -47.00000000000000711, 0.000000000000000000, 0.000000000000000000 ) ) ;
#15216 = EDGE_CURVE ( 'NONE', #62620, #8491, #42627, .T. ) ;
#15217 = CIRCLE ( 'NONE', #37538, 4.999999999999999112 ) ;
#15218 = DIRECTION ( 'NONE',  ( 1.000000000000000000, 0.000000000000000000, 0.000000000000000000 ) ) ;
#15219 = CIRCLE ( 'NONE', #4621, 2.899999999999996358 ) ;
#15220 = ORIENTED_EDGE ( 'NONE', *, *, #6976, .F. ) ;
#15221 = B_SPLINE_CURVE_WITH_KNOTS ( 'NONE', 3,
 ( #15820, #56403, #31139, #51449, #46429, #874, #21147, #41419, #27779, #48413, #3184, #33432, #32103, #57739, #58054, #52421 ),
 .UNSPECIFIED., .F., .F.,
 ( 4, 3, 3, 3, 3, 4 ),
 ( 0.000000000000000000, 0.0003017745587525252470, 0.0006035491769808760173, 0.0009053241094668197176, 0.001207275924539396922, 0.001510325902531781811 ),
 .UNSPECIFIED. ) ;
#15222 = CARTESIAN_POINT ( 'NONE',  ( -35.00000000000000000, 7.561043153947966999, 9.557269938331581116 ) ) ;
#15223 = B_SPLINE_CURVE_WITH_KNOTS ( 'NONE', 3,
 ( #30902, #22243, #1662, #56871, #31563, #61490 ),
 .UNSPECIFIED., .F., .F.,
 ( 4, 2, 4 ),
 ( 0.0001654224980408431343, 0.0006219428995476530570, 0.001078463301054462817 ),
 .UNSPECIFIED. ) ;
#15224 = ORIENTED_EDGE ( 'NONE', *, *, #29636, .T. ) ;
#15225 = LINE ( 'NONE', #55807, #27512 ) ;
#15226 = LINE ( 'NONE', #61759, #63772 ) ;
#15227 = CARTESIAN_POINT ( 'NONE',  ( -17.13652129973968741, 7.269150443694792685, -11.37692447958999864 ) ) ;
#15228 = AXIS2_PLACEMENT_3D ( 'NONE', #38542, #1678, #33225 ) ;
#15229 = CARTESIAN_POINT ( 'NONE',  ( 2.717984159219388740, -7.719081760284177030, -1.073093837952627361 ) ) ;
#15230 = CARTESIAN_POINT ( 'NONE',  ( 0.000000000000000000, -3.224464355699781848, -6.771471746882029130 ) ) ;
#15231 = ADVANCED_FACE ( 'NONE', ( #4415 ), #49955, .T. ) ;
#15232 = ORIENTED_EDGE ( 'NONE', *, *, #24083, .T. ) ;
#15233 = CIRCLE ( 'NONE', #56649, 12.75000000000000178 ) ;
#15234 = LINE ( 'NONE', #6257, #37776 ) ;
#15235 = DIRECTION ( 'NONE',  ( -1.000000000000000000, 0.000000000000000000, 0.000000000000000000 ) ) ;
#15236 = CARTESIAN_POINT ( 'NONE',  ( -37.00000000000000711, 10.12742074351907817, -7.745827850122903868 ) ) ;
#15237 = CARTESIAN_POINT ( 'NONE',  ( -27.15525204139121840, -0.5628609503965525951, 2.440367606305302139 ) ) ;
#15238 = CIRCLE ( 'NONE', #1450, 5.000000000000000888 ) ;
#15239 = CARTESIAN_POINT ( 'NONE',  ( 10.21737588954345100, 7.427574052226248114, -11.27660933775315755 ) ) ;
#15240 = CARTESIAN_POINT ( 'NONE',  ( -27.28573687977897322, 1.818142657385575900, -2.255103317860381207 ) ) ;
#15241 = ORIENTED_EDGE ( 'NONE', *, *, #11700, .T. ) ;
#15242 = AXIS2_PLACEMENT_3D ( 'NONE', #3296, #23233, #53834 ) ;
#15243 = CARTESIAN_POINT ( 'NONE',  ( 1.937114397841932290, 12.76557247859000555, -1.334979369128294291 ) ) ;
#15244 = ORIENTED_EDGE ( 'NONE', *, *, #11683, .T. ) ;
#15245 = CARTESIAN_POINT ( 'NONE',  ( 0.2651627923886309968, 12.24583724871548540, 0.08809136839520097240 ) ) ;
#15246 = DIRECTION ( 'NONE',  ( 0.000000000000000000, -0.9289767198167871998, -0.3701381553399246682 ) ) ;
#15247 = CARTESIAN_POINT ( 'NONE',  ( 29.22756163550774033, -7.948250717091969619, 9.002011177893463056 ) ) ;
#15248 = EDGE_CURVE ( 'NONE', #28155, #52774, #43693, .T. ) ;
#15249 = CARTESIAN_POINT ( 'NONE',  ( -37.00000000000000711, 11.30684963584389280, 4.545979934229452901 ) ) ;
#15250 = EDGE_CURVE ( 'NONE', #41694, #63262, #41195, .T. ) ;
#15251 = VECTOR ( 'NONE', #62451, 1000.000000000000000 ) ;
#15252 = ORIENTED_EDGE ( 'NONE', *, *, #32394, .F. ) ;
#15253 = ORIENTED_EDGE ( 'NONE', *, *, #24393, .T. ) ;
#15254 = CARTESIAN_POINT ( 'NONE',  ( 0.2646305136544065406, -1.996350543472912076, -12.08286001766537510 ) ) ;
#15255 = ADVANCED_FACE ( 'NONE', ( #10305 ), #35578, .T. ) ;
#15256 = ORIENTED_EDGE ( 'NONE', *, *, #62323, .T. ) ;
#15257 = CARTESIAN_POINT ( 'NONE',  ( 2.249013661412228249, -6.552953334857887668, -3.921976945965406358 ) ) ;
#15258 = CYLINDRICAL_SURFACE ( 'NONE', #47010, 4.285769192180103992 ) ;
#15259 = FACE_OUTER_BOUND ( 'NONE', #4305, .T. ) ;
#15260 = CARTESIAN_POINT ( 'NONE',  ( 37.00000000000000711, -7.379373053628790480, 10.39746860227898395 ) ) ;
#15261 = CARTESIAN_POINT ( 'NONE',  ( 0.4613984246114886667, 9.246873830556006979, -8.128335150814411492 ) ) ;
#15262 = EDGE_CURVE ( 'NONE', #41856, #63348, #49042, .T. ) ;
#15263 = CARTESIAN_POINT ( 'NONE',  ( 0.2646305136544065406, -7.770320294339109424, -9.465888453933038349 ) ) ;
#15264 = CARTESIAN_POINT ( 'NONE',  ( 1.109979610370706027, -12.51859925746133051, -0.4797593171730065165 ) ) ;
#15265 = ORIENTED_EDGE ( 'NONE', *, *, #56521, .F. ) ;
#15266 = AXIS2_PLACEMENT_3D ( 'NONE', #27435, #38066, #1858 ) ;
#15267 = CIRCLE ( 'NONE', #52461, 20.19615242270663558 ) ;
#15268 = CARTESIAN_POINT ( 'NONE',  ( 1.634816307076136122, -11.34285134320839816, 5.718391684266176611 ) ) ;
#15269 = ORIENTED_EDGE ( 'NONE', *, *, #22157, .T. ) ;
#15270 = CARTESIAN_POINT ( 'NONE',  ( 1.948354844646524642, -9.612178954896725358, -7.125078658759304240 ) ) ;
#15271 = AXIS2_PLACEMENT_3D ( 'NONE', #57372, #32080, #21125 ) ;
#15272 = CARTESIAN_POINT ( 'NONE',  ( -27.09252613521594455, 1.914180209340472283, -1.304094283669201770 ) ) ;
#15273 = EDGE_LOOP ( 'NONE', ( #49699, #54346, #7069, #16104 ) ) ;
#15274 = DIRECTION ( 'NONE',  ( -1.000000000000000000, 0.000000000000000000, 0.000000000000000000 ) ) ;
#15275 = ORIENTED_EDGE ( 'NONE', *, *, #39691, .F. ) ;
#15276 = CARTESIAN_POINT ( 'NONE',  ( 37.00000000000000711, 1.463443770872944194, 12.09831040184922024 ) ) ;
#15277 = AXIS2_PLACEMENT_3D ( 'NONE', #5197, #10489, #62036 ) ;
#15278 = FACE_OUTER_BOUND ( 'NONE', #49319, .T. ) ;
#15279 = CARTESIAN_POINT ( 'NONE',  ( 1.000000000000000888, -2.473437528934089524, -7.080403010455012414 ) ) ;
#15280 = CARTESIAN_POINT ( 'NONE',  ( -27.08485414902839494, -2.215517476308469735, -0.5917839443972630065 ) ) ;
#15281 = ORIENTED_EDGE ( 'NONE', *, *, #26804, .F. ) ;
#15282 = CIRCLE ( 'NONE', #60958, 12.75000000000000178 ) ;
#15283 = ORIENTED_EDGE ( 'NONE', *, *, #39709, .F. ) ;
#15284 = DIRECTION ( 'NONE',  ( -1.000000000000000000, 0.000000000000000000, 0.000000000000000000 ) ) ;
#15285 = VERTEX_POINT ( 'NONE', #10624 ) ;
#15286 = CARTESIAN_POINT ( 'NONE',  ( 0.000000000000000000, -1.693411908627144635, -7.306323022404617618 ) ) ;
#15287 = ORIENTED_EDGE ( 'NONE', *, *, #35766, .F. ) ;
#15288 = ORIENTED_EDGE ( 'NONE', *, *, #61312, .F. ) ;
#15289 = ORIENTED_EDGE ( 'NONE', *, *, #56688, .F. ) ;
#15290 = CARTESIAN_POINT ( 'NONE',  ( 2.653899356899400264, -5.782420802795832593, 5.192946150929120819 ) ) ;
#15291 = CIRCLE ( 'NONE', #49310, 5.000000000000000888 ) ;
#15292 = CARTESIAN_POINT ( 'NONE',  ( -12.41459945261391340, -27.32694502519497703, 12.80960016232523024 ) ) ;
#15293 = PRODUCT_RELATED_PRODUCT_CATEGORY ( 'part', '', ( #54612 ) ) ;
#15294 = ADVANCED_FACE ( 'NONE', ( #11302 ), #9993, .T. ) ;
#15295 = DIRECTION ( 'NONE',  ( 1.000000000000000000, 0.000000000000000000, 0.000000000000000000 ) ) ;
#15296 = DIRECTION ( 'NONE',  ( -1.000000000000000000, 0.000000000000000000, 0.000000000000000000 ) ) ;
#15297 = DIRECTION ( 'NONE',  ( -1.000000000000000000, 0.000000000000000000, 0.000000000000000000 ) ) ;
#15298 = ORIENTED_EDGE ( 'NONE', *, *, #23302, .T. ) ;
#15299 = LINE ( 'NONE', #20933, #3562 ) ;
#15300 = EDGE_CURVE ( 'NONE', #26580, #4994, #59656, .T. ) ;
#15301 = VERTEX_POINT ( 'NONE', #51231 ) ;
#15302 = CARTESIAN_POINT ( 'NONE',  ( -37.00000000000000711, -6.102719229070750373, 10.54834585426218041 ) ) ;
#15303 = AXIS2_PLACEMENT_3D ( 'NONE', #44091, #58085, #28461 ) ;
#15304 = DIRECTION ( 'NONE',  ( 0.000000000000000000, 0.01356324068817998940, -0.9999080150203990547 ) ) ;
#15305 = ORIENTED_EDGE ( 'NONE', *, *, #6981, .F. ) ;
#15306 = CARTESIAN_POINT ( 'NONE',  ( 0.3053067050349138056, -10.73055518945191800, 5.928821939311894162 ) ) ;
#15307 = CARTESIAN_POINT ( 'NONE',  ( 5.520433897694421610, 0.01120198501134884658, -0.01006947824912454194 ) ) ;
#15308 = DIRECTION ( 'NONE',  ( 0.9606638835031803270, 0.2762341707520464262, -0.02862840969242635286 ) ) ;
#15309 = ADVANCED_FACE ( 'NONE', ( #30272 ), #31569, .T. ) ;
#15310 = AXIS2_PLACEMENT_3D ( 'NONE', #41630, #46626, #36314 ) ;
#15311 = ORIENTED_EDGE ( 'NONE', *, *, #40086, .T. ) ;
#15312 = DIRECTION ( 'NONE',  ( -1.000000000000000000, -0.000000000000000000, 0.000000000000000000 ) ) ;
#15313 = ORIENTED_EDGE ( 'NONE', *, *, #695, .F. ) ;
#15314 = CARTESIAN_POINT ( 'NONE',  ( 0.2872850955227753134, 10.71476594226533763, 5.944938343726287933 ) ) ;
#15315 = CARTESIAN_POINT ( 'NONE',  ( -6.902482536246134615, -26.23992191484883918, -14.86511077371810963 ) ) ;
#15316 = CARTESIAN_POINT ( 'NONE',  ( -6.997870572558772650, -27.10943569200530590, 15.36011607788394784 ) ) ;
#15317 = CARTESIAN_POINT ( 'NONE',  ( 2.261269890821706596, -3.699080366006974874, -6.685978463721846232 ) ) ;
#15318 = CARTESIAN_POINT ( 'NONE',  ( 2.000000000000001776, 0.000000000000000000, 0.000000000000000000 ) ) ;
#15319 = EDGE_CURVE ( 'NONE', #15877, #4941, #1542, .T. ) ;
#15320 = EDGE_CURVE ( 'NONE', #18772, #52982, #8714, .T. ) ;
#15321 = EDGE_LOOP ( 'NONE', ( #61815, #22539, #27997, #43860 ) ) ;
#15322 = CIRCLE ( 'NONE', #32304, 4.999999999999999112 ) ;
#15323 = DIRECTION ( 'NONE',  ( -1.000000000000000000, 0.000000000000000000, 0.000000000000000000 ) ) ;
#15324 = CYLINDRICAL_SURFACE ( 'NONE', #48247, 12.74999999999999822 ) ;
#15325 = DIRECTION ( 'NONE',  ( 1.000000000000000000, 0.000000000000000000, 0.000000000000000000 ) ) ;
#15326 = CARTESIAN_POINT ( 'NONE',  ( 2.705197763288543999, 3.649695155981514727, 6.881024880055361947 ) ) ;
#15327 = ADVANCED_FACE ( 'NONE', ( #63146 ), #57857, .T. ) ;
#15328 = DIRECTION ( 'NONE',  ( -1.000000000000000000, 0.000000000000000000, 0.000000000000000000 ) ) ;
#15329 = CARTESIAN_POINT ( 'NONE',  ( -22.27218376572352554, 0.3046453028544620634, 3.670373711461409005 ) ) ;
#15330 = CARTESIAN_POINT ( 'NONE',  ( 0.2653141617321010393, -2.169890202573276472, 12.05243138604825148 ) ) ;
#15331 = CARTESIAN_POINT ( 'NONE',  ( 5.516018279890452902, -0.006440244342253015342, -0.002104829434640740401 ) ) ;
#15332 = FACE_OUTER_BOUND ( 'NONE', #16054, .T. ) ;
#15333 = AXIS2_PLACEMENT_3D ( 'NONE', #96, #10080, #24376 ) ;
#15334 = ADVANCED_FACE ( 'NONE', ( #57191 ), #6970, .T. ) ;
#15335 = CIRCLE ( 'NONE', #32318, 4.999999999999999112 ) ;
#15336 = VERTEX_POINT ( 'NONE', #37876 ) ;
#15337 = EDGE_CURVE ( 'NONE', #55606, #5144, #30972, .T. ) ;
#15338 = ORIENTED_EDGE ( 'NONE', *, *, #2808, .F. ) ;
#15340 =( BOUNDED_SURFACE ( )  B_SPLINE_SURFACE ( 3, 1, ( 
 ( #28632, #48937 ),
 ( #9012, #55554 ),
 ( #19658, #55211 ),
 ( #54586, #9997 ) ),
 .UNSPECIFIED., .F., .F., .F. ) 
 B_SPLINE_SURFACE_WITH_KNOTS ( ( 4, 4 ),
 ( 2, 2 ),
 ( 0.000000000000000000, 1.000000000000000000 ),
 ( 0.000000000000000000, 1.000000000000000000 ),
 .UNSPECIFIED. ) 
 GEOMETRIC_REPRESENTATION_ITEM ( )  RATIONAL_B_SPLINE_SURFACE ( (
 ( 1.000000000000000000, 1.000000000000000000),
 ( 0.9942764183789327692, 0.8450855930916585379),
 ( 0.9942764183789327692, 0.8450855930916585379),
 ( 1.000000000000000000, 1.000000000000000000) ) ) 
 REPRESENTATION_ITEM ( '' )  SURFACE ( )  );
#15339 = CARTESIAN_POINT ( 'NONE',  ( -35.00000000000000000, 0.000000000000000000, 0.000000000000000000 ) ) ;
#15341 = CARTESIAN_POINT ( 'NONE',  ( 5.515188684475870851, 0.0005703990286342820910, 0.005320786921497272677 ) ) ;
#15342 = DIRECTION ( 'NONE',  ( -0.9582930651793755139, -0.1972632429577093616, 0.2067888154783157351 ) ) ;
#15343 = CONICAL_SURFACE ( 'NONE', #23859, 7.580821595991582562, 0.3217505529694035249 ) ;
#15344 = DIRECTION ( 'NONE',  ( 1.000000000000000000, 0.000000000000000000, 0.000000000000000000 ) ) ;
#15345 = EDGE_LOOP ( 'NONE', ( #10622, #49239, #5980, #33092 ) ) ;
#15346 = ORIENTED_EDGE ( 'NONE', *, *, #63581, .F. ) ;
#15347 = ORIENTED_EDGE ( 'NONE', *, *, #28909, .F. ) ;
#15348 = CARTESIAN_POINT ( 'NONE',  ( 0.3040950598368144520, 8.072385578287596175, -9.229598020917608281 ) ) ;
#15349 = VECTOR ( 'NONE', #4272, 1000.000000000000000 ) ;
#15350 = CARTESIAN_POINT ( 'NONE',  ( 2.305787727787083519, -6.545285700970500109, -3.971363876084033961 ) ) ;
#15351 = ORIENTED_EDGE ( 'NONE', *, *, #44055, .T. ) ;
#15352 = DIRECTION ( 'NONE',  ( 0.000000000000000000, 0.000000000000000000, 1.000000000000000000 ) ) ;
#15353 = DIRECTION ( 'NONE',  ( 0.000000000000000000, -1.000000000000000000, 0.000000000000000000 ) ) ;
#15354 = CARTESIAN_POINT ( 'NONE',  ( 2.034671305879984349, -11.60021725667404624, 1.331347915349250233 ) ) ;
#15355 = VERTEX_POINT ( 'NONE', #12583 ) ;
#15356 = CARTESIAN_POINT ( 'NONE',  ( 2.260457164927716978, 4.804526096742694818, -5.941202713844608851 ) ) ;
#15357 = CARTESIAN_POINT ( 'NONE',  ( 6.263846918920576989, -28.63916073140924112, -12.80708683763842082 ) ) ;
#15358 = CARTESIAN_POINT ( 'NONE',  ( -35.00000000000000000, -6.891188680298757419, -9.512294188640973758 ) ) ;
#15359 = VERTEX_POINT ( 'NONE', #17925 ) ;
#15360 = DIRECTION ( 'NONE',  ( -1.000000000000000000, 0.000000000000000000, 0.000000000000000000 ) ) ;
#15361 = ORIENTED_EDGE ( 'NONE', *, *, #58971, .F. ) ;
#15362 = CARTESIAN_POINT ( 'NONE',  ( -35.00000000000000000, 12.57916205664481168, 2.080187960898605581 ) ) ;
#15363 = ORIENTED_EDGE ( 'NONE', *, *, #37117, .T. ) ;
#15364 = CARTESIAN_POINT ( 'NONE',  ( 13.08854576485774857, -9.765169235090553457, -6.977652523680585972 ) ) ;
#15365 = CARTESIAN_POINT ( 'NONE',  ( 4.037157412408303976E-12, -31.03649492335491544, 14.44372008463339085 ) ) ;
#15366 = DIRECTION ( 'NONE',  ( 1.000000000000000000, 0.000000000000000000, 0.000000000000000000 ) ) ;
#15367 = B_SPLINE_CURVE_WITH_KNOTS ( 'NONE', 3,
 ( #42292, #46655, #16411, #46340, #16059, #780, #31674 ),
 .UNSPECIFIED., .F., .F.,
 ( 4, 3, 4 ),
 ( 9.707054739159190006E-15, 0.002398160485435410494, 0.005002426799386534319 ),
 .UNSPECIFIED. ) ;
#15368 = CARTESIAN_POINT ( 'NONE',  ( 37.00000000000000711, 9.240395740215630482, -7.251710744571611578 ) ) ;
#15369 = CARTESIAN_POINT ( 'NONE',  ( 0.000000000000000000, -4.915517050588423587, 4.717154614762070430 ) ) ;
#15370 = CARTESIAN_POINT ( 'NONE',  ( 2.263328370261531219, 5.761609105518052942, -5.019946231381251067 ) ) ;
#15371 = CARTESIAN_POINT ( 'NONE',  ( -27.08421860617808008, 2.271664812096775066, -0.2990745872176354681 ) ) ;
#15372 = CARTESIAN_POINT ( 'NONE',  ( 0.3053067050349155820, -3.975408458060438299, -11.59706307017086857 ) ) ;
#15374 = VERTEX_POINT ( 'NONE', #7621 ) ;
#15373 = CARTESIAN_POINT ( 'NONE',  ( -27.35552965826137140, -2.548625910254533888, -1.773915698030580357 ) ) ;
#15375 = CARTESIAN_POINT ( 'NONE',  ( 35.00000000000000000, 12.08216339958902630, 1.591260454995109930 ) ) ;
#15376 = ADVANCED_FACE ( 'NONE', ( #27904 ), #48214, .T. ) ;
#15377 = AXIS2_PLACEMENT_3D ( 'NONE', #44101, #4192, #18834 ) ;
#15378 = ORIENTED_EDGE ( 'NONE', *, *, #51138, .F. ) ;
#15379 = CARTESIAN_POINT ( 'NONE',  ( 0.3675815128205894289, -4.447030445008257615, 11.44679196252407927 ) ) ;
#15380 = ORIENTED_EDGE ( 'NONE', *, *, #58557, .T. ) ;
#15381 = DIRECTION ( 'NONE',  ( 0.000000000000000000, 0.9551603052523489623, -0.2960891610144475439 ) ) ;
#15382 = AXIS2_PLACEMENT_3D ( 'NONE', #21688, #16678, #22668 ) ;
#15383 = ORIENTED_EDGE ( 'NONE', *, *, #1855, .T. ) ;
#15384 = CARTESIAN_POINT ( 'NONE',  ( 1.194176325881337597, -12.54527478469375801, 0.5141316333310796960 ) ) ;
#15385 = CARTESIAN_POINT ( 'NONE',  ( 0.3040950598368152291, 10.74226959800791370, 5.912066680610649883 ) ) ;
#15386 = CARTESIAN_POINT ( 'NONE',  ( 35.00000000000000000, -9.621072037176933378, 8.366449238204463512 ) ) ;
#15387 = FACE_OUTER_BOUND ( 'NONE', #65421, .T. ) ;
#15388 = AXIS2_PLACEMENT_3D ( 'NONE', #15358, #9366, #9702 ) ;
#15389 = CARTESIAN_POINT ( 'NONE',  ( 3.455078800971986386, 8.284346402942343701, -10.65933643386987306 ) ) ;
#15390 = EDGE_CURVE ( 'NONE', #14439, #6208, #42028, .T. ) ;
#15391 = ORIENTED_EDGE ( 'NONE', *, *, #62654, .T. ) ;
#15392 = CARTESIAN_POINT ( 'NONE',  ( 1.547277799339151105, -11.29700934613339669, -5.744300480442161572 ) ) ;
#15393 = ORIENTED_EDGE ( 'NONE', *, *, #38840, .F. ) ;
#15394 = CARTESIAN_POINT ( 'NONE',  ( 9.650011408859194617, -13.48023745212356239, -0.7481333718491276485 ) ) ;
#15395 = CARTESIAN_POINT ( 'NONE',  ( 1.000000000000000888, 6.160607635185464837, -4.277489166005534749 ) ) ;
#15396 = LINE ( 'NONE', #30673, #45585 ) ;
#15397 = ORIENTED_EDGE ( 'NONE', *, *, #35011, .T. ) ;
#15398 = CARTESIAN_POINT ( 'NONE',  ( -27.08704841010891329, -0.9786466045354095256, 2.081152044925695943 ) ) ;
#15399 = AXIS2_PLACEMENT_3D ( 'NONE', #38367, #19079, #2830 ) ;
#15400 = CARTESIAN_POINT ( 'NONE',  ( 33.05588761701184808, -2.860689001541081744, 23.72276540370177145 ) ) ;
#15401 = DIRECTION ( 'NONE',  ( -1.000000000000000000, 0.000000000000000000, 0.000000000000000000 ) ) ;
#15402 = B_SPLINE_CURVE_WITH_KNOTS ( 'NONE', 3,
 ( #3488, #13742, #3820, #28086, #34030, #17773, #29066, #44331, #64608, #54677, #29380, #33048, #34676, #24383, #24726, #40993, #45007, #4456, #60287, #14715 ),
 .UNSPECIFIED., .F., .F.,
 ( 4, 2, 2, 2, 2, 2, 2, 2, 2, 4 ),
 ( 1.274756208291110993E-17, 0.001996908854952089522, 0.002995363282428130380, 0.003993817709904172106, 0.004992272137380212964, 0.005491499351118232959, 0.005990726564856252954, 0.006489953778594273817, 0.006989180992332292945, 0.007987635419808342477 ),
 .UNSPECIFIED. ) ;
#15403 = LINE ( 'NONE', #55968, #49815 ) ;
#15404 = ORIENTED_EDGE ( 'NONE', *, *, #11541, .F. ) ;
#15405 = CARTESIAN_POINT ( 'NONE',  ( 35.00000000000000000, 3.287724142101414504, -11.73463472867577373 ) ) ;
#15406 = AXIS2_PLACEMENT_3D ( 'NONE', #59601, #64892, #13065 ) ;
#15407 = CARTESIAN_POINT ( 'NONE',  ( 11.92950489381524370, -32.88714273283334677, 11.67197772323657112 ) ) ;
#15408 = CARTESIAN_POINT ( 'NONE',  ( 1.462291587750753630, -3.724645088506430834, -12.08418494300916279 ) ) ;
#15409 = ADVANCED_FACE ( 'NONE', ( #26924 ), #28232, .T. ) ;
#15410 = DIRECTION ( 'NONE',  ( 0.000000000000000000, 0.01356324068817998940, -0.9999080150203990547 ) ) ;
#15411 = CARTESIAN_POINT ( 'NONE',  ( 0.3665391374699472626, -10.76665847464308534, -5.911453292029715811 ) ) ;
#15412 = CIRCLE ( 'NONE', #9058, 12.18649999999999878 ) ;
#15413 = VERTEX_POINT ( 'NONE', #57521 ) ;
#15414 = CARTESIAN_POINT ( 'NONE',  ( -35.04643116707788408, -0.008094444324497490628, -0.009112266603826177369 ) ) ;
#15415 = CARTESIAN_POINT ( 'NONE',  ( -22.27721701579900682, 3.478642907697087505, 1.205877546543679291 ) ) ;
#15416 = CARTESIAN_POINT ( 'NONE',  ( 0.3665391374699465965, 5.911453292029754003, -10.76665847464306403 ) ) ;
#15417 = ORIENTED_EDGE ( 'NONE', *, *, #58394, .T. ) ;
#15418 = CARTESIAN_POINT ( 'NONE',  ( 2.000000000000001776, -4.409940824963459960, 5.354199675985231721 ) ) ;
#15419 = CARTESIAN_POINT ( 'NONE',  ( -2.952869152607106251, 25.00000000000000000, 3.755417052241485365 ) ) ;
#15420 = EDGE_LOOP ( 'NONE', ( #7709, #51510, #15275, #46283 ) ) ;
#15421 = VERTEX_POINT ( 'NONE', #32224 ) ;
#15422 = ORIENTED_EDGE ( 'NONE', *, *, #21982, .F. ) ;
#15423 = CIRCLE ( 'NONE', #41995, 5.000000000000001776 ) ;
#15424 = EDGE_CURVE ( 'NONE', #41991, #60869, #45685, .T. ) ;
#15425 = ORIENTED_EDGE ( 'NONE', *, *, #43964, .T. ) ;
#15426 = CARTESIAN_POINT ( 'NONE',  ( -28.67667724226168602, 1.574547667005687490, -1.049259427760464547 ) ) ;
#15427 = CARTESIAN_POINT ( 'NONE',  ( 0.000000000000000000, -30.00000000000000000, 0.000000000000000000 ) ) ;
#15428 = DIRECTION ( 'NONE',  ( 1.000000000000000000, 0.000000000000000000, 0.000000000000000000 ) ) ;
#15429 = CARTESIAN_POINT ( 'NONE',  ( 6.661406098020968614, -4.211117136771885150, 11.23710102852283299 ) ) ;
#15430 = CARTESIAN_POINT ( 'NONE',  ( -35.00000000000000000, -3.093009498344009955, 11.78745411414838884 ) ) ;
#15431 = CARTESIAN_POINT ( 'NONE',  ( -7.278994278378053018, -26.30414574191657096, 14.75709246356266036 ) ) ;
#15432 = CARTESIAN_POINT ( 'NONE',  ( 35.00000000000000000, 4.705694406421931860E-17, -3.469127814946512892E-15 ) ) ;
#15434 = EDGE_LOOP ( 'NONE', ( #21529, #24201, #35116, #3694 ) ) ;
#15433 = DIRECTION ( 'NONE',  ( -1.000000000000000000, 0.000000000000000000, 0.000000000000000000 ) ) ;
#15435 = CARTESIAN_POINT ( 'NONE',  ( 47.00000000000000711, 4.705694406421931860E-17, -3.469127814946512892E-15 ) ) ;
#15436 = ORIENTED_EDGE ( 'NONE', *, *, #46782, .T. ) ;
#15437 = DIRECTION ( 'NONE',  ( -0.3865475372811021937, 0.6075346789811162385, 0.6938894834606063045 ) ) ;
#15438 = VERTEX_POINT ( 'NONE', #59157 ) ;
#15439 = ORIENTED_EDGE ( 'NONE', *, *, #45696, .T. ) ;
#15440 = CARTESIAN_POINT ( 'NONE',  ( -22.28415773361649954, -0.9182279841529923381, 3.586804264761546790 ) ) ;
#15441 = CARTESIAN_POINT ( 'NONE',  ( 8.240410296153402925, -29.00819526741667076, 11.87861853819304514 ) ) ;
#15442 = DIRECTION ( 'NONE',  ( 0.000000000000000000, -0.01356324068817991828, 0.9999080150203990547 ) ) ;
#15443 = AXIS2_PLACEMENT_3D ( 'NONE', #6667, #46557, #5694 ) ;
#15444 = EDGE_CURVE ( 'NONE', #32997, #34038, #55690, .T. ) ;
#15445 = CARTESIAN_POINT ( 'NONE',  ( -11.40165637463000614, -7.508992741355387857, -11.21895841913464587 ) ) ;
#15446 = LINE ( 'NONE', #45706, #62224 ) ;
#15447 = LINE ( 'NONE', #6146, #17141 ) ;
#15448 = ORIENTED_EDGE ( 'NONE', *, *, #14596, .F. ) ;
#15449 = EDGE_CURVE ( 'NONE', #38095, #5162, #53105, .T. ) ;
#15450 = ORIENTED_EDGE ( 'NONE', *, *, #50631, .F. ) ;
#15451 = CARTESIAN_POINT ( 'NONE',  ( -23.41523303002442091, -3.856096202952855823, -2.683951991546297045 ) ) ;
#15452 = VERTEX_POINT ( 'NONE', #64437 ) ;
#15453 = ADVANCED_FACE ( 'NONE', ( #8591 ), #38528, .T. ) ;
#15454 = EDGE_CURVE ( 'NONE', #53805, #43974, #61033, .T. ) ;
#15455 = ORIENTED_EDGE ( 'NONE', *, *, #18326, .T. ) ;
#15456 = CARTESIAN_POINT ( 'NONE',  ( 3.291290029914074378, 8.250315036047103590, 8.713914264323182834 ) ) ;
#15457 = CARTESIAN_POINT ( 'NONE',  ( 9.887190305652888256, 7.804856637177040035, -9.121441579706537794 ) ) ;
#15458 = CARTESIAN_POINT ( 'NONE',  ( 2.241526690369555208, 1.342748965918883597, 7.515450538999841612 ) ) ;
#15459 = CARTESIAN_POINT ( 'NONE',  ( 18.41452685719870530, -4.205716937948009715, 11.29046638959579063 ) ) ;
#15460 = CARTESIAN_POINT ( 'NONE',  ( 2.251139882113959434, 7.636654603229073857, 0.1241612276496930622 ) ) ;
#15461 = DIRECTION ( 'NONE',  ( 0.000000000000000000, 0.01356324068817992175, -0.9999080150203990547 ) ) ;
#15462 = EDGE_CURVE ( 'NONE', #51695, #26384, #26139, .T. ) ;
#15463 = EDGE_LOOP ( 'NONE', ( #58325, #55498, #47033, #26592 ) ) ;
#15464 = EDGE_CURVE ( 'NONE', #20267, #19209, #61817, .T. ) ;
#15465 = ORIENTED_EDGE ( 'NONE', *, *, #5994, .F. ) ;
#15466 = DIRECTION ( 'NONE',  ( -1.000000000000000000, 0.000000000000000000, 0.000000000000000000 ) ) ;
#15467 = CARTESIAN_POINT ( 'NONE',  ( 2.305787727787085295, 7.508843116234176662, -1.493241775258346227 ) ) ;
#15468 = CARTESIAN_POINT ( 'NONE',  ( 37.00000000000000711, 3.307597835713414369, 12.31350058095519096 ) ) ;
#15469 = AXIS2_PLACEMENT_3D ( 'NONE', #61993, #10136, #35049 ) ;
#15470 = CARTESIAN_POINT ( 'NONE',  ( 2.000000000000001776, 3.230174184210066191, 5.998318953995321223 ) ) ;
#15471 = CARTESIAN_POINT ( 'NONE',  ( -35.05175862995318425, -0.003178856583444314432, 0.01216930940958239893 ) ) ;
#15472 = ADVANCED_FACE ( 'NONE', ( #34815 ), #53837, .T. ) ;
#15473 = FACE_OUTER_BOUND ( 'NONE', #35897, .T. ) ;
#15474 = CARTESIAN_POINT ( 'NONE',  ( 1.549075743846762387, 2.862200647102950857, -12.34675572956577660 ) ) ;
#15475 = DIRECTION ( 'NONE',  ( -1.000000000000000000, 0.000000000000000000, 0.000000000000000000 ) ) ;
#15476 = ORIENTED_EDGE ( 'NONE', *, *, #908, .F. ) ;
#15477 = CARTESIAN_POINT ( 'NONE',  ( -27.15511094194037867, 2.237231637349079261, 1.124668417986046220 ) ) ;
#15478 = DIRECTION ( 'NONE',  ( 0.000000000000000000, 0.000000000000000000, 1.000000000000000000 ) ) ;
#15479 = CARTESIAN_POINT ( 'NONE',  ( 3.152665057736245391, 2.258875078500370837, -7.609997527622033076 ) ) ;
#15480 = CARTESIAN_POINT ( 'NONE',  ( 5.514624014163232779, 0.004137701579365773812, -0.0001700579043838819533 ) ) ;
#15481 = DIRECTION ( 'NONE',  ( 1.000000000000000000, -0.000000000000000000, 0.000000000000000000 ) ) ;
#15482 = ORIENTED_EDGE ( 'NONE', *, *, #24232, .T. ) ;
#15483 = CARTESIAN_POINT ( 'NONE',  ( -17.17991164731014564, -8.042067640992478061, -10.84821509031881526 ) ) ;
#15484 = CARTESIAN_POINT ( 'NONE',  ( 5.514970785353741078, 0.004324946436530184915, 0.001897634820904495461 ) ) ;
#15485 = CARTESIAN_POINT ( 'NONE',  ( 2.242819959140645025, 1.224821922055974177, 7.536009875295339278 ) ) ;
#15486 = ORIENTED_EDGE ( 'NONE', *, *, #41382, .F. ) ;
#15487 = CARTESIAN_POINT ( 'NONE',  ( 0.3675815128205912052, -6.367184624550238148, 10.50067073900649461 ) ) ;
#15488 = CARTESIAN_POINT ( 'NONE',  ( -17.70181089779288186, 6.586671166928411481, -10.03326520023147594 ) ) ;
#15489 = CARTESIAN_POINT ( 'NONE',  ( -22.28856623400852399, -1.018212315222191355, -3.573466130470484003 ) ) ;
#15491 = ORIENTED_EDGE ( 'NONE', *, *, #9179, .T. ) ;
#15490 = CARTESIAN_POINT ( 'NONE',  ( 2.994568964204208594, 0.9739368093814753102, 7.825096839971880769 ) ) ;
#15492 = CYLINDRICAL_SURFACE ( 'NONE', #46945, 5.000000000000000000 ) ;
#15493 = EDGE_CURVE ( 'NONE', #8461, #45502, #28069, .T. ) ;
#15494 = CARTESIAN_POINT ( 'NONE',  ( 2.589278595513413439, -7.361833592938442195, -2.423168677231957613 ) ) ;
#15495 = ORIENTED_EDGE ( 'NONE', *, *, #57069, .T. ) ;
#15496 = CARTESIAN_POINT ( 'NONE',  ( -35.04834644901396956, 0.004537648929124128358, 0.01306875526353049738 ) ) ;
#15497 = CARTESIAN_POINT ( 'NONE',  ( -9.008580248661141709, 10.91680307554687523, -7.949412954711231549 ) ) ;
#15499 = AXIS2_PLACEMENT_3D ( 'NONE', #49386, #38720, #18464 ) ;
#15498 = LINE ( 'NONE', #36773, #32169 ) ;
#15500 = CARTESIAN_POINT ( 'NONE',  ( 0.7446945582528449181, -1.802628359587426621, -12.27434006248856235 ) ) ;
#15501 = FACE_OUTER_BOUND ( 'NONE', #63413, .T. ) ;
#15502 = DIRECTION ( 'NONE',  ( 0.000000000000000000, 0.01356324068817998940, -0.9999080150203989437 ) ) ;
#15503 = CARTESIAN_POINT ( 'NONE',  ( 0.3632410797595273522, 11.44577450250092632, -4.445654054452411685 ) ) ;
#15504 = VERTEX_POINT ( 'NONE', #64130 ) ;
#15505 = DIRECTION ( 'NONE',  ( 0.000000000000000000, -0.01356324068817991828, 0.9999080150203990547 ) ) ;
#15506 = ORIENTED_EDGE ( 'NONE', *, *, #9156, .F. ) ;
#15507 =( NAMED_UNIT ( * ) SI_UNIT ( $, .STERADIAN. ) SOLID_ANGLE_UNIT ( ) );
#15508 = CARTESIAN_POINT ( 'NONE',  ( 2.000000000000001776, 6.796153407501448029, 1.388283512725836388 ) ) ;
#15509 = CARTESIAN_POINT ( 'NONE',  ( 2.781367136452630451, 1.659348694504713562, 7.636197200465927537 ) ) ;
#15510 = EDGE_CURVE ( 'NONE', #42839, #15077, #36733, .T. ) ;
#15511 = DIRECTION ( 'NONE',  ( 0.000000000000000000, 0.9970832820307036215, 0.07632122047556835764 ) ) ;
#15512 = ORIENTED_EDGE ( 'NONE', *, *, #61683, .F. ) ;
#15513 = CYLINDRICAL_SURFACE ( 'NONE', #52108, 2.899999999999994582 ) ;
#15514 =( BOUNDED_SURFACE ( )  B_SPLINE_SURFACE ( 3, 1, ( 
 ( #64994, #30411 ),
 ( #44703, #45058 ),
 ( #61320, #19794 ),
 ( #10132, #34722 ) ),
 .UNSPECIFIED., .F., .F., .F. ) 
 B_SPLINE_SURFACE_WITH_KNOTS ( ( 4, 4 ),
 ( 2, 2 ),
 ( 0.000000000000000000, 1.000000000000000000 ),
 ( 0.000000000000000000, 1.000000000000000000 ),
 .UNSPECIFIED. ) 
 GEOMETRIC_REPRESENTATION_ITEM ( )  RATIONAL_B_SPLINE_SURFACE ( (
 ( 1.000000000000000000, 1.000000000000000000),
 ( 0.9932032654565553509, 0.8386279382598736953),
 ( 0.9932032654565553509, 0.8386279382598736953),
 ( 1.000000000000000000, 1.000000000000000000) ) ) 
 REPRESENTATION_ITEM ( '' )  SURFACE ( )  );
#15515 = CARTESIAN_POINT ( 'NONE',  ( -35.00000000000000000, 6.564808257521927537, -10.93004082984011482 ) ) ;
#15516 = EDGE_CURVE ( 'NONE', #65388, #17474, #5776, .T. ) ;
#15517 = FACE_BOUND ( 'NONE', #39262, .T. ) ;
#15518 = ORIENTED_EDGE ( 'NONE', *, *, #33160, .T. ) ;
#15519 = ORIENTED_EDGE ( 'NONE', *, *, #57144, .T. ) ;
#15520 = CARTESIAN_POINT ( 'NONE',  ( 2.273267844204863941, -7.234348261136791969, -2.472013099045105022 ) ) ;
#15521 = ADVANCED_FACE ( 'NONE', ( #37045 ), #1165, .T. ) ;
#15522 = ORIENTED_EDGE ( 'NONE', *, *, #58041, .T. ) ;
#15523 = FACE_OUTER_BOUND ( 'NONE', #47028, .T. ) ;
#15524 = CARTESIAN_POINT ( 'NONE',  ( 1.937114397841935398, 5.226660192101590496, 11.72279974487465459 ) ) ;
#15525 = CARTESIAN_POINT ( 'NONE',  ( -37.00000000000000711, -3.340853584269456888, -11.26103545359859304 ) ) ;
#15526 = LINE ( 'NONE', #591, #53919 ) ;
#15527 = DIRECTION ( 'NONE',  ( 1.000000000000000000, 0.000000000000000000, 0.000000000000000000 ) ) ;
#15528 = CARTESIAN_POINT ( 'NONE',  ( -14.17344535826537744, 8.096743466816493040, 10.80418385471381448 ) ) ;
#15529 = EDGE_CURVE ( 'NONE', #54167, #59596, #54617, .T. ) ;
#15530 = CARTESIAN_POINT ( 'NONE',  ( -22.39032720737625937, -1.170177197944852754, -3.847057950743297816 ) ) ;
#15531 = VERTEX_POINT ( 'NONE', #21101 ) ;
#15532 = DIRECTION ( 'NONE',  ( 1.000000000000000000, 0.000000000000000000, 0.000000000000000000 ) ) ;
#15533 = EDGE_CURVE ( 'NONE', #35052, #64499, #9863, .T. ) ;
#15534 = CYLINDRICAL_SURFACE ( 'NONE', #62910, 6.095312090839646757 ) ;
#15535 = CARTESIAN_POINT ( 'NONE',  ( 0.000000000000000000, 3.155844197800189210, -6.177028383390422484 ) ) ;
#15536 = CARTESIAN_POINT ( 'NONE',  ( -19.32298883157327296, 13.49691393547099239, -0.7062062602696702607 ) ) ;
#15537 = CARTESIAN_POINT ( 'NONE',  ( -27.01437459610461644, 25.00000000000000000, -2.220455681983952267 ) ) ;
#15538 = DIRECTION ( 'NONE',  ( -0.000000000000000000, -0.000000000000000000, -1.000000000000000000 ) ) ;
#15539 = CARTESIAN_POINT ( 'NONE',  ( 2.350038591458241566, 9.744161863086068465, 4.227970903880576614 ) ) ;
#15540 = CARTESIAN_POINT ( 'NONE',  ( -37.00000000000000711, -10.49626516989265923, -7.238157050195740183 ) ) ;
#15541 = ADVANCED_FACE ( 'NONE', ( #12110 ), #42037, .T. ) ;
#15542 = ORIENTED_EDGE ( 'NONE', *, *, #38962, .T. ) ;
#15543 = CARTESIAN_POINT ( 'NONE',  ( 0.000000000000000000, -3.152010634611731366, 6.039758645301271933 ) ) ;
#15544 = AXIS2_PLACEMENT_3D ( 'NONE', #35371, #29410, #19111 ) ;
#15545 = EDGE_CURVE ( 'NONE', #56025, #666, #31653, .T. ) ;
#15546 = VECTOR ( 'NONE', #19990, 1000.000000000000000 ) ;
#15547 = ORIENTED_EDGE ( 'NONE', *, *, #47234, .T. ) ;
#15548 = CARTESIAN_POINT ( 'NONE',  ( -2.748241610611773300, -11.18522623946203609, 4.360826414742480672 ) ) ;
#15549 = CARTESIAN_POINT ( 'NONE',  ( -22.30527770659433173, -3.757123197210717525, 0.2559941915621729014 ) ) ;
#15550 = CARTESIAN_POINT ( 'NONE',  ( -14.86395414634036882, 7.932783874389932599, -10.92342345601903908 ) ) ;
#15551 = EDGE_CURVE ( 'NONE', #2297, #14551, #26425, .T. ) ;
#15552 = CARTESIAN_POINT ( 'NONE',  ( 0.2648978790185584908, -12.08224454301450201, 1.996248716311589400 ) ) ;
#15553 = LINE ( 'NONE', #10557, #41375 ) ;
#15554 = B_SPLINE_CURVE_WITH_KNOTS ( 'NONE', 3,
 ( #2570, #17520, #22839, #12497, #13484, #63370, #58410, #49104, #58084, #48445 ),
 .UNSPECIFIED., .F., .F.,
 ( 4, 2, 2, 2, 4 ),
 ( 0.000000000000000000, 0.002581029528971738683, 0.003226286911214673245, 0.003871544293457608241, 0.005162059057943477365 ),
 .UNSPECIFIED. ) ;
#15555 = ORIENTED_EDGE ( 'NONE', *, *, #29695, .T. ) ;
#15556 = CARTESIAN_POINT ( 'NONE',  ( 0.3040950598368152291, 9.552450779732110320, 7.687624643091462318 ) ) ;
#15557 = CARTESIAN_POINT ( 'NONE',  ( -30.16280033943767336, -2.214233674731126644, -11.80068582467317739 ) ) ;
#15558 = CARTESIAN_POINT ( 'NONE',  ( 0.9232167919969122005, -1.756271097262150027, 12.34114433434356961 ) ) ;
#15559 = CARTESIAN_POINT ( 'NONE',  ( -22.38932658256919339, 3.587092141214309748, 1.810630688302267588 ) ) ;
#15560 = CARTESIAN_POINT ( 'NONE',  ( 5.530133899448235191, 0.001124651387254991695, 0.01594518557925637264 ) ) ;
#15561 = CARTESIAN_POINT ( 'NONE',  ( -27.32337605527166957, 1.812546145273359111, -2.404211887218399735 ) ) ;
#15562 = ORIENTED_EDGE ( 'NONE', *, *, #44087, .T. ) ;
#15563 = CARTESIAN_POINT ( 'NONE',  ( -27.09569413923886216, -0.5521997980573341014, 2.259195818745851181 ) ) ;
#15564 = ORIENTED_EDGE ( 'NONE', *, *, #3587, .F. ) ;
#15565 = CARTESIAN_POINT ( 'NONE',  ( 0.3164563675027623479, -0.2404665832030537798, -12.26087493884172019 ) ) ;
#15566 = CARTESIAN_POINT ( 'NONE',  ( 0.000000000000000000, -33.00000000000000000, 0.000000000000000000 ) ) ;
#15567 = CARTESIAN_POINT ( 'NONE',  ( 29.21000934519853942, -6.487399748294825130, 10.13727455448839798 ) ) ;
#15568 = FACE_OUTER_BOUND ( 'NONE', #24849, .T. ) ;
#15569 = EDGE_CURVE ( 'NONE', #11924, #39344, #41867, .T. ) ;
#15570 = ORIENTED_EDGE ( 'NONE', *, *, #20445, .F. ) ;
#15571 = ORIENTED_EDGE ( 'NONE', *, *, #49546, .T. ) ;
#15572 = CARTESIAN_POINT ( 'NONE',  ( 5.514970785353741078, -0.004532877335078326457, 0.001326349372336564462 ) ) ;
#15573 = ORIENTED_EDGE ( 'NONE', *, *, #14154, .T. ) ;
#15574 = DIRECTION ( 'NONE',  ( -1.000000000000000000, 0.000000000000000000, 0.000000000000000000 ) ) ;
#15575 = CARTESIAN_POINT ( 'NONE',  ( 0.2638984909335720941, -0.1991813963113141794, -12.24571285024409129 ) ) ;
#15576 = FACE_OUTER_BOUND ( 'NONE', #11986, .T. ) ;
#15577 = CARTESIAN_POINT ( 'NONE',  ( -27.01437459610461644, 10.69338818478080455, -8.240233560378637634 ) ) ;
#15578 = CARTESIAN_POINT ( 'NONE',  ( -35.00000000000000000, -11.98254675519229906, 2.220215194441857331 ) ) ;
#15579 = CYLINDRICAL_SURFACE ( 'NONE', #45575, 4.999999999999999112 ) ;
#15580 = DIRECTION ( 'NONE',  ( 0.000000000000000000, -0.01356324068817998940, 0.9999080150203990547 ) ) ;
#15581 = ORIENTED_EDGE ( 'NONE', *, *, #45190, .T. ) ;
#15582 = EDGE_CURVE ( 'NONE', #13554, #16743, #2597, .T. ) ;
#15583 = CARTESIAN_POINT ( 'NONE',  ( 1.719304012341584365, 10.22720798541559439, -7.581471372738991299 ) ) ;
#15584 = ORIENTED_EDGE ( 'NONE', *, *, #14327, .F. ) ;
#15585 = AXIS2_PLACEMENT_3D ( 'NONE', #31322, #11356, #45619 ) ;
#15586 = CARTESIAN_POINT ( 'NONE',  ( 37.00000000000000711, -10.12742074351890764, 7.745827850123116143 ) ) ;
#15587 = CARTESIAN_POINT ( 'NONE',  ( 0.3665391374699464300, 9.576575648339126445, -7.691255657244195909 ) ) ;
#15588 = CYLINDRICAL_SURFACE ( 'NONE', #21551, 12.74999999999999822 ) ;
#15589 = EDGE_CURVE ( 'NONE', #43482, #58117, #49367, .T. ) ;
#15590 = EDGE_LOOP ( 'NONE', ( #18515, #43582, #29258, #27949 ) ) ;
#15591 = CIRCLE ( 'NONE', #9229, 12.18649999999999878 ) ;
#15592 = CARTESIAN_POINT ( 'NONE',  ( -18.91767133624980701, -29.93867241416544545, 6.768471019338283767 ) ) ;
#15593 = ORIENTED_EDGE ( 'NONE', *, *, #28278, .F. ) ;
#15594 = DIRECTION ( 'NONE',  ( -1.000000000000000000, 0.000000000000000000, 0.000000000000000000 ) ) ;
#15595 = CARTESIAN_POINT ( 'NONE',  ( 4.640500126211298593, -10.09411786235453690, -8.965292744499050670 ) ) ;
#15596 = LINE ( 'NONE', #5657, #30759 ) ;
#15597 = CARTESIAN_POINT ( 'NONE',  ( 6.516094201635106664, -8.971286330002193665, 7.981610909288549216 ) ) ;
#15598 = ORIENTED_EDGE ( 'NONE', *, *, #31657, .T. ) ;
#15599 = ORIENTED_EDGE ( 'NONE', *, *, #64780, .T. ) ;
#15600 = CARTESIAN_POINT ( 'NONE',  ( -27.08429572838383947, 1.632445743623435197, -1.608131779585709076 ) ) ;
#15601 = EDGE_CURVE ( 'NONE', #476, #48664, #58895, .T. ) ;
#15602 = ORIENTED_EDGE ( 'NONE', *, *, #48493, .T. ) ;
#15603 = LINE ( 'NONE', #6305, #18916 ) ;
#15604 = VERTEX_POINT ( 'NONE', #47055 ) ;
#15605 = B_SPLINE_CURVE_WITH_KNOTS ( 'NONE', 3,
 ( #25155, #51095, #36444, #11178, #55752, #16499, #30463, #31453, #25477, #46421 ),
 .UNSPECIFIED., .F., .F.,
 ( 4, 3, 3, 4 ),
 ( 5.401523115762199855E-05, 0.0008136511341527787088, 0.004068255670953081944, 0.005063778443040923075 ),
 .UNSPECIFIED. ) ;
#15606 = ORIENTED_EDGE ( 'NONE', *, *, #39577, .T. ) ;
#15607 = VERTEX_POINT ( 'NONE', #52036 ) ;
#15608 = LINE ( 'NONE', #65804, #25617 ) ;
#15609 = CARTESIAN_POINT ( 'NONE',  ( 14.88292245651501844, -27.94758995389112854, 11.26211297105860787 ) ) ;
#15610 = DIRECTION ( 'NONE',  ( 1.000000000000000000, 0.000000000000000000, 0.000000000000000000 ) ) ;
#15611 = CARTESIAN_POINT ( 'NONE',  ( 2.253265082352433613, 2.732639326785903489, -7.132841660187132504 ) ) ;
#15612 = DIRECTION ( 'NONE',  ( -1.000000000000000000, 0.000000000000000000, 0.000000000000000000 ) ) ;
#15613 = ORIENTED_EDGE ( 'NONE', *, *, #61127, .T. ) ;
#15614 = DIRECTION ( 'NONE',  ( -1.000000000000000000, 0.000000000000000000, 0.000000000000000000 ) ) ;
#15615 = ORIENTED_EDGE ( 'NONE', *, *, #49745, .F. ) ;
#15616 = CARTESIAN_POINT ( 'NONE',  ( -17.08916676964391357, 2.790706569880187171, 13.20909463602864697 ) ) ;
#15617 = DIRECTION ( 'NONE',  ( 0.000000000000000000, 0.01356324068817998940, -0.9999080150203989437 ) ) ;
#15618 = CARTESIAN_POINT ( 'NONE',  ( 35.00000000000000000, 9.321877890560537949, 7.146664589317804683 ) ) ;
#15619 = CARTESIAN_POINT ( 'NONE',  ( 1.462291587751620714, 10.08151577215017447, -7.633056170897675408 ) ) ;
#15620 = CARTESIAN_POINT ( 'NONE',  ( -37.00000000000000711, 1.456211999474342766, 11.65554240571057854 ) ) ;
#15621 = DIRECTION ( 'NONE',  ( 0.000000000000000000, -0.8827602140260367714, 0.4698238015817268742 ) ) ;
#15622 = ADVANCED_FACE ( 'NONE', ( #46387 ), #31418, .T. ) ;
#15623 = ORIENTED_EDGE ( 'NONE', *, *, #37533, .F. ) ;
#15624 = DIRECTION ( 'NONE',  ( 0.000000000000000000, 0.8276889981568920085, -0.5611870653623801664 ) ) ;
#15625 = EDGE_CURVE ( 'NONE', #19640, #63755, #11074, .T. ) ;
#15626 = ORIENTED_EDGE ( 'NONE', *, *, #27381, .F. ) ;
#15627 = CARTESIAN_POINT ( 'NONE',  ( 0.2717059086739003759, 10.69429229731978026, 5.971041827598861040 ) ) ;
#15628 = DIRECTION ( 'NONE',  ( -1.000000000000000000, 0.000000000000000000, -0.000000000000000000 ) ) ;
#15629 = EDGE_CURVE ( 'NONE', #19799, #31314, #32057, .T. ) ;
#15630 = CARTESIAN_POINT ( 'NONE',  ( 2.242819959140599284, -3.728423299585179151, -6.662619100654629811 ) ) ;
#15631 = CARTESIAN_POINT ( 'NONE',  ( 2.241536586108912488, 7.519576125149805002, 1.319514354261222211 ) ) ;
#15632 = ORIENTED_EDGE ( 'NONE', *, *, #35470, .F. ) ;
#15633 = CARTESIAN_POINT ( 'NONE',  ( 1.948354844646327688, 5.347695345042151160, -10.70340528295104399 ) ) ;
#15634 = CARTESIAN_POINT ( 'NONE',  ( -28.66013792860432119, 0.7552004871165373112, -1.673433383655440920 ) ) ;
#15635 = DIRECTION ( 'NONE',  ( -1.000000000000000000, 0.000000000000000000, 0.000000000000000000 ) ) ;
#15636 = AXIS2_PLACEMENT_3D ( 'NONE', #57511, #36563, #57179 ) ;
#15637 = CARTESIAN_POINT ( 'NONE',  ( 2.770579946183327813, 3.639932028439821998, 6.910873157406250300 ) ) ;
#15638 = AXIS2_PLACEMENT_3D ( 'NONE', #51456, #50775, #45781 ) ;
#15639 = CARTESIAN_POINT ( 'NONE',  ( 1.000000000000000888, -6.253963800348261159, 4.139799123620986343 ) ) ;
#15640 = CARTESIAN_POINT ( 'NONE',  ( 1.452237505248555660, -4.880303821310934431, -11.67686475128084567 ) ) ;
#15641 = CARTESIAN_POINT ( 'NONE',  ( 2.276905613633648517, -5.955225895210555009, -4.795880183929630114 ) ) ;
#15642 = CARTESIAN_POINT ( 'NONE',  ( -35.00000000000000000, -1.113475361586400814, -12.70128625845194215 ) ) ;
#15643 = EDGE_CURVE ( 'NONE', #5805, #40836, #53349, .T. ) ;
#15644 = ORIENTED_EDGE ( 'NONE', *, *, #48047, .F. ) ;
#15645 = EDGE_CURVE ( 'NONE', #44474, #50020, #2490, .T. ) ;
#15646 = ORIENTED_EDGE ( 'NONE', *, *, #54760, .T. ) ;
#15647 = CARTESIAN_POINT ( 'NONE',  ( 31.19808003874557301, -3.097905286366202660, -23.19915556217947739 ) ) ;
#15648 = CARTESIAN_POINT ( 'NONE',  ( 22.00000000000000711, -20.00000000000000000, 1.500000000000002887 ) ) ;
#15649 = DIRECTION ( 'NONE',  ( -1.000000000000000000, 0.000000000000000000, 0.000000000000000000 ) ) ;
#15650 = ORIENTED_EDGE ( 'NONE', *, *, #55768, .F. ) ;
#15651 = EDGE_CURVE ( 'NONE', #31935, #44696, #27019, .T. ) ;
#15652 = ORIENTED_EDGE ( 'NONE', *, *, #26567, .F. ) ;
#15653 = EDGE_LOOP ( 'NONE', ( #40261, #22376, #41273, #45608 ) ) ;
#15654 = FACE_OUTER_BOUND ( 'NONE', #33888, .T. ) ;
#15655 = AXIS2_PLACEMENT_3D ( 'NONE', #38930, #58913, #13326 ) ;
#15656 = CARTESIAN_POINT ( 'NONE',  ( -22.27715239060371744, 0.8317362037004401021, 3.586346956688089449 ) ) ;
#15657 = VERTEX_POINT ( 'NONE', #28391 ) ;
#15658 = CYLINDRICAL_SURFACE ( 'NONE', #21527, 4.999999999999999112 ) ;
#15660 = EDGE_LOOP ( 'NONE', ( #11443, #29688, #29984, #44319 ) ) ;
#15659 = CIRCLE ( 'NONE', #10352, 12.74999999999999822 ) ;
#15661 = DIRECTION ( 'NONE',  ( -0.000000000000000000, -0.000000000000000000, -1.000000000000000000 ) ) ;
#15662 = CARTESIAN_POINT ( 'NONE',  ( 13.74768401152559250, -28.58623978001741861, -12.41178146356746836 ) ) ;
#15663 = FACE_OUTER_BOUND ( 'NONE', #18607, .T. ) ;
#15664 = ORIENTED_EDGE ( 'NONE', *, *, #42312, .T. ) ;
#15665 = FACE_OUTER_BOUND ( 'NONE', #57800, .T. ) ;
#15666 = EDGE_CURVE ( 'NONE', #29924, #1294, #53996, .T. ) ;
#15667 = ORIENTED_EDGE ( 'NONE', *, *, #27777, .F. ) ;
#15668 = CARTESIAN_POINT ( 'NONE',  ( 0.2958664285830455154, -6.318165763623551534, -10.50235171906346388 ) ) ;
#15669 = ORIENTED_EDGE ( 'NONE', *, *, #64598, .T. ) ;
#15670 = CARTESIAN_POINT ( 'NONE',  ( -28.67667724226168602, 0.5419187306520724112, 1.812862320140625982 ) ) ;
#15671 = ADVANCED_FACE ( 'NONE', ( #48688 ), #28078, .T. ) ;
#15672 = CARTESIAN_POINT ( 'NONE',  ( -35.00000000000000000, 3.805206332242643263, -12.16893194857546057 ) ) ;
#15673 = DIRECTION ( 'NONE',  ( 1.000000000000000000, 0.000000000000000000, -0.000000000000000000 ) ) ;
#15674 = LINE ( 'NONE', #46298, #60165 ) ;
#15675 = CARTESIAN_POINT ( 'NONE',  ( 37.00000000000000711, 9.506317355798490354, 8.496612874013054650 ) ) ;
#15676 = AXIS2_PLACEMENT_3D ( 'NONE', #64735, #43828, #18589 ) ;
#15677 = CARTESIAN_POINT ( 'NONE',  ( 35.00000000000000000, -4.732539170486179003, 11.23004253107769124 ) ) ;
#15678 = CARTESIAN_POINT ( 'NONE',  ( -27.08421723179412410, 2.234476190936505180, -0.5069555058557374538 ) ) ;
#15679 = DIRECTION ( 'NONE',  ( -0.000000000000000000, -0.000000000000000000, -1.000000000000000000 ) ) ;
#15681 = ORIENTED_EDGE ( 'NONE', *, *, #25654, .T. ) ;
#15680 = FACE_OUTER_BOUND ( 'NONE', #1261, .T. ) ;
#15682 = LINE ( 'NONE', #25039, #20474 ) ;
#15683 = ORIENTED_EDGE ( 'NONE', *, *, #61763, .F. ) ;
#15684 = CARTESIAN_POINT ( 'NONE',  ( 13.15144582642090754, -12.98672512126129419, -3.693064144862436837 ) ) ;
#15685 = VERTEX_POINT ( 'NONE', #33385 ) ;
#15686 = CARTESIAN_POINT ( 'NONE',  ( 3.100650473569726007, -5.767490999797071360, -5.429218121582424672 ) ) ;
#15687 = ORIENTED_EDGE ( 'NONE', *, *, #60542, .T. ) ;
#15688 = CARTESIAN_POINT ( 'NONE',  ( 0.2739690278137239532, 8.012873994335690142, 9.264642836915861324 ) ) ;
#15689 = DIRECTION ( 'NONE',  ( -0.000000000000000000, -0.000000000000000000, -1.000000000000000000 ) ) ;
#15690 = LINE ( 'NONE', #22008, #56723 ) ;
#15691 = FACE_OUTER_BOUND ( 'NONE', #27372, .T. ) ;
#15692 = ADVANCED_FACE ( 'NONE', ( #59007 ), #34414, .F. ) ;
#15693 = DIRECTION ( 'NONE',  ( 0.000000000000000000, 0.000000000000000000, 1.000000000000000000 ) ) ;
#15694 = VERTEX_POINT ( 'NONE', #18761 ) ;
#15695 = CARTESIAN_POINT ( 'NONE',  ( 37.00000000000000711, -10.23119532541066867, 7.608228585767832897 ) ) ;
#15696 = EDGE_CURVE ( 'NONE', #42832, #35285, #14232, .T. ) ;
#15697 =( BOUNDED_CURVE ( )  B_SPLINE_CURVE ( 3, ( #48237, #33880, #8615, #18287 ),
 .UNSPECIFIED., .F., .F. ) 
 B_SPLINE_CURVE_WITH_KNOTS ( ( 4, 4 ),
 ( 1.904964486966213011, 1.936058588204076836 ),
 .UNSPECIFIED. ) 
 CURVE ( )  GEOMETRIC_REPRESENTATION_ITEM ( )  RATIONAL_B_SPLINE_CURVE ( ( 1.000000000000000000, 0.9999194313618959828, 0.9999194313618959828, 1.000000000000000000 ) ) 
 REPRESENTATION_ITEM ( '' )  );
#15698 = ORIENTED_EDGE ( 'NONE', *, *, #44705, .F. ) ;
#15699 = CARTESIAN_POINT ( 'NONE',  ( 9.612882454814815958, -13.47023598955340162, -0.9106303824545916026 ) ) ;
#15700 = LINE ( 'NONE', #10083, #57903 ) ;
#15701 = EDGE_CURVE ( 'NONE', #15987, #38977, #1543, .T. ) ;
#15702 = DIRECTION ( 'NONE',  ( 0.000000000000000000, 0.000000000000000000, 1.000000000000000000 ) ) ;
#15703 = ORIENTED_EDGE ( 'NONE', *, *, #39872, .T. ) ;
#15704 = CARTESIAN_POINT ( 'NONE',  ( -36.00000000000000711, -1.286231064351400555, 12.68495603654571369 ) ) ;
#15705 = CIRCLE ( 'NONE', #39068, 2.899999999999994582 ) ;
#15706 = CARTESIAN_POINT ( 'NONE',  ( 29.22869416613001547, 10.03734508462482289, 9.037510697015965988 ) ) ;
#15707 =( BOUNDED_SURFACE ( )  B_SPLINE_SURFACE ( 3, 1, ( 
 ( #39774, #9833 ),
 ( #38800, #19825 ),
 ( #39435, #28815 ),
 ( #44412, #30125 ) ),
 .UNSPECIFIED., .F., .F., .F. ) 
 B_SPLINE_SURFACE_WITH_KNOTS ( ( 4, 4 ),
 ( 2, 2 ),
 ( 0.000000000000000000, 1.000000000000000000 ),
 ( 0.000000000000000000, 1.000000000000000000 ),
 .UNSPECIFIED. ) 
 GEOMETRIC_REPRESENTATION_ITEM ( )  RATIONAL_B_SPLINE_SURFACE ( (
 ( 1.000000000000000000, 1.000000000000000000),
 ( 0.6933888150995267674, 0.9895912004443193632),
 ( 0.6933888150995267674, 0.9895912004443193632),
 ( 1.000000000000000000, 1.000000000000000000) ) ) 
 REPRESENTATION_ITEM ( '' )  SURFACE ( )  );
#15708 = CARTESIAN_POINT ( 'NONE',  ( -29.60090551182471685, -2.920537340839129303, 11.66374641461455042 ) ) ;
#15709 = CARTESIAN_POINT ( 'NONE',  ( -37.00000000000000711, 0.000000000000000000, 0.000000000000000000 ) ) ;
#15711 = VECTOR ( 'NONE', #11132, 1000.000000000000000 ) ;
#15710 = CARTESIAN_POINT ( 'NONE',  ( -35.00000000000000000, 9.390600770287994337, 8.624332853796092380 ) ) ;
#15712 = VERTEX_POINT ( 'NONE', #37719 ) ;
#15713 = LINE ( 'NONE', #5115, #22455 ) ;
#15714 = DIRECTION ( 'NONE',  ( -1.000000000000000000, -0.000000000000000000, -0.000000000000000000 ) ) ;
#15715 = CARTESIAN_POINT ( 'NONE',  ( 2.000000000000001776, 6.539067737394503865, 2.314222412769824544 ) ) ;
#15716 = VECTOR ( 'NONE', #17768, 1000.000000000000000 ) ;
#15717 = B_SPLINE_CURVE_WITH_KNOTS ( 'NONE', 3,
 ( #30067, #65622, #40359, #36373, #148, #16084, #65317, #20429 ),
 .UNSPECIFIED., .F., .F.,
 ( 4, 2, 2, 4 ),
 ( 0.004604583187049208354, 0.006625549100428843735, 0.007636032057118663161, 0.008646515013808482586 ),
 .UNSPECIFIED. ) ;
#15718 = CARTESIAN_POINT ( 'NONE',  ( 0.2646305136544072623, 9.296005949277228453, 7.972778379581582975 ) ) ;
#15719 = CARTESIAN_POINT ( 'NONE',  ( 18.90103867708235086, -7.635891018350232429, 11.15525402366580821 ) ) ;
#15720 = ADVANCED_FACE ( 'NONE', ( #53683 ), #13418, .T. ) ;
#15721 = ORIENTED_EDGE ( 'NONE', *, *, #37307, .F. ) ;
#15722 = CARTESIAN_POINT ( 'NONE',  ( 0.5572780756278413739, 10.53376864352694042, 6.434474476007812527 ) ) ;
#15723 = CARTESIAN_POINT ( 'NONE',  ( 3.245536480809931401, 4.729013804446176472, -11.03678433915268364 ) ) ;
#15724 = CARTESIAN_POINT ( 'NONE',  ( -22.27878402819508707, 3.558531829368145605, -0.9624056734348108710 ) ) ;
#15725 = VERTEX_POINT ( 'NONE', #3483 ) ;
#15726 = CARTESIAN_POINT ( 'NONE',  ( 5.515539859299206427, -0.005618668168217476680, 0.002251761459665986825 ) ) ;
#15727 = CYLINDRICAL_SURFACE ( 'NONE', #15017, 12.74999999999999822 ) ;
#15728 = ORIENTED_EDGE ( 'NONE', *, *, #16835, .T. ) ;
#15729 = ORIENTED_EDGE ( 'NONE', *, *, #55900, .F. ) ;
#15730 = ORIENTED_EDGE ( 'NONE', *, *, #27608, .F. ) ;
#15731 = CARTESIAN_POINT ( 'NONE',  ( -27.08419642509983305, -1.697757994346402510, 1.538761233743662693 ) ) ;
#15732 = EDGE_CURVE ( 'NONE', #43228, #12145, #23752, .T. ) ;
#15733 = EDGE_LOOP ( 'NONE', ( #19246, #19772, #46554, #26508 ) ) ;
#15734 = DIRECTION ( 'NONE',  ( 1.000000000000000000, -0.000000000000000000, 0.000000000000000000 ) ) ;
#15735 = CARTESIAN_POINT ( 'NONE',  ( 0.3665391374699472626, -7.691255657244357558, 9.576575648338993219 ) ) ;
#15736 = LINE ( 'NONE', #36366, #20570 ) ;
#15737 = DIRECTION ( 'NONE',  ( 0.000000000000000000, 0.8515178078024887576, -0.5243256840888532722 ) ) ;
#15738 = ORIENTED_EDGE ( 'NONE', *, *, #25616, .T. ) ;
#15739 = CARTESIAN_POINT ( 'NONE',  ( 0.2646305136544065406, 4.064188116014548768, 11.55263159009959750 ) ) ;
#15740 = VECTOR ( 'NONE', #65338, 1000.000000000000000 ) ;
#15741 = B_SPLINE_CURVE_WITH_KNOTS ( 'NONE', 3,
 ( #3195, #49086, #12814, #24118, #9141, #17820, #59058, #28440, #29424, #34076, #18810, #39069, #59364, #53409, #43076, #63673, #59699, #18150, #23133, #13160, #33442, #23461, #14126, #2551 ),
 .UNSPECIFIED., .F., .F.,
 ( 4, 2, 2, 2, 2, 2, 2, 2, 2, 2, 2, 4 ),
 ( 6.009258394948636926E-18, 0.001190494761224138035, 0.002380989522448269998, 0.003571484283672401745, 0.004166731664284471087, 0.004761979044896539129, 0.005357226425508608038, 0.005952473806120676079, 0.006547721186732744121, 0.007142968567344811295, 0.008333463328568954318, 0.009523958089793097340 ),
 .UNSPECIFIED. ) ;
#15742 = CARTESIAN_POINT ( 'NONE',  ( -12.81094353615569048, -29.07674955874489342, 3.635823793965939466 ) ) ;
#15743 = CARTESIAN_POINT ( 'NONE',  ( 37.00000000000000711, 11.60979404548634619, -3.704519465651352483 ) ) ;
#15745 = ORIENTED_EDGE ( 'NONE', *, *, #28018, .T. ) ;
#15744 = CARTESIAN_POINT ( 'NONE',  ( 16.66082797316812503, -33.00000000000000000, 4.257284274447473926 ) ) ;
#15746 = DIRECTION ( 'NONE',  ( -1.000000000000000000, -0.000000000000000000, 0.000000000000000000 ) ) ;
#15747 = EDGE_CURVE ( 'NONE', #27703, #34385, #2826, .T. ) ;
#15748 = ORIENTED_EDGE ( 'NONE', *, *, #64353, .F. ) ;
#15749 = LINE ( 'NONE', #55350, #50809 ) ;
#15750 = ORIENTED_EDGE ( 'NONE', *, *, #15079, .T. ) ;
#15751 = ORIENTED_EDGE ( 'NONE', *, *, #60559, .F. ) ;
#15752 = DIRECTION ( 'NONE',  ( 1.000000000000000000, 0.000000000000000000, -0.000000000000000000 ) ) ;
#15753 = CARTESIAN_POINT ( 'NONE',  ( 19.56743653832047869, -29.99999999999999645, 4.999999999999984013 ) ) ;
#15754 = ADVANCED_FACE ( 'NONE', ( #64294 ), #3145, .T. ) ;
#15755 = AXIS2_PLACEMENT_3D ( 'NONE', #11611, #57515, #36567 ) ;
#15756 = CARTESIAN_POINT ( 'NONE',  ( 3.152665057736003362, 6.378477742801834438, 4.725420687649379836 ) ) ;
#15757 = CARTESIAN_POINT ( 'NONE',  ( 2.963017218115625795, 7.812878240621082604, -0.9869543242667312422 ) ) ;
#15758 = CARTESIAN_POINT ( 'NONE',  ( 0.7446945582511041994, -2.504154979875959253, 12.15064199164589986 ) ) ;
#15759 = CARTESIAN_POINT ( 'NONE',  ( 35.00000000000000000, 4.561791185930414549, -11.90598845858535526 ) ) ;
#15760 = EDGE_LOOP ( 'NONE', ( #15581, #44277, #46074, #21586 ) ) ;
#15761 = AXIS2_PLACEMENT_3D ( 'NONE', #2601, #57451, #26522 ) ;
#15762 = ORIENTED_EDGE ( 'NONE', *, *, #63187, .F. ) ;
#15763 = CARTESIAN_POINT ( 'NONE',  ( 47.00000000000000711, 4.705694406421931860E-17, -3.469127814946512892E-15 ) ) ;
#15764 = EDGE_LOOP ( 'NONE', ( #45911, #41756, #9342, #59868 ) ) ;
#15765 = AXIS2_PLACEMENT_3D ( 'NONE', #45631, #20367, #60940 ) ;
#15766 = ORIENTED_EDGE ( 'NONE', *, *, #39285, .T. ) ;
#15767 = CARTESIAN_POINT ( 'NONE',  ( 37.00000000000000711, 10.80478261802181805, -5.636262487437360136 ) ) ;
#15768 = CARTESIAN_POINT ( 'NONE',  ( 0.3675815128205894289, -10.50067073900656212, 6.367184624550128014 ) ) ;
#15769 = AXIS2_PLACEMENT_3D ( 'NONE', #18830, #43767, #13809 ) ;
#15770 = CARTESIAN_POINT ( 'NONE',  ( 2.000000000000001776, -5.814643797626899868, -3.550179297009637747 ) ) ;
#15771 = CARTESIAN_POINT ( 'NONE',  ( 1.547277799338578230, -12.34637640861317820, 2.861188171558898929 ) ) ;
#15772 = CARTESIAN_POINT ( 'NONE',  ( -22.27718112499583469, 1.380338971069160925, -3.412978993569787622 ) ) ;
#15773 = EDGE_CURVE ( 'NONE', #6738, #14524, #62044, .T. ) ;
#15774 = FACE_OUTER_BOUND ( 'NONE', #53172, .T. ) ;
#15775 = CARTESIAN_POINT ( 'NONE',  ( -22.27721056931765631, -0.7178530073137546763, -3.610969226755205153 ) ) ;
#15776 = EDGE_LOOP ( 'NONE', ( #35903, #42665, #22384, #35119 ) ) ;
#15777 = DIRECTION ( 'NONE',  ( 0.000000000000000000, 0.4698238015817364777, 0.8827602140260315533 ) ) ;
#15778 = DIRECTION ( 'NONE',  ( 1.000000000000000000, 0.000000000000000000, 0.000000000000000000 ) ) ;
#15779 = CARTESIAN_POINT ( 'NONE',  ( 2.305787727787083519, 2.461236246751071555, 7.249469779319919205 ) ) ;
#15780 = EDGE_CURVE ( 'NONE', #54088, #14585, #46000, .T. ) ;
#15781 = CARTESIAN_POINT ( 'NONE',  ( 37.00000000000000711, -11.35427606708803161, 4.426194442447358490 ) ) ;
#15782 = AXIS2_PLACEMENT_3D ( 'NONE', #13665, #9321, #9020 ) ;
#15783 = DIRECTION ( 'NONE',  ( 0.000000000000000000, -0.6269146997507876184, -0.7790879021242596014 ) ) ;
#15784 = VECTOR ( 'NONE', #10382, 1000.000000000000000 ) ;
#15785 = DIRECTION ( 'NONE',  ( 0.000000000000000000, 0.9718671068226450993, -0.2355298848897551256 ) ) ;
#15786 = DIRECTION ( 'NONE',  ( 0.000000000000000000, 0.1118654143051546479, 0.9937233664769768993 ) ) ;
#15787 = CARTESIAN_POINT ( 'NONE',  ( 3.152665057734095555, 3.546019893116337141, 7.102135024645864547 ) ) ;
#15788 = VERTEX_POINT ( 'NONE', #29061 ) ;
#15789 = CARTESIAN_POINT ( 'NONE',  ( 0.2648978790185593790, 10.67083876753491900, 6.008231198269021078 ) ) ;
#15790 = DIRECTION ( 'NONE',  ( -1.000000000000000000, -0.000000000000000000, 0.000000000000000000 ) ) ;
#15791 = FACE_OUTER_BOUND ( 'NONE', #43161, .T. ) ;
#15792 = CIRCLE ( 'NONE', #17916, 2.899999999999994582 ) ;
#15793 = CARTESIAN_POINT ( 'NONE',  ( 2.705197763288547996, -6.601241161176654160, -4.134294772209995195 ) ) ;
#15794 = CARTESIAN_POINT ( 'NONE',  ( 37.00000000000000711, 7.561043153948100226, 9.557269938331470982 ) ) ;
#15795 = AXIS2_PLACEMENT_3D ( 'NONE', #4465, #53777, #8214 ) ;
#15796 = EDGE_CURVE ( 'NONE', #55428, #6208, #4732, .T. ) ;
#15797 = ORIENTED_EDGE ( 'NONE', *, *, #4016, .F. ) ;
#15798 = CARTESIAN_POINT ( 'NONE',  ( -17.87896547527707014, -5.103338146098263195, -12.49897969532171160 ) ) ;
#15799 = DIRECTION ( 'NONE',  ( -0.000000000000000000, -0.000000000000000000, -1.000000000000000000 ) ) ;
#15800 = CARTESIAN_POINT ( 'NONE',  ( 2.249013661412229581, 1.207748565003235575, 7.540851674528672888 ) ) ;
#15801 = ORIENTED_EDGE ( 'NONE', *, *, #34370, .F. ) ;
#15802 = AXIS2_PLACEMENT_3D ( 'NONE', #47457, #61408, #40822 ) ;
#15803 = EDGE_CURVE ( 'NONE', #23216, #58222, #49366, .T. ) ;
#15804 = CARTESIAN_POINT ( 'NONE',  ( 35.00000000000000000, 2.696588552979229725, 12.46157735505186004 ) ) ;
#15805 = DIRECTION ( 'NONE',  ( 0.000000000000000000, -0.5155538571770288403, 0.8568571761675849441 ) ) ;
#15806 = CARTESIAN_POINT ( 'NONE',  ( -30.18541646480390384, -1.416020129149325513, 13.42553116244798517 ) ) ;
#15807 = CIRCLE ( 'NONE', #24321, 12.74999999999999822 ) ;
#15809 = ORIENTED_EDGE ( 'NONE', *, *, #22626, .T. ) ;
#15808 = FACE_OUTER_BOUND ( 'NONE', #32844, .T. ) ;
#15810 = DIRECTION ( 'NONE',  ( -1.000000000000000000, 0.000000000000000000, 0.000000000000000000 ) ) ;
#15811 = EDGE_CURVE ( 'NONE', #50088, #41521, #45000, .T. ) ;
#15812 = CARTESIAN_POINT ( 'NONE',  ( 2.368238019615253709, -7.273245349264763071, -2.455958560214716258 ) ) ;
#15813 = ORIENTED_EDGE ( 'NONE', *, *, #16498, .F. ) ;
#15814 = CARTESIAN_POINT ( 'NONE',  ( -36.00000000000000711, 8.017674001891920810, -9.913596905230035006 ) ) ;
#15815 = DIRECTION ( 'NONE',  ( 1.000000000000000000, 0.000000000000000000, 0.000000000000000000 ) ) ;
#15816 = CARTESIAN_POINT ( 'NONE',  ( -27.32337605527168023, -2.988381643048340752, -0.3676050637290815826 ) ) ;
#15817 = CARTESIAN_POINT ( 'NONE',  ( 37.00000000000000711, 4.705694406421931860E-17, -3.469127814946512892E-15 ) ) ;
#15818 = CARTESIAN_POINT ( 'NONE',  ( -14.47334165536100059, 0.000000000000000000, -1.000000000000000000 ) ) ;
#15819 = CARTESIAN_POINT ( 'NONE',  ( -18.45078447393003529, 4.179087011105350413, 12.83947810587989657 ) ) ;
#15820 = CARTESIAN_POINT ( 'NONE',  ( 0.3675815128205894289, 0.2638082659428422350, 12.27743992903066328 ) ) ;
#15821 = EDGE_CURVE ( 'NONE', #6431, #38541, #10022, .T. ) ;
#15822 = EDGE_LOOP ( 'NONE', ( #42286, #57999, #41698, #10973 ) ) ;
#15823 = CARTESIAN_POINT ( 'NONE',  ( 2.241352910868908310, -4.970878533273800137, 5.794346703933830334 ) ) ;
#15824 = ORIENTED_EDGE ( 'NONE', *, *, #2071, .F. ) ;
#15825 = CARTESIAN_POINT ( 'NONE',  ( 1.719304012340734822, -5.690355757825686922, -11.38834240361529737 ) ) ;
#15826 = DIRECTION ( 'NONE',  ( -1.000000000000000000, 0.000000000000000000, 0.000000000000000000 ) ) ;
#15827 = AXIS2_PLACEMENT_3D ( 'NONE', #31583, #46895, #35594 ) ;
#15828 = CARTESIAN_POINT ( 'NONE',  ( 37.00000000000000711, -3.704519465651390675, -11.60979404548633731 ) ) ;
#15829 = VERTEX_POINT ( 'NONE', #55294 ) ;
#15830 = DIRECTION ( 'NONE',  ( -1.000000000000000000, 0.000000000000000000, 0.000000000000000000 ) ) ;
#15831 = CARTESIAN_POINT ( 'NONE',  ( -24.33291729085842192, -8.849064928703691990, 8.108208844799051462 ) ) ;
#15832 = CIRCLE ( 'NONE', #20077, 2.899999999999994582 ) ;
#15833 = CARTESIAN_POINT ( 'NONE',  ( -22.27716857039623477, -1.095155339732089894, 3.514919882996458078 ) ) ;
#15834 = VERTEX_POINT ( 'NONE', #30361 ) ;
#15835 = ORIENTED_EDGE ( 'NONE', *, *, #25219, .T. ) ;
#15836 = CARTESIAN_POINT ( 'NONE',  ( 27.36401306237657849, -12.63164339974623829, 4.766274618149700437 ) ) ;
#15837 = VERTEX_POINT ( 'NONE', #34361 ) ;
#15838 = CARTESIAN_POINT ( 'NONE',  ( 5.515539859299206427, 0.004037661319610825333, -0.004509673239148351796 ) ) ;
#15839 = CARTESIAN_POINT ( 'NONE',  ( -35.00000000000000000, 6.036400161834567513, 10.07641281632180075 ) ) ;
#15840 = DIRECTION ( 'NONE',  ( 0.000000000000000000, -0.9903235168508535136, -0.1387779952735919697 ) ) ;
#15842 = VECTOR ( 'NONE', #56750, 1000.000000000000000 ) ;
#15841 = CARTESIAN_POINT ( 'NONE',  ( -27.09483304420744787, 1.013994808269859771, -2.090133548855283241 ) ) ;
#15843 = DIRECTION ( 'NONE',  ( 0.000000000000000000, 0.000000000000000000, -1.000000000000000000 ) ) ;
#15844 = CARTESIAN_POINT ( 'NONE',  ( 2.963017218115628015, -7.812878240621079051, 0.9869543242667844218 ) ) ;
#15845 = CARTESIAN_POINT ( 'NONE',  ( 2.000000000000001776, 3.805198749487521681, -5.799611601383208637 ) ) ;
#15846 = VECTOR ( 'NONE', #30217, 1000.000000000000000 ) ;
#15847 = ORIENTED_EDGE ( 'NONE', *, *, #23934, .T. ) ;
#15848 = FACE_OUTER_BOUND ( 'NONE', #42491, .T. ) ;
#15849 = LINE ( 'NONE', #21182, #58683 ) ;
#15850 = LINE ( 'NONE', #36129, #13641 ) ;
#15851 = DIRECTION ( 'NONE',  ( -1.000000000000000000, 0.000000000000000000, 0.000000000000000000 ) ) ;
#15852 = CARTESIAN_POINT ( 'NONE',  ( 35.00000000000000000, 1.457575200925545822, -12.66641127287626567 ) ) ;
#15853 = FACE_OUTER_BOUND ( 'NONE', #33754, .T. ) ;
#15854 = CYLINDRICAL_SURFACE ( 'NONE', #5850, 12.74999999999999822 ) ;
#15855 = CIRCLE ( 'NONE', #43488, 4.999999999999999112 ) ;
#15856 = LINE ( 'NONE', #51145, #10677 ) ;
#15857 = ORIENTED_EDGE ( 'NONE', *, *, #38292, .T. ) ;
#15858 = ADVANCED_FACE ( 'NONE', ( #4450 ), #59644, .T. ) ;
#15859 = ORIENTED_EDGE ( 'NONE', *, *, #5267, .F. ) ;
#15860 = CARTESIAN_POINT ( 'NONE',  ( 0.000000000000000000, 4.472310526050849333, -6.020667617347339906 ) ) ;
#15861 = AXIS2_PLACEMENT_3D ( 'NONE', #64845, #29294, #65191 ) ;
#15862 = ORIENTED_EDGE ( 'NONE', *, *, #35585, .F. ) ;
#15863 = CARTESIAN_POINT ( 'NONE',  ( -22.28776923226070750, -3.702096209084111855, 0.2883912626656597866 ) ) ;
#15864 = CARTESIAN_POINT ( 'NONE',  ( -35.00000000000000000, -6.657191900728257394, -9.677500615117970995 ) ) ;
#15865 = LINE ( 'NONE', #31506, #20319 ) ;
#15866 = CARTESIAN_POINT ( 'NONE',  ( -35.00000000000000000, 0.000000000000000000, 0.000000000000000000 ) ) ;
#15867 = VERTEX_POINT ( 'NONE', #25051 ) ;
#15868 = CARTESIAN_POINT ( 'NONE',  ( -22.27834755396594346, 2.756126180273648085, -2.447855249718977166 ) ) ;
#15869 = DIRECTION ( 'NONE',  ( 0.000000000000000000, 0.000000000000000000, 1.000000000000000000 ) ) ;
#15870 = CARTESIAN_POINT ( 'NONE',  ( 1.462291587749843691, -12.54737685278368353, 1.569662666436692389 ) ) ;
#15871 = CARTESIAN_POINT ( 'NONE',  ( -22.35190811654612020, 3.498661567523018601, 1.736165297230968463 ) ) ;
#15872 = CIRCLE ( 'NONE', #25439, 5.000000000000000000 ) ;
#15873 = ADVANCED_FACE ( 'NONE', ( #9396 ), #34671, .T. ) ;
#15874 = AXIS2_PLACEMENT_3D ( 'NONE', #37374, #37713, #6813 ) ;
#15875 = CARTESIAN_POINT ( 'NONE',  ( 9.147487969233463190, 5.798649334944467881, -12.19629036017794377 ) ) ;
#15876 = CARTESIAN_POINT ( 'NONE',  ( -35.00000000000000000, -6.475373545682229448, -10.32377448871674908 ) ) ;
#15877 = VERTEX_POINT ( 'NONE', #14706 ) ;
#15878 = VECTOR ( 'NONE', #28718, 1000.000000000000000 ) ;
#15879 = EDGE_CURVE ( 'NONE', #54738, #22062, #35329, .T. ) ;
#15880 = CARTESIAN_POINT ( 'NONE',  ( -27.09833916700337753, -0.5492787772339994268, 2.268067253347839429 ) ) ;
#15881 = ORIENTED_EDGE ( 'NONE', *, *, #5156, .T. ) ;
#15882 = EDGE_CURVE ( 'NONE', #41187, #36819, #54673, .T. ) ;
#15883 = CARTESIAN_POINT ( 'NONE',  ( -35.00000000000000000, 12.08216339958900676, 1.591260454995285789 ) ) ;
#15884 = DIRECTION ( 'NONE',  ( 0.000000000000000000, 0.000000000000000000, 1.000000000000000000 ) ) ;
#15885 = CARTESIAN_POINT ( 'NONE',  ( 26.47593756983254210, -11.32194551905248048, 3.984718518152139399 ) ) ;
#15886 = CARTESIAN_POINT ( 'NONE',  ( 35.00000000000000000, 4.705694406421931860E-17, -3.469127814946512892E-15 ) ) ;
#15887 = AXIS2_PLACEMENT_3D ( 'NONE', #31296, #16336, #16653 ) ;
#15888 = ORIENTED_EDGE ( 'NONE', *, *, #59476, .F. ) ;
#15890 = VERTEX_POINT ( 'NONE', #44327 ) ;
#15889 = ADVANCED_FACE ( 'NONE', ( #49990 ), #9091, .T. ) ;
#15891 = DIRECTION ( 'NONE',  ( 1.000000000000000000, 0.000000000000000000, 0.000000000000000000 ) ) ;
#15892 = VERTEX_POINT ( 'NONE', #30024 ) ;
#15893 = VECTOR ( 'NONE', #40343, 1000.000000000000000 ) ;
#15894 = CYLINDRICAL_SURFACE ( 'NONE', #64864, 12.18649999999999878 ) ;
#15896 = CARTESIAN_POINT ( 'NONE',  ( 35.00000000000000000, -0.4871980014160587347, 12.74068829017553739 ) ) ;
#15895 =( BOUNDED_SURFACE ( )  B_SPLINE_SURFACE ( 3, 1, ( 
 ( #42273, #32317 ),
 ( #42957, #42604 ),
 ( #53274, #7057 ),
 ( #28009, #37650 ) ),
 .UNSPECIFIED., .F., .F., .F. ) 
 B_SPLINE_SURFACE_WITH_KNOTS ( ( 4, 4 ),
 ( 2, 2 ),
 ( 0.000000000000000000, 1.000000000000000000 ),
 ( 0.000000000000000000, 1.000000000000000000 ),
 .UNSPECIFIED. ) 
 GEOMETRIC_REPRESENTATION_ITEM ( )  RATIONAL_B_SPLINE_SURFACE ( (
 ( 1.000000000000000000, 1.000000000000000000),
 ( 0.9942764183789327692, 0.8450855930916580938),
 ( 0.9942764183789327692, 0.8450855930916580938),
 ( 1.000000000000000000, 1.000000000000000000) ) ) 
 REPRESENTATION_ITEM ( '' )  SURFACE ( )  );
#15897 = DIRECTION ( 'NONE',  ( 0.000000000000000000, 0.000000000000000000, 1.000000000000000000 ) ) ;
#15898 = CARTESIAN_POINT ( 'NONE',  ( 1.000000000000000888, 1.530946385938382059, 7.342084388195351252 ) ) ;
#15899 = DIRECTION ( 'NONE',  ( -1.000000000000000000, 0.000000000000000000, 0.000000000000000000 ) ) ;
#15900 = ADVANCED_FACE ( 'NONE', ( #24721 ), #64934, .T. ) ;
#15901 = DIRECTION ( 'NONE',  ( -1.000000000000000000, 0.000000000000000000, 0.000000000000000000 ) ) ;
#15902 = CARTESIAN_POINT ( 'NONE',  ( 0.9296196016868064627, 12.34355205587819171, -1.754499435239005756 ) ) ;
#15903 = ORIENTED_EDGE ( 'NONE', *, *, #2602, .T. ) ;
#15904 = CARTESIAN_POINT ( 'NONE',  ( -9.036476730761222598, -11.24534018395614154, -4.204006637871185781 ) ) ;
#15905 = CIRCLE ( 'NONE', #53092, 12.18649999999999878 ) ;
#15906 = VERTEX_POINT ( 'NONE', #59978 ) ;
#15907 = CARTESIAN_POINT ( 'NONE',  ( 0.5572780756290103277, 4.507550621618655384, -11.49107179558557412 ) ) ;
#15908 = CARTESIAN_POINT ( 'NONE',  ( 21.64317917535383984, -12.68252773215642470, -4.630549806628736498 ) ) ;
#15909 = CARTESIAN_POINT ( 'NONE',  ( 3.152665057736163678, 7.923639299009212600, -0.4801242025614006481 ) ) ;
#15910 = ORIENTED_EDGE ( 'NONE', *, *, #65521, .F. ) ;
#15911 = EDGE_CURVE ( 'NONE', #63611, #39378, #19075, .T. ) ;
#15912 = DIRECTION ( 'NONE',  ( 1.000000000000000000, 1.836970198721029688E-16, 0.000000000000000000 ) ) ;
#15913 = VERTEX_POINT ( 'NONE', #19742 ) ;
#15914 = CYLINDRICAL_SURFACE ( 'NONE', #14801, 12.18649999999999878 ) ;
#15915 = LINE ( 'NONE', #56857, #50972 ) ;
#15916 = CARTESIAN_POINT ( 'NONE',  ( -37.00843563923471891, -2.297594674915165225, -20.79457751400812171 ) ) ;
#15917 = ORIENTED_EDGE ( 'NONE', *, *, #46413, .F. ) ;
#15919 = EDGE_CURVE ( 'NONE', #59239, #62900, #20507, .T. ) ;
#15918 = EDGE_LOOP ( 'NONE', ( #33634, #6064, #55265, #8498, #35976, #60986, #15009, #18954, #8622, #64024, #62458, #37604, #21436, #36469, #19400, #61395, #22549, #46026, #10348, #18723, #26863, #44141, #59583, #37096, #4980, #6135, #51696, #57669, #37134, #59769, #57565, #43975, #61575, #970, #35394, #7348, #13337, #41342, #23921, #45987, #21744, #7660, #24998, #35222, #22216, #55719, #20763, #26934, #712, #32925, #7634, #51045, #23977, #43364, #55688, #52426, #12315, #8647, #11420, #28487, #8068, #10085, #27066, #40216, #54465, #32521, #28848, #49600, #56517, #9307, #35055, #62459, #49439, #5125, #37282, #57370, #51226, #55176, #62444, #20934, #2964, #16772, #18121, #13875, #19919, #33433, #64833, #26803, #53808, #23018, #38684, #8778, #58365, #42815, #3450, #25751, #14857, #61513, #6453, #36320, #35023, #28143, #55107, #56503, #24160, #45248, #29643, #59238, #53186, #63257, #3395, #39713 ) ) ;
#15920 = DIRECTION ( 'NONE',  ( -1.000000000000000000, -0.000000000000000000, 0.000000000000000000 ) ) ;
#15921 = ORIENTED_EDGE ( 'NONE', *, *, #4328, .T. ) ;
#15922 = CARTESIAN_POINT ( 'NONE',  ( -35.00000000000000000, -11.07407352312210058, -3.916263239775468197 ) ) ;
#15923 = ORIENTED_EDGE ( 'NONE', *, *, #62272, .T. ) ;
#15924 = ORIENTED_EDGE ( 'NONE', *, *, #41815, .T. ) ;
#15925 = ORIENTED_EDGE ( 'NONE', *, *, #51005, .T. ) ;
#15926 = CARTESIAN_POINT ( 'NONE',  ( 0.000000000000000000, 0.000000000000000000, 0.000000000000000000 ) ) ;
#15927 = CARTESIAN_POINT ( 'NONE',  ( -6.902482536246133726, -26.23992191484884273, 14.86511077371810430 ) ) ;
#15928 = AXIS2_PLACEMENT_3D ( 'NONE', #16320, #41904, #15328 ) ;
#15929 = DIRECTION ( 'NONE',  ( 0.3939253465568944290, -0.4679616473074953431, 0.7910971609033152774 ) ) ;
#15930 = CARTESIAN_POINT ( 'NONE',  ( 2.249013661412229581, 2.724484898587385739, -7.134443398813845150 ) ) ;
#15931 = CARTESIAN_POINT ( 'NONE',  ( 2.000000000000001776, 6.338823199656684615, 2.816798305433696470 ) ) ;
#15932 = ORIENTED_EDGE ( 'NONE', *, *, #54329, .F. ) ;
#15933 = DIRECTION ( 'NONE',  ( 0.000000000000000000, -0.5767582926625031137, -0.8169148498130233138 ) ) ;
#15934 = ORIENTED_EDGE ( 'NONE', *, *, #15320, .T. ) ;
#15935 = DIRECTION ( 'NONE',  ( 1.000000000000000000, 0.000000000000000000, 0.000000000000000000 ) ) ;
#15936 = DIRECTION ( 'NONE',  ( -1.000000000000000000, 0.000000000000000000, 0.000000000000000000 ) ) ;
#15937 = CARTESIAN_POINT ( 'NONE',  ( 5.514970785353741078, 0.0005190732562558549642, 0.004694330894494371832 ) ) ;
#15938 = FACE_OUTER_BOUND ( 'NONE', #13185, .T. ) ;
#15939 = CARTESIAN_POINT ( 'NONE',  ( 2.827825597296807381, -4.031992772938934877, -8.073505504738399452 ) ) ;
#15940 = CARTESIAN_POINT ( 'NONE',  ( 2.639814597422738718, -7.763021810282388913, -0.2564041122425915198 ) ) ;
#15941 = B_SPLINE_CURVE_WITH_KNOTS ( 'NONE', 3,
 ( #6739, #63231, #62558, #52932, #7366, #27014, #42267 ),
 .UNSPECIFIED., .F., .F.,
 ( 4, 3, 4 ),
 ( 5.151706802971572009E-15, 0.002398160485434644180, 0.005002426799381929495 ),
 .UNSPECIFIED. ) ;
#15942 = AXIS2_PLACEMENT_3D ( 'NONE', #32829, #52810, #7931 ) ;
#15943 = ADVANCED_FACE ( 'NONE', ( #4789 ), #60613, .T. ) ;
#15944 = VERTEX_POINT ( 'NONE', #26346 ) ;
#15945 = DIRECTION ( 'NONE',  ( -1.000000000000000000, 0.000000000000000000, 0.000000000000000000 ) ) ;
#15946 = ORIENTED_EDGE ( 'NONE', *, *, #29375, .T. ) ;
#15947 = CARTESIAN_POINT ( 'NONE',  ( 36.00000000000000711, 2.250029553613756228, -12.54989509947652060 ) ) ;
#15948 = DIRECTION ( 'NONE',  ( 1.000000000000000000, 0.000000000000000000, 0.000000000000000000 ) ) ;
#15949 = CARTESIAN_POINT ( 'NONE',  ( 2.305787727787085295, 5.970480882365287734, -4.792270232040832134 ) ) ;
#15950 = CARTESIAN_POINT ( 'NONE',  ( 2.653899356899655171, 4.109946795501193684, 6.596318473603771437 ) ) ;
#15951 = CARTESIAN_POINT ( 'NONE',  ( -22.51237073810381162, -1.333315726166072190, -4.218051923713597162 ) ) ;
#15952 = VERTEX_POINT ( 'NONE', #15695 ) ;
#15953 = ADVANCED_FACE ( 'NONE', ( #1746 ), #41300, .T. ) ;
#15954 = CARTESIAN_POINT ( 'NONE',  ( 37.00000000000000711, 4.705694406421931860E-17, -3.469127814946512892E-15 ) ) ;
#15956 = VECTOR ( 'NONE', #2043, 1000.000000000000000 ) ;
#15955 = CARTESIAN_POINT ( 'NONE',  ( 0.8320506296491554377, 5.883188144889929916, -10.95539209551940907 ) ) ;
#15957 = CARTESIAN_POINT ( 'NONE',  ( 2.000000000000001776, 6.767909380267608022, -0.7805499053121014441 ) ) ;
#15958 = CARTESIAN_POINT ( 'NONE',  ( 24.73714956085536798, -10.89644250736724729, -7.972329006067469415 ) ) ;
#15959 = EDGE_CURVE ( 'NONE', #19892, #64485, #61583, .T. ) ;
#15960 = AXIS2_PLACEMENT_3D ( 'NONE', #579, #15830, #44792 ) ;
#15961 = CARTESIAN_POINT ( 'NONE',  ( 0.2739690278137261736, 12.24770428423990687, -0.1830199730327832508 ) ) ;
#15962 = CARTESIAN_POINT ( 'NONE',  ( -36.00000000000000711, -12.74613886779085270, 0.3137578094508789439 ) ) ;
#15963 = AXIS2_PLACEMENT_3D ( 'NONE', #58460, #23536, #17888 ) ;
#15964 = EDGE_CURVE ( 'NONE', #48363, #15014, #57271, .T. ) ;
#15965 = CYLINDRICAL_SURFACE ( 'NONE', #64932, 4.999999999999999112 ) ;
#15966 = DIRECTION ( 'NONE',  ( 1.000000000000000000, 0.000000000000000000, -0.000000000000000000 ) ) ;
#15967 = CARTESIAN_POINT ( 'NONE',  ( 25.05309951391468459, 10.77522019223767558, -8.132934882857098202 ) ) ;
#15968 = AXIS2_PLACEMENT_3D ( 'NONE', #57797, #7555, #12214 ) ;
#15969 = AXIS2_PLACEMENT_3D ( 'NONE', #4038, #10004, #40583 ) ;
#15970 = CIRCLE ( 'NONE', #36140, 4.999999999999999112 ) ;
#15971 = ORIENTED_EDGE ( 'NONE', *, *, #46835, .F. ) ;
#15972 = VERTEX_POINT ( 'NONE', #1086 ) ;
#15973 = CARTESIAN_POINT ( 'NONE',  ( 0.2651627923886306082, 2.039714259676174812, 12.07509237025071691 ) ) ;
#15974 = CARTESIAN_POINT ( 'NONE',  ( 45.37278721346743282, -0.8995687559120728594, 12.71067884230445344 ) ) ;
#15975 = CARTESIAN_POINT ( 'NONE',  ( -28.67667724226168602, 1.299025457479356938, -1.375746547601627956 ) ) ;
#15976 = EDGE_CURVE ( 'NONE', #62523, #9962, #43623, .T. ) ;
#15977 = CARTESIAN_POINT ( 'NONE',  ( 2.000000000000001776, 0.4804830611970945520, -6.919838746524566986 ) ) ;
#15978 = EDGE_LOOP ( 'NONE', ( #49108, #53262, #3666, #20346 ) ) ;
#15979 = EDGE_CURVE ( 'NONE', #56247, #36611, #54509, .T. ) ;
#15980 = ORIENTED_EDGE ( 'NONE', *, *, #32209, .T. ) ;
#15981 = VERTEX_POINT ( 'NONE', #5428 ) ;
#15982 = DIRECTION ( 'NONE',  ( 0.000000000000000000, 0.07632122047555796318, -0.9970832820307042876 ) ) ;
#15983 = ADVANCED_FACE ( 'NONE', ( #42264 ), #56928, .F. ) ;
#15984 = AXIS2_PLACEMENT_3D ( 'NONE', #63935, #54644, #29652 ) ;
#15985 = CIRCLE ( 'NONE', #42556, 5.000000000000000000 ) ;
#15986 = DIRECTION ( 'NONE',  ( -1.000000000000000000, 0.000000000000000000, 0.000000000000000000 ) ) ;
#15987 = VERTEX_POINT ( 'NONE', #6403 ) ;
#15988 = EDGE_CURVE ( 'NONE', #9912, #58567, #19476, .T. ) ;
#15989 = CARTESIAN_POINT ( 'NONE',  ( 2.000000000000001776, -3.073484823194374993, 6.841322316745024779 ) ) ;
#15990 = AXIS2_PLACEMENT_3D ( 'NONE', #6517, #17801, #32422 ) ;
#15991 = VECTOR ( 'NONE', #41612, 1000.000000000000000 ) ;
#15992 = CARTESIAN_POINT ( 'NONE',  ( -35.00000000000000000, 8.573591947375437172, -8.029056188533592930 ) ) ;
#15993 = VERTEX_POINT ( 'NONE', #36966 ) ;
#15994 = CARTESIAN_POINT ( 'NONE',  ( -22.27706485742869091, 0.3729136217356220917, 3.662257305743802149 ) ) ;
#15995 = CARTESIAN_POINT ( 'NONE',  ( 15.59065549519859317, -34.16917994668161640, -7.755393724196137484 ) ) ;
#15996 = CARTESIAN_POINT ( 'NONE',  ( 2.242819959140781805, 7.138786956203901468, 2.707278038035910939 ) ) ;
#15997 = ORIENTED_EDGE ( 'NONE', *, *, #41018, .T. ) ;
#15998 = CIRCLE ( 'NONE', #30850, 5.000000000000001776 ) ;
#15999 = EDGE_CURVE ( 'NONE', #22166, #32661, #52297, .T. ) ;
#16000 = DIRECTION ( 'NONE',  ( 0.000000000000000000, 0.000000000000000000, 1.000000000000000000 ) ) ;
#16001 = ORIENTED_EDGE ( 'NONE', *, *, #51277, .F. ) ;
#16002 = CARTESIAN_POINT ( 'NONE',  ( 37.00000000000000711, 3.093009498343925134, -11.78745411414841016 ) ) ;
#16003 = CIRCLE ( 'NONE', #10689, 12.74999999999999822 ) ;
#16004 = VERTEX_POINT ( 'NONE', #37300 ) ;
#16005 = FACE_OUTER_BOUND ( 'NONE', #5395, .T. ) ;
#16006 = CARTESIAN_POINT ( 'NONE',  ( -18.58686583997218378, 5.151216734910788908, -10.83812558286602012 ) ) ;
#16007 = LINE ( 'NONE', #48198, #16377 ) ;
#16008 = DIRECTION ( 'NONE',  ( -1.000000000000000000, 0.000000000000000000, 0.000000000000000000 ) ) ;
#16009 = CARTESIAN_POINT ( 'NONE',  ( -37.00000000000000711, -2.968224442958319553, -11.81949347079750368 ) ) ;
#16010 = CARTESIAN_POINT ( 'NONE',  ( 8.437200413559441614, 4.217676196305609970, 11.23783527720358855 ) ) ;
#16011 = CARTESIAN_POINT ( 'NONE',  ( -27.08579483061203064, -0.2015567301747530349, -2.287150433979712627 ) ) ;
#16012 = CARTESIAN_POINT ( 'NONE',  ( 1.719304012338199517, 0.000000000000000000, 0.000000000000000000 ) ) ;
#16014 = ORIENTED_EDGE ( 'NONE', *, *, #56000, .F. ) ;
#16013 = DIRECTION ( 'NONE',  ( 1.000000000000000000, -0.000000000000000000, 0.000000000000000000 ) ) ;
#16015 = CARTESIAN_POINT ( 'NONE',  ( 2.903928887688777660, 8.407112942775256670, 2.496183838365350738 ) ) ;
#16016 = ORIENTED_EDGE ( 'NONE', *, *, #54064, .F. ) ;
#16017 = CYLINDRICAL_SURFACE ( 'NONE', #50816, 2.899999999999994582 ) ;
#16018 = CARTESIAN_POINT ( 'NONE',  ( 2.835339799623989521, -5.783398714696522447, -5.281994181469054972 ) ) ;
#16019 = EDGE_LOOP ( 'NONE', ( #26921, #60652, #51691, #9545 ) ) ;
#16020 = CARTESIAN_POINT ( 'NONE',  ( 2.000000000000001776, 6.767909380267608022, -0.7805499053121014441 ) ) ;
#16021 = CARTESIAN_POINT ( 'NONE',  ( 0.5572780756290403037, 11.70006938410089248, -3.933334466452371725 ) ) ;
#16022 = DIRECTION ( 'NONE',  ( 0.000000000000000000, 0.01356324068817992175, -0.9999080150203990547 ) ) ;
#16023 = CARTESIAN_POINT ( 'NONE',  ( -47.00000000000000711, 0.000000000000000000, 0.000000000000000000 ) ) ;
#16024 = CIRCLE ( 'NONE', #22390, 12.75000000000000178 ) ;
#16025 = ADVANCED_FACE ( 'NONE', ( #25699 ), #45988, .T. ) ;
#16026 = AXIS2_PLACEMENT_3D ( 'NONE', #27256, #6983, #12599 ) ;
#16027 = AXIS2_PLACEMENT_3D ( 'NONE', #61449, #20589, #30541 ) ;
#16028 = ORIENTED_EDGE ( 'NONE', *, *, #13925, .F. ) ;
#16029 = CARTESIAN_POINT ( 'NONE',  ( -17.57581661391215988, -5.612678105267818296, -10.60769512666424674 ) ) ;
#16030 = ORIENTED_EDGE ( 'NONE', *, *, #52189, .T. ) ;
#16031 = CARTESIAN_POINT ( 'NONE',  ( 9.687175622948608122, -13.48729812737142986, -0.5854820436212360146 ) ) ;
#16032 = CARTESIAN_POINT ( 'NONE',  ( 35.00000000000000000, 4.705694406421931860E-17, -3.469127814946512892E-15 ) ) ;
#16033 = DIRECTION ( 'NONE',  ( -1.000000000000000000, 0.000000000000000000, 0.000000000000000000 ) ) ;
#16034 = ORIENTED_EDGE ( 'NONE', *, *, #36957, .T. ) ;
#16035 = EDGE_CURVE ( 'NONE', #15413, #40664, #24788, .T. ) ;
#16036 = CARTESIAN_POINT ( 'NONE',  ( -27.08456565417846562, -0.9533904527919623284, 2.084650034356363424 ) ) ;
#16037 = AXIS2_PLACEMENT_3D ( 'NONE', #54307, #29028, #19381 ) ;
#16038 = CIRCLE ( 'NONE', #23462, 2.899999999999994582 ) ;
#16039 = B_SPLINE_CURVE_WITH_KNOTS ( 'NONE', 3,
 ( #11907, #36183, #51529, #41175, #11583, #6619, #25567, #56489, #16253, #960, #16589, #5643, #36536, #21583, #45862, #32183, #56843, #26233, #11267, #26888, #61151, #317, #46508, #31852 ),
 .UNSPECIFIED., .F., .F.,
 ( 4, 2, 2, 2, 2, 2, 2, 2, 2, 2, 2, 4 ),
 ( 3.529906531158615134E-18, 0.001336163118173039517, 0.002004244677259556240, 0.002672326236346072963, 0.004008489354519103806, 0.004676570913605619662, 0.005344652472692135517, 0.006012734031778651372, 0.006680815590865167228, 0.008016978709038195469, 0.009353141827211225445, 0.01068930494538425542 ),
 .UNSPECIFIED. ) ;
#16040 = AXIS2_PLACEMENT_3D ( 'NONE', #12283, #16311, #11315 ) ;
#16041 = AXIS2_PLACEMENT_3D ( 'NONE', #61987, #31701, #53975 ) ;
#16042 = CARTESIAN_POINT ( 'NONE',  ( 2.000000000000001776, 0.000000000000000000, 0.000000000000000000 ) ) ;
#16043 = DIRECTION ( 'NONE',  ( 1.000000000000000000, 0.000000000000000000, 0.000000000000000000 ) ) ;
#16044 = CIRCLE ( 'NONE', #53237, 20.00000000000000000 ) ;
#16045 = CARTESIAN_POINT ( 'NONE',  ( 37.00000000000000711, 4.824807283154291859, 11.80185301892974969 ) ) ;
#16046 = CARTESIAN_POINT ( 'NONE',  ( 8.814021188620074554, 6.315961215693210562, 11.93714002953281117 ) ) ;
#16047 = EDGE_CURVE ( 'NONE', #26236, #35632, #17697, .T. ) ;
#16048 = CARTESIAN_POINT ( 'NONE',  ( 37.00000000000000711, 7.376655759824882530, -9.700295462048689643 ) ) ;
#16049 = CYLINDRICAL_SURFACE ( 'NONE', #50569, 12.75000000000000178 ) ;
#16050 = DIRECTION ( 'NONE',  ( -1.000000000000000000, 0.000000000000000000, 0.000000000000000000 ) ) ;
#16051 = AXIS2_PLACEMENT_3D ( 'NONE', #33846, #54147, #39163 ) ;
#16052 = EDGE_CURVE ( 'NONE', #63452, #13640, #28637, .T. ) ;
#16053 = B_SPLINE_CURVE_WITH_KNOTS ( 'NONE', 3,
 ( #57895, #23278, #57559, #7005, #43219, #47901, #8008, #33589, #12303, #32261, #18308, #8313, #11979, #48891, #28271, #53876, #63184, #7663, #7312 ),
 .UNSPECIFIED., .F., .F.,
 ( 4, 3, 3, 3, 3, 3, 4 ),
 ( 0.000000000000000000, 2.832085443540691141E-05, 4.217789847394793712E-05, 5.603488375046113660E-05, 6.989180858579362990E-05, 9.821094829918940096E-05, 0.0001178165571465098204 ),
 .UNSPECIFIED. ) ;
#16054 = EDGE_LOOP ( 'NONE', ( #46025, #13528, #58869, #16384, #57937, #13198, #46825, #835, #510, #47934, #25270, #1458, #63700, #19964, #50557, #27527, #14849, #32485, #59226, #17063, #17154, #39911, #42507, #3355, #8481, #45944, #27485, #12245, #35385, #19048, #6000, #10727, #9204, #17771, #18787, #30540, #35451, #29637, #48589, #65571, #8178, #24599, #12410, #48715, #51629, #26549, #17812, #51859, #50854, #18072, #61275, #4435, #23882, #60161, #17106, #44596, #57106, #12340, #48573, #41851, #62253, #63173, #32596, #42823, #30013, #31073, #25947, #12871, #31607, #14259, #47146, #23457, #30570, #3727, #51028, #64811, #45346, #10702, #56514, #53601, #26366, #41780, #13808, #21496, #5013, #51765, #29979, #22238, #64317, #61355, #21737, #50964, #48929, #28511, #28865, #48065, #59055, #47104, #58153, #9269, #58208, #29584, #20249, #29978, #29872, #33260, #52613, #16928, #55192, #29002, #22960, #47588, #5353, #32276, #65181, #51317, #61999, #38329, #61017, #19215, #29627, #31450, #24169, #52395, #33409, #34601, #52083, #54846, #55267, #41114, #10357, #47281, #4503, #10765, #33823, #1454, #60435, #39416, #44190, #52793, #5279, #28430, #26582, #53477, #50381, #33955, #32668, #64529, #61528, #4184, #13069, #2062, #560, #24182, #38894, #25702, #8151, #30248, #15436, #37143, #12373, #61786, #44972, #28081, #30388, #43052, #57176, #61234, #59997, #62952, #47456, #32552, #39329, #19046, #34598, #63123, #40182, #32518, #51359, #42216, #20010, #43483, #42746, #48193, #59873, #11197, #35428, #34031, #51382, #51416, #7398, #9105, #41752, #34767, #33696, #52800, #42170, #20296, #15602, #64247, #20415, #56013, #54165, #54623, #63708, #53697, #40890, #40378, #29720, #13135, #11136, #28606, #27175, #27250, #43408, #60317, #32877, #28192, #34633, #7712, #39671, #28972, #54799, #41917, #36625, #36868, #29191, #36686, #1596, #47613, #19553, #63390, #56886, #59707, #53236, #15571, #15917, #17894, #34010, #30693, #64249, #17188, #2089, #21847, #54883, #39091, #8670, #41042, #50538, #28305, #57177, #1077, #33627, #58037, #33577, #15903, #23542, #25808, #42474, #31914, #62883, #38285, #3900, #19620, #48149, #56227, #4342, #51492, #2211, #35960, #2562, #56071, #49083, #19907, #6801, #63499, #13366, #51450, #12258, #26713, #27602, #40882, #53642, #1048, #35619, #18657, #34747, #36559, #6957, #52286, #43743, #49904, #34051, #61951, #20844, #58550, #59218, #2710, #23186, #57319, #43317, #43593, #8579, #30689, #24906, #388, #36004, #20857, #32585, #41424, #17433, #8818, #32092, #4530, #35483, #32643, #12391, #23531, #2193, #62388, #49498, #34047, #56026, #56395, #26389, #62491, #51929, #11718, #23255, #15232, #6290, #15040, #40694, #1168, #9704, #65552, #62293, #28205, #38080, #38350, #39305, #4828, #29488, #23727, #1535, #24583, #25559, #6006, #48210, #29612, #60684, #28544, #30071, #54313, #38395, #56390, #40247, #5147, #10690, #45324, #22236, #60207, #16549, #20612, #36144, #44889, #28755, #17586, #39064, #2724, #2852, #21748, #22483, #11518, #32258, #59525, #59399, #54591, #31081, #20556, #3445, #38901, #11763, #63200, #37858, #17935, #48833, #52925, #1270, #20086, #308, #33278, #32617, #5691, #61915, #37974, #59200, #19756, #45752, #62728, #45977, #8338, #64725, #37917, #33994 ) ) ;
#16055 = CARTESIAN_POINT ( 'NONE',  ( -35.00000000000000000, -8.258652103341496797, 8.352657516904644197 ) ) ;
#16056 = DIRECTION ( 'NONE',  ( -0.3865475372811021382, 0.7187975063895682970, 0.5778504531711067260 ) ) ;
#16057 = CIRCLE ( 'NONE', #18218, 7.499999999999988454 ) ;
#16058 = ORIENTED_EDGE ( 'NONE', *, *, #19786, .F. ) ;
#16059 = CARTESIAN_POINT ( 'NONE',  ( 2.655192694323234459, -5.716669423976344255, 7.714239566602159037 ) ) ;
#16060 = DIRECTION ( 'NONE',  ( 0.000000000000000000, 0.01356324068817998940, -0.9999080150203990547 ) ) ;
#16061 = CARTESIAN_POINT ( 'NONE',  ( 8.981012069803050224, 5.156238751367448359, -10.84194425323662436 ) ) ;
#16062 = ORIENTED_EDGE ( 'NONE', *, *, #46056, .F. ) ;
#16063 = CARTESIAN_POINT ( 'NONE',  ( 3.152665057734040488, 0.000000000000000000, 0.000000000000000000 ) ) ;
#16064 = AXIS2_PLACEMENT_3D ( 'NONE', #41497, #60478, #35199 ) ;
#16065 = CARTESIAN_POINT ( 'NONE',  ( -35.00000000000000000, -8.146229107149334681, -9.063649021439044162 ) ) ;
#16066 = VERTEX_POINT ( 'NONE', #57939 ) ;
#16067 = CARTESIAN_POINT ( 'NONE',  ( 0.2671309869109492752, -5.982543484153297619, 10.68612389951475627 ) ) ;
#16068 = EDGE_LOOP ( 'NONE', ( #46409, #33013, #35515, #5660 ) ) ;
#16069 = ORIENTED_EDGE ( 'NONE', *, *, #15138, .F. ) ;
#16070 = EDGE_CURVE ( 'NONE', #19449, #55094, #2494, .T. ) ;
#16071 = AXIS2_PLACEMENT_3D ( 'NONE', #57145, #51516, #55828 ) ;
#16072 = CARTESIAN_POINT ( 'NONE',  ( -35.00000000000000000, 2.627174906296914525, 11.44858830469741129 ) ) ;
#16073 = AXIS2_PLACEMENT_3D ( 'NONE', #30118, #35076, #62021 ) ;
#16074 = AXIS2_PLACEMENT_3D ( 'NONE', #47165, #62113, #11241 ) ;
#16075 = ORIENTED_EDGE ( 'NONE', *, *, #3641, .F. ) ;
#16076 = EDGE_CURVE ( 'NONE', #59854, #23038, #42798, .T. ) ;
#16077 = DIRECTION ( 'NONE',  ( -1.000000000000000000, 0.000000000000000000, 0.000000000000000000 ) ) ;
#16078 = CARTESIAN_POINT ( 'NONE',  ( -22.30861784526116054, -3.620936716852757087, 1.070462554923811593 ) ) ;
#16079 = LINE ( 'NONE', #55992, #49262 ) ;
#16080 = DIRECTION ( 'NONE',  ( 0.000000000000000000, -0.01356324068817998940, 0.9999080150203990547 ) ) ;
#16081 = ORIENTED_EDGE ( 'NONE', *, *, #17325, .T. ) ;
#16082 = FACE_OUTER_BOUND ( 'NONE', #45940, .T. ) ;
#16083 = CARTESIAN_POINT ( 'NONE',  ( 8.295782569430503628, -26.46630966554524278, 14.48708413691750074 ) ) ;
#16084 = CARTESIAN_POINT ( 'NONE',  ( -17.62527007572664317, 11.56525963221033138, 3.218409487716447082 ) ) ;
#16086 = VERTEX_POINT ( 'NONE', #28317 ) ;
#16085 = CARTESIAN_POINT ( 'NONE',  ( 0.2652384529303126182, -12.07141085622971843, -2.061422456317149265 ) ) ;
#16087 = EDGE_CURVE ( 'NONE', #31565, #7333, #32309, .T. ) ;
#16088 = CARTESIAN_POINT ( 'NONE',  ( 5.520433897694421610, -0.003119431460922313538, -0.01473594271720287882 ) ) ;
#16089 = VERTEX_POINT ( 'NONE', #27320 ) ;
#16090 = CARTESIAN_POINT ( 'NONE',  ( 37.00000000000000711, 4.705694406421931860E-17, -3.469127814946512892E-15 ) ) ;
#16091 = ORIENTED_EDGE ( 'NONE', *, *, #20056, .F. ) ;
#16092 = ORIENTED_EDGE ( 'NONE', *, *, #13852, .F. ) ;
#16093 = DIRECTION ( 'NONE',  ( -1.000000000000000000, 0.000000000000000000, 0.000000000000000000 ) ) ;
#16094 = AXIS2_PLACEMENT_3D ( 'NONE', #27456, #58392, #43401 ) ;
#16095 = CARTESIAN_POINT ( 'NONE',  ( -35.00000000000000000, 0.000000000000000000, 0.000000000000000000 ) ) ;
#16096 = CARTESIAN_POINT ( 'NONE',  ( 35.00000000000000000, 8.534258022646096009, -8.699265615723016154 ) ) ;
#16097 = AXIS2_PLACEMENT_3D ( 'NONE', #11710, #36669, #31993 ) ;
#16098 = ORIENTED_EDGE ( 'NONE', *, *, #13278, .T. ) ;
#16099 = DIRECTION ( 'NONE',  ( 1.000000000000000000, -0.000000000000000000, 0.000000000000000000 ) ) ;
#16100 = ADVANCED_FACE ( 'NONE', ( #47615 ), #2753, .T. ) ;
#16101 = CARTESIAN_POINT ( 'NONE',  ( -21.17861794710831091, 11.44571409049744304, -3.604945070120774808 ) ) ;
#16102 = CARTESIAN_POINT ( 'NONE',  ( -18.10941110424454337, -9.537088721069784114, -9.555689318548479250 ) ) ;
#16104 = ORIENTED_EDGE ( 'NONE', *, *, #9527, .T. ) ;
#16103 = CIRCLE ( 'NONE', #24600, 12.18650000000000055 ) ;
#16105 =( BOUNDED_CURVE ( )  B_SPLINE_CURVE ( 3, ( #5190, #29156, #4549, #44411 ),
 .UNSPECIFIED., .F., .F. ) 
 B_SPLINE_CURVE_WITH_KNOTS ( ( 4, 4 ),
 ( 1.948709165869125792, 1.984325536053276551 ),
 .UNSPECIFIED. ) 
 CURVE ( )  GEOMETRIC_REPRESENTATION_ITEM ( )  RATIONAL_B_SPLINE_CURVE ( ( 1.000000000000000000, 0.9998942923082225764, 0.9998942923082225764, 1.000000000000000000 ) ) 
 REPRESENTATION_ITEM ( '' )  );
#16106 = ORIENTED_EDGE ( 'NONE', *, *, #47364, .F. ) ;
#16107 = CARTESIAN_POINT ( 'NONE',  ( 37.00000000000000711, 9.040300684349800164, 7.499679039483956977 ) ) ;
#16108 = VERTEX_POINT ( 'NONE', #23008 ) ;
#16109 = AXIS2_PLACEMENT_3D ( 'NONE', #4829, #35034, #151 ) ;
#16110 = ORIENTED_EDGE ( 'NONE', *, *, #43223, .F. ) ;
#16111 = AXIS2_PLACEMENT_3D ( 'NONE', #22411, #11769, #57686 ) ;
#16112 = DIRECTION ( 'NONE',  ( 0.000000000000000000, 0.01356324068817991828, -0.9999080150203990547 ) ) ;
#16113 = DIRECTION ( 'NONE',  ( 0.000000000000000000, 0.000000000000000000, 1.000000000000000000 ) ) ;
#16114 = CARTESIAN_POINT ( 'NONE',  ( 1.719304012340549859, -10.62216384465898500, -7.017415949616274240 ) ) ;
#16115 = CARTESIAN_POINT ( 'NONE',  ( -21.17861794710831091, 11.44571409049744304, -3.604945070120774808 ) ) ;
#16116 = CARTESIAN_POINT ( 'NONE',  ( -35.00000000000000000, 0.000000000000000000, 0.000000000000000000 ) ) ;
#16117 = CARTESIAN_POINT ( 'NONE',  ( -4.989057617119011745, -0.9162120371760335003, -11.96497202265568660 ) ) ;
#16118 = CARTESIAN_POINT ( 'NONE',  ( -22.27716857039623477, -0.8090275962000452736, -3.591587580808010660 ) ) ;
#16119 = VECTOR ( 'NONE', #4445, 1000.000000000000000 ) ;
#16120 = EDGE_CURVE ( 'NONE', #52686, #38454, #35344, .T. ) ;
#16121 =( BOUNDED_SURFACE ( )  B_SPLINE_SURFACE ( 3, 1, ( 
 ( #4885, #24830 ),
 ( #25150, #220 ),
 ( #60390, #14813 ),
 ( #10495, #49770 ) ),
 .UNSPECIFIED., .F., .F., .F. ) 
 B_SPLINE_SURFACE_WITH_KNOTS ( ( 4, 4 ),
 ( 2, 2 ),
 ( 0.000000000000000000, 1.000000000000000000 ),
 ( 0.000000000000000000, 1.000000000000000000 ),
 .UNSPECIFIED. ) 
 GEOMETRIC_REPRESENTATION_ITEM ( )  RATIONAL_B_SPLINE_SURFACE ( (
 ( 1.000000000000000000, 1.000000000000000000),
 ( 0.9856612449720755231, 0.9999558406602322425),
 ( 0.9856612449720755231, 0.9999558406602322425),
 ( 1.000000000000000000, 1.000000000000000000) ) ) 
 REPRESENTATION_ITEM ( '' )  SURFACE ( )  );
#16122 = ORIENTED_EDGE ( 'NONE', *, *, #46727, .T. ) ;
#16123 = AXIS2_PLACEMENT_3D ( 'NONE', #48172, #22888, #31531 ) ;
#16124 = CARTESIAN_POINT ( 'NONE',  ( -22.27706485742869091, -2.985151051101489372, 2.154081322712201096 ) ) ;
#16125 = DIRECTION ( 'NONE',  ( 1.000000000000000000, 0.000000000000000000, -0.000000000000000000 ) ) ;
#16126 = AXIS2_PLACEMENT_3D ( 'NONE', #50443, #49141, #13525 ) ;
#16127 = VECTOR ( 'NONE', #60855, 1000.000000000000000 ) ;
#16128 = DIRECTION ( 'NONE',  ( 1.000000000000000000, 0.000000000000000000, 0.000000000000000000 ) ) ;
#16129 = CIRCLE ( 'NONE', #53309, 5.000000000000000000 ) ;
#16130 = CARTESIAN_POINT ( 'NONE',  ( -35.04834644901396956, 0.007161132384411757375, 0.01183641858481125804 ) ) ;
#16131 = B_SPLINE_CURVE_WITH_KNOTS ( 'NONE', 3,
 ( #33022, #63948, #54656, #64276, #38011, #14052, #13721, #48359, #33687, #44310, #54321, #3468, #59295 ),
 .UNSPECIFIED., .F., .F.,
 ( 4, 3, 3, 3, 4 ),
 ( 1.734723475976807094E-18, 6.607593386745445657E-05, 0.0001321518677373518917, 0.0001982171734706195316, 0.0002642860854759485545 ),
 .UNSPECIFIED. ) ;
#16132 = CARTESIAN_POINT ( 'NONE',  ( -27.10719052120871098, -0.5475695427849570640, 2.295785794152556125 ) ) ;
#16133 = CARTESIAN_POINT ( 'NONE',  ( 3.878878013157130766, 5.423588667954382103, -10.70679124709716135 ) ) ;
#16134 = CARTESIAN_POINT ( 'NONE',  ( -35.04582288351658548, -0.009684687560356024585, -0.008224400713808234509 ) ) ;
#16135 = EDGE_CURVE ( 'NONE', #52529, #2297, #37492, .T. ) ;
#16137 = ORIENTED_EDGE ( 'NONE', *, *, #12212, .F. ) ;
#16136 = EDGE_CURVE ( 'NONE', #47803, #62620, #39627, .T. ) ;
#16138 = CARTESIAN_POINT ( 'NONE',  ( -35.00000000000000000, -12.57916205664479925, -2.080187960898692623 ) ) ;
#16139 = CARTESIAN_POINT ( 'NONE',  ( -25.74864769002726561, 4.845157721295412223, 10.98320407977279345 ) ) ;
#16140 = FACE_OUTER_BOUND ( 'NONE', #51181, .T. ) ;
#16141 = B_SPLINE_CURVE_WITH_KNOTS ( 'NONE', 3,
 ( #54818, #33552, #64759, #64135, #29218, #49513, #8276, #23916 ),
 .UNSPECIFIED., .F., .F.,
 ( 4, 2, 2, 4 ),
 ( 0.000000000000000000, 0.0003639104015150007761, 0.0007278208030300015521, 0.001455641606060003104 ),
 .UNSPECIFIED. ) ;
#16142 = VECTOR ( 'NONE', #18940, 1000.000000000000000 ) ;
#16143 = EDGE_CURVE ( 'NONE', #19699, #57845, #53267, .T. ) ;
#16144 = AXIS2_PLACEMENT_3D ( 'NONE', #38138, #33157, #37496 ) ;
#16145 = CIRCLE ( 'NONE', #4491, 5.000000000000000888 ) ;
#16146 = CARTESIAN_POINT ( 'NONE',  ( 10.88715743210410203, 1.032614531350164011, -13.46093288850865655 ) ) ;
#16147 = FACE_OUTER_BOUND ( 'NONE', #31162, .T. ) ;
#16148 = ORIENTED_EDGE ( 'NONE', *, *, #38025, .T. ) ;
#16149 = CARTESIAN_POINT ( 'NONE',  ( 2.241451721903217731, 7.634225434981125602, 0.06083185034798754831 ) ) ;
#16150 = LINE ( 'NONE', #10829, #385 ) ;
#16151 = VECTOR ( 'NONE', #15016, 1000.000000000000000 ) ;
#16152 = CARTESIAN_POINT ( 'NONE',  ( 2.255723233588952326, 1.196143347838711790, 7.544965460065571783 ) ) ;
#16153 = EDGE_LOOP ( 'NONE', ( #43080, #3958, #59906, #30549 ) ) ;
#16154 = CARTESIAN_POINT ( 'NONE',  ( -35.00000000000000000, -10.64792938439751246, -5.927257550915431494 ) ) ;
#16155 = DIRECTION ( 'NONE',  ( 1.000000000000000000, 0.000000000000000000, 0.000000000000000000 ) ) ;
#16157 = ORIENTED_EDGE ( 'NONE', *, *, #16605, .F. ) ;
#16156 = CYLINDRICAL_SURFACE ( 'NONE', #58408, 12.18649999999999878 ) ;
#16158 = DIRECTION ( 'NONE',  ( 0.000000000000000000, 0.000000000000000000, 1.000000000000000000 ) ) ;
#16159 = ADVANCED_FACE ( 'NONE', ( #47951 ), #63541, .T. ) ;
#16160 = CARTESIAN_POINT ( 'NONE',  ( 2.889800649504073782, 2.156828754871467968, 5.728825117897715202 ) ) ;
#16161 = ORIENTED_EDGE ( 'NONE', *, *, #8531, .F. ) ;
#16162 = CIRCLE ( 'NONE', #38470, 5.000000000000001776 ) ;
#16163 = DIRECTION ( 'NONE',  ( 0.000000000000000000, 0.9999080150203989437, 0.01356324068818348313 ) ) ;
#16164 = CARTESIAN_POINT ( 'NONE',  ( 24.35223141888314302, -1.455662175893269961, -11.91666582609157210 ) ) ;
#16165 = CARTESIAN_POINT ( 'NONE',  ( 0.000000000000000000, -1.058508696395003890, 6.730038252034888480 ) ) ;
#16166 = LINE ( 'NONE', #63024, #6602 ) ;
#16167 = PLANE ( 'NONE',  #2655 ) ;
#16169 = ORIENTED_EDGE ( 'NONE', *, *, #5209, .T. ) ;
#16168 = CARTESIAN_POINT ( 'NONE',  ( 2.000000000000001776, 5.217815162096836268, 5.387430271863580700 ) ) ;
#16170 = ORIENTED_EDGE ( 'NONE', *, *, #44360, .T. ) ;
#16171 = CARTESIAN_POINT ( 'NONE',  ( 24.17474130245189912, -3.383288635110214937, -11.51882187244559930 ) ) ;
#16172 = ORIENTED_EDGE ( 'NONE', *, *, #31735, .F. ) ;
#16173 = AXIS2_PLACEMENT_3D ( 'NONE', #24176, #8237, #13228 ) ;
#16174 =( NAMED_UNIT ( * ) SI_UNIT ( $, .STERADIAN. ) SOLID_ANGLE_UNIT ( ) );
#16175 = DIRECTION ( 'NONE',  ( -1.000000000000000000, 0.000000000000000000, 0.000000000000000000 ) ) ;
#16176 = EDGE_CURVE ( 'NONE', #33730, #26919, #60862, .T. ) ;
#16178 = CARTESIAN_POINT ( 'NONE',  ( -17.32414925028539443, 3.214166590961689440, 11.56290286403455880 ) ) ;
#16177 = CIRCLE ( 'NONE', #54453, 5.000000000000002665 ) ;
#16179 = CIRCLE ( 'NONE', #58693, 12.75000000000000178 ) ;
#16180 = B_SPLINE_CURVE_WITH_KNOTS ( 'NONE', 3,
 ( #44265, #59911, #3749, #39274, #60219, #8370, #43954 ),
 .UNSPECIFIED., .F., .F.,
 ( 4, 3, 4 ),
 ( 5.561277602346480916E-15, 0.002398160485434703160, 0.005002426799382430830 ),
 .UNSPECIFIED. ) ;
#16181 = DIRECTION ( 'NONE',  ( 0.000000000000000000, 0.000000000000000000, 1.000000000000000000 ) ) ;
#16182 = ORIENTED_EDGE ( 'NONE', *, *, #21254, .T. ) ;
#16183 = CARTESIAN_POINT ( 'NONE',  ( 0.3040950598368144520, -10.49113473328026380, -6.347045025870875712 ) ) ;
#16184 = DIRECTION ( 'NONE',  ( 1.000000000000000000, 0.000000000000000000, 0.000000000000000000 ) ) ;
#16185 = DIRECTION ( 'NONE',  ( 1.000000000000000000, 0.000000000000000000, 0.000000000000000000 ) ) ;
#16186 = ORIENTED_EDGE ( 'NONE', *, *, #16552, .T. ) ;
#16187 = ORIENTED_EDGE ( 'NONE', *, *, #28893, .T. ) ;
#16188 = DIRECTION ( 'NONE',  ( -0.000000000000000000, -0.000000000000000000, -1.000000000000000000 ) ) ;
#16189 = B_SPLINE_CURVE_WITH_KNOTS ( 'NONE', 3,
 ( #48701, #12434, #42694, #49041, #64304, #23092, #27412, #2152, #53696, #52707, #47708, #48046, #8452, #18770, #22779, #62995, #13114, #17455 ),
 .UNSPECIFIED., .F., .F.,
 ( 4, 2, 2, 2, 2, 2, 2, 2, 4 ),
 ( 0.004456855160748429343, 0.005198565759172233368, 0.005940276357596038261, 0.006681986956019843153, 0.007423697554443648046, 0.008165408152867453806, 0.008907118751291256964, 0.009648829349715063591, 0.01039053994813886848 ),
 .UNSPECIFIED. ) ;
#16190 = EDGE_LOOP ( 'NONE', ( #65694, #45778, #17495, #25366 ) ) ;
#16191 = CARTESIAN_POINT ( 'NONE',  ( -47.00000000000000711, 0.000000000000000000, 0.000000000000000000 ) ) ;
#16192 = CARTESIAN_POINT ( 'NONE',  ( 35.00000000000000000, -8.389074212634222150, 8.839356091080130540 ) ) ;
#16193 = AXIS2_PLACEMENT_3D ( 'NONE', #7244, #16905, #32187 ) ;
#16194 = CARTESIAN_POINT ( 'NONE',  ( -27.09252613521643127, 2.309775830546442865, -0.1722886739160208736 ) ) ;
#16195 = DIRECTION ( 'NONE',  ( 0.000000000000000000, 0.9289767198167924178, -0.3701381553399118451 ) ) ;
#16196 = FACE_OUTER_BOUND ( 'NONE', #40739, .T. ) ;
#16197 = DIRECTION ( 'NONE',  ( 0.000000000000000000, 0.000000000000000000, -1.000000000000000000 ) ) ;
#16198 = DIRECTION ( 'NONE',  ( -1.000000000000000000, 0.000000000000000000, 0.000000000000000000 ) ) ;
#16199 = ADVANCED_FACE ( 'NONE', ( #53924 ), #42950, .F. ) ;
#16200 = VERTEX_POINT ( 'NONE', #40238 ) ;
#16201 = VECTOR ( 'NONE', #52891, 1000.000000000000000 ) ;
#16202 = DIRECTION ( 'NONE',  ( -1.000000000000000000, 0.000000000000000000, 0.000000000000000000 ) ) ;
#16203 = CIRCLE ( 'NONE', #37407, 5.000000000000001776 ) ;
#16204 = EDGE_CURVE ( 'NONE', #60647, #8323, #27730, .T. ) ;
#16205 = CARTESIAN_POINT ( 'NONE',  ( 2.573738926104378155, 4.074516960797472720, -6.586859681822621937 ) ) ;
#16206 = DIRECTION ( 'NONE',  ( 0.000000000000000000, 0.01356324068817998940, -0.9999080150203989437 ) ) ;
#16207 = CYLINDRICAL_SURFACE ( 'NONE', #41376, 4.999999999999999112 ) ;
#16208 = CARTESIAN_POINT ( 'NONE',  ( 1.452237505248552996, 7.672309600508697258, 10.06489946308204786 ) ) ;
#16209 = CARTESIAN_POINT ( 'NONE',  ( -10.00000000000000178, 0.000000000000000000, 0.000000000000000000 ) ) ;
#16210 = VERTEX_POINT ( 'NONE', #4365 ) ;
#16211 = ORIENTED_EDGE ( 'NONE', *, *, #46413, .T. ) ;
#16212 = EDGE_CURVE ( 'NONE', #59842, #49890, #60233, .T. ) ;
#16213 = CARTESIAN_POINT ( 'NONE',  ( -37.00000000000000711, -4.983891302653500333, -11.73555825188281787 ) ) ;
#16214 = AXIS2_PLACEMENT_3D ( 'NONE', #10766, #60657, #15095 ) ;
#16215 = ORIENTED_EDGE ( 'NONE', *, *, #41243, .F. ) ;
#16216 = DIRECTION ( 'NONE',  ( -0.9606638835031804380, 0.2689826995745335236, -0.06908842350339303162 ) ) ;
#16217 = CYLINDRICAL_SURFACE ( 'NONE', #7915, 1.500000000000000222 ) ;
#16218 = CARTESIAN_POINT ( 'NONE',  ( 2.259830038565016963, 4.804964945109173158, 5.940579220577212105 ) ) ;
#16219 = DIRECTION ( 'NONE',  ( -1.000000000000000000, 0.000000000000000000, 0.000000000000000000 ) ) ;
#16220 = EDGE_CURVE ( 'NONE', #17445, #14898, #24300, .T. ) ;
#16221 = ADVANCED_FACE ( 'NONE', ( #55217 ), #39264, .F. ) ;
#16222 = ORIENTED_EDGE ( 'NONE', *, *, #5438, .T. ) ;
#16223 = VECTOR ( 'NONE', #53948, 1000.000000000000114 ) ;
#16224 = DIRECTION ( 'NONE',  ( -0.9746931518056332067, -0.2235469969004301727, 0.000000000000000000 ) ) ;
#16225 = FACE_OUTER_BOUND ( 'NONE', #51191, .T. ) ;
#16226 = CARTESIAN_POINT ( 'NONE',  ( 1.719304012338836563, -1.452142814150213734, 12.64775761152536759 ) ) ;
#16227 = DIRECTION ( 'NONE',  ( 0.000000000000000000, 0.000000000000000000, 1.000000000000000000 ) ) ;
#16228 = AXIS2_PLACEMENT_3D ( 'NONE', #46171, #16561, #51502 ) ;
#16229 = AXIS2_PLACEMENT_3D ( 'NONE', #39953, #28664, #43625 ) ;
#16230 = CARTESIAN_POINT ( 'NONE',  ( 0.2759803524722200252, 6.288205958087932146, -10.51260004517005875 ) ) ;
#16231 = CARTESIAN_POINT ( 'NONE',  ( 2.297017764050092392, 2.771707546665591604, 7.133399178907324334 ) ) ;
#16232 = ORIENTED_EDGE ( 'NONE', *, *, #17590, .T. ) ;
#16233 = CARTESIAN_POINT ( 'NONE',  ( -35.00000000000000000, 4.237620530777800987, 11.42599468261430928 ) ) ;
#16234 = VERTEX_POINT ( 'NONE', #33945 ) ;
#16235 = DIRECTION ( 'NONE',  ( 1.000000000000000000, 0.000000000000000000, 0.000000000000000000 ) ) ;
#16236 = DIRECTION ( 'NONE',  ( -1.000000000000000000, -0.000000000000000000, 0.000000000000000000 ) ) ;
#16237 = DIRECTION ( 'NONE',  ( 1.000000000000000000, 0.000000000000000000, 0.000000000000000000 ) ) ;
#16238 = AXIS2_PLACEMENT_3D ( 'NONE', #54903, #9328, #39934 ) ;
#16239 = CARTESIAN_POINT ( 'NONE',  ( 29.10306999346632040, -8.924211771781015656, 8.035139106930564878 ) ) ;
#16240 = CARTESIAN_POINT ( 'NONE',  ( -9.953223611451470276, -4.237682741712822221, 11.22833300639604204 ) ) ;
#16241 = CIRCLE ( 'NONE', #36413, 12.74999999999999822 ) ;
#16242 = ORIENTED_EDGE ( 'NONE', *, *, #3993, .F. ) ;
#16243 = ORIENTED_EDGE ( 'NONE', *, *, #54188, .F. ) ;
#16244 = CARTESIAN_POINT ( 'NONE',  ( -37.00000000000000711, -5.143145423404365424, 11.66664283989678275 ) ) ;
#16245 = VERTEX_POINT ( 'NONE', #29944 ) ;
#16246 = DIRECTION ( 'NONE',  ( 1.000000000000000000, 0.000000000000000000, 0.000000000000000000 ) ) ;
#16247 = DIRECTION ( 'NONE',  ( 1.000000000000000000, -0.000000000000000000, 0.000000000000000000 ) ) ;
#16248 = DIRECTION ( 'NONE',  ( -1.000000000000000000, 0.000000000000000000, 0.000000000000000000 ) ) ;
#16249 = DIRECTION ( 'NONE',  ( -0.000000000000000000, -0.000000000000000000, -1.000000000000000000 ) ) ;
#16250 = CARTESIAN_POINT ( 'NONE',  ( 35.00000000000000000, 4.705694406421931860E-17, -3.469127814946512892E-15 ) ) ;
#16251 = VECTOR ( 'NONE', #21691, 1000.000000000000000 ) ;
#16252 = CARTESIAN_POINT ( 'NONE',  ( 0.000000000000000000, -5.107597897712365054, 4.693343793638375061 ) ) ;
#16253 = CARTESIAN_POINT ( 'NONE',  ( -8.371944397756363898, -1.942763698273609840, 11.84475809039481931 ) ) ;
#16254 = ORIENTED_EDGE ( 'NONE', *, *, #57829, .T. ) ;
#16255 = EDGE_CURVE ( 'NONE', #60814, #55613, #56642, .T. ) ;
#16256 = DIRECTION ( 'NONE',  ( 0.000000000000000000, 0.01356324068817998940, -0.9999080150203990547 ) ) ;
#16257 = ORIENTED_EDGE ( 'NONE', *, *, #28770, .F. ) ;
#16258 = DIRECTION ( 'NONE',  ( 1.000000000000000000, 0.000000000000000000, -0.000000000000000000 ) ) ;
#16259 = EDGE_CURVE ( 'NONE', #20729, #1896, #54253, .T. ) ;
#16260 = PLANE ( 'NONE',  #31083 ) ;
#16261 = ORIENTED_EDGE ( 'NONE', *, *, #30602, .T. ) ;
#16262 = CARTESIAN_POINT ( 'NONE',  ( -27.08485414902845534, 1.622802444813718381, 1.620258667553423182 ) ) ;
#16263 = CARTESIAN_POINT ( 'NONE',  ( -22.27721688985630522, 3.631967556481313864, -0.6032462375556627565 ) ) ;
#16264 = ORIENTED_EDGE ( 'NONE', *, *, #47054, .T. ) ;
#16265 = DIRECTION ( 'NONE',  ( 0.000000000000000000, -0.01356324068817998940, 0.9999080150203990547 ) ) ;
#16266 = CARTESIAN_POINT ( 'NONE',  ( 36.00000000000000711, -11.59605747147790211, -5.300372733891606458 ) ) ;
#16267 = DIRECTION ( 'NONE',  ( 0.000000000000000000, 0.000000000000000000, 1.000000000000000000 ) ) ;
#16268 = ORIENTED_EDGE ( 'NONE', *, *, #15959, .F. ) ;
#16269 = ORIENTED_EDGE ( 'NONE', *, *, #15066, .T. ) ;
#16270 = DIRECTION ( 'NONE',  ( 0.000000000000000000, -0.01356324068817992175, 0.9999080150203990547 ) ) ;
#16271 = EDGE_LOOP ( 'NONE', ( #14131, #41389, #6638, #39812 ) ) ;
#16272 = DIRECTION ( 'NONE',  ( 0.000000000000000000, 0.01356324068817992175, -0.9999080150203990547 ) ) ;
#16273 = ORIENTED_EDGE ( 'NONE', *, *, #468, .T. ) ;
#16274 = AXIS2_PLACEMENT_3D ( 'NONE', #28926, #55506, #9950 ) ;
#16275 = CIRCLE ( 'NONE', #44935, 2.899999999999995470 ) ;
#16276 = VERTEX_POINT ( 'NONE', #14961 ) ;
#16277 = ORIENTED_EDGE ( 'NONE', *, *, #63203, .F. ) ;
#16278 = DIRECTION ( 'NONE',  ( 0.000000000000000000, -0.9105187689795911643, 0.4134677391718608597 ) ) ;
#16279 = CARTESIAN_POINT ( 'NONE',  ( -15.65911990706704593, -28.15205781829744680, 10.62195165830229726 ) ) ;
#16280 = AXIS2_PLACEMENT_3D ( 'NONE', #59661, #50671, #64618 ) ;
#16281 = CIRCLE ( 'NONE', #13102, 12.18649999999999878 ) ;
#16282 = ADVANCED_FACE ( 'NONE', ( #35251 ), #24666, .F. ) ;
#16283 = CARTESIAN_POINT ( 'NONE',  ( -37.00000000000000711, 6.475373545682302279, 10.32377448871670467 ) ) ;
#16284 = DIRECTION ( 'NONE',  ( 1.000000000000000000, 0.000000000000000000, 0.000000000000000000 ) ) ;
#16285 = LINE ( 'NONE', #62803, #44413 ) ;
#16286 = VERTEX_POINT ( 'NONE', #51240 ) ;
#16287 = CARTESIAN_POINT ( 'NONE',  ( -22.49803948133826381, -3.817825231362863558, -2.073427785788384270 ) ) ;
#16288 = ADVANCED_FACE ( 'NONE', ( #10985 ), #31268, .T. ) ;
#16289 = VERTEX_POINT ( 'NONE', #10631 ) ;
#16290 = CARTESIAN_POINT ( 'NONE',  ( 35.00000000000000000, -2.544412758415763864, 11.91791701451268715 ) ) ;
#16291 = EDGE_CURVE ( 'NONE', #42846, #46638, #61197, .T. ) ;
#16293 = DIRECTION ( 'NONE',  ( -1.000000000000000000, -1.836970198721029688E-16, -0.000000000000000000 ) ) ;
#16292 = AXIS2_PLACEMENT_3D ( 'NONE', #62898, #37641, #32619 ) ;
#16294 = EDGE_CURVE ( 'NONE', #56356, #44514, #32161, .T. ) ;
#16295 = DIRECTION ( 'NONE',  ( -1.000000000000000000, 0.000000000000000000, 0.000000000000000000 ) ) ;
#16296 = CARTESIAN_POINT ( 'NONE',  ( 0.4626703367448973814, 9.611037151103600351, -7.694993290995405744 ) ) ;
#16297 = VECTOR ( 'NONE', #32245, 1000.000000000000000 ) ;
#16298 = LINE ( 'NONE', #31572, #12147 ) ;
#16299 = CARTESIAN_POINT ( 'NONE',  ( 0.9296196016852520394, -10.58347995892885862, -6.590257778218327367 ) ) ;
#16300 = AXIS2_PLACEMENT_3D ( 'NONE', #58723, #17148, #63022 ) ;
#16301 = VERTEX_POINT ( 'NONE', #16303 ) ;
#16302 = EDGE_CURVE ( 'NONE', #52904, #22369, #21616, .T. ) ;
#16303 = CARTESIAN_POINT ( 'NONE',  ( 0.2648978790185593790, -2.256510822326224464, 12.03635331166811540 ) ) ;
#16304 = AXIS2_PLACEMENT_3D ( 'NONE', #22375, #17062, #41682 ) ;
#16305 = ORIENTED_EDGE ( 'NONE', *, *, #41600, .F. ) ;
#16306 = EDGE_CURVE ( 'NONE', #16747, #44474, #46002, .T. ) ;
#16307 = CARTESIAN_POINT ( 'NONE',  ( 2.903928887688531191, 3.491800274468411569, 8.044738195288426041 ) ) ;
#16308 = DIRECTION ( 'NONE',  ( 0.000000000000000000, 0.000000000000000000, 1.000000000000000000 ) ) ;
#16309 = CIRCLE ( 'NONE', #366, 12.73084802173761787 ) ;
#16310 = CARTESIAN_POINT ( 'NONE',  ( 10.75388052849570109, -27.84561629232752722, 14.03224735226134712 ) ) ;
#16311 = DIRECTION ( 'NONE',  ( -1.000000000000000000, 0.000000000000000000, 0.000000000000000000 ) ) ;
#16312 = FACE_OUTER_BOUND ( 'NONE', #51193, .T. ) ;
#16313 = ORIENTED_EDGE ( 'NONE', *, *, #12366, .F. ) ;
#16314 = CYLINDRICAL_SURFACE ( 'NONE', #49438, 5.000000000000000888 ) ;
#16315 = CARTESIAN_POINT ( 'NONE',  ( 0.2759803524722195811, 2.313459762622696925, -12.02930579076647000 ) ) ;
#16316 = DIRECTION ( 'NONE',  ( 0.000000000000000000, 0.000000000000000000, 1.000000000000000000 ) ) ;
#16317 = DIRECTION ( 'NONE',  ( 1.000000000000000000, 0.000000000000000000, 0.000000000000000000 ) ) ;
#16318 = CIRCLE ( 'NONE', #423, 2.899999999999995026 ) ;
#16319 = EDGE_CURVE ( 'NONE', #21959, #40917, #18449, .T. ) ;
#16320 = CARTESIAN_POINT ( 'NONE',  ( -4.806344283790351390, -7.508992741355383416, 25.00000000000000000 ) ) ;
#16321 =( BOUNDED_SURFACE ( )  B_SPLINE_SURFACE ( 3, 1, ( 
 ( #10806, #56361 ),
 ( #31095, #51409 ),
 ( #17368, #32313 ),
 ( #7053, #27326 ) ),
 .UNSPECIFIED., .F., .F., .F. ) 
 B_SPLINE_SURFACE_WITH_KNOTS ( ( 4, 4 ),
 ( 2, 2 ),
 ( 0.000000000000000000, 1.000000000000000000 ),
 ( 0.000000000000000000, 1.000000000000000000 ),
 .UNSPECIFIED. ) 
 GEOMETRIC_REPRESENTATION_ITEM ( )  RATIONAL_B_SPLINE_SURFACE ( (
 ( 1.000000000000000000, 1.000000000000000000),
 ( 0.9932032654565553509, 0.8386279382598736953),
 ( 0.9932032654565553509, 0.8386279382598736953),
 ( 1.000000000000000000, 1.000000000000000000) ) ) 
 REPRESENTATION_ITEM ( '' )  SURFACE ( )  );
#16322 = DIRECTION ( 'NONE',  ( 1.000000000000000000, -0.000000000000000000, -0.000000000000000000 ) ) ;
#16323 = CARTESIAN_POINT ( 'NONE',  ( 35.00000000000000000, 9.060822531526046220, -7.474872387601039669 ) ) ;
#16324 = LINE ( 'NONE', #41576, #53520 ) ;
#16325 = CARTESIAN_POINT ( 'NONE',  ( 2.262775599886254874, 0.1412024122916927804, -7.640237753423678058 ) ) ;
#16326 = B_SPLINE_CURVE_WITH_KNOTS ( 'NONE', 3,
 ( #37890, #46893, #1352, #57205, #62489, #7292, #16634 ),
 .UNSPECIFIED., .F., .F.,
 ( 4, 3, 4 ),
 ( 7.634253333962453795E-15, 0.002398160485434851479, 0.005002426799384450916 ),
 .UNSPECIFIED. ) ;
#16327 = AXIS2_PLACEMENT_3D ( 'NONE', #49649, #44622, #4426 ) ;
#16328 = AXIS2_PLACEMENT_3D ( 'NONE', #2921, #17872, #64703 ) ;
#16329 = ORIENTED_EDGE ( 'NONE', *, *, #27889, .F. ) ;
#16330 = ORIENTED_EDGE ( 'NONE', *, *, #14786, .T. ) ;
#16332 = AXIS2_PLACEMENT_3D ( 'NONE', #27422, #47720, #38051 ) ;
#16331 = FACE_OUTER_BOUND ( 'NONE', #38706, .T. ) ;
#16333 = CARTESIAN_POINT ( 'NONE',  ( 46.52334308975179056, -0.6843348755673265282, 10.64746346056991833 ) ) ;
#16334 = DIRECTION ( 'NONE',  ( -1.000000000000000000, 0.000000000000000000, 0.000000000000000000 ) ) ;
#16335 = AXIS2_PLACEMENT_3D ( 'NONE', #56451, #40835, #10896 ) ;
#16336 = DIRECTION ( 'NONE',  ( -1.000000000000000000, 0.000000000000000000, 0.000000000000000000 ) ) ;
#16337 = ORIENTED_EDGE ( 'NONE', *, *, #16076, .F. ) ;
#16338 = CIRCLE ( 'NONE', #44655, 4.999999999999999112 ) ;
#16340 = VERTEX_POINT ( 'NONE', #26932 ) ;
#16339 = B_SPLINE_CURVE_WITH_KNOTS ( 'NONE', 3,
 ( #9602, #22723, #53644, #12711, #42985, #32995, #29900, #50208, #4665, #37678, #37990, #52307, #7722, #17029, #1758, #23339, #23020, #27653, #48622 ),
 .UNSPECIFIED., .F., .F.,
 ( 4, 3, 3, 3, 3, 3, 4 ),
 ( 8.523235939525396438E-18, 4.457896483014765320E-05, 6.639290541542085754E-05, 8.820687556478969962E-05, 0.0001100173248778915706, 0.0001545671401658112892, 0.0001830328308068612602 ),
 .UNSPECIFIED. ) ;
#16341 = VERTEX_POINT ( 'NONE', #31576 ) ;
#16342 = CARTESIAN_POINT ( 'NONE',  ( 35.00000000000000000, 2.905556151562782574, 11.38112321385047210 ) ) ;
#16343 = VECTOR ( 'NONE', #53648, 1000.000000000000000 ) ;
#16344 = EDGE_CURVE ( 'NONE', #58914, #12785, #25615, .T. ) ;
#16345 = CARTESIAN_POINT ( 'NONE',  ( -47.00000000000000711, 0.000000000000000000, 0.000000000000000000 ) ) ;
#16346 = VERTEX_POINT ( 'NONE', #687 ) ;
#16347 = CARTESIAN_POINT ( 'NONE',  ( 37.25000000000000711, -27.44817602132957646, -3.024649682742619472 ) ) ;
#16348 = CARTESIAN_POINT ( 'NONE',  ( 35.00000000000000000, 4.705694406421931860E-17, -3.469127814946512892E-15 ) ) ;
#16349 = ORIENTED_EDGE ( 'NONE', *, *, #62032, .T. ) ;
#16350 = CARTESIAN_POINT ( 'NONE',  ( -22.28482751661422867, 0.2989970708918424647, 3.692400780723903875 ) ) ;
#16351 = CARTESIAN_POINT ( 'NONE',  ( 17.02556425888772296, -29.48112685930881227, -9.540979227922154138 ) ) ;
#16352 = CARTESIAN_POINT ( 'NONE',  ( 24.89778902934379090, -0.9306873417793930514, 11.96553346855706934 ) ) ;
#16353 = ORIENTED_EDGE ( 'NONE', *, *, #32193, .T. ) ;
#16354 = DIRECTION ( 'NONE',  ( -1.000000000000000000, 0.000000000000000000, -0.000000000000000000 ) ) ;
#16355 = ORIENTED_EDGE ( 'NONE', *, *, #52243, .F. ) ;
#16356 = CARTESIAN_POINT ( 'NONE',  ( 1.719304012341583476, 7.581471372739232883, -10.22720798541541498 ) ) ;
#16357 = B_SPLINE_CURVE_WITH_KNOTS ( 'NONE', 3,
 ( #56366, #10160, #51414, #36744, #46397, #16133, #36417, #11154, #51728, #40753, #6174, #51068, #21457, #62022, #16475, #20473, #35737, #57038, #31736, #25453, #25793, #61042 ),
 .UNSPECIFIED., .F., .F.,
 ( 4, 2, 2, 2, 2, 2, 2, 2, 2, 2, 4 ),
 ( 2.453269466693398698E-18, 0.002704593263307899717, 0.003380741579134873345, 0.004056889894961846973, 0.005409186526615791628, 0.006085334842442765256, 0.006761483158269738017, 0.008113779789923683539, 0.008789928105750657167, 0.009466076421577630795, 0.01081837305323157805 ),
 .UNSPECIFIED. ) ;
#16358 = CARTESIAN_POINT ( 'NONE',  ( 35.00000000000000000, -9.512294188640847636, 6.891188680298922620 ) ) ;
#16359 = CARTESIAN_POINT ( 'NONE',  ( -12.31625042011401838, -33.75886355119370563, 10.24605909438714946 ) ) ;
#16360 = FACE_OUTER_BOUND ( 'NONE', #46651, .T. ) ;
#16361 = VECTOR ( 'NONE', #61263, 1000.000000000000000 ) ;
#16362 = CARTESIAN_POINT ( 'NONE',  ( 145.1370849898475797, 3.309064568108273190E-14, 0.000000000000000000 ) ) ;
#16363 = EDGE_CURVE ( 'NONE', #42534, #55068, #53463, .T. ) ;
#16364 = CARTESIAN_POINT ( 'NONE',  ( 10.39253138699964474, 0.7544984855469610840, 11.97748485473318780 ) ) ;
#16365 = CARTESIAN_POINT ( 'NONE',  ( 0.8375941296816619142, 6.548446001456726506, -10.57337970710577224 ) ) ;
#16366 = CARTESIAN_POINT ( 'NONE',  ( 8.682549669955445637, 5.989798744006710862, -10.40639624049628686 ) ) ;
#16367 = ORIENTED_EDGE ( 'NONE', *, *, #26594, .T. ) ;
#16368 = CARTESIAN_POINT ( 'NONE',  ( 36.00000000000000711, -12.26766708251988902, 3.473736367725380081 ) ) ;
#16369 = ORIENTED_EDGE ( 'NONE', *, *, #65790, .T. ) ;
#16370 = CARTESIAN_POINT ( 'NONE',  ( -36.00000000000000711, 11.47561260193584864, -5.556331110570289944 ) ) ;
#16371 = EDGE_CURVE ( 'NONE', #10789, #56661, #1441, .T. ) ;
#16372 = CARTESIAN_POINT ( 'NONE',  ( -47.00000000000000711, 0.000000000000000000, 0.000000000000000000 ) ) ;
#16373 = ADVANCED_FACE ( 'NONE', ( #30590 ), #35895, .T. ) ;
#16374 = CIRCLE ( 'NONE', #40759, 5.000000000000000888 ) ;
#16375 = ORIENTED_EDGE ( 'NONE', *, *, #25734, .T. ) ;
#16377 = VECTOR ( 'NONE', #22235, 1000.000000000000000 ) ;
#16376 = CARTESIAN_POINT ( 'NONE',  ( 2.717984159219859475, 7.415470774237106433, 2.397195612260604403 ) ) ;
#16378 = CARTESIAN_POINT ( 'NONE',  ( 0.9296196016851566712, 11.85136013469101890, -3.871279966919404458 ) ) ;
#16379 = FACE_OUTER_BOUND ( 'NONE', #39974, .T. ) ;
#16380 = CARTESIAN_POINT ( 'NONE',  ( 9.575800908719084958, -13.45729701195359240, -1.072919909436246266 ) ) ;
#16381 = DIRECTION ( 'NONE',  ( -1.000000000000000000, -0.000000000000000000, -0.000000000000000000 ) ) ;
#16382 = ORIENTED_EDGE ( 'NONE', *, *, #2503, .F. ) ;
#16383 = CARTESIAN_POINT ( 'NONE',  ( -19.16689948115911335, -3.912184365920206464, -11.34481683777750582 ) ) ;
#16384 = ORIENTED_EDGE ( 'NONE', *, *, #22016, .T. ) ;
#16385 = EDGE_CURVE ( 'NONE', #6586, #32962, #15181, .T. ) ;
#16386 = CARTESIAN_POINT ( 'NONE',  ( -37.00000000000000711, -45.00200000000000244, -4.500000000000000888 ) ) ;
#16387 = CARTESIAN_POINT ( 'NONE',  ( -22.23402523511428086, 3.673940397442055431E-16, 2.999999999999992006 ) ) ;
#16388 = DIRECTION ( 'NONE',  ( 0.000000000000000000, -0.01356324068817998940, 0.9999080150203990547 ) ) ;
#16389 = EDGE_CURVE ( 'NONE', #44234, #61480, #361, .T. ) ;
#16390 = EDGE_LOOP ( 'NONE', ( #14437, #12551, #56325, #30772 ) ) ;
#16391 = AXIS2_PLACEMENT_3D ( 'NONE', #14228, #54814, #18264 ) ;
#16392 = DIRECTION ( 'NONE',  ( 0.000000000000000000, 0.2960891610144441022, 0.9551603052523500725 ) ) ;
#16393 = EDGE_CURVE ( 'NONE', #49368, #63364, #18491, .T. ) ;
#16394 = CIRCLE ( 'NONE', #57794, 11.99999999999999822 ) ;
#16395 = EDGE_CURVE ( 'NONE', #7895, #31335, #52419, .T. ) ;
#16396 = CARTESIAN_POINT ( 'NONE',  ( 24.97568612634365337, -8.683198485571610448, -8.285225425757140272 ) ) ;
#16397 = CARTESIAN_POINT ( 'NONE',  ( 2.655192694323989411, 0.5793947661801427396, 9.584054627287489581 ) ) ;
#16398 = VECTOR ( 'NONE', #42984, 1000.000000000000000 ) ;
#16399 = EDGE_CURVE ( 'NONE', #451, #2871, #63025, .T. ) ;
#16400 = DIRECTION ( 'NONE',  ( 0.000000000000000000, 0.6876994588534245390, -0.7259954919231296211 ) ) ;
#16401 = CARTESIAN_POINT ( 'NONE',  ( 0.2759803524722218571, -5.960075719898764390, -10.70204612651783549 ) ) ;
#16402 = CARTESIAN_POINT ( 'NONE',  ( 0.2655924914740778187, 4.147079829127255479, 11.52280271232872089 ) ) ;
#16403 = CARTESIAN_POINT ( 'NONE',  ( 2.266490820343223245, -5.760233951938548813, 5.023127813992176449 ) ) ;
#16404 = CARTESIAN_POINT ( 'NONE',  ( 35.00000000000000000, 9.076753354953996933, -8.954052073409636492 ) ) ;
#16405 = AXIS2_PLACEMENT_3D ( 'NONE', #48134, #57785, #22859 ) ;
#16406 = AXIS2_PLACEMENT_3D ( 'NONE', #24545, #54161, #60780 ) ;
#16407 = VERTEX_POINT ( 'NONE', #61843 ) ;
#16408 = DIRECTION ( 'NONE',  ( 1.000000000000000000, 0.000000000000000000, 0.000000000000000000 ) ) ;
#16409 = LINE ( 'NONE', #7072, #49009 ) ;
#16410 = ORIENTED_EDGE ( 'NONE', *, *, #22766, .F. ) ;
#16411 = CARTESIAN_POINT ( 'NONE',  ( 2.177405672430794414, -6.668684901900762796, 8.997150696571290851 ) ) ;
#16412 = CARTESIAN_POINT ( 'NONE',  ( -22.27706485742869091, 3.358064672837120401, 1.508175983031588840 ) ) ;
#16413 = CARTESIAN_POINT ( 'NONE',  ( 37.00000000000000711, -12.05416472667166694, -1.791059740004382839 ) ) ;
#16414 = ORIENTED_EDGE ( 'NONE', *, *, #49142, .F. ) ;
#16415 = CARTESIAN_POINT ( 'NONE',  ( -22.31328051695926007, 3.633840107626944871, -1.076152733467184985 ) ) ;
#16416 = VERTEX_POINT ( 'NONE', #56884 ) ;
#16417 = CIRCLE ( 'NONE', #23834, 12.75000000000000178 ) ;
#16418 = AXIS2_PLACEMENT_3D ( 'NONE', #50752, #44762, #5202 ) ;
#16419 = CARTESIAN_POINT ( 'NONE',  ( 0.2915757698887287419, -5.940579417090853021, 10.71881693660620094 ) ) ;
#16420 = ORIENTED_EDGE ( 'NONE', *, *, #24628, .F. ) ;
#16421 = ORIENTED_EDGE ( 'NONE', *, *, #38232, .T. ) ;
#16423 = ADVANCED_FACE ( 'NONE', ( #11310 ), #31459, .F. ) ;
#16422 = CARTESIAN_POINT ( 'NONE',  ( -2.952869152607111136, -7.581333670610126418, 11.17020052527586138 ) ) ;
#16424 = ORIENTED_EDGE ( 'NONE', *, *, #29848, .T. ) ;
#16425 = DIRECTION ( 'NONE',  ( 0.000000000000000000, -0.01356324068817998940, 0.9999080150203990547 ) ) ;
#16426 = CARTESIAN_POINT ( 'NONE',  ( 0.6511581176968108675, -11.51117493088908361, -4.541862140119740765 ) ) ;
#16427 = FACE_OUTER_BOUND ( 'NONE', #46693, .T. ) ;
#16428 = FACE_OUTER_BOUND ( 'NONE', #20333, .T. ) ;
#16429 = VERTEX_POINT ( 'NONE', #42868 ) ;
#16430 = AXIS2_PLACEMENT_3D ( 'NONE', #36061, #56722, #22097 ) ;
#16431 = CARTESIAN_POINT ( 'NONE',  ( 2.889800649504073782, -3.986129653162616471, -4.645655809191405083 ) ) ;
#16432 = CARTESIAN_POINT ( 'NONE',  ( 4.261270162784661863, -31.40576903066106240, 14.03034928007075344 ) ) ;
#16433 = LINE ( 'NONE', #36700, #14333 ) ;
#16435 = ORIENTED_EDGE ( 'NONE', *, *, #12359, .T. ) ;
#16434 = DIRECTION ( 'NONE',  ( 0.000000000000000000, 0.01356324068817998940, -0.9999080150203990547 ) ) ;
#16436 = CARTESIAN_POINT ( 'NONE',  ( -27.67932024734484031, 8.922843848540177092, -8.046304320001306465 ) ) ;
#16437 = EDGE_LOOP ( 'NONE', ( #9362, #6640, #6469, #63738 ) ) ;
#16438 = CARTESIAN_POINT ( 'NONE',  ( 0.2648978790185593790, 9.465406350830713578, -7.769924372105106336 ) ) ;
#16439 = EDGE_CURVE ( 'NONE', #21988, #45204, #22937, .T. ) ;
#16440 = ORIENTED_EDGE ( 'NONE', *, *, #1302, .F. ) ;
#16441 = CARTESIAN_POINT ( 'NONE',  ( 22.83619264212346067, -9.759093346436447547, -6.990946369225183865 ) ) ;
#16442 = DIRECTION ( 'NONE',  ( 0.000000000000000000, -0.3193015301359669600, -0.9476531711828067861 ) ) ;
#16443 = CIRCLE ( 'NONE', #8979, 12.18649999999999700 ) ;
#16444 = CARTESIAN_POINT ( 'NONE',  ( 2.245754705088394143, -7.635057163463319974, -0.1113317465207585011 ) ) ;
#16445 = ORIENTED_EDGE ( 'NONE', *, *, #10221, .F. ) ;
#16446 = CARTESIAN_POINT ( 'NONE',  ( 35.00000000000000000, -1.591260454995155671, 12.08216339958901742 ) ) ;
#16447 = EDGE_CURVE ( 'NONE', #29014, #10001, #43911, .T. ) ;
#16448 = DIRECTION ( 'NONE',  ( -1.000000000000000000, 0.000000000000000000, 0.000000000000000000 ) ) ;
#16449 = CARTESIAN_POINT ( 'NONE',  ( 2.000000000000001776, -6.250523986463956128, -3.007653927006670003 ) ) ;
#16450 = ORIENTED_EDGE ( 'NONE', *, *, #1091, .F. ) ;
#16451 = ORIENTED_EDGE ( 'NONE', *, *, #35872, .F. ) ;
#16452 = CARTESIAN_POINT ( 'NONE',  ( 0.2657645697724694833, 12.03308811492268759, 2.275433120353130612 ) ) ;
#16453 = VERTEX_POINT ( 'NONE', #22605 ) ;
#16454 = EDGE_CURVE ( 'NONE', #12453, #2190, #23756, .T. ) ;
#16455 = VERTEX_POINT ( 'NONE', #27252 ) ;
#16456 = B_SPLINE_CURVE_WITH_KNOTS ( 'NONE', 3,
 ( #5210, #559, #45763, #65693, #45426, #20500, #40784, #866, #61065, #15494, #51753, #35760, #41089, #61368, #15812, #56394 ),
 .UNSPECIFIED., .F., .F.,
 ( 4, 3, 3, 3, 3, 4 ),
 ( 2.948971425439945768E-15, 0.0002126834539179795619, 0.0004253519300366472239, 0.0006380165497224497828, 0.0007442707582428645472, 0.0009453531351415651613 ),
 .UNSPECIFIED. ) ;
#16457 = DIRECTION ( 'NONE',  ( 1.000000000000000000, 0.000000000000000000, 0.000000000000000000 ) ) ;
#16458 = DIRECTION ( 'NONE',  ( 0.000000000000000000, -0.8169148498130212044, 0.5767582926625058892 ) ) ;
#16459 = CARTESIAN_POINT ( 'NONE',  ( -22.27706485742869091, 2.580541389029920030, 2.625261754997667119 ) ) ;
#16460 = CARTESIAN_POINT ( 'NONE',  ( -22.29018399051993882, 1.024613686459469930, 3.576688584977234964 ) ) ;
#16461 = DIRECTION ( 'NONE',  ( 1.000000000000000000, -0.000000000000000000, 0.000000000000000000 ) ) ;
#16462 = CARTESIAN_POINT ( 'NONE',  ( -10.00003325919894692, -3.438199368958688940, -11.49838662738022954 ) ) ;
#16463 = AXIS2_PLACEMENT_3D ( 'NONE', #35334, #64939, #5773 ) ;
#16464 = CARTESIAN_POINT ( 'NONE',  ( 22.78397477906666779, 3.290341966830230724, -11.54089583822152854 ) ) ;
#16465 = EDGE_LOOP ( 'NONE', ( #14731, #41086, #12604, #4831 ) ) ;
#16466 = CARTESIAN_POINT ( 'NONE',  ( 5.516018279890452902, 0.003191189039764439229, -0.005976902763918727837 ) ) ;
#16467 = AXIS2_PLACEMENT_3D ( 'NONE', #8086, #9053, #3106 ) ;
#16468 = SURFACE_SIDE_STYLE ('',( #55724 ) ) ;
#16469 = EDGE_CURVE ( 'NONE', #23887, #18752, #64074, .T. ) ;
#16470 = CARTESIAN_POINT ( 'NONE',  ( 0.3218525148189834151, 4.423735011438986398, -11.43947393562872605 ) ) ;
#16471 = CARTESIAN_POINT ( 'NONE',  ( 1.937114397841935398, -9.228205347192510288, 8.920887662793440143 ) ) ;
#16472 = EDGE_CURVE ( 'NONE', #65189, #14785, #35398, .T. ) ;
#16473 = AXIS2_PLACEMENT_3D ( 'NONE', #58522, #33234, #18286 ) ;
#16474 = DIRECTION ( 'NONE',  ( 0.000000000000000000, 0.000000000000000000, 1.000000000000000000 ) ) ;
#16475 = CARTESIAN_POINT ( 'NONE',  ( 2.510731577322978136, 1.829398357709037803, -11.86532612209469484 ) ) ;
#16476 = ADVANCED_FACE ( 'NONE', ( #63156 ), #53185, .T. ) ;
#16477 = CARTESIAN_POINT ( 'NONE',  ( 47.00000000000000711, 4.705694406421931860E-17, -3.469127814946512892E-15 ) ) ;
#16478 = ORIENTED_EDGE ( 'NONE', *, *, #28667, .T. ) ;
#16479 = DIRECTION ( 'NONE',  ( 0.000000000000000000, -1.000000000000000000, 0.000000000000000000 ) ) ;
#16480 = DIRECTION ( 'NONE',  ( 0.000000000000000000, 0.7617968321374856133, 0.6478160128811973895 ) ) ;
#16481 = DIRECTION ( 'NONE',  ( 0.000000000000000000, -0.01356324068818000328, 0.9999080150203990547 ) ) ;
#16482 = CARTESIAN_POINT ( 'NONE',  ( 14.81924285005721131, -34.67057711548305576, 7.362581078980241500 ) ) ;
#16483 = VECTOR ( 'NONE', #19380, 1000.000000000000000 ) ;
#16484 = CARTESIAN_POINT ( 'NONE',  ( 9.274649623867711412, 2.850288540387552416, -13.19772255816346807 ) ) ;
#16485 = CARTESIAN_POINT ( 'NONE',  ( -24.85888762414873909, -9.907586878531645880, 9.176240764607326739 ) ) ;
#16486 = ORIENTED_EDGE ( 'NONE', *, *, #21713, .T. ) ;
#16487 = CARTESIAN_POINT ( 'NONE',  ( -27.28563798457903289, -2.487904455214891897, -1.483130241384915893 ) ) ;
#16488 = DIRECTION ( 'NONE',  ( 1.000000000000000000, -0.000000000000000000, 0.000000000000000000 ) ) ;
#16489 = FACE_OUTER_BOUND ( 'NONE', #31454, .T. ) ;
#16490 = EDGE_LOOP ( 'NONE', ( #13599, #62362 ) ) ;
#16491 = CARTESIAN_POINT ( 'NONE',  ( 2.556980015513956150, 6.815084337351906107, 3.668282146013149170 ) ) ;
#16492 = CARTESIAN_POINT ( 'NONE',  ( 5.515188684475870851, 0.003857086913166444826, -0.003709313826050250878 ) ) ;
#16493 = DIRECTION ( 'NONE',  ( 1.000000000000000000, 0.000000000000000000, 0.000000000000000000 ) ) ;
#16495 = EDGE_LOOP ( 'NONE', ( #45308, #7323, #7010, #62154 ) ) ;
#16494 = CARTESIAN_POINT ( 'NONE',  ( 2.931247277082679847, 0.9994150891046325036, 7.800615791174658753 ) ) ;
#16496 = CARTESIAN_POINT ( 'NONE',  ( 19.56743653832047158, -33.00000000000000000, 5.000000000000007994 ) ) ;
#16497 = CIRCLE ( 'NONE', #2764, 5.000000000000000888 ) ;
#16498 = EDGE_CURVE ( 'NONE', #20276, #17391, #7632, .T. ) ;
#16499 = CARTESIAN_POINT ( 'NONE',  ( -25.42680463514451006, -3.871126486605853678, -0.3277218550990906309 ) ) ;
#16500 = ORIENTED_EDGE ( 'NONE', *, *, #16527, .T. ) ;
#16501 = DIRECTION ( 'NONE',  ( -1.000000000000000000, 0.000000000000000000, 0.000000000000000000 ) ) ;
#16502 = EDGE_CURVE ( 'NONE', #3105, #62664, #40728, .T. ) ;
#16503 = CARTESIAN_POINT ( 'NONE',  ( 35.00000000000000000, 6.753013023069713405, -10.14433819232436917 ) ) ;
#16505 = CARTESIAN_POINT ( 'NONE',  ( 2.000000000000001776, -3.859771122243078167, 5.613913289150019637 ) ) ;
#16504 =( BOUNDED_CURVE ( )  B_SPLINE_CURVE ( 3, ( #23397, #45314, #56265, #34982 ),
 .UNSPECIFIED., .F., .F. ) 
 B_SPLINE_CURVE_WITH_KNOTS ( ( 4, 4 ),
 ( 0.7743326424653215190, 0.8261054116032431338 ),
 .UNSPECIFIED. ) 
 CURVE ( )  GEOMETRIC_REPRESENTATION_ITEM ( )  RATIONAL_B_SPLINE_CURVE ( ( 1.000000000000000000, 0.9997766441710536078, 0.9997766441710536078, 1.000000000000000000 ) ) 
 REPRESENTATION_ITEM ( '' )  );
#16506 = FACE_OUTER_BOUND ( 'NONE', #8394, .T. ) ;
#16507 = FACE_OUTER_BOUND ( 'NONE', #498, .T. ) ;
#16508 = DIRECTION ( 'NONE',  ( 1.000000000000000000, 0.000000000000000000, 0.000000000000000000 ) ) ;
#16510 = EDGE_LOOP ( 'NONE', ( #36195, #61872, #31467, #20115 ) ) ;
#16509 = DIRECTION ( 'NONE',  ( 0.000000000000000000, -0.01356324068817991828, 0.9999080150203990547 ) ) ;
#16511 = ORIENTED_EDGE ( 'NONE', *, *, #50149, .F. ) ;
#16512 = DIRECTION ( 'NONE',  ( 1.000000000000000000, 0.000000000000000000, 0.000000000000000000 ) ) ;
#16513 = ORIENTED_EDGE ( 'NONE', *, *, #8361, .T. ) ;
#16514 = ADVANCED_FACE ( 'NONE', ( #32543 ), #53533, .T. ) ;
#16515 = SHAPE_REPRESENTATION_RELATIONSHIP ( 'NONE' , 'NONE' ,  #39018, #28612 ) ;
#16516 = DIRECTION ( 'NONE',  ( 0.000000000000000000, 0.000000000000000000, 1.000000000000000000 ) ) ;
#16517 = CARTESIAN_POINT ( 'NONE',  ( 0.9232058338315048962, -9.791640253608198563, 7.723624854284683927 ) ) ;
#16518 = CARTESIAN_POINT ( 'NONE',  ( 0.2655924914740778742, 4.147079829127409134, -11.52280271232866582 ) ) ;
#16519 = ORIENTED_EDGE ( 'NONE', *, *, #58437, .F. ) ;
#16520 = CARTESIAN_POINT ( 'NONE',  ( 1.719304012338199517, 0.000000000000000000, 0.000000000000000000 ) ) ;
#16521 = AXIS2_PLACEMENT_3D ( 'NONE', #13590, #28901, #34203 ) ;
#16522 = CARTESIAN_POINT ( 'NONE',  ( 37.00000000000000711, -9.677500615117850202, 6.657191900728419043 ) ) ;
#16523 = FACE_BOUND ( 'NONE', #27943, .T. ) ;
#16524 = ORIENTED_EDGE ( 'NONE', *, *, #23685, .T. ) ;
#16525 = ORIENTED_EDGE ( 'NONE', *, *, #33665, .T. ) ;
#16526 = LINE ( 'NONE', #10870, #10935 ) ;
#16527 = EDGE_CURVE ( 'NONE', #39221, #27370, #49253, .T. ) ;
#16528 = EDGE_CURVE ( 'NONE', #60783, #39489, #11818, .T. ) ;
#16529 = ORIENTED_EDGE ( 'NONE', *, *, #756, .T. ) ;
#16530 = DIRECTION ( 'NONE',  ( 1.000000000000000000, 0.000000000000000000, 0.000000000000000000 ) ) ;
#16531 = CARTESIAN_POINT ( 'NONE',  ( -35.00000000000000000, 3.287724142101577485, -11.73463472867572932 ) ) ;
#16532 = CARTESIAN_POINT ( 'NONE',  ( 9.777492251018479408, 2.011184903788696410, 13.35065112715840563 ) ) ;
#16533 = EDGE_CURVE ( 'NONE', #12570, #30330, #33558, .T. ) ;
#16534 = AXIS2_PLACEMENT_3D ( 'NONE', #23814, #14765, #19470 ) ;
#16535 = DIRECTION ( 'NONE',  ( 0.000000000000000000, 0.01356324068817998940, -0.9999080150203990547 ) ) ;
#16536 = DIRECTION ( 'NONE',  ( 0.000000000000000000, -0.2618041379715496664, 0.9651210252299831094 ) ) ;
#16537 = CARTESIAN_POINT ( 'NONE',  ( 2.899286259009688838, -7.788326766693359104, 1.011320371384315298 ) ) ;
#16538 = LINE ( 'NONE', #15845, #20575 ) ;
#16539 = EDGE_LOOP ( 'NONE', ( #45558, #22875, #17534, #17698 ) ) ;
#16540 = DIRECTION ( 'NONE',  ( 1.000000000000000000, -0.000000000000000000, 0.000000000000000000 ) ) ;
#16541 = VERTEX_POINT ( 'NONE', #62818 ) ;
#16542 = LINE ( 'NONE', #11858, #33208 ) ;
#16543 = CARTESIAN_POINT ( 'NONE',  ( -35.05175862995318425, 0.01212835938693528071, -0.003331684148556030012 ) ) ;
#16544 = CARTESIAN_POINT ( 'NONE',  ( 35.00000000000000000, 5.644643009979216863, 10.30098186818242922 ) ) ;
#16545 = CARTESIAN_POINT ( 'NONE',  ( 2.241311220309555097, -3.897297589552028096, 6.564680916077786144 ) ) ;
#16546 = CARTESIAN_POINT ( 'NONE',  ( 0.2648978790185619880, -10.67083876753487637, -6.008231198269095685 ) ) ;
#16547 = LINE ( 'NONE', #27168, #13844 ) ;
#16548 = EDGE_CURVE ( 'NONE', #42325, #12979, #58614, .T. ) ;
#16549 = ORIENTED_EDGE ( 'NONE', *, *, #46011, .F. ) ;
#16550 = EDGE_LOOP ( 'NONE', ( #21526, #17984, #1622, #28318 ) ) ;
#16551 = DIRECTION ( 'NONE',  ( -1.000000000000000000, 0.000000000000000000, -0.000000000000000000 ) ) ;
#16552 = EDGE_CURVE ( 'NONE', #55547, #14742, #26099, .T. ) ;
#16553 = B_SPLINE_CURVE_WITH_KNOTS ( 'NONE', 3,
 ( #9660, #60882, #34290, #35263, #24984, #54604, #9027 ),
 .UNSPECIFIED., .F., .F.,
 ( 4, 3, 4 ),
 ( 7.780893502321468812E-16, 0.002398160485434359685, 0.005002426799377646463 ),
 .UNSPECIFIED. ) ;
#16554 = ORIENTED_EDGE ( 'NONE', *, *, #30700, .F. ) ;
#16555 = CARTESIAN_POINT ( 'NONE',  ( 0.2653519890538384995, 1.477274386607676477E-15, 12.24619734961521189 ) ) ;
#16556 = DIRECTION ( 'NONE',  ( 0.000000000000000000, 0.000000000000000000, 1.000000000000000000 ) ) ;
#16557 = CARTESIAN_POINT ( 'NONE',  ( 35.00000000000000000, -0.3137578094510123927, -12.74613886779084737 ) ) ;
#16558 = CARTESIAN_POINT ( 'NONE',  ( 2.298277635560284082, 1.491234112749290963, -7.506689984432308727 ) ) ;
#16559 = ORIENTED_EDGE ( 'NONE', *, *, #1952, .T. ) ;
#16560 = DIRECTION ( 'NONE',  ( 1.000000000000000000, 0.000000000000000000, 0.000000000000000000 ) ) ;
#16561 = DIRECTION ( 'NONE',  ( -1.000000000000000000, 0.000000000000000000, 0.000000000000000000 ) ) ;
#16562 = DIRECTION ( 'NONE',  ( -1.000000000000000000, 0.000000000000000000, -0.000000000000000000 ) ) ;
#16563 = CARTESIAN_POINT ( 'NONE',  ( -21.17861794710831091, 25.00000000000000000, -3.604945070120774808 ) ) ;
#16564 = CIRCLE ( 'NONE', #10182, 12.75000000000000178 ) ;
#16565 = CARTESIAN_POINT ( 'NONE',  ( -36.00000000000000711, 2.865935305911801123, -12.42372387097879383 ) ) ;
#16566 = CARTESIAN_POINT ( 'NONE',  ( 35.00000000000000000, 11.05394794832829497, -5.130401251914769922 ) ) ;
#16567 = VECTOR ( 'NONE', #13507, 1000.000000000000000 ) ;
#16568 = ORIENTED_EDGE ( 'NONE', *, *, #57234, .F. ) ;
#16569 = DIRECTION ( 'NONE',  ( -1.000000000000000000, -0.000000000000000000, 0.000000000000000000 ) ) ;
#16570 = ORIENTED_EDGE ( 'NONE', *, *, #35554, .T. ) ;
#16571 = DIRECTION ( 'NONE',  ( -1.000000000000000000, 0.000000000000000000, 0.000000000000000000 ) ) ;
#16572 = DIRECTION ( 'NONE',  ( 0.000000000000000000, 0.000000000000000000, 1.000000000000000000 ) ) ;
#16573 = DIRECTION ( 'NONE',  ( 0.000000000000000000, 0.2149704402110177992, 0.9766205557100881007 ) ) ;
#16574 = CARTESIAN_POINT ( 'NONE',  ( -35.04683013664716640, -0.006090538653939255552, 0.01075274317998137219 ) ) ;
#16575 = B_SPLINE_CURVE_WITH_KNOTS ( 'NONE', 3,
 ( #21802, #53022, #37394, #26771, #57363, #1837, #21460, #22103, #47069, #62649 ),
 .UNSPECIFIED., .F., .F.,
 ( 4, 3, 3, 4 ),
 ( 0.0001763147164361759890, 0.0002097400188389094170, 0.0002811534801551362692, 0.0003526297678872490409 ),
 .UNSPECIFIED. ) ;
#16576 = CARTESIAN_POINT ( 'NONE',  ( -37.00000000000000711, -5.636262487437237567, -10.80478261802188023 ) ) ;
#16577 = AXIS2_PLACEMENT_3D ( 'NONE', #56255, #11046, #51626 ) ;
#16578 = ORIENTED_EDGE ( 'NONE', *, *, #2604, .T. ) ;
#16579 = VERTEX_POINT ( 'NONE', #19242 ) ;
#16580 = CARTESIAN_POINT ( 'NONE',  ( -25.00000000000000355, -30.00000000000000000, 24.00000000000000000 ) ) ;
#16581 = VERTEX_POINT ( 'NONE', #55467 ) ;
#16582 = EDGE_CURVE ( 'NONE', #10662, #2752, #43859, .T. ) ;
#16583 = CARTESIAN_POINT ( 'NONE',  ( -35.00000000000000000, -2.021542716731318912, -12.01765980939844169 ) ) ;
#16584 = DIRECTION ( 'NONE',  ( 1.000000000000000000, 0.000000000000000000, -0.000000000000000000 ) ) ;
#16585 = FACE_OUTER_BOUND ( 'NONE', #1116, .T. ) ;
#16586 = LINE ( 'NONE', #26229, #53450 ) ;
#16587 = CARTESIAN_POINT ( 'NONE',  ( 2.653899356898011153, 7.767552767343518738, -0.2611590963040564817 ) ) ;
#16588 = CARTESIAN_POINT ( 'NONE',  ( -11.40165637462999904, -7.508992741355383416, 11.21895841913464409 ) ) ;
#16589 = CARTESIAN_POINT ( 'NONE',  ( -9.082707185599058874, -2.483053339704398788, 11.74128942805037212 ) ) ;
#16590 = VERTEX_POINT ( 'NONE', #18618 ) ;
#16591 = CARTESIAN_POINT ( 'NONE',  ( 0.9232167919969161973, -5.871274944231774207, 10.99620217063213623 ) ) ;
#16592 = VERTEX_POINT ( 'NONE', #38874 ) ;
#16593 = DIRECTION ( 'NONE',  ( -1.000000000000000000, 0.000000000000000000, 0.000000000000000000 ) ) ;
#16594 = CARTESIAN_POINT ( 'NONE',  ( 16.87411378711497179, 11.83810385330096082, 6.535220105381315037 ) ) ;
#16595 = EDGE_CURVE ( 'NONE', #13015, #37639, #47152, .T. ) ;
#16596 = DIRECTION ( 'NONE',  ( -1.000000000000000000, 0.000000000000000000, -0.000000000000000000 ) ) ;
#16597 = ORIENTED_EDGE ( 'NONE', *, *, #5118, .F. ) ;
#16598 = DIRECTION ( 'NONE',  ( 0.000000000000000000, 0.7621620551276333533, 0.6473862847818311339 ) ) ;
#16599 = CARTESIAN_POINT ( 'NONE',  ( -35.00000000000000000, 12.05416472667165806, 1.791059740004466994 ) ) ;
#16600 = CARTESIAN_POINT ( 'NONE',  ( 2.889800649504073782, -4.645655809191337582, -3.986129653162696407 ) ) ;
#16601 = EDGE_LOOP ( 'NONE', ( #38499, #11191, #44066, #34647 ) ) ;
#16602 = ORIENTED_EDGE ( 'NONE', *, *, #55402, .F. ) ;
#16603 = CARTESIAN_POINT ( 'NONE',  ( 37.00000000000000711, -11.42599468261426132, 4.237620530777920891 ) ) ;
#16604 = VERTEX_POINT ( 'NONE', #8603 ) ;
#16605 = EDGE_CURVE ( 'NONE', #60108, #60760, #34365, .T. ) ;
#16606 = DIRECTION ( 'NONE',  ( -1.000000000000000000, -0.000000000000000000, 0.000000000000000000 ) ) ;
#16607 = ORIENTED_EDGE ( 'NONE', *, *, #62738, .F. ) ;
#16608 = ORIENTED_EDGE ( 'NONE', *, *, #12539, .T. ) ;
#16609 = VERTEX_POINT ( 'NONE', #39512 ) ;
#16610 = CARTESIAN_POINT ( 'NONE',  ( 0.3223008802179245791, 4.423848692584686937, 11.43958962819733571 ) ) ;
#16611 = EDGE_CURVE ( 'NONE', #65410, #725, #42856, .T. ) ;
#16612 = DIRECTION ( 'NONE',  ( 0.000000000000000000, 0.000000000000000000, 1.000000000000000000 ) ) ;
#16613 = LINE ( 'NONE', #7269, #43702 ) ;
#16614 = DIRECTION ( 'NONE',  ( 0.000000000000000000, -0.9903235168508566222, -0.1387779952735712363 ) ) ;
#16615 = DIRECTION ( 'NONE',  ( 0.000000000000000000, -0.01356324068818000328, 0.9999080150203990547 ) ) ;
#16616 = VERTEX_POINT ( 'NONE', #59809 ) ;
#16617 = AXIS2_PLACEMENT_3D ( 'NONE', #26386, #41680, #46031 ) ;
#16618 = CARTESIAN_POINT ( 'NONE',  ( 2.080613030138688480, 0.000000000000000000, 4.000000000000000000 ) ) ;
#16619 = CIRCLE ( 'NONE', #33560, 6.936499999999988120 ) ;
#16620 = VERTEX_POINT ( 'NONE', #13901 ) ;
#16621 = FACE_OUTER_BOUND ( 'NONE', #26847, .T. ) ;
#16622 = CARTESIAN_POINT ( 'NONE',  ( -3.548017078132182700, 11.40818985387241824, 7.227869169360847224 ) ) ;
#16623 = CARTESIAN_POINT ( 'NONE',  ( 35.00000000000000000, 4.705694406421931860E-17, -3.469127814946512892E-15 ) ) ;
#16624 = CARTESIAN_POINT ( 'NONE',  ( 0.5572780756290603987, 9.649189244958913392, -7.697784780878635935 ) ) ;
#16625 = CARTESIAN_POINT ( 'NONE',  ( 5.515539859299206427, -0.001886660928063928948, -0.005751553894234946035 ) ) ;
#16626 = CARTESIAN_POINT ( 'NONE',  ( 2.705197763288547552, -7.783989928191463292, -0.2797837188787176133 ) ) ;
#16627 = ADVANCED_FACE ( 'NONE', ( #29224 ), #33973, .F. ) ;
#16628 = EDGE_LOOP ( 'NONE', ( #34202, #43449, #654, #63841 ) ) ;
#16629 = CARTESIAN_POINT ( 'NONE',  ( 5.514624014163232779, -0.004137701579365678402, -0.0001700579043834388670 ) ) ;
#16630 = EDGE_LOOP ( 'NONE', ( #25428, #24248, #25587, #13993 ) ) ;
#16631 = DIRECTION ( 'NONE',  ( 0.000000000000000000, 1.000000000000000000, 0.000000000000000000 ) ) ;
#16632 = CARTESIAN_POINT ( 'NONE',  ( -2.496508956744591057, -25.79293017570256552, -15.56347233531499441 ) ) ;
#16633 = CARTESIAN_POINT ( 'NONE',  ( 0.3675815128205912052, 7.689697408877274931, 9.574637318041988365 ) ) ;
#16634 = CARTESIAN_POINT ( 'NONE',  ( 3.152665057735760445, 4.725420687649616092, -6.378477742801607953 ) ) ;
#16635 = LINE ( 'NONE', #36242, #57251 ) ;
#16636 = VERTEX_POINT ( 'NONE', #15860 ) ;
#16637 = DIRECTION ( 'NONE',  ( -1.000000000000000000, 0.000000000000000000, 0.000000000000000000 ) ) ;
#16638 = CYLINDRICAL_SURFACE ( 'NONE', #1527, 5.000000000000000000 ) ;
#16639 = DIRECTION ( 'NONE',  ( 0.000000000000000000, 0.000000000000000000, 1.000000000000000000 ) ) ;
#16640 = CARTESIAN_POINT ( 'NONE',  ( 8.843349564587759559, -31.89871022336092921, -13.45657735392536480 ) ) ;
#16641 = EDGE_CURVE ( 'NONE', #34196, #17686, #57737, .T. ) ;
#16642 = CARTESIAN_POINT ( 'NONE',  ( 5.516018279890452902, 0.0002248006052446666569, -0.006771744149385742172 ) ) ;
#16643 = CARTESIAN_POINT ( 'NONE',  ( 2.241528039335008327, 2.596349773934880201, 7.179411278563565091 ) ) ;
#16644 = DIRECTION ( 'NONE',  ( 1.000000000000000000, -0.000000000000000000, 0.000000000000000000 ) ) ;
#16645 = AXIS2_PLACEMENT_3D ( 'NONE', #12485, #38429, #23469 ) ;
#16646 = CIRCLE ( 'NONE', #24099, 12.75000000000000178 ) ;
#16647 = EDGE_LOOP ( 'NONE', ( #41592, #9049, #49556, #16414 ) ) ;
#16649 = VERTEX_POINT ( 'NONE', #61111 ) ;
#16648 = EDGE_CURVE ( 'NONE', #11726, #59597, #41462, .T. ) ;
#16650 = DIRECTION ( 'NONE',  ( 1.000000000000000000, 0.000000000000000000, 0.000000000000000000 ) ) ;
#16651 = CARTESIAN_POINT ( 'NONE',  ( 39.62372872010316627, -1.894461972532903271, 19.09391518418254208 ) ) ;
#16652 = CARTESIAN_POINT ( 'NONE',  ( -29.66426065917772092, -2.171908341933164621, 13.32952346240084118 ) ) ;
#16653 = DIRECTION ( 'NONE',  ( 0.000000000000000000, -0.01356324068817999114, 0.9999080150203989437 ) ) ;
#16654 = EDGE_CURVE ( 'NONE', #11684, #60382, #59869, .T. ) ;
#16655 = ORIENTED_EDGE ( 'NONE', *, *, #25131, .F. ) ;
#16656 = VERTEX_POINT ( 'NONE', #30831 ) ;
#16657 = ORIENTED_EDGE ( 'NONE', *, *, #35083, .F. ) ;
#16658 = DIRECTION ( 'NONE',  ( -1.000000000000000000, 0.000000000000000000, 0.000000000000000000 ) ) ;
#16659 = CARTESIAN_POINT ( 'NONE',  ( 22.21055375121776976, 11.96926186085322286, -0.8606626411553330858 ) ) ;
#16660 = EDGE_CURVE ( 'NONE', #59695, #2788, #41808, .T. ) ;
#16661 = ORIENTED_EDGE ( 'NONE', *, *, #60909, .F. ) ;
#16662 = LINE ( 'NONE', #20979, #29407 ) ;
#16663 = CARTESIAN_POINT ( 'NONE',  ( 35.00000000000000000, -4.309077947445731027, -10.92721691015454510 ) ) ;
#16664 = VERTEX_POINT ( 'NONE', #56108 ) ;
#16665 = CARTESIAN_POINT ( 'NONE',  ( 35.00000000000000000, 12.14284015767851166, 1.030638227056429157 ) ) ;
#16666 = CARTESIAN_POINT ( 'NONE',  ( 14.53304282576173634, -29.99999999999999289, -3.713578627762628592 ) ) ;
#16667 = DIRECTION ( 'NONE',  ( -1.000000000000000000, 0.000000000000000000, -0.000000000000000000 ) ) ;
#16668 = VERTEX_POINT ( 'NONE', #50807 ) ;
#16669 = DIRECTION ( 'NONE',  ( 0.000000000000000000, 0.01356324068817998940, -0.9999080150203990547 ) ) ;
#16670 = VERTEX_POINT ( 'NONE', #20554 ) ;
#16671 = EDGE_CURVE ( 'NONE', #8268, #18329, #29064, .T. ) ;
#16672 = LINE ( 'NONE', #41611, #30521 ) ;
#16673 = CARTESIAN_POINT ( 'NONE',  ( 2.241352910868908310, 4.843133558968128582, 5.901537464758471074 ) ) ;
#16674 = CARTESIAN_POINT ( 'NONE',  ( 2.000000000000001776, 0.000000000000000000, 0.000000000000000000 ) ) ;
#16675 = CARTESIAN_POINT ( 'NONE',  ( -36.00000000000000711, -11.32068061209291265, -5.865551165831199398 ) ) ;
#16676 = CARTESIAN_POINT ( 'NONE',  ( 35.00000000000000000, -11.59095880812006385, 1.903127969211307224 ) ) ;
#16677 = CARTESIAN_POINT ( 'NONE',  ( 8.932556049095349948, 2.405355177192989746, 11.75892528794417835 ) ) ;
#16678 = DIRECTION ( 'NONE',  ( -1.000000000000000000, 0.000000000000000000, 0.000000000000000000 ) ) ;
#16679 = CARTESIAN_POINT ( 'NONE',  ( 0.2648978790185584908, 4.063980959785046032, 11.55204314799265042 ) ) ;
#16680 = EDGE_LOOP ( 'NONE', ( #54715, #3550, #53871, #24758 ) ) ;
#16681 = EDGE_CURVE ( 'NONE', #50289, #44901, #36820, .T. ) ;
#16682 = DIRECTION ( 'NONE',  ( -1.000000000000000000, 0.000000000000000000, 0.000000000000000000 ) ) ;
#16683 = ORIENTED_EDGE ( 'NONE', *, *, #4959, .T. ) ;
#16684 = LINE ( 'NONE', #36955, #60387 ) ;
#16685 = FACE_OUTER_BOUND ( 'NONE', #28661, .T. ) ;
#16686 = EDGE_LOOP ( 'NONE', ( #59547, #61005, #30977, #35567 ) ) ;
#16687 = CARTESIAN_POINT ( 'NONE',  ( -35.00000000000000000, 11.68758509253248334, -1.171570255487489609 ) ) ;
#16688 = CARTESIAN_POINT ( 'NONE',  ( -35.00000000000000000, 0.000000000000000000, 0.000000000000000000 ) ) ;
#16689 = CARTESIAN_POINT ( 'NONE',  ( -4.806344283790351390, -7.508992741355383416, 25.00000000000000000 ) ) ;
#16690 = AXIS2_PLACEMENT_3D ( 'NONE', #7341, #36947, #2389 ) ;
#16691 = B_SPLINE_CURVE_WITH_KNOTS ( 'NONE', 3,
 ( #28116, #37757, #33427, #2184, #54035, #42384, #58050, #37421, #48409, #12465 ),
 .UNSPECIFIED., .F., .F.,
 ( 4, 3, 3, 4 ),
 ( 8.673617379884035472E-19, 6.607638129004486172E-05, 9.911389841680541231E-05, 0.0001667630577588623383 ),
 .UNSPECIFIED. ) ;
#16692 = DIRECTION ( 'NONE',  ( -1.000000000000000000, 0.000000000000000000, 0.000000000000000000 ) ) ;
#16693 = VERTEX_POINT ( 'NONE', #16213 ) ;
#16694 = VERTEX_POINT ( 'NONE', #62101 ) ;
#16695 = CARTESIAN_POINT ( 'NONE',  ( -18.33734242530290004, -4.538935765794358979, -11.11102257328130172 ) ) ;
#16696 =( BOUNDED_SURFACE ( )  B_SPLINE_SURFACE ( 3, 1, ( 
 ( #8816, #59687 ),
 ( #29105, #3849 ),
 ( #49708, #64642 ),
 ( #19114, #39385 ) ),
 .UNSPECIFIED., .F., .F., .F. ) 
 B_SPLINE_SURFACE_WITH_KNOTS ( ( 4, 4 ),
 ( 2, 2 ),
 ( 0.000000000000000000, 1.000000000000000000 ),
 ( 0.000000000000000000, 1.000000000000000000 ),
 .UNSPECIFIED. ) 
 GEOMETRIC_REPRESENTATION_ITEM ( )  RATIONAL_B_SPLINE_SURFACE ( (
 ( 1.000000000000000000, 1.000000000000000000),
 ( 0.9932032654565553509, 0.8386279382598736953),
 ( 0.9932032654565553509, 0.8386279382598736953),
 ( 1.000000000000000000, 1.000000000000000000) ) ) 
 REPRESENTATION_ITEM ( '' )  SURFACE ( )  );
#16697 = ORIENTED_EDGE ( 'NONE', *, *, #50173, .F. ) ;
#16698 = DIRECTION ( 'NONE',  ( -1.000000000000000000, 0.000000000000000000, -0.000000000000000000 ) ) ;
#16699 = CARTESIAN_POINT ( 'NONE',  ( -37.00000000000000711, 0.000000000000000000, 0.000000000000000000 ) ) ;
#16700 = CARTESIAN_POINT ( 'NONE',  ( 5.530133899448235191, 0.01594518557925582100, 0.001124651387255043086 ) ) ;
#16701 = ORIENTED_EDGE ( 'NONE', *, *, #24564, .F. ) ;
#16702 = DIRECTION ( 'NONE',  ( -1.000000000000000000, 0.000000000000000000, -0.000000000000000000 ) ) ;
#16703 = EDGE_CURVE ( 'NONE', #42839, #49489, #31192, .T. ) ;
#16704 = CARTESIAN_POINT ( 'NONE',  ( 2.000000000000001776, 1.145812388885215194, -6.715725538143608730 ) ) ;
#16705 = CARTESIAN_POINT ( 'NONE',  ( -25.00000000000000355, -3.797884998337192286, -23.99999999999999289 ) ) ;
#16706 = B_SPLINE_CURVE_WITH_KNOTS ( 'NONE', 3,
 ( #30152, #45122, #41095, #65384, #45434, #65699, #20170, #40442, #60740, #15179, #52418, #57068, #11819, #31767, #46427, #52738, #7162, #11184, #1213 ),
 .UNSPECIFIED., .F., .F.,
 ( 4, 3, 3, 3, 3, 3, 4 ),
 ( 9.899098333708122648E-18, 4.457896483014865609E-05, 6.639290541542039676E-05, 8.820687556478868318E-05, 0.0001100173248778915164, 0.0001545671401658093647, 0.0001830328308068584413 ),
 .UNSPECIFIED. ) ;
#16707 = CYLINDRICAL_SURFACE ( 'NONE', #7658, 5.000000000000000888 ) ;
#16708 = CARTESIAN_POINT ( 'NONE',  ( 37.00000000000000711, 11.38112321385050585, -2.905556151562669331 ) ) ;
#16709 = DIRECTION ( 'NONE',  ( 0.000000000000000000, 0.01356324068818000848, -0.9999080150203990547 ) ) ;
#16710 = DIRECTION ( 'NONE',  ( 0.000000000000000000, -0.01356324068817999114, 0.9999080150203989437 ) ) ;
#16711 = CARTESIAN_POINT ( 'NONE',  ( 0.2648978790185602672, 7.972372351883029395, 9.295532325666474804 ) ) ;
#16712 = VECTOR ( 'NONE', #10688, 1000.000000000000000 ) ;
#16713 = EDGE_CURVE ( 'NONE', #29713, #25020, #37552, .T. ) ;
#16714 = EDGE_LOOP ( 'NONE', ( #40894, #42648, #24454, #50704 ) ) ;
#16715 = CARTESIAN_POINT ( 'NONE',  ( 2.000000000000001776, -6.812627895098285258, -0.04423456934733380197 ) ) ;
#16716 = CARTESIAN_POINT ( 'NONE',  ( 11.74548640120467979, 25.00000000000000000, -8.184666801472349817 ) ) ;
#16717 = ORIENTED_EDGE ( 'NONE', *, *, #7381, .F. ) ;
#16718 = EDGE_CURVE ( 'NONE', #25248, #51431, #11228, .T. ) ;
#16719 = FACE_OUTER_BOUND ( 'NONE', #65628, .T. ) ;
#16720 = DIRECTION ( 'NONE',  ( 0.000000000000000000, -0.01356324068817998940, 0.9999080150203990547 ) ) ;
#16721 = ORIENTED_EDGE ( 'NONE', *, *, #59149, .F. ) ;
#16722 = CARTESIAN_POINT ( 'NONE',  ( -22.51237073810381162, -2.023441661740717379, 3.933875531624984490 ) ) ;
#16723 = EDGE_CURVE ( 'NONE', #7740, #924, #56807, .T. ) ;
#16724 = ORIENTED_EDGE ( 'NONE', *, *, #48114, .T. ) ;
#16725 = CARTESIAN_POINT ( 'NONE',  ( 0.2717059086739035401, -5.971041827598893903, 10.69429229731975894 ) ) ;
#16726 = ORIENTED_EDGE ( 'NONE', *, *, #33780, .F. ) ;
#16727 = AXIS2_PLACEMENT_3D ( 'NONE', #48443, #48759, #59712 ) ;
#16728 = ORIENTED_EDGE ( 'NONE', *, *, #32219, .T. ) ;
#16729 = DIRECTION ( 'NONE',  ( -0.000000000000000000, -0.000000000000000000, -1.000000000000000000 ) ) ;
#16730 = AXIS2_PLACEMENT_3D ( 'NONE', #18742, #38997, #54314 ) ;
#16731 = EDGE_CURVE ( 'NONE', #13080, #6530, #28014, .T. ) ;
#16732 = VERTEX_POINT ( 'NONE', #51802 ) ;
#16733 = CARTESIAN_POINT ( 'NONE',  ( -25.36156277276711535, -9.869979630862522058, 6.826986832051105125 ) ) ;
#16734 = DIRECTION ( 'NONE',  ( 0.000000000000000000, 0.000000000000000000, -1.000000000000000000 ) ) ;
#16735 = CARTESIAN_POINT ( 'NONE',  ( -35.00000000000000000, 0.000000000000000000, 0.000000000000000000 ) ) ;
#16736 = CARTESIAN_POINT ( 'NONE',  ( 1.014383007554946037, -0.4441500209062191895, -12.48801387563329790 ) ) ;
#16737 = ORIENTED_EDGE ( 'NONE', *, *, #3002, .T. ) ;
#16738 = CARTESIAN_POINT ( 'NONE',  ( 1.719304012340734378, -7.017415949613340587, -10.62216384465587282 ) ) ;
#16739 = EDGE_CURVE ( 'NONE', #48166, #24413, #65165, .T. ) ;
#16740 = CARTESIAN_POINT ( 'NONE',  ( -1.729917593620911020, -27.85289612474432275, 12.49635169356267106 ) ) ;
#16741 = CARTESIAN_POINT ( 'NONE',  ( -37.00000000000000711, 0.000000000000000000, 0.000000000000000000 ) ) ;
#16743 = VERTEX_POINT ( 'NONE', #60784 ) ;
#16742 = CARTESIAN_POINT ( 'NONE',  ( -24.88606550871976708, 5.771222983236214965, 10.55595544087139004 ) ) ;
#16744 = FACE_OUTER_BOUND ( 'NONE', #60682, .T. ) ;
#16745 = ORIENTED_EDGE ( 'NONE', *, *, #14859, .F. ) ;
#16746 = DIRECTION ( 'NONE',  ( -1.000000000000000000, 0.000000000000000000, 0.000000000000000000 ) ) ;
#16747 = VERTEX_POINT ( 'NONE', #55804 ) ;
#16748 = DIRECTION ( 'NONE',  ( 1.000000000000000000, 0.000000000000000000, 0.000000000000000000 ) ) ;
#16749 = EDGE_CURVE ( 'NONE', #23475, #2241, #4682, .T. ) ;
#16750 = LINE ( 'NONE', #6140, #64878 ) ;
#16751 = CARTESIAN_POINT ( 'NONE',  ( 1.549075743844138042, -4.962709020479777244, 11.66216484053746427 ) ) ;
#16752 = ORIENTED_EDGE ( 'NONE', *, *, #52425, .F. ) ;
#16753 = CARTESIAN_POINT ( 'NONE',  ( 37.00000000000000711, 4.705694406421931860E-17, -3.469127814946512892E-15 ) ) ;
#16754 = CARTESIAN_POINT ( 'NONE',  ( -35.00000000000000000, 0.000000000000000000, 0.000000000000000000 ) ) ;
#16755 = CARTESIAN_POINT ( 'NONE',  ( -35.00000000000000000, -4.041347439435779343, -11.02904044024213270 ) ) ;
#16757 = VERTEX_POINT ( 'NONE', #46796 ) ;
#16756 = EDGE_CURVE ( 'NONE', #20776, #173, #5717, .T. ) ;
#16758 = VERTEX_POINT ( 'NONE', #30509 ) ;
#16759 = CARTESIAN_POINT ( 'NONE',  ( -37.00000000000000711, -0.8294751490780184477, 12.15823808070322620 ) ) ;
#16760 = ORIENTED_EDGE ( 'NONE', *, *, #83, .F. ) ;
#16761 = EDGE_CURVE ( 'NONE', #3506, #62548, #25528, .T. ) ;
#16762 = ORIENTED_EDGE ( 'NONE', *, *, #50923, .T. ) ;
#16763 = CARTESIAN_POINT ( 'NONE',  ( 2.000000000000001776, 6.750946897830741200, -1.593658756657007514 ) ) ;
#16764 = FACE_OUTER_BOUND ( 'NONE', #21595, .T. ) ;
#16765 = DIRECTION ( 'NONE',  ( 0.000000000000000000, 0.01356324068817992175, -0.9999080150203990547 ) ) ;
#16766 = CARTESIAN_POINT ( 'NONE',  ( 3.152665057734004073, 7.102135024645805039, -3.546019893116331811 ) ) ;
#16767 = CARTESIAN_POINT ( 'NONE',  ( 2.941278708680199916, 0.9331242451664990556, 6.068329152486379385 ) ) ;
#16768 = VECTOR ( 'NONE', #18160, 1000.000000000000000 ) ;
#16769 = DIRECTION ( 'NONE',  ( -1.000000000000000000, 0.000000000000000000, -0.000000000000000000 ) ) ;
#16770 = DIRECTION ( 'NONE',  ( 0.000000000000000000, -0.7621620551276286903, -0.6473862847818365740 ) ) ;
#16771 = CIRCLE ( 'NONE', #10398, 4.999999999999999112 ) ;
#16772 = ORIENTED_EDGE ( 'NONE', *, *, #10420, .T. ) ;
#16773 = CIRCLE ( 'NONE', #53951, 7.499999999999988454 ) ;
#16774 = CARTESIAN_POINT ( 'NONE',  ( -22.27704833740210333, -2.993786163585782312, 2.142029987820952996 ) ) ;
#16775 = DIRECTION ( 'NONE',  ( 1.000000000000000000, 0.000000000000000000, 0.000000000000000000 ) ) ;
#16776 = AXIS2_PLACEMENT_3D ( 'NONE', #44639, #45985, #5095 ) ;
#16777 = EDGE_CURVE ( 'NONE', #25335, #56385, #9972, .T. ) ;
#16778 = CARTESIAN_POINT ( 'NONE',  ( 0.2869720083484372797, 4.386174336869755663, -11.44147823180126977 ) ) ;
#16779 = EDGE_CURVE ( 'NONE', #38095, #35612, #16860, .T. ) ;
#16780 = CYLINDRICAL_SURFACE ( 'NONE', #42755, 12.18649999999999878 ) ;
#16781 = CARTESIAN_POINT ( 'NONE',  ( 35.00000000000000000, -7.499679039483992504, 9.040300684349768190 ) ) ;
#16782 = CARTESIAN_POINT ( 'NONE',  ( 2.080613030138687591, 0.000000000000000000, 0.000000000000000000 ) ) ;
#16783 = ORIENTED_EDGE ( 'NONE', *, *, #30224, .F. ) ;
#16784 = DIRECTION ( 'NONE',  ( -0.000000000000000000, -1.000000000000000000, -0.000000000000000000 ) ) ;
#16785 = DIRECTION ( 'NONE',  ( -1.000000000000000000, 0.000000000000000000, 0.000000000000000000 ) ) ;
#16786 = CARTESIAN_POINT ( 'NONE',  ( -25.86628395826706850, 5.139808748864376220, 10.84354029019568522 ) ) ;
#16787 = EDGE_CURVE ( 'NONE', #37684, #5634, #4678, .T. ) ;
#16788 = LINE ( 'NONE', #42699, #2546 ) ;
#16789 = EDGE_CURVE ( 'NONE', #983, #4358, #26963, .T. ) ;
#16790 = CARTESIAN_POINT ( 'NONE',  ( 11.56239109567838597, 0.7119215618323401218, -13.48139877484980609 ) ) ;
#16791 = FACE_OUTER_BOUND ( 'NONE', #62288, .T. ) ;
#16792 = EDGE_LOOP ( 'NONE', ( #62406, #25557, #3712, #20270 ) ) ;
#16793 = CIRCLE ( 'NONE', #25298, 5.000000000000000000 ) ;
#16794 = FACE_OUTER_BOUND ( 'NONE', #2816, .T. ) ;
#16795 = CARTESIAN_POINT ( 'NONE',  ( -35.00000000000000000, -11.38112321385052716, 2.905556151562584954 ) ) ;
#16796 = DIRECTION ( 'NONE',  ( -0.000000000000000000, -1.000000000000000000, -0.000000000000000000 ) ) ;
#16797 = DIRECTION ( 'NONE',  ( 0.000000000000000000, -0.01356324068817998940, 0.9999080150203990547 ) ) ;
#16798 = ORIENTED_EDGE ( 'NONE', *, *, #39196, .F. ) ;
#16799 = CARTESIAN_POINT ( 'NONE',  ( 2.524535260912660561, 6.801151891677185368, 3.671333852642844064 ) ) ;
#16800 = DIRECTION ( 'NONE',  ( 1.000000000000000000, -0.000000000000000000, 0.000000000000000000 ) ) ;
#16801 = EDGE_CURVE ( 'NONE', #63362, #3618, #46101, .T. ) ;
#16803 = VERTEX_POINT ( 'NONE', #42433 ) ;
#16802 = CARTESIAN_POINT ( 'NONE',  ( 4.037157412408303976E-12, -31.03649492335491544, 14.44372008463339085 ) ) ;
#16804 = FACE_OUTER_BOUND ( 'NONE', #39883, .T. ) ;
#16805 = VECTOR ( 'NONE', #25186, 1000.000000000000000 ) ;
#16806 = DIRECTION ( 'NONE',  ( -1.000000000000000000, 0.000000000000000000, 0.000000000000000000 ) ) ;
#16807 = EDGE_LOOP ( 'NONE', ( #31567, #10839, #18763, #40896 ) ) ;
#16808 = DIRECTION ( 'NONE',  ( 1.000000000000000000, 0.000000000000000000, 0.000000000000000000 ) ) ;
#16809 = CARTESIAN_POINT ( 'NONE',  ( -37.00000000000000711, -5.672855678558757830, 10.28547182238005853 ) ) ;
#16810 = AXIS2_PLACEMENT_3D ( 'NONE', #60458, #50825, #35175 ) ;
#16811 = CARTESIAN_POINT ( 'NONE',  ( 0.2652384529303112304, -7.820949643217205427, 9.423437232855640389 ) ) ;
#16812 = CIRCLE ( 'NONE', #60342, 12.18649999999999878 ) ;
#16813 = CARTESIAN_POINT ( 'NONE',  ( -2.952869152607107139, -12.96714474214480717, 3.755417052241487585 ) ) ;
#16814 = CARTESIAN_POINT ( 'NONE',  ( -7.489022030332961322, 5.127957880411581293, -10.84914964302385521 ) ) ;
#16815 = ADVANCED_FACE ( 'NONE', ( #28162 ), #32789, .T. ) ;
#16816 = DIRECTION ( 'NONE',  ( -1.000000000000000000, 0.000000000000000000, 0.000000000000000000 ) ) ;
#16818 = ORIENTED_EDGE ( 'NONE', *, *, #51406, .F. ) ;
#16817 = DIRECTION ( 'NONE',  ( 0.000000000000000000, -0.3554799084908835116, -0.9346839223284592046 ) ) ;
#16819 = EDGE_CURVE ( 'NONE', #40162, #11383, #15282, .T. ) ;
#16820 = ORIENTED_EDGE ( 'NONE', *, *, #65400, .T. ) ;
#16821 = CARTESIAN_POINT ( 'NONE',  ( 24.79913956981017975, -1.736766911523203172, -11.87527920162771089 ) ) ;
#16822 = ORIENTED_EDGE ( 'NONE', *, *, #15780, .T. ) ;
#16823 = AXIS2_PLACEMENT_3D ( 'NONE', #23578, #18910, #39833 ) ;
#16824 = APPLICATION_PROTOCOL_DEFINITION ( 'draft international standard', 'automotive_design', 1998, #64631 ) ;
#16825 = DIRECTION ( 'NONE',  ( -1.000000000000000000, 0.000000000000000000, 0.000000000000000000 ) ) ;
#16826 = ADVANCED_FACE ( 'NONE', ( #48456 ), #2240, .T. ) ;
#16827 = CARTESIAN_POINT ( 'NONE',  ( -17.59990429990587657, 3.555202520397811039, 11.46264038328473589 ) ) ;
#16828 = ADVANCED_FACE ( 'NONE', ( #22518 ), #61187, .F. ) ;
#16829 = CARTESIAN_POINT ( 'NONE',  ( 5.514970785353741078, -0.003805873180274332770, 0.002796696073589857289 ) ) ;
#16830 = VERTEX_POINT ( 'NONE', #52777 ) ;
#16831 = DIRECTION ( 'NONE',  ( 0.000000000000000000, 0.000000000000000000, -1.000000000000000000 ) ) ;
#16832 = CARTESIAN_POINT ( 'NONE',  ( 3.742705681669799667, 4.513412766533817511, -12.75114006814483680 ) ) ;
#16833 = VERTEX_POINT ( 'NONE', #7204 ) ;
#16834 = ORIENTED_EDGE ( 'NONE', *, *, #45473, .T. ) ;
#16835 = EDGE_CURVE ( 'NONE', #38215, #27894, #2904, .T. ) ;
#16836 = CARTESIAN_POINT ( 'NONE',  ( 26.76944249566220435, -12.82941635345952847, 4.211941481156896039 ) ) ;
#16837 = ORIENTED_EDGE ( 'NONE', *, *, #29798, .F. ) ;
#16838 = DIRECTION ( 'NONE',  ( 0.000000000000000000, -0.9985334138511231528, -0.05413890858542833723 ) ) ;
#16839 = CARTESIAN_POINT ( 'NONE',  ( -22.49803948133827092, 3.704553751086694380, -2.269619744675233086 ) ) ;
#16840 = DIRECTION ( 'NONE',  ( 0.000000000000000000, 0.01356324068817991828, -0.9999080150203990547 ) ) ;
#16841 = CARTESIAN_POINT ( 'NONE',  ( 0.7400311444011722362, 12.27261279799597737, 1.803686700615449112 ) ) ;
#16842 = FACE_OUTER_BOUND ( 'NONE', #21234, .T. ) ;
#16843 = DIRECTION ( 'NONE',  ( -1.000000000000000000, -0.000000000000000000, 0.000000000000000000 ) ) ;
#16844 = CIRCLE ( 'NONE', #31683, 1.399999999999999911 ) ;
#16845 = DIRECTION ( 'NONE',  ( 0.000000000000000000, 0.01356324068817992175, -0.9999080150203990547 ) ) ;
#16846 = VERTEX_POINT ( 'NONE', #33136 ) ;
#16847 = DIRECTION ( 'NONE',  ( -1.000000000000000000, 0.000000000000000000, 0.000000000000000000 ) ) ;
#16848 = AXIS2_PLACEMENT_3D ( 'NONE', #17764, #53000, #31717 ) ;
#16849 = EDGE_LOOP ( 'NONE', ( #571, #18897, #21815, #6879 ) ) ;
#16850 = LINE ( 'NONE', #27165, #9800 ) ;
#16851 = DIRECTION ( 'NONE',  ( 0.000000000000000000, -0.1740410799127685149, -0.9847383929261604996 ) ) ;
#16852 = CARTESIAN_POINT ( 'NONE',  ( 5.514970785353741078, 0.001897634820904955163, 0.004324946436530311550 ) ) ;
#16853 = CARTESIAN_POINT ( 'NONE',  ( 2.368238019615144907, -2.793778585134617742, -7.150288915654806843 ) ) ;
#16854 = DIRECTION ( 'NONE',  ( 0.000000000000000000, 0.01356324068817992175, -0.9999080150203990547 ) ) ;
#16855 = CARTESIAN_POINT ( 'NONE',  ( 0.2638984909335720941, 4.375449752477134524, 11.43908195192331334 ) ) ;
#16856 = AXIS2_PLACEMENT_3D ( 'NONE', #2782, #58633, #49551 ) ;
#16857 = ORIENTED_EDGE ( 'NONE', *, *, #7691, .T. ) ;
#16858 = ADVANCED_FACE ( 'NONE', ( #38455 ), #27827, .T. ) ;
#16859 = ORIENTED_EDGE ( 'NONE', *, *, #29005, .F. ) ;
#16860 = LINE ( 'NONE', #7536, #55647 ) ;
#16861 = EDGE_CURVE ( 'NONE', #13432, #53221, #13192, .T. ) ;
#16862 = VECTOR ( 'NONE', #35988, 1000.000000000000000 ) ;
#16863 = AXIS2_PLACEMENT_3D ( 'NONE', #43916, #7686, #48280 ) ;
#16864 = VERTEX_POINT ( 'NONE', #45088 ) ;
#16865 = DIRECTION ( 'NONE',  ( 1.000000000000000000, 0.000000000000000000, -0.000000000000000000 ) ) ;
#16866 = CARTESIAN_POINT ( 'NONE',  ( 5.514970785353741078, -0.002619824551223247366, 0.003929719953530060386 ) ) ;
#16867 = CIRCLE ( 'NONE', #54042, 12.75000000000000178 ) ;
#16868 = CARTESIAN_POINT ( 'NONE',  ( 2.242819959140648134, 4.828731837260225923, 5.913965034148179534 ) ) ;
#16869 = CARTESIAN_POINT ( 'NONE',  ( -35.04834644901396956, 0.01183641858481722896, -0.007161132384423698344 ) ) ;
#16870 = ORIENTED_EDGE ( 'NONE', *, *, #25086, .T. ) ;
#16871 = CARTESIAN_POINT ( 'NONE',  ( 3.047904605210420836, 2.299870214474541541, 7.561255571389395413 ) ) ;
#16872 = CYLINDRICAL_SURFACE ( 'NONE', #3537, 5.000000000000000888 ) ;
#16873 = EDGE_CURVE ( 'NONE', #24405, #65324, #19495, .T. ) ;
#16874 = DIRECTION ( 'NONE',  ( 0.000000000000000000, 0.000000000000000000, -1.000000000000000000 ) ) ;
#16875 = AXIS2_PLACEMENT_3D ( 'NONE', #55722, #55379, #40398 ) ;
#16876 = CARTESIAN_POINT ( 'NONE',  ( -26.65194590272819042, -3.631858188236755769, 25.00000000000000000 ) ) ;
#16877 = DIRECTION ( 'NONE',  ( 0.000000000000000000, -0.01356324068817991828, 0.9999080150203990547 ) ) ;
#16878 = LINE ( 'NONE', #52790, #40371 ) ;
#16879 =( BOUNDED_SURFACE ( )  B_SPLINE_SURFACE ( 3, 1, ( 
 ( #56511, #57838 ),
 ( #6636, #62790 ),
 ( #981, #6955 ),
 ( #11284, #6303 ) ),
 .UNSPECIFIED., .F., .F., .F. ) 
 B_SPLINE_SURFACE_WITH_KNOTS ( ( 4, 4 ),
 ( 2, 2 ),
 ( 0.000000000000000000, 1.000000000000000000 ),
 ( 0.000000000000000000, 1.000000000000000000 ),
 .UNSPECIFIED. ) 
 GEOMETRIC_REPRESENTATION_ITEM ( )  RATIONAL_B_SPLINE_SURFACE ( (
 ( 1.000000000000000000, 1.000000000000000000),
 ( 0.9942764183789327692, 0.8450855930916585379),
 ( 0.9942764183789327692, 0.8450855930916585379),
 ( 1.000000000000000000, 1.000000000000000000) ) ) 
 REPRESENTATION_ITEM ( '' )  SURFACE ( )  );
#16880 = ORIENTED_EDGE ( 'NONE', *, *, #61756, .F. ) ;
#16881 = DIRECTION ( 'NONE',  ( 1.000000000000000000, -0.000000000000000000, -0.000000000000000000 ) ) ;
#16882 = ORIENTED_EDGE ( 'NONE', *, *, #23246, .F. ) ;
#16883 = FACE_OUTER_BOUND ( 'NONE', #20577, .T. ) ;
#16884 = DIRECTION ( 'NONE',  ( 0.000000000000000000, -0.01356324068817999114, 0.9999080150203989437 ) ) ;
#16885 = CARTESIAN_POINT ( 'NONE',  ( 0.2655924914740778187, 12.24627751708824341, 0.04405032194307429566 ) ) ;
#16886 = EDGE_CURVE ( 'NONE', #21123, #1597, #32263, .T. ) ;
#16887 = DIRECTION ( 'NONE',  ( 0.000000000000000000, -0.8989688749565110104, -0.4380125133594070519 ) ) ;
#16888 = ADVANCED_FACE ( 'NONE', ( #49747 ), #63681, .F. ) ;
#16889 = CYLINDRICAL_SURFACE ( 'NONE', #64912, 4.999999999999998224 ) ;
#16890 = VECTOR ( 'NONE', #38761, 1000.000000000000000 ) ;
#16891 = ORIENTED_EDGE ( 'NONE', *, *, #45001, .F. ) ;
#16892 = VERTEX_POINT ( 'NONE', #28805 ) ;
#16893 = CARTESIAN_POINT ( 'NONE',  ( 0.3537226245948366654, 1.874138792913011553, 12.13174752084887054 ) ) ;
#16894 = EDGE_LOOP ( 'NONE', ( #35038, #61752, #59556, #4869 ) ) ;
#16895 = CARTESIAN_POINT ( 'NONE',  ( 3.291290029914074378, 8.250315036047103590, 8.713914264323182834 ) ) ;
#16896 = CARTESIAN_POINT ( 'NONE',  ( 3.291290029914074378, 8.250315036047103590, -10.68561190601526079 ) ) ;
#16897 = CYLINDRICAL_SURFACE ( 'NONE', #61729, 5.000000000000000888 ) ;
#16898 =( BOUNDED_CURVE ( )  B_SPLINE_CURVE ( 3, ( #58691, #43687, #54007, #45256 ),
 .UNSPECIFIED., .F., .F. ) 
 B_SPLINE_CURVE_WITH_KNOTS ( ( 4, 4 ),
 ( 1.238310171490985434, 1.242866721674340758 ),
 .UNSPECIFIED. ) 
 CURVE ( )  GEOMETRIC_REPRESENTATION_ITEM ( )  RATIONAL_B_SPLINE_CURVE ( ( 1.000000000000000000, 0.9999982698216172139, 0.9999982698216172139, 1.000000000000000000 ) ) 
 REPRESENTATION_ITEM ( '' )  );
#16899 = CARTESIAN_POINT ( 'NONE',  ( 0.6473888112830272767, 3.920507224439243377, -11.73602097806015720 ) ) ;
#16901 = CARTESIAN_POINT ( 'NONE',  ( 2.491965175172130120, 7.715025372670220705, -0.2120508241292647922 ) ) ;
#16900 = CIRCLE ( 'NONE', #50895, 12.18649999999999878 ) ;
#16902 = CARTESIAN_POINT ( 'NONE',  ( 2.253265082353315130, 5.768060979106778063, 5.007416537587866756 ) ) ;
#16903 = CARTESIAN_POINT ( 'NONE',  ( -37.00000000000000711, 7.882940143791919319, -10.02106554660700333 ) ) ;
#16904 = VERTEX_POINT ( 'NONE', #59088 ) ;
#16905 = DIRECTION ( 'NONE',  ( 1.000000000000000000, 0.000000000000000000, 0.000000000000000000 ) ) ;
#16906 = ORIENTED_EDGE ( 'NONE', *, *, #50573, .F. ) ;
#16907 = SURFACE_SIDE_STYLE ('',( #2637 ) ) ;
#16908 = AXIS2_PLACEMENT_3D ( 'NONE', #58448, #3252, #7913 ) ;
#16909 = EDGE_CURVE ( 'NONE', #41059, #37494, #18906, .T. ) ;
#16910 = FACE_OUTER_BOUND ( 'NONE', #54764, .T. ) ;
#16911 = AXIS2_PLACEMENT_3D ( 'NONE', #26232, #15901, #20247 ) ;
#16912 = CARTESIAN_POINT ( 'NONE',  ( 1.634816307077934461, 8.702988562441301923, -9.253014110594602215 ) ) ;
#16913 = EDGE_CURVE ( 'NONE', #50873, #64499, #63078, .T. ) ;
#16914 = CARTESIAN_POINT ( 'NONE',  ( -27.08430792439084556, 1.614882584890349637, 1.625846845508313487 ) ) ;
#16916 = ORIENTED_EDGE ( 'NONE', *, *, #27243, .F. ) ;
#16915 = CIRCLE ( 'NONE', #30706, 5.000000000000000000 ) ;
#16917 = LINE ( 'NONE', #1646, #53494 ) ;
#16918 = DIRECTION ( 'NONE',  ( -1.000000000000000000, -0.000000000000000000, -0.000000000000000000 ) ) ;
#16919 = DIRECTION ( 'NONE',  ( 1.000000000000000000, -0.000000000000000000, 0.000000000000000000 ) ) ;
#16920 = VERTEX_POINT ( 'NONE', #24460 ) ;
#16921 = ORIENTED_EDGE ( 'NONE', *, *, #30204, .T. ) ;
#16922 = EDGE_CURVE ( 'NONE', #46560, #63220, #40772, .T. ) ;
#16923 = CARTESIAN_POINT ( 'NONE',  ( 3.427798639585919016, 7.593315936193067550, 11.19287808785590066 ) ) ;
#16924 = ORIENTED_EDGE ( 'NONE', *, *, #8900, .F. ) ;
#16925 = EDGE_LOOP ( 'NONE', ( #12474, #4338, #11036, #65401 ) ) ;
#16926 = ORIENTED_EDGE ( 'NONE', *, *, #15551, .F. ) ;
#16927 = AXIS2_PLACEMENT_3D ( 'NONE', #21024, #51647, #27017 ) ;
#16928 = ORIENTED_EDGE ( 'NONE', *, *, #23266, .T. ) ;
#16929 = CARTESIAN_POINT ( 'NONE',  ( -22.27711653538342773, -2.958138731383645581, 2.191780254295684571 ) ) ;
#16930 = FACE_OUTER_BOUND ( 'NONE', #12743, .T. ) ;
#16931 = B_SPLINE_CURVE_WITH_KNOTS ( 'NONE', 3,
 ( #54460, #33813, #18221, #8890, #38492, #8235 ),
 .UNSPECIFIED., .F., .F.,
 ( 4, 2, 4 ),
 ( 0.000000000000000000, 0.0004528561986909396394, 0.0009057123973818792789 ),
 .UNSPECIFIED. ) ;
#16932 = FACE_BOUND ( 'NONE', #57881, .T. ) ;
#16933 = CARTESIAN_POINT ( 'NONE',  ( 0.9232058338315048962, 5.905985151448150283, 10.98407661738930763 ) ) ;
#16934 = CARTESIAN_POINT ( 'NONE',  ( -35.00000000000000000, 4.732539170486427693, -11.23004253107759176 ) ) ;
#16935 = ORIENTED_EDGE ( 'NONE', *, *, #56803, .F. ) ;
#16936 = ADVANCED_FACE ( 'NONE', ( #23497 ), #54749, .T. ) ;
#16937 = FACE_OUTER_BOUND ( 'NONE', #57531, .T. ) ;
#16938 = ORIENTED_EDGE ( 'NONE', *, *, #21895, .F. ) ;
#16939 = DIRECTION ( 'NONE',  ( 1.000000000000000000, 0.000000000000000000, 0.000000000000000000 ) ) ;
#16940 = CARTESIAN_POINT ( 'NONE',  ( 3.047904605210329798, 4.747272783555662734, 6.318654123925870891 ) ) ;
#16941 = LINE ( 'NONE', #27246, #35278 ) ;
#16942 = CARTESIAN_POINT ( 'NONE',  ( 0.3109076770649044086, -8.060731492642734253, -9.239379580302180983 ) ) ;
#16943 = DIRECTION ( 'NONE',  ( 0.000000000000000000, 0.000000000000000000, -1.000000000000000000 ) ) ;
#16944 = FACE_OUTER_BOUND ( 'NONE', #35586, .T. ) ;
#16945 = VECTOR ( 'NONE', #47550, 1000.000000000000000 ) ;
#16946 = ORIENTED_EDGE ( 'NONE', *, *, #49342, .F. ) ;
#16947 = DIRECTION ( 'NONE',  ( 0.000000000000000000, -0.1118654143051477368, -0.9937233664769776764 ) ) ;
#16948 = EDGE_CURVE ( 'NONE', #60501, #9614, #12099, .T. ) ;
#16949 = AXIS2_PLACEMENT_3D ( 'NONE', #28393, #64296, #44648 ) ;
#16950 = ORIENTED_EDGE ( 'NONE', *, *, #45461, .F. ) ;
#16951 = CARTESIAN_POINT ( 'NONE',  ( 5.515539859299206427, -0.003193223631739290028, -0.005142293699651858188 ) ) ;
#16952 = DIRECTION ( 'NONE',  ( -1.000000000000000000, 0.000000000000000000, 0.000000000000000000 ) ) ;
#16953 = DIRECTION ( 'NONE',  ( -1.000000000000000000, 0.000000000000000000, -0.000000000000000000 ) ) ;
#16954 = CARTESIAN_POINT ( 'NONE',  ( 37.00000000000000711, 6.102719229070675766, -10.54834585426222482 ) ) ;
#16955 = CARTESIAN_POINT ( 'NONE',  ( 2.255723233588950105, -6.680843247642341609, 3.704537245405018275 ) ) ;
#16956 = ORIENTED_EDGE ( 'NONE', *, *, #25296, .F. ) ;
#16957 = CARTESIAN_POINT ( 'NONE',  ( 0.6473888112830219477, 10.54705164520787442, -6.470260187014609699 ) ) ;
#16958 = CARTESIAN_POINT ( 'NONE',  ( 1.000000000000000888, 6.936109781200720192, -2.853135311044974198 ) ) ;
#16959 = DIRECTION ( 'NONE',  ( 1.000000000000000000, 0.000000000000000000, 0.000000000000000000 ) ) ;
#16960 = CARTESIAN_POINT ( 'NONE',  ( -1.318817192132426526E-11, -30.53649492335491544, -15.30974548841782834 ) ) ;
#16961 = AXIS2_PLACEMENT_3D ( 'NONE', #64484, #39551, #18953 ) ;
#16962 = CIRCLE ( 'NONE', #24400, 4.999999999999999112 ) ;
#16963 = DIRECTION ( 'NONE',  ( -1.000000000000000000, -0.000000000000000000, 0.000000000000000000 ) ) ;
#16964 = ORIENTED_EDGE ( 'NONE', *, *, #19704, .T. ) ;
#16965 = CARTESIAN_POINT ( 'NONE',  ( 0.2655924914740778742, 7.905499957109238807, 9.352877839710629360 ) ) ;
#16967 = ADVANCED_FACE ( 'NONE', ( #65021 ), #18537, .T. ) ;
#16966 = CARTESIAN_POINT ( 'NONE',  ( 0.2650492433740064269, -2.017984765249154488, 12.07870441534855743 ) ) ;
#16968 = AXIS2_PLACEMENT_3D ( 'NONE', #60496, #20265, #40545 ) ;
#16969 = ADVANCED_FACE ( 'NONE', ( #60055 ), #23840, .T. ) ;
#16970 = VERTEX_POINT ( 'NONE', #49446 ) ;
#16971 = VERTEX_POINT ( 'NONE', #24144 ) ;
#16972 = CARTESIAN_POINT ( 'NONE',  ( 0.2653141334712580401, 2.169900597054518432, 12.05242949860144286 ) ) ;
#16973 = CYLINDRICAL_SURFACE ( 'NONE', #51326, 12.74999999999999822 ) ;
#16974 = FACE_OUTER_BOUND ( 'NONE', #34485, .T. ) ;
#16975 = CARTESIAN_POINT ( 'NONE',  ( 1.000000000000000888, 6.160607635185406217, 4.277489166005578269 ) ) ;
#16976 = ORIENTED_EDGE ( 'NONE', *, *, #2714, .F. ) ;
#16977 = ORIENTED_EDGE ( 'NONE', *, *, #51650, .F. ) ;
#16978 = ORIENTED_EDGE ( 'NONE', *, *, #58394, .F. ) ;
#16979 = DIRECTION ( 'NONE',  ( -1.000000000000000000, -0.000000000000000000, -0.000000000000000000 ) ) ;
#16980 = EDGE_CURVE ( 'NONE', #32845, #31042, #49881, .T. ) ;
#16982 = CARTESIAN_POINT ( 'NONE',  ( -37.00000000000000711, -10.14433819232429812, -6.753013023069823539 ) ) ;
#16981 = AXIS2_PLACEMENT_3D ( 'NONE', #33576, #62838, #42885 ) ;
#16983 = AXIS2_PLACEMENT_3D ( 'NONE', #17930, #37879, #53178 ) ;
#16984 = ORIENTED_EDGE ( 'NONE', *, *, #62145, .F. ) ;
#16985 = DIRECTION ( 'NONE',  ( -1.000000000000000000, -0.000000000000000000, -0.000000000000000000 ) ) ;
#16986 = DIRECTION ( 'NONE',  ( -1.000000000000000000, 0.000000000000000000, 0.000000000000000000 ) ) ;
#16987 = ORIENTED_EDGE ( 'NONE', *, *, #29485, .F. ) ;
#16988 = CARTESIAN_POINT ( 'NONE',  ( -27.08416974970326052, -0.4041872645907051420, -2.255186831366117417 ) ) ;
#16989 = FACE_OUTER_BOUND ( 'NONE', #54194, .T. ) ;
#16990 = FACE_OUTER_BOUND ( 'NONE', #64558, .T. ) ;
#16991 = EDGE_LOOP ( 'NONE', ( #40232, #1964, #37600, #56151 ) ) ;
#16992 = DIRECTION ( 'NONE',  ( 0.000000000000000000, -0.01356324068817998940, 0.9999080150203990547 ) ) ;
#16993 = ORIENTED_EDGE ( 'NONE', *, *, #30968, .T. ) ;
#16994 = DIRECTION ( 'NONE',  ( 1.000000000000000000, 0.000000000000000000, 0.000000000000000000 ) ) ;
#16995 = CARTESIAN_POINT ( 'NONE',  ( 2.241537034860907607, 4.903726641589524426, 5.851376807350157527 ) ) ;
#16996 = AXIS2_PLACEMENT_3D ( 'NONE', #23451, #17489, #16817 ) ;
#16997 = EDGE_CURVE ( 'NONE', #10987, #43919, #46715, .T. ) ;
#16998 = CARTESIAN_POINT ( 'NONE',  ( 0.000000000000000000, -45.00000000000000000, 0.000000000000000000 ) ) ;
#16999 = CARTESIAN_POINT ( 'NONE',  ( 2.241352910868909643, -6.569501556381469598, 3.889181972941426313 ) ) ;
#17000 = DIRECTION ( 'NONE',  ( 1.000000000000000000, -0.000000000000000000, 0.000000000000000000 ) ) ;
#17001 = CARTESIAN_POINT ( 'NONE',  ( 0.3040950598368144520, -6.347045025870841073, 10.49113473328028867 ) ) ;
#17002 = CARTESIAN_POINT ( 'NONE',  ( 35.00000000000000000, 4.705694406421931860E-17, -3.469127814946512892E-15 ) ) ;
#17003 = ORIENTED_EDGE ( 'NONE', *, *, #39388, .F. ) ;
#17004 = CARTESIAN_POINT ( 'NONE',  ( -35.00000000000000000, -9.512294188640947112, 6.891188680298791169 ) ) ;
#17005 = EDGE_LOOP ( 'NONE', ( #64632, #44083, #33224, #49518 ) ) ;
#17006 = CARTESIAN_POINT ( 'NONE',  ( -35.00000000000000000, 0.000000000000000000, 0.000000000000000000 ) ) ;
#17007 = CARTESIAN_POINT ( 'NONE',  ( 5.530133899448235191, 0.001661287012794044910, 0.01589823604557701400 ) ) ;
#17008 = ORIENTED_EDGE ( 'NONE', *, *, #17879, .F. ) ;
#17009 = B_SPLINE_CURVE_WITH_KNOTS ( 'NONE', 3,
 ( #51498, #12204, #32473, #56812, #62736, #37478, #52782, #27494, #5945, #2244, #21195, #41466, #61762, #11234, #51806, #28168 ),
 .UNSPECIFIED., .F., .F.,
 ( 4, 3, 3, 3, 3, 4 ),
 ( 5.963111948670274387E-19, 0.0003017745587525257349, 0.0006035491769808738489, 0.0009053241094668159229, 0.001207275924540508662, 0.001510325902534021556 ),
 .UNSPECIFIED. ) ;
#17010 = CARTESIAN_POINT ( 'NONE',  ( -37.00000000000000711, -12.46157735505191333, 2.696588552979012121 ) ) ;
#17011 = DIRECTION ( 'NONE',  ( 0.000000000000000000, 0.000000000000000000, 1.000000000000000000 ) ) ;
#17012 = CIRCLE ( 'NONE', #62653, 12.18650000000000055 ) ;
#17013 = CARTESIAN_POINT ( 'NONE',  ( -35.00000000000000000, -11.13736569743278082, 4.946702696913133579 ) ) ;
#17014 = ORIENTED_EDGE ( 'NONE', *, *, #27955, .T. ) ;
#17015 = B_SPLINE_CURVE_WITH_KNOTS ( 'NONE', 3,
 ( #11712, #20733, #41316, #36671, #31668, #62261, #46648, #26055, #30684, #36986 ),
 .UNSPECIFIED., .F., .F.,
 ( 4, 3, 3, 4 ),
 ( 5.401523115762567128E-05, 0.0008136511341527817446, 0.004068255670953089750, 0.005063778443040923942 ),
 .UNSPECIFIED. ) ;
#17016 = ORIENTED_EDGE ( 'NONE', *, *, #22167, .T. ) ;
#17017 = CARTESIAN_POINT ( 'NONE',  ( 5.520433897694421610, 0.01278034823631963093, 0.007971295965052456120 ) ) ;
#17018 = B_SPLINE_CURVE_WITH_KNOTS ( 'NONE', 3,
 ( #8418, #43005, #54315, #12733, #34338, #58988, #48355, #2805, #18074, #3463, #63600, #8755, #59292, #9070, #14047, #63280, #38337, #64272, #54652, #29036, #3791, #48011 ),
 .UNSPECIFIED., .F., .F.,
 ( 4, 3, 3, 3, 3, 3, 3, 4 ),
 ( 1.764953265579307567E-18, 4.449119708436945902E-05, 6.626296329540647860E-05, 8.803456484962896152E-05, 0.0001098060367612814227, 0.0001315774408628525083, 0.0001760698110411161544, 0.0001829697163287809084 ),
 .UNSPECIFIED. ) ;
#17019 = AXIS2_PLACEMENT_3D ( 'NONE', #47224, #32535, #1670 ) ;
#17020 = EDGE_CURVE ( 'NONE', #64858, #2304, #12005, .T. ) ;
#17021 = ORIENTED_EDGE ( 'NONE', *, *, #22722, .F. ) ;
#17022 = CARTESIAN_POINT ( 'NONE',  ( 3.152665057734129750, 3.161213418913565221, -7.281573230474259972 ) ) ;
#17023 = DIRECTION ( 'NONE',  ( 0.000000000000000000, 0.2006870767258820687, -0.9796553971857756560 ) ) ;
#17024 = ADVANCED_FACE ( 'NONE', ( #40403 ), #51066, .T. ) ;
#17025 = CARTESIAN_POINT ( 'NONE',  ( 3.152665057734087117, 7.886634106564184954, -0.9030954876737516956 ) ) ;
#17026 = CARTESIAN_POINT ( 'NONE',  ( 36.00000000000000711, -0.1414404973753014549, -12.74921544981111055 ) ) ;
#17027 = DIRECTION ( 'NONE',  ( 0.3939253465568943735, -0.9068155327749454209, 0.1500280335741383531 ) ) ;
#17028 = ORIENTED_EDGE ( 'NONE', *, *, #8175, .F. ) ;
#17029 = CARTESIAN_POINT ( 'NONE',  ( 0.2759803524722191925, -12.02930579076649131, -2.313459762622668947 ) ) ;
#17030 = CIRCLE ( 'NONE', #58490, 5.000000000000000000 ) ;
#17031 = STYLED_ITEM ( 'NONE', ( #38954 ), #7045 ) ;
#17032 = EDGE_CURVE ( 'NONE', #2632, #53954, #30437, .T. ) ;
#17033 = CIRCLE ( 'NONE', #57384, 5.000000000000000000 ) ;
#17034 = CARTESIAN_POINT ( 'NONE',  ( 29.23374216858299945, 9.169383756589978063, 9.943439309940176329 ) ) ;
#17035 = DIRECTION ( 'NONE',  ( -0.000000000000000000, -0.000000000000000000, -1.000000000000000000 ) ) ;
#17036 = CARTESIAN_POINT ( 'NONE',  ( 24.44415356966865360, 11.03103468991324654, -7.786488058063032014 ) ) ;
#17037 = CARTESIAN_POINT ( 'NONE',  ( -35.00000000000000000, 14.99999999999998757, 1.836970198721028406E-15 ) ) ;
#17038 = CARTESIAN_POINT ( 'NONE',  ( 0.2655924914740778742, 4.229867354073558516, 11.49267051747969681 ) ) ;
#17039 = EDGE_CURVE ( 'NONE', #50979, #59495, #841, .T. ) ;
#17040 = CARTESIAN_POINT ( 'NONE',  ( 0.7400311444011685724, 4.574267895796849892, 11.53023780418227950 ) ) ;
#17041 = CARTESIAN_POINT ( 'NONE',  ( 2.994568964204221473, 5.368337437440340310, -5.775954174106879613 ) ) ;
#17042 = B_SPLINE_CURVE_WITH_KNOTS ( 'NONE', 3,
 ( #4814, #65612, #44355, #39707, #20412, #60985, #24093, #20083, #59674, #35687 ),
 .UNSPECIFIED., .F., .F.,
 ( 4, 3, 3, 4 ),
 ( 8.673617379884035472E-19, 6.607638129004594592E-05, 9.911389841680703862E-05, 0.0001667630577588622570 ),
 .UNSPECIFIED. ) ;
#17043 = ORIENTED_EDGE ( 'NONE', *, *, #1312, .T. ) ;
#17044 = CARTESIAN_POINT ( 'NONE',  ( 0.000000000000000000, 6.201547234537079234, -2.820401998297854096 ) ) ;
#17045 = CARTESIAN_POINT ( 'NONE',  ( 4.492447587936224451, -10.17925049329322107, 8.868279803853196697 ) ) ;
#17046 = ORIENTED_EDGE ( 'NONE', *, *, #42742, .F. ) ;
#17047 = DIRECTION ( 'NONE',  ( 1.000000000000000000, -0.000000000000000000, -0.000000000000000000 ) ) ;
#17048 = DIRECTION ( 'NONE',  ( -1.000000000000000000, 0.000000000000000000, 0.000000000000000000 ) ) ;
#17049 = ORIENTED_EDGE ( 'NONE', *, *, #2976, .T. ) ;
#17050 = CARTESIAN_POINT ( 'NONE',  ( 2.251139882114759239, 6.551456272498336730, 3.925854078925700374 ) ) ;
#17051 = EDGE_LOOP ( 'NONE', ( #54504, #38830, #60244, #55044 ) ) ;
#17052 = AXIS2_PLACEMENT_3D ( 'NONE', #34265, #29928, #55541 ) ;
#17053 = CARTESIAN_POINT ( 'NONE',  ( -35.00000000000000000, -8.534258022646161734, 8.699265615722952205 ) ) ;
#17054 = ORIENTED_EDGE ( 'NONE', *, *, #21244, .T. ) ;
#17055 = ORIENTED_EDGE ( 'NONE', *, *, #43434, .F. ) ;
#17056 = DIRECTION ( 'NONE',  ( 1.000000000000000000, -0.000000000000000000, 0.000000000000000000 ) ) ;
#17057 = VERTEX_POINT ( 'NONE', #6169 ) ;
#17058 = CARTESIAN_POINT ( 'NONE',  ( 2.000000000000001776, 0.000000000000000000, 0.000000000000000000 ) ) ;
#17059 = CARTESIAN_POINT ( 'NONE',  ( -22.29570301036918423, -3.588849529203739674, 1.042190670255894736 ) ) ;
#17060 = DIRECTION ( 'NONE',  ( 0.000000000000000000, -0.01356324068817999114, 0.9999080150203989437 ) ) ;
#17061 = VECTOR ( 'NONE', #9530, 1000.000000000000000 ) ;
#17062 = DIRECTION ( 'NONE',  ( -1.000000000000000000, 0.000000000000000000, 0.000000000000000000 ) ) ;
#17063 = ORIENTED_EDGE ( 'NONE', *, *, #20516, .T. ) ;
#17064 = CARTESIAN_POINT ( 'NONE',  ( 0.3223008802179215260, -7.695050880595557530, 9.550960164375572603 ) ) ;
#17065 = CARTESIAN_POINT ( 'NONE',  ( 8.088853370213684002, -28.65367229866794219, 10.33367282332777393 ) ) ;
#17066 = CARTESIAN_POINT ( 'NONE',  ( -22.59969328935896726, -4.594269189967464584, -0.7214993884004354818 ) ) ;
#17068 = ORIENTED_EDGE ( 'NONE', *, *, #62816, .T. ) ;
#17067 = CARTESIAN_POINT ( 'NONE',  ( -24.79033130866653067, 9.927070015466320285, 6.752286632236016217 ) ) ;
#17070 = VECTOR ( 'NONE', #49781, 1000.000000000000000 ) ;
#17069 = CARTESIAN_POINT ( 'NONE',  ( 37.00000000000000711, -9.621072037176935154, 8.366449238204463512 ) ) ;
#17071 = ORIENTED_EDGE ( 'NONE', *, *, #28185, .F. ) ;
#17072 = APPLICATION_CONTEXT ( 'automotive_design' ) ;
#17073 = CARTESIAN_POINT ( 'NONE',  ( 0.2651627682582927692, 9.324228491541633801, -7.938957913267660871 ) ) ;
#17074 = EDGE_LOOP ( 'NONE', ( #50353, #13864, #30730, #35867 ) ) ;
#17075 = DIRECTION ( 'NONE',  ( -1.000000000000000000, -0.000000000000000000, 0.000000000000000000 ) ) ;
#17076 = DIRECTION ( 'NONE',  ( -1.000000000000000000, 0.000000000000000000, 0.000000000000000000 ) ) ;
#17077 = CARTESIAN_POINT ( 'NONE',  ( 0.9296196016823148334, -4.652334946094635271, 11.56707937094485139 ) ) ;
#17078 = ADVANCED_FACE ( 'NONE', ( #10473 ), #25791, .T. ) ;
#17079 = AXIS2_PLACEMENT_3D ( 'NONE', #63002, #37067, #37401 ) ;
#17080 = VERTEX_POINT ( 'NONE', #30749 ) ;
#17081 = CIRCLE ( 'NONE', #22392, 2.899999999999994582 ) ;
#17083 = VECTOR ( 'NONE', #33509, 1000.000000000000000 ) ;
#17082 = LINE ( 'NONE', #17426, #61183 ) ;
#17084 = DIRECTION ( 'NONE',  ( -1.000000000000000000, 0.000000000000000000, 0.000000000000000000 ) ) ;
#17086 = CARTESIAN_POINT ( 'NONE',  ( -22.30398854582847790, -3.656532484463038024, -0.8844201765542353266 ) ) ;
#17085 = B_SPLINE_CURVE_WITH_KNOTS ( 'NONE', 3,
 ( #13486, #3559, #33770, #38103, #63695, #53433, #13805, #2224, #54416, #22841, #18173, #29135, #22504, #43096, #42764, #7876, #32773, #39088, #28151 ),
 .UNSPECIFIED., .F., .F.,
 ( 4, 3, 3, 3, 3, 3, 4 ),
 ( 1.226634733346699349E-18, 2.831840207499513698E-05, 4.217266859840391790E-05, 5.602024318395954422E-05, 6.290810167969108978E-05, 9.120440630945299103E-05, 0.0001153103026479744092 ),
 .UNSPECIFIED. ) ;
#17087 = VERTEX_POINT ( 'NONE', #20796 ) ;
#17088 =( BOUNDED_SURFACE ( )  B_SPLINE_SURFACE ( 3, 1, ( 
 ( #22879, #53123 ),
 ( #38140, #32491 ),
 ( #28190, #48478 ),
 ( #63409, #58450 ) ),
 .UNSPECIFIED., .F., .F., .F. ) 
 B_SPLINE_SURFACE_WITH_KNOTS ( ( 4, 4 ),
 ( 2, 2 ),
 ( 0.000000000000000000, 1.000000000000000000 ),
 ( 0.000000000000000000, 1.000000000000000000 ),
 .UNSPECIFIED. ) 
 GEOMETRIC_REPRESENTATION_ITEM ( )  RATIONAL_B_SPLINE_SURFACE ( (
 ( 1.000000000000000000, 1.000000000000000000),
 ( 0.6933888150995267674, 0.9895912004443193632),
 ( 0.6933888150995267674, 0.9895912004443193632),
 ( 1.000000000000000000, 1.000000000000000000) ) ) 
 REPRESENTATION_ITEM ( '' )  SURFACE ( )  );
#17089 = EDGE_LOOP ( 'NONE', ( #31705, #29164, #52254, #47482 ) ) ;
#17090 = CIRCLE ( 'NONE', #50034, 12.18650000000000055 ) ;
#17091 = CARTESIAN_POINT ( 'NONE',  ( -19.47984447937493613, -1.416020129149132334, 25.00000000000000000 ) ) ;
#17092 = ORIENTED_EDGE ( 'NONE', *, *, #30774, .F. ) ;
#17093 = ORIENTED_EDGE ( 'NONE', *, *, #35702, .T. ) ;
#17094 = DIRECTION ( 'NONE',  ( 0.000000000000000000, 0.8009703041134146329, 0.5987040770935705414 ) ) ;
#17095 = CYLINDRICAL_SURFACE ( 'NONE', #14743, 5.000000000000000888 ) ;
#17096 = CARTESIAN_POINT ( 'NONE',  ( 1.719304012341432264, 5.066286238787408358, -11.67935079956426847 ) ) ;
#17097 = DIRECTION ( 'NONE',  ( 0.000000000000000000, -0.9847383929261634972, 0.1740410799127515007 ) ) ;
#17099 = VECTOR ( 'NONE', #60413, 1000.000000000000000 ) ;
#17098 = CARTESIAN_POINT ( 'NONE',  ( 5.515188684475870851, -0.001283816547384759822, 0.005194992164431476087 ) ) ;
#17100 = AXIS2_PLACEMENT_3D ( 'NONE', #44558, #34900, #39913 ) ;
#17101 = DIRECTION ( 'NONE',  ( 1.000000000000000000, 0.000000000000000000, 0.000000000000000000 ) ) ;
#17102 = EDGE_CURVE ( 'NONE', #35595, #18920, #48107, .T. ) ;
#17103 = CARTESIAN_POINT ( 'NONE',  ( -22.27718150314433387, -0.7862703917636514328, -3.596602356343918672 ) ) ;
#17104 = AXIS2_PLACEMENT_3D ( 'NONE', #13353, #33638, #48948 ) ;
#17105 = EDGE_CURVE ( 'NONE', #6053, #22102, #61670, .T. ) ;
#17106 = ORIENTED_EDGE ( 'NONE', *, *, #6617, .F. ) ;
#17107 = VECTOR ( 'NONE', #57111, 1000.000000000000000 ) ;
#17108 = LINE ( 'NONE', #22770, #14303 ) ;
#17109 = EDGE_CURVE ( 'NONE', #32649, #63467, #13207, .T. ) ;
#17110 = CARTESIAN_POINT ( 'NONE',  ( -22.28482751661422512, -3.048214341614495559, 2.105139449411428387 ) ) ;
#17111 = AXIS2_PLACEMENT_3D ( 'NONE', #13562, #13261, #2311 ) ;
#17112 = CYLINDRICAL_SURFACE ( 'NONE', #14162, 12.74999999999999822 ) ;
#17113 = DIRECTION ( 'NONE',  ( -1.000000000000000000, 0.000000000000000000, 0.000000000000000000 ) ) ;
#17114 = EDGE_CURVE ( 'NONE', #34626, #59781, #59771, .T. ) ;
#17115 = AXIS2_PLACEMENT_3D ( 'NONE', #10056, #31320, #61558 ) ;
#17116 = CARTESIAN_POINT ( 'NONE',  ( 1.719304012340653998, -9.242227816403676854, -8.755325027797448811 ) ) ;
#17117 = EDGE_CURVE ( 'NONE', #50873, #7202, #39593, .T. ) ;
#17118 = CARTESIAN_POINT ( 'NONE',  ( 9.213956812938336682, 1.933777648958550310, -11.84564966864138746 ) ) ;
#17119 = VERTEX_POINT ( 'NONE', #30116 ) ;
#17120 = DIRECTION ( 'NONE',  ( 0.000000000000000000, 0.9651210252299786685, 0.2618041379715667083 ) ) ;
#17121 = CARTESIAN_POINT ( 'NONE',  ( -27.08429572838383947, -1.608131779585707299, -1.632445743623455847 ) ) ;
#17122 = CARTESIAN_POINT ( 'NONE',  ( -35.00000000000000000, 3.213188559034398040, -11.29812557209473667 ) ) ;
#17123 = CARTESIAN_POINT ( 'NONE',  ( 2.844750968616420739, -1.686994672842389242, -7.651810733888938287 ) ) ;
#17124 = CIRCLE ( 'NONE', #26714, 2.899999999999994582 ) ;
#17125 = AXIS2_PLACEMENT_3D ( 'NONE', #34751, #55054, #48779 ) ;
#17126 = VECTOR ( 'NONE', #9495, 1000.000000000000000 ) ;
#17127 = EDGE_CURVE ( 'NONE', #59321, #6328, #50418, .T. ) ;
#17128 = CARTESIAN_POINT ( 'NONE',  ( -24.90406945800131311, 9.123033189230673301, 7.797728632319192776 ) ) ;
#17129 = DIRECTION ( 'NONE',  ( 1.000000000000000000, -0.000000000000000000, -0.000000000000000000 ) ) ;
#17130 = ORIENTED_EDGE ( 'NONE', *, *, #60548, .T. ) ;
#17131 = DIRECTION ( 'NONE',  ( -1.000000000000000000, -0.000000000000000000, -0.000000000000000000 ) ) ;
#17132 = CARTESIAN_POINT ( 'NONE',  ( 0.3675815128205894289, 2.391755495700764289, -12.04510820461657161 ) ) ;
#17133 = CARTESIAN_POINT ( 'NONE',  ( -37.00000000000000711, -2.346765782874520312, 11.95840593935200857 ) ) ;
#17134 = CARTESIAN_POINT ( 'NONE',  ( 1.547277799339153104, -12.58038279313752739, -1.534072017332470450 ) ) ;
#17135 = ORIENTED_EDGE ( 'NONE', *, *, #26536, .F. ) ;
#17136 = CARTESIAN_POINT ( 'NONE',  ( 145.1370849898475797, 3.309064568108273190E-14, 0.000000000000000000 ) ) ;
#17137 = CARTESIAN_POINT ( 'NONE',  ( -35.00000000000000000, 6.584150480049696164, -10.25474254703945931 ) ) ;
#17139 = ORIENTED_EDGE ( 'NONE', *, *, #9100, .F. ) ;
#17138 = CARTESIAN_POINT ( 'NONE',  ( 0.2651627923886338833, -12.24583724871547474, -0.08809136839528641794 ) ) ;
#17140 = CARTESIAN_POINT ( 'NONE',  ( -10.00000000000000178, 0.000000000000000000, 0.000000000000000000 ) ) ;
#17141 = VECTOR ( 'NONE', #25763, 1000.000000000000000 ) ;
#17142 = CIRCLE ( 'NONE', #41532, 7.499999999999988454 ) ;
#17143 = CARTESIAN_POINT ( 'NONE',  ( -37.25000000000000711, -20.00000000000000000, 1.500000000000002887 ) ) ;
#17144 = ORIENTED_EDGE ( 'NONE', *, *, #18184, .T. ) ;
#17145 = CIRCLE ( 'NONE', #1263, 6.936499999999990784 ) ;
#17146 = CARTESIAN_POINT ( 'NONE',  ( 0.3278977287071203062, -9.554671284920345897, 7.693417476735495697 ) ) ;
#17147 = CARTESIAN_POINT ( 'NONE',  ( -36.00000000000000711, 6.018036132182325915, -11.24036214326513949 ) ) ;
#17148 = DIRECTION ( 'NONE',  ( -1.000000000000000000, 0.000000000000000000, -0.000000000000000000 ) ) ;
#17149 = DIRECTION ( 'NONE',  ( -0.3939253465568943735, 0.8603393047165004415, -0.3234796780324220578 ) ) ;
#17150 = CARTESIAN_POINT ( 'NONE',  ( 26.08439714455133185, 12.97057518889166516, 3.743551691817328386 ) ) ;
#17151 = CIRCLE ( 'NONE', #63898, 2.899999999999994582 ) ;
#17152 = CARTESIAN_POINT ( 'NONE',  ( 0.7400311444011719031, 11.77295732453934640, 3.907401494354961979 ) ) ;
#17154 = ORIENTED_EDGE ( 'NONE', *, *, #53422, .T. ) ;
#17153 = CARTESIAN_POINT ( 'NONE',  ( -37.00000000000000711, -10.23119532541078058, 7.608228585767692564 ) ) ;
#17155 = CARTESIAN_POINT ( 'NONE',  ( -37.00000000000000711, 0.000000000000000000, 0.000000000000000000 ) ) ;
#17156 = ORIENTED_EDGE ( 'NONE', *, *, #15625, .F. ) ;
#17157 = CARTESIAN_POINT ( 'NONE',  ( 1.719304012338836563, -1.452142814150213734, 12.64775761152536759 ) ) ;
#17158 = ORIENTED_EDGE ( 'NONE', *, *, #35881, .T. ) ;
#17159 = CARTESIAN_POINT ( 'NONE',  ( -37.00000000000000711, 0.000000000000000000, 0.000000000000000000 ) ) ;
#17160 = CARTESIAN_POINT ( 'NONE',  ( -3.689171339445763032, 10.77932410358149795, 5.277713104131331434 ) ) ;
#17161 = ADVANCED_FACE ( 'NONE', ( #25450 ), #19998, .F. ) ;
#17162 = CARTESIAN_POINT ( 'NONE',  ( -48.79774903324594248, -0.2423453535664360781, -3.134413741627059213 ) ) ;
#17163 = CARTESIAN_POINT ( 'NONE',  ( -27.08429572838383947, 0.6096735944848206135, -2.208905845566032866 ) ) ;
#17164 = ORIENTED_EDGE ( 'NONE', *, *, #42843, .F. ) ;
#17165 = AXIS2_PLACEMENT_3D ( 'NONE', #29204, #49809, #44466 ) ;
#17166 = CARTESIAN_POINT ( 'NONE',  ( -24.60592215467821831, -6.662391132441423558, 9.982918610336051657 ) ) ;
#17167 = CARTESIAN_POINT ( 'NONE',  ( -22.39032720737627002, -3.847057950743281385, 1.170177197944854530 ) ) ;
#17168 = EDGE_LOOP ( 'NONE', ( #16513, #34548, #44568, #40380 ) ) ;
#17169 = VERTEX_POINT ( 'NONE', #37389 ) ;
#17170 = CARTESIAN_POINT ( 'NONE',  ( 2.907497136250630554, 7.666666002096657273, -1.716624290781218809 ) ) ;
#17171 = CIRCLE ( 'NONE', #54351, 12.18649999999999878 ) ;
#17172 = VECTOR ( 'NONE', #21049, 1000.000000000000000 ) ;
#17173 = EDGE_CURVE ( 'NONE', #32750, #50873, #27739, .T. ) ;
#17174 = EDGE_LOOP ( 'NONE', ( #3372, #6514, #43912, #41016 ) ) ;
#17175 = CARTESIAN_POINT ( 'NONE',  ( 29.03457606387295087, -7.862146963512102182, 10.97436308512422265 ) ) ;
#17176 = DIRECTION ( 'NONE',  ( -0.000000000000000000, -0.000000000000000000, -1.000000000000000000 ) ) ;
#17177 = CARTESIAN_POINT ( 'NONE',  ( 11.56167612769134045, 0.7121690593505338729, 13.48138618271499745 ) ) ;
#17178 = CARTESIAN_POINT ( 'NONE',  ( 1.104777566491141672, 12.40974092093472514, 1.703053712365368177 ) ) ;
#17179 = CIRCLE ( 'NONE', #55432, 12.18649999999999878 ) ;
#17180 = DIRECTION ( 'NONE',  ( 0.000000000000000000, 0.5472293298355215274, -0.8369827122275381726 ) ) ;
#17181 = DIRECTION ( 'NONE',  ( 0.000000000000000000, -0.01356324068817992175, 0.9999080150203990547 ) ) ;
#17182 = CIRCLE ( 'NONE', #60707, 5.000000000000000888 ) ;
#17183 = ADVANCED_FACE ( 'NONE', ( #27409 ), #47063, .T. ) ;
#17184 = DIRECTION ( 'NONE',  ( 0.000000000000000000, -0.7790879021242573810, 0.6269146997507903940 ) ) ;
#17185 = ORIENTED_EDGE ( 'NONE', *, *, #38962, .F. ) ;
#17186 = DIRECTION ( 'NONE',  ( 0.000000000000000000, -0.8276889981568840149, -0.5611870653623919347 ) ) ;
#17187 = EDGE_CURVE ( 'NONE', #34326, #37599, #49157, .T. ) ;
#17188 = ORIENTED_EDGE ( 'NONE', *, *, #25008, .T. ) ;
#17189 = CARTESIAN_POINT ( 'NONE',  ( 35.00000000000000000, 10.63508530065521640, -4.986700593229742573 ) ) ;
#17190 = EDGE_CURVE ( 'NONE', #6215, #23985, #42045, .T. ) ;
#17191 = CARTESIAN_POINT ( 'NONE',  ( -9.316487364114289349, -12.33901589261846254, -5.488921151462630377 ) ) ;
#17192 = CARTESIAN_POINT ( 'NONE',  ( 2.249013661412229137, -3.921976945965382377, 6.552953334857902767 ) ) ;
#17193 = CYLINDRICAL_SURFACE ( 'NONE', #38302, 7.499999999999988454 ) ;
#17194 = ORIENTED_EDGE ( 'NONE', *, *, #29215, .F. ) ;
#17195 = AXIS2_PLACEMENT_3D ( 'NONE', #61440, #1618, #16884 ) ;
#17196 = ORIENTED_EDGE ( 'NONE', *, *, #63421, .F. ) ;
#17197 = CARTESIAN_POINT ( 'NONE',  ( 0.2655924914740778187, 11.49267051747968438, 4.229867354073594043 ) ) ;
#17198 = CIRCLE ( 'NONE', #61805, 12.74999999999999822 ) ;
#17199 = EDGE_LOOP ( 'NONE', ( #65126, #44906, #47605, #22192 ) ) ;
#17200 = CARTESIAN_POINT ( 'NONE',  ( -29.92777678363736626, -3.750539801530011985, 11.39883551934754635 ) ) ;
#17201 = EDGE_CURVE ( 'NONE', #32661, #56228, #62934, .T. ) ;
#17202 = CARTESIAN_POINT ( 'NONE',  ( 8.489363379069230220, 5.256536079434125597, 10.79531771019706810 ) ) ;
#17203 = AXIS2_PLACEMENT_3D ( 'NONE', #12001, #62218, #16669 ) ;
#17204 = CARTESIAN_POINT ( 'NONE',  ( 5.514970785353741078, 0.003805873180274783798, 0.002796696073589750170 ) ) ;
#17205 = CARTESIAN_POINT ( 'NONE',  ( 0.2648978790185602672, -0.1321385342561549048, -12.24533305150758267 ) ) ;
#17206 = ADVANCED_FACE ( 'NONE', ( #36742 ), #16780, .T. ) ;
#17207 = ORIENTED_EDGE ( 'NONE', *, *, #27126, .T. ) ;
#17208 = CARTESIAN_POINT ( 'NONE',  ( 2.573738926104369718, 2.426778239006456062, 7.355212866432303542 ) ) ;
#17210 = VECTOR ( 'NONE', #44021, 1000.000000000000000 ) ;
#17209 = DIRECTION ( 'NONE',  ( 1.000000000000000000, -0.000000000000000000, 0.000000000000000000 ) ) ;
#17211 = CARTESIAN_POINT ( 'NONE',  ( 0.2653519890518156177, -10.60552241699063103, -6.123091032184257543 ) ) ;
#17212 = DIRECTION ( 'NONE',  ( 0.000000000000000000, -1.000000000000000000, 0.000000000000000000 ) ) ;
#17213 = ADVANCED_FACE ( 'NONE', ( #47705 ), #53016, .T. ) ;
#17214 = ADVANCED_FACE ( 'NONE', ( #11781 ), #57036, .T. ) ;
#17215 = EDGE_CURVE ( 'NONE', #30167, #50893, #304, .T. ) ;
#17216 = LINE ( 'NONE', #42131, #35144 ) ;
#17217 = VECTOR ( 'NONE', #7515, 1000.000000000000000 ) ;
#17218 = FACE_OUTER_BOUND ( 'NONE', #31749, .T. ) ;
#17219 = ORIENTED_EDGE ( 'NONE', *, *, #48125, .T. ) ;
#17221 = ADVANCED_FACE ( 'NONE', ( #62990 ), #52383, .T. ) ;
#17220 = CARTESIAN_POINT ( 'NONE',  ( 5.514970785353741078, 0.0003039746380528312057, 0.004713149585127536512 ) ) ;
#17222 = ORIENTED_EDGE ( 'NONE', *, *, #38128, .T. ) ;
#17223 = CARTESIAN_POINT ( 'NONE',  ( -5.434714954071925064, -0.9285630528112753801, -13.46803340916659231 ) ) ;
#17224 = CARTESIAN_POINT ( 'NONE',  ( 0.3675815128205912052, 9.574637318042068301, -7.689697408877177232 ) ) ;
#17225 = FACE_OUTER_BOUND ( 'NONE', #5088, .T. ) ;
#17226 = AXIS2_PLACEMENT_3D ( 'NONE', #49947, #33429, #64890 ) ;
#17227 = DIRECTION ( 'NONE',  ( 1.000000000000000000, 0.000000000000000000, 0.000000000000000000 ) ) ;
#17228 = DIRECTION ( 'NONE',  ( 1.000000000000000000, -0.000000000000000000, 0.000000000000000000 ) ) ;
#17229 = AXIS2_PLACEMENT_3D ( 'NONE', #61123, #20223, #40501 ) ;
#17230 = ORIENTED_EDGE ( 'NONE', *, *, #61029, .F. ) ;
#17231 = ORIENTED_EDGE ( 'NONE', *, *, #59094, .F. ) ;
#17232 = CARTESIAN_POINT ( 'NONE',  ( 0.2706063244538048362, 1.954041462022419573, 12.09107863371558089 ) ) ;
#17233 = ORIENTED_EDGE ( 'NONE', *, *, #64979, .F. ) ;
#17234 = CARTESIAN_POINT ( 'NONE',  ( 1.294038020999240590, 1.103269716799493150, 11.95280541775544592 ) ) ;
#17235 = CARTESIAN_POINT ( 'NONE',  ( 1.292668453954261221, 1.054608513093608924, -13.47545724770707487 ) ) ;
#17236 = DIRECTION ( 'NONE',  ( -1.000000000000000000, 0.000000000000000000, 0.000000000000000000 ) ) ;
#17237 = CARTESIAN_POINT ( 'NONE',  ( 0.3675815128205894289, 3.951233083390626177, -11.62724744438061641 ) ) ;
#17238 = DIRECTION ( 'NONE',  ( 0.000000000000000000, -0.01356324068817991828, 0.9999080150203990547 ) ) ;
#17239 = CARTESIAN_POINT ( 'NONE',  ( 2.256373768223415066, 7.545294827890042022, 1.195444820369703232 ) ) ;
#17240 = CARTESIAN_POINT ( 'NONE',  ( 35.00000000000000000, 4.705694406421931860E-17, -3.469127814946512892E-15 ) ) ;
#17241 = ORIENTED_EDGE ( 'NONE', *, *, #30308, .F. ) ;
#17242 = VERTEX_POINT ( 'NONE', #32393 ) ;
#17243 = CARTESIAN_POINT ( 'NONE',  ( 2.827825597296808269, -6.207590800588422830, 6.550135365664063514 ) ) ;
#17244 = EDGE_LOOP ( 'NONE', ( #17858, #46218, #50579, #24514 ) ) ;
#17245 = AXIS2_PLACEMENT_3D ( 'NONE', #35773, #20511, #51108 ) ;
#17246 = CARTESIAN_POINT ( 'NONE',  ( 24.82652845881425208, -10.42385221765392700, -8.578654028722157321 ) ) ;
#17247 = CIRCLE ( 'NONE', #3466, 2.899999999999994582 ) ;
#17248 = CARTESIAN_POINT ( 'NONE',  ( 35.00000000000000000, 9.321877890560537949, 7.146664589317804683 ) ) ;
#17249 = EDGE_CURVE ( 'NONE', #14636, #44685, #7747, .T. ) ;
#17250 = CARTESIAN_POINT ( 'NONE',  ( 41.00000000000000711, -25.03188948156373428, -4.500000000000011546 ) ) ;
#17251 = EDGE_LOOP ( 'NONE', ( #57084, #6980, #39743, #57494 ) ) ;
#17252 = FACE_OUTER_BOUND ( 'NONE', #44224, .T. ) ;
#17253 = VECTOR ( 'NONE', #50542, 1000.000000000000000 ) ;
#17254 = CARTESIAN_POINT ( 'NONE',  ( -17.03240540343445986, -29.48295256022982969, -9.532950799340856207 ) ) ;
#17255 = CARTESIAN_POINT ( 'NONE',  ( 35.00000000000000000, 9.217970097227839332, 7.971186206369370808 ) ) ;
#17256 = ORIENTED_EDGE ( 'NONE', *, *, #40682, .T. ) ;
#17257 = AXIS2_PLACEMENT_3D ( 'NONE', #59449, #13871, #38850 ) ;
#17258 = ORIENTED_EDGE ( 'NONE', *, *, #32557, .T. ) ;
#17259 = DIRECTION ( 'NONE',  ( 0.000000000000000000, -0.01356324068817999114, 0.9999080150203989437 ) ) ;
#17260 = VERTEX_POINT ( 'NONE', #12432 ) ;
#17261 = ORIENTED_EDGE ( 'NONE', *, *, #39669, .F. ) ;
#17262 = DIRECTION ( 'NONE',  ( 0.000000000000000000, 0.1740410799127544150, 0.9847383929261631641 ) ) ;
#17263 = ADVANCED_FACE ( 'NONE', ( #43033 ), #8941, .F. ) ;
#17264 = ORIENTED_EDGE ( 'NONE', *, *, #3843, .F. ) ;
#17265 = ORIENTED_EDGE ( 'NONE', *, *, #35342, .T. ) ;
#17266 = DIRECTION ( 'NONE',  ( 0.000000000000000000, 0.9796553971857749898, 0.2006870767258855104 ) ) ;
#17267 = CARTESIAN_POINT ( 'NONE',  ( -35.00000000000000000, 10.63508530065528923, -4.986700593229593359 ) ) ;
#17268 = FACE_OUTER_BOUND ( 'NONE', #5822, .T. ) ;
#17269 = CARTESIAN_POINT ( 'NONE',  ( -35.00000000000000000, -1.030638227056651424, 12.14284015767849567 ) ) ;
#17270 = CARTESIAN_POINT ( 'NONE',  ( 1.937114397841935398, -5.620553190833057045, 11.53912442307253450 ) ) ;
#17271 = CARTESIAN_POINT ( 'NONE',  ( -37.00000000000000711, -12.05416472667164207, -1.791059740004549372 ) ) ;
#17272 = VECTOR ( 'NONE', #17927, 1000.000000000000000 ) ;
#17273 = ORIENTED_EDGE ( 'NONE', *, *, #45320, .F. ) ;
#17274 = CARTESIAN_POINT ( 'NONE',  ( -35.00000000000000000, 0.000000000000000000, 0.000000000000000000 ) ) ;
#17275 = DIRECTION ( 'NONE',  ( 0.000000000000000000, -0.01356324068818000848, 0.9999080150203990547 ) ) ;
#17276 = EDGE_CURVE ( 'NONE', #36432, #47922, #27926, .T. ) ;
#17278 = DIRECTION ( 'NONE',  ( 1.000000000000000000, 0.000000000000000000, 0.000000000000000000 ) ) ;
#17277 = CIRCLE ( 'NONE', #51269, 5.000000000000001776 ) ;
#17279 = DIRECTION ( 'NONE',  ( -1.000000000000000000, 0.000000000000000000, 0.000000000000000000 ) ) ;
#17280 = FACE_OUTER_BOUND ( 'NONE', #11884, .T. ) ;
#17281 = CIRCLE ( 'NONE', #27914, 4.999999999999999112 ) ;
#17282 = VECTOR ( 'NONE', #12058, 1000.000000000000000 ) ;
#17283 = ORIENTED_EDGE ( 'NONE', *, *, #37826, .T. ) ;
#17284 = CARTESIAN_POINT ( 'NONE',  ( -14.11589373245165469, 8.250315036047107142, -8.713914264323175729 ) ) ;
#17285 =( BOUNDED_CURVE ( )  B_SPLINE_CURVE ( 3, ( #57237, #46281, #61544, #723 ),
 .UNSPECIFIED., .F., .F. ) 
 B_SPLINE_CURVE_WITH_KNOTS ( ( 4, 4 ),
 ( 5.023979252657118977, 5.040864206341344911 ),
 .UNSPECIFIED. ) 
 CURVE ( )  GEOMETRIC_REPRESENTATION_ITEM ( )  RATIONAL_B_SPLINE_CURVE ( ( 1.000000000000000000, 0.9999762416693727118, 0.9999762416693727118, 1.000000000000000000 ) ) 
 REPRESENTATION_ITEM ( '' )  );
#17286 = VERTEX_POINT ( 'NONE', #33957 ) ;
#17287 = DIRECTION ( 'NONE',  ( -1.000000000000000000, 0.000000000000000000, -0.000000000000000000 ) ) ;
#17288 = CARTESIAN_POINT ( 'NONE',  ( 2.255723233588949661, 5.936060085173614276, -4.808373255828823467 ) ) ;
#17289 = CARTESIAN_POINT ( 'NONE',  ( 9.967256768512323006, -13.45016586142041959, -1.162363687967992165 ) ) ;
#17290 = FACE_OUTER_BOUND ( 'NONE', #55969, .T. ) ;
#17291 = CARTESIAN_POINT ( 'NONE',  ( 2.770579946183333586, -4.784693811915849970, -6.173813901927596604 ) ) ;
#17292 = EDGE_LOOP ( 'NONE', ( #55282, #47623, #24904, #45673 ) ) ;
#17293 = VECTOR ( 'NONE', #31427, 1000.000000000000227 ) ;
#17294 = CYLINDRICAL_SURFACE ( 'NONE', #7993, 4.999999999999999112 ) ;
#17295 = CARTESIAN_POINT ( 'NONE',  ( 35.00000000000000000, 3.827046518385079032, -11.56998259273179386 ) ) ;
#17296 = B_SPLINE_CURVE_WITH_KNOTS ( 'NONE', 3,
 ( #47283, #1723, #21989, #22301, #32929, #17988, #18334, #32595, #38249, #43567, #2728, #38599, #27972, #43241, #18670, #52903, #2383, #59217 ),
 .UNSPECIFIED., .F., .F.,
 ( 4, 2, 2, 2, 2, 2, 2, 2, 4 ),
 ( 0.000000000000000000, 0.0008320272794029127473, 0.001664054558805825495, 0.002496081838208737917, 0.003328109117611650989, 0.004160136397014563628, 0.004992163676417476700, 0.005824190955820389773, 0.006656218235223304580 ),
 .UNSPECIFIED. ) ;
#17297 = CARTESIAN_POINT ( 'NONE',  ( 35.00000000000000000, 10.99909370905164430, 5.246972444133898072 ) ) ;
#17298 = CARTESIAN_POINT ( 'NONE',  ( -3.472928581034699924, 8.809056386856843446, 10.25973817351390416 ) ) ;
#17299 = EDGE_CURVE ( 'NONE', #43792, #43254, #46694, .T. ) ;
#17300 = AXIS2_PLACEMENT_3D ( 'NONE', #48256, #18645, #38905 ) ;
#17301 = EDGE_CURVE ( 'NONE', #41809, #15421, #16553, .T. ) ;
#17302 = DIRECTION ( 'NONE',  ( 0.000000000000000000, -0.01356324068817992175, 0.9999080150203990547 ) ) ;
#17303 = VERTEX_POINT ( 'NONE', #4378 ) ;
#17304 = B_SPLINE_CURVE_WITH_KNOTS ( 'NONE', 3,
 ( #1804, #62297, #16751, #37024, #22389, #57327, #11749, #32036, #6796, #17077, #27070, #47361, #37357, #57668, #12090, #32368 ),
 .UNSPECIFIED., .F., .F.,
 ( 4, 3, 3, 3, 3, 4 ),
 ( 0.000000000000000000, 0.0002999043160757280165, 0.0005998071753050859302, 0.0008997092107374342861, 0.001204458948194992189, 0.001510329163475222867 ),
 .UNSPECIFIED. ) ;
#17305 = VECTOR ( 'NONE', #20699, 1000.000000000000000 ) ;
#17306 = PRODUCT_DEFINITION_CONTEXT ( 'detailed design', #12786, 'design' ) ;
#17308 = EDGE_CURVE ( 'NONE', #59495, #51211, #45963, .T. ) ;
#17307 = CARTESIAN_POINT ( 'NONE',  ( 37.00000000000000711, -3.093009498343839869, 11.78745411414842437 ) ) ;
#17309 = CARTESIAN_POINT ( 'NONE',  ( 0.2648978790185619880, -1.996248716311710414, 12.08224454301447892 ) ) ;
#17310 = ORIENTED_EDGE ( 'NONE', *, *, #8748, .T. ) ;
#17311 = ORIENTED_EDGE ( 'NONE', *, *, #52586, .T. ) ;
#17312 = CARTESIAN_POINT ( 'NONE',  ( 0.2646305136544065406, 10.53923716745246608, 6.237419468587114935 ) ) ;
#17313 = CARTESIAN_POINT ( 'NONE',  ( 0.2652384529303146166, 2.191562200667183546, 12.04846370803829103 ) ) ;
#17314 = CARTESIAN_POINT ( 'NONE',  ( 35.62304844322793684, -2.500997609376311548, 21.53526926371174000 ) ) ;
#17315 = DIRECTION ( 'NONE',  ( -1.000000000000000000, -1.836970198721029688E-16, -0.000000000000000000 ) ) ;
#17316 = LINE ( 'NONE', #8316, #34966 ) ;
#17317 = ORIENTED_EDGE ( 'NONE', *, *, #12422, .T. ) ;
#17318 = CIRCLE ( 'NONE', #62970, 5.000000000000000888 ) ;
#17319 = VECTOR ( 'NONE', #53061, 1000.000000000000000 ) ;
#17320 = EDGE_LOOP ( 'NONE', ( #59894, #19864, #9874, #55466 ) ) ;
#17321 = ORIENTED_EDGE ( 'NONE', *, *, #12758, .T. ) ;
#17322 = FACE_OUTER_BOUND ( 'NONE', #52539, .T. ) ;
#17323 = AXIS2_PLACEMENT_3D ( 'NONE', #23690, #9036, #14984 ) ;
#17324 = DIRECTION ( 'NONE',  ( 1.000000000000000000, -0.000000000000000000, 0.000000000000000000 ) ) ;
#17325 = EDGE_CURVE ( 'NONE', #64117, #54444, #1402, .T. ) ;
#17326 = ORIENTED_EDGE ( 'NONE', *, *, #21466, .T. ) ;
#17327 = CARTESIAN_POINT ( 'NONE',  ( 2.000000000000001776, 6.812627895098307462, -0.04423456934727655609 ) ) ;
#17328 = DIRECTION ( 'NONE',  ( 0.000000000000000000, -0.01356324068818685717, 0.9999080150203989437 ) ) ;
#17329 = EDGE_CURVE ( 'NONE', #45530, #34672, #47060, .T. ) ;
#17330 = VERTEX_POINT ( 'NONE', #29308 ) ;
#17331 = DIRECTION ( 'NONE',  ( 0.000000000000000000, 0.000000000000000000, 1.000000000000000000 ) ) ;
#17332 = DIRECTION ( 'NONE',  ( 0.000000000000000000, 0.01356324068817992175, -0.9999080150203990547 ) ) ;
#17333 = DIRECTION ( 'NONE',  ( 0.000000000000000000, 0.4134677391718512007, 0.9105187689795953832 ) ) ;
#17334 = ORIENTED_EDGE ( 'NONE', *, *, #42675, .F. ) ;
#17335 = AXIS2_PLACEMENT_3D ( 'NONE', #6663, #31895, #21626 ) ;
#17336 = ORIENTED_EDGE ( 'NONE', *, *, #21479, .F. ) ;
#17337 = CARTESIAN_POINT ( 'NONE',  ( -16.98800322446194855, 2.922502605998049674, 25.00000000000000000 ) ) ;
#17338 = EDGE_LOOP ( 'NONE', ( #53383, #41493, #6316, #4735 ) ) ;
#17339 = DIRECTION ( 'NONE',  ( 1.000000000000000000, 0.000000000000000000, 0.000000000000000000 ) ) ;
#17340 = EDGE_CURVE ( 'NONE', #30787, #45191, #41859, .T. ) ;
#17341 = LINE ( 'NONE', #51619, #39352 ) ;
#17342 = CARTESIAN_POINT ( 'NONE',  ( 2.665405856346790614, -2.723742051529387975, -9.171500569027763561 ) ) ;
#17343 = LINE ( 'NONE', #16675, #5032 ) ;
#17344 = CARTESIAN_POINT ( 'NONE',  ( 0.000000000000000000, -6.796153407501424049, -1.388283512725909219 ) ) ;
#17345 = CARTESIAN_POINT ( 'NONE',  ( -22.31328051695926007, -3.781397440874596061, 0.2528478350593901802 ) ) ;
#17346 = DIRECTION ( 'NONE',  ( 1.000000000000000000, 0.000000000000000000, -0.000000000000000000 ) ) ;
#17347 = CARTESIAN_POINT ( 'NONE',  ( 6.530088489467589241, -4.706431572448715350, -11.04498340397446654 ) ) ;
#17348 = ORIENTED_EDGE ( 'NONE', *, *, #27310, .F. ) ;
#17349 = CARTESIAN_POINT ( 'NONE',  ( -35.00000000000000000, 0.000000000000000000, 0.000000000000000000 ) ) ;
#17350 = EDGE_LOOP ( 'NONE', ( #389, #37607, #20759, #61369 ) ) ;
#17351 = DIRECTION ( 'NONE',  ( 0.000000000000000000, 0.01356324068818000848, -0.9999080150203990547 ) ) ;
#17352 = CIRCLE ( 'NONE', #53484, 4.999999999999999112 ) ;
#17353 = CARTESIAN_POINT ( 'NONE',  ( 2.251152103361936163, 6.676162264138683966, 3.709836606815780424 ) ) ;
#17354 = EDGE_CURVE ( 'NONE', #35137, #3903, #40250, .T. ) ;
#17355 = ADVANCED_FACE ( 'NONE', ( #24648 ), #14973, .T. ) ;
#17356 = ORIENTED_EDGE ( 'NONE', *, *, #32945, .T. ) ;
#17357 = CARTESIAN_POINT ( 'NONE',  ( 1.719304012339893051, -12.70777170743898310, 0.7661785589588769874 ) ) ;
#17358 = DIRECTION ( 'NONE',  ( -0.000000000000000000, -1.000000000000000000, -0.000000000000000000 ) ) ;
#17359 = CARTESIAN_POINT ( 'NONE',  ( 0.2739690278137246748, -2.307031017960371688, -12.02985305092653334 ) ) ;
#17360 = EDGE_CURVE ( 'NONE', #6941, #22369, #40680, .T. ) ;
#17361 = EDGE_LOOP ( 'NONE', ( #42903, #29088, #45630, #3699 ) ) ;
#17362 = AXIS2_PLACEMENT_3D ( 'NONE', #55388, #8857, #19157 ) ;
#17363 = ORIENTED_EDGE ( 'NONE', *, *, #7567, .T. ) ;
#17364 = DIRECTION ( 'NONE',  ( 0.000000000000000000, 0.7381862504171926576, -0.6745969609292690183 ) ) ;
#17365 = ORIENTED_EDGE ( 'NONE', *, *, #62921, .F. ) ;
#17366 = CARTESIAN_POINT ( 'NONE',  ( -47.00000000000000711, 0.000000000000000000, 0.000000000000000000 ) ) ;
#17367 = CARTESIAN_POINT ( 'NONE',  ( -35.00000000000000000, -1.488153103997047033, 11.65150730582934102 ) ) ;
#17368 = CARTESIAN_POINT ( 'NONE',  ( -35.04660725145885891, -0.01191704700713449618, 0.003039313842342893004 ) ) ;
#17369 = CARTESIAN_POINT ( 'NONE',  ( -18.71095331498199243, -4.888783180482830559, 10.95964276331128318 ) ) ;
#17370 = VERTEX_POINT ( 'NONE', #44926 ) ;
#17371 = CIRCLE ( 'NONE', #25866, 6.936499999999989896 ) ;
#17372 = AXIS2_PLACEMENT_3D ( 'NONE', #30001, #65258, #59623 ) ;
#17373 = DIRECTION ( 'NONE',  ( 0.000000000000000000, -0.2960891610144378849, -0.9551603052523519599 ) ) ;
#17374 = EDGE_CURVE ( 'NONE', #48262, #53955, #45572, .T. ) ;
#17375 = CIRCLE ( 'NONE', #58840, 12.75000000000000178 ) ;
#17376 = AXIS2_PLACEMENT_3D ( 'NONE', #36450, #41761, #42726 ) ;
#17377 = EDGE_CURVE ( 'NONE', #55094, #23142, #33233, .T. ) ;
#17378 = CARTESIAN_POINT ( 'NONE',  ( -27.45775109278350712, -13.35262336282553441, -1.989333891161978674 ) ) ;
#17379 = DIRECTION ( 'NONE',  ( -1.000000000000000000, 0.000000000000000000, 0.000000000000000000 ) ) ;
#17380 = VECTOR ( 'NONE', #25874, 1000.000000000000000 ) ;
#17381 = CARTESIAN_POINT ( 'NONE',  ( -36.00000000000000711, 10.02106554660708859, 7.882940143791811849 ) ) ;
#17382 = DIRECTION ( 'NONE',  ( -1.000000000000000000, 0.000000000000000000, 0.000000000000000000 ) ) ;
#17383 = DIRECTION ( 'NONE',  ( -1.000000000000000000, -0.000000000000000000, 0.000000000000000000 ) ) ;
#17384 = FACE_OUTER_BOUND ( 'NONE', #23870, .T. ) ;
#17385 = CARTESIAN_POINT ( 'NONE',  ( -22.27878402819508352, -2.612733676624904522, -2.600576127690928718 ) ) ;
#17386 = AXIS2_PLACEMENT_3D ( 'NONE', #19506, #34759, #55061 ) ;
#17387 = AXIS2_PLACEMENT_3D ( 'NONE', #26387, #46670, #36694 ) ;
#17388 = EDGE_LOOP ( 'NONE', ( #15664, #9294, #15283, #45165 ) ) ;
#17389 = CARTESIAN_POINT ( 'NONE',  ( -27.04788180060269198, 1.373100113388795673, 2.923150379392631670 ) ) ;
#17390 = CARTESIAN_POINT ( 'NONE',  ( 4.038317478791936033, -10.40617629760990859, 8.603232183407900635 ) ) ;
#17391 = VERTEX_POINT ( 'NONE', #55893 ) ;
#17392 = CARTESIAN_POINT ( 'NONE',  ( -22.27706485742869091, 3.662257305743817692, -0.3729136217355926153 ) ) ;
#17393 = DIRECTION ( 'NONE',  ( -1.000000000000000000, -0.000000000000000000, 0.000000000000000000 ) ) ;
#17394 = AXIS2_PLACEMENT_3D ( 'NONE', #22163, #57769, #43763 ) ;
#17395 = ORIENTED_EDGE ( 'NONE', *, *, #35412, .T. ) ;
#17396 = CARTESIAN_POINT ( 'NONE',  ( 2.284126774969133855, 6.543266298866131869, 3.960764882115977770 ) ) ;
#17397 = VERTEX_POINT ( 'NONE', #19676 ) ;
#17398 = FACE_OUTER_BOUND ( 'NONE', #54858, .T. ) ;
#17399 = ORIENTED_EDGE ( 'NONE', *, *, #12828, .F. ) ;
#17400 = ORIENTED_EDGE ( 'NONE', *, *, #38317, .F. ) ;
#17401 = CARTESIAN_POINT ( 'NONE',  ( -35.00000000000000000, 11.50504120060943158, 4.018060380616439886 ) ) ;
#17402 = CIRCLE ( 'NONE', #55623, 12.75000000000000178 ) ;
#17403 = ORIENTED_EDGE ( 'NONE', *, *, #27108, .T. ) ;
#17404 = CARTESIAN_POINT ( 'NONE',  ( -27.27855387000350262, -10.59660315834921107, 5.631341004100471892 ) ) ;
#17405 = CARTESIAN_POINT ( 'NONE',  ( 0.000000000000000000, 0.000000000000000000, 0.000000000000000000 ) ) ;
#17406 = DIRECTION ( 'NONE',  ( 0.000000000000000000, 0.01356324068817992175, -0.9999080150203990547 ) ) ;
#17407 = FACE_OUTER_BOUND ( 'NONE', #21846, .T. ) ;
#17408 = EDGE_CURVE ( 'NONE', #42135, #35454, #9868, .T. ) ;
#17409 = ORIENTED_EDGE ( 'NONE', *, *, #42067, .F. ) ;
#17410 = CARTESIAN_POINT ( 'NONE',  ( -35.00000000000000000, 5.015831474386455824, -10.62137734850263016 ) ) ;
#17411 = CARTESIAN_POINT ( 'NONE',  ( -3.416103270178013407, -31.26314776370590209, 14.19449313401761081 ) ) ;
#17412 = CARTESIAN_POINT ( 'NONE',  ( -2.952869152607111136, 4.384817011589738911, 11.17020052527586138 ) ) ;
#17414 = ORIENTED_EDGE ( 'NONE', *, *, #27685, .T. ) ;
#17413 = LINE ( 'NONE', #37689, #52085 ) ;
#17415 = DIRECTION ( 'NONE',  ( 1.000000000000000000, 0.000000000000000000, -0.000000000000000000 ) ) ;
#17416 = VERTEX_POINT ( 'NONE', #3748 ) ;
#17417 = CARTESIAN_POINT ( 'NONE',  ( 0.2646305136544072623, 6.237419468587079407, 10.53923716745249095 ) ) ;
#17418 = AXIS2_PLACEMENT_3D ( 'NONE', #64424, #9219, #29502 ) ;
#17419 = ORIENTED_EDGE ( 'NONE', *, *, #57768, .T. ) ;
#17420 = FACE_OUTER_BOUND ( 'NONE', #32679, .T. ) ;
#17421 = CARTESIAN_POINT ( 'NONE',  ( -35.00000000000000000, -12.68495603654570836, -1.286231064351444742 ) ) ;
#17423 = DIRECTION ( 'NONE',  ( 0.000000000000000000, 0.01356324068817998940, -0.9999080150203990547 ) ) ;
#17422 = AXIS2_PLACEMENT_3D ( 'NONE', #23700, #63568, #18043 ) ;
#17424 = ORIENTED_EDGE ( 'NONE', *, *, #31435, .F. ) ;
#17425 = ADVANCED_FACE ( 'NONE', ( #14639 ), #26799, .F. ) ;
#17426 = CARTESIAN_POINT ( 'NONE',  ( -35.00000000000000000, -8.146229107149334681, -9.063649021439044162 ) ) ;
#17427 = CARTESIAN_POINT ( 'NONE',  ( 5.515188684475870851, -0.004442604682416460317, -0.002983184900674899515 ) ) ;
#17428 = CARTESIAN_POINT ( 'NONE',  ( 2.241537034860906719, -5.851376807350176179, 4.903726641589506663 ) ) ;
#17429 = ORIENTED_EDGE ( 'NONE', *, *, #60292, .F. ) ;
#17430 = AXIS2_PLACEMENT_3D ( 'NONE', #12777, #42058, #32409 ) ;
#17431 = ORIENTED_EDGE ( 'NONE', *, *, #36328, .F. ) ;
#17432 = CARTESIAN_POINT ( 'NONE',  ( -36.00000000000000711, 12.08151691381196002, -4.074242145635880163 ) ) ;
#17433 = ORIENTED_EDGE ( 'NONE', *, *, #22048, .T. ) ;
#17434 = B_SPLINE_CURVE_WITH_KNOTS ( 'NONE', 3,
 ( #46208, #20909, #56499, #41183, #61465, #31230, #53146, #6292, #47832, #27534, #16594, #41854 ),
 .UNSPECIFIED., .F., .F.,
 ( 4, 2, 2, 2, 2, 4 ),
 ( 2.693015029076738270E-17, 0.002303342557757002800, 0.004606685115513976109, 0.005758356394392463197, 0.006910027673270949418, 0.009213370231027924462 ),
 .UNSPECIFIED. ) ;
#17435 = ORIENTED_EDGE ( 'NONE', *, *, #9364, .F. ) ;
#17436 = AXIS2_PLACEMENT_3D ( 'NONE', #6480, #51718, #26758 ) ;
#17437 = DIRECTION ( 'NONE',  ( 0.000000000000000000, 0.000000000000000000, -1.000000000000000000 ) ) ;
#17438 = CARTESIAN_POINT ( 'NONE',  ( 35.00000000000000000, -7.110831038798346881, -9.896810808925367908 ) ) ;
#17439 = CARTESIAN_POINT ( 'NONE',  ( 35.00000000000000000, 4.705694406421931860E-17, -3.469127814946512892E-15 ) ) ;
#17440 = CARTESIAN_POINT ( 'NONE',  ( 1.000000000000000888, -4.472310526050724100, -6.020667617347421618 ) ) ;
#17441 = DIRECTION ( 'NONE',  ( 0.000000000000000000, 0.000000000000000000, 1.000000000000000000 ) ) ;
#17442 = AXIS2_PLACEMENT_3D ( 'NONE', #6177, #27104, #17120 ) ;
#17443 = CARTESIAN_POINT ( 'NONE',  ( -37.00000000000000711, 11.42599468261435192, -4.237620530777677530 ) ) ;
#17444 = DIRECTION ( 'NONE',  ( 0.000000000000000000, 0.9970832820307041766, 0.07632122047556146038 ) ) ;
#17445 = VERTEX_POINT ( 'NONE', #21956 ) ;
#17446 = AXIS2_PLACEMENT_3D ( 'NONE', #4509, #35391, #10784 ) ;
#17447 = CARTESIAN_POINT ( 'NONE',  ( 0.3675815128205912052, 12.04510820461662668, -2.391755495700480516 ) ) ;
#17448 = CARTESIAN_POINT ( 'NONE',  ( 47.00000000000000711, 4.705694406421931860E-17, -3.469127814946512892E-15 ) ) ;
#17449 = EDGE_CURVE ( 'NONE', #50524, #14759, #36594, .T. ) ;
#17450 = CARTESIAN_POINT ( 'NONE',  ( 2.297017764050095057, -4.791851130936013448, 5.967068736727098255 ) ) ;
#17451 = CARTESIAN_POINT ( 'NONE',  ( -35.00000000000000000, 0.000000000000000000, 0.000000000000000000 ) ) ;
#17452 = AXIS2_PLACEMENT_3D ( 'NONE', #45556, #44909, #60868 ) ;
#17453 = CARTESIAN_POINT ( 'NONE',  ( -35.00000000000000000, 0.000000000000000000, 0.000000000000000000 ) ) ;
#17454 = DIRECTION ( 'NONE',  ( -1.000000000000000000, 0.000000000000000000, -0.000000000000000000 ) ) ;
#17455 = CARTESIAN_POINT ( 'NONE',  ( 12.52750123246316072, 0.4973700281276248192, -11.98968819674306374 ) ) ;
#17456 = ORIENTED_EDGE ( 'NONE', *, *, #16718, .T. ) ;
#17457 = CARTESIAN_POINT ( 'NONE',  ( -34.00000000000000000, 1.836970198721035357E-16, 0.000000000000000000 ) ) ;
#17458 = AXIS2_PLACEMENT_3D ( 'NONE', #60653, #60320, #15091 ) ;
#17459 = DIRECTION ( 'NONE',  ( -1.000000000000000000, 0.000000000000000000, 0.000000000000000000 ) ) ;
#17460 = CARTESIAN_POINT ( 'NONE',  ( 35.00000000000000000, 7.745827850123149005, 10.12742074351887744 ) ) ;
#17461 = AXIS2_PLACEMENT_3D ( 'NONE', #42453, #11563, #31836 ) ;
#17462 = CARTESIAN_POINT ( 'NONE',  ( -17.72811806012732916, -13.27197368940280064, 2.555533621652877230 ) ) ;
#17463 = ADVANCED_FACE ( 'NONE', ( #5700, #31907 ), #56895, .F. ) ;
#17464 = CARTESIAN_POINT ( 'NONE',  ( -25.27881376661855484, 6.347467180810850707, 10.18972282614729608 ) ) ;
#17465 = CARTESIAN_POINT ( 'NONE',  ( -25.80019021537189516, -11.91931523669747151, 6.339780118509601436 ) ) ;
#17466 = ORIENTED_EDGE ( 'NONE', *, *, #60136, .T. ) ;
#17467 = CARTESIAN_POINT ( 'NONE',  ( 2.903928887688250970, 6.365315087929518612, -6.032681461746785878 ) ) ;
#17468 = CARTESIAN_POINT ( 'NONE',  ( -37.00000000000000711, -11.23004253107761130, -4.732539170486383284 ) ) ;
#17469 = CARTESIAN_POINT ( 'NONE',  ( -37.00000000000000711, -4.545979934229493757, 11.30684963584387859 ) ) ;
#17470 = DIRECTION ( 'NONE',  ( -1.000000000000000000, 0.000000000000000000, 0.000000000000000000 ) ) ;
#17471 = ORIENTED_EDGE ( 'NONE', *, *, #20317, .F. ) ;
#17472 = CARTESIAN_POINT ( 'NONE',  ( 23.57978631083511445, 11.05404059788998161, -7.754718420896370645 ) ) ;
#17473 = CARTESIAN_POINT ( 'NONE',  ( 37.00000000000000711, 11.72397916322012179, -0.7214809346829029746 ) ) ;
#17474 = VERTEX_POINT ( 'NONE', #6030 ) ;
#17475 = ORIENTED_EDGE ( 'NONE', *, *, #47479, .T. ) ;
#17476 = DIRECTION ( 'NONE',  ( 0.000000000000000000, -0.01356324068817999114, 0.9999080150203989437 ) ) ;
#17478 = CIRCLE ( 'NONE', #34459, 12.74999999999999822 ) ;
#17477 = AXIS2_PLACEMENT_3D ( 'NONE', #34147, #3613, #38827 ) ;
#17479 = DIRECTION ( 'NONE',  ( 0.000000000000000000, 0.01356324068817991481, -0.9999080150203990547 ) ) ;
#17480 = ORIENTED_EDGE ( 'NONE', *, *, #140, .F. ) ;
#17481 = CARTESIAN_POINT ( 'NONE',  ( 0.2648321136542702292, -9.471460387169321038, 7.762514728658064911 ) ) ;
#17482 = PLANE ( 'NONE',  #37871 ) ;
#17483 = CARTESIAN_POINT ( 'NONE',  ( -37.00000000000000711, 8.927548052241016663, -8.295159312811756891 ) ) ;
#17484 = CYLINDRICAL_SURFACE ( 'NONE', #14910, 6.936499999999988120 ) ;
#17485 = EDGE_CURVE ( 'NONE', #4690, #9839, #26872, .T. ) ;
#17486 =( BOUNDED_SURFACE ( )  B_SPLINE_SURFACE ( 3, 1, ( 
 ( #6448, #52668 ),
 ( #17742, #12723 ),
 ( #1793, #38000 ),
 ( #11423, #42314 ) ),
 .UNSPECIFIED., .F., .F., .F. ) 
 B_SPLINE_SURFACE_WITH_KNOTS ( ( 4, 4 ),
 ( 2, 2 ),
 ( 0.000000000000000000, 1.000000000000000000 ),
 ( 0.000000000000000000, 1.000000000000000000 ),
 .UNSPECIFIED. ) 
 GEOMETRIC_REPRESENTATION_ITEM ( )  RATIONAL_B_SPLINE_SURFACE ( (
 ( 1.000000000000000000, 1.000000000000000000),
 ( 0.6933888150995267674, 0.9895912004443193632),
 ( 0.6933888150995267674, 0.9895912004443193632),
 ( 1.000000000000000000, 1.000000000000000000) ) ) 
 REPRESENTATION_ITEM ( '' )  SURFACE ( )  );
#17487 = DIRECTION ( 'NONE',  ( -1.000000000000000000, 0.000000000000000000, 0.000000000000000000 ) ) ;
#17488 = CARTESIAN_POINT ( 'NONE',  ( 0.2706063244538030044, 5.971590789837518898, 10.69357582853948863 ) ) ;
#17490 = VERTEX_POINT ( 'NONE', #62187 ) ;
#17489 = DIRECTION ( 'NONE',  ( -1.000000000000000000, -0.000000000000000000, 0.000000000000000000 ) ) ;
#17491 = EDGE_CURVE ( 'NONE', #54227, #17416, #15187, .T. ) ;
#17492 = DIRECTION ( 'NONE',  ( -1.000000000000000000, 0.000000000000000000, 0.000000000000000000 ) ) ;
#17493 = ORIENTED_EDGE ( 'NONE', *, *, #18400, .F. ) ;
#17494 = DIRECTION ( 'NONE',  ( -1.000000000000000000, 0.000000000000000000, 0.000000000000000000 ) ) ;
#17495 = ORIENTED_EDGE ( 'NONE', *, *, #8361, .F. ) ;
#17496 = ORIENTED_EDGE ( 'NONE', *, *, #24914, .T. ) ;
#17497 = PRODUCT_CONTEXT ( 'NONE', #27271, 'mechanical' ) ;
#17498 = CARTESIAN_POINT ( 'NONE',  ( 1.014383007554949367, -11.58298623339617706, 4.688516792764573893 ) ) ;
#17499 = CARTESIAN_POINT ( 'NONE',  ( -22.27722022243424149, 3.619868281251748421, -0.6721023714405434113 ) ) ;
#17500 = CARTESIAN_POINT ( 'NONE',  ( -17.16655223576323408, 3.059552638032528638, 11.60427096643701361 ) ) ;
#17501 = VECTOR ( 'NONE', #40829, 1000.000000000000000 ) ;
#17502 = EDGE_CURVE ( 'NONE', #4318, #4780, #33804, .T. ) ;
#17503 = CARTESIAN_POINT ( 'NONE',  ( -37.67868074218839780, -2.196220884325941203, -20.39261666198438760 ) ) ;
#17504 = CARTESIAN_POINT ( 'NONE',  ( -28.85619398320021745, 3.750539801530000439, 25.00000000000000000 ) ) ;
#17505 = ORIENTED_EDGE ( 'NONE', *, *, #12828, .T. ) ;
#17506 = CARTESIAN_POINT ( 'NONE',  ( -22.27721038036499834, -0.5802312083658355268, -3.635620891621751394 ) ) ;
#17508 = EDGE_CURVE ( 'NONE', #38941, #51664, #36909, .T. ) ;
#17507 = CARTESIAN_POINT ( 'NONE',  ( 3.154808525168153022, 2.889958543828632820, -13.21403070427456505 ) ) ;
#17509 = EDGE_LOOP ( 'NONE', ( #37193, #1906, #18851, #20630 ) ) ;
#17510 = EDGE_LOOP ( 'NONE', ( #48559, #57136, #22654, #34618 ) ) ;
#17511 = CARTESIAN_POINT ( 'NONE',  ( 5.520433897694421610, -0.01329351892498009322, -0.007082458259338525290 ) ) ;
#17512 = EDGE_CURVE ( 'NONE', #1280, #27364, #37498, .T. ) ;
#17513 = MECHANICAL_DESIGN_GEOMETRIC_PRESENTATION_REPRESENTATION (  '', ( #46184 ), #50457 ) ;
#17514 = ORIENTED_EDGE ( 'NONE', *, *, #20860, .T. ) ;
#17515 = CARTESIAN_POINT ( 'NONE',  ( 37.00000000000000711, -11.78745411414841726, -3.093009498343884722 ) ) ;
#17516 = CARTESIAN_POINT ( 'NONE',  ( 5.516018279890452902, 0.006629829924290471695, -0.001397286410094441449 ) ) ;
#17517 = CARTESIAN_POINT ( 'NONE',  ( 35.00000000000000000, 7.215058775251253387, -9.821084925794595577 ) ) ;
#17518 = DIRECTION ( 'NONE',  ( 6.123233995736778362E-17, -0.8660254037844380415, 0.5000000000000009992 ) ) ;
#17519 = FACE_OUTER_BOUND ( 'NONE', #45189, .T. ) ;
#17520 = CARTESIAN_POINT ( 'NONE',  ( -28.82752767077929335, 2.766519351427261686, 13.23585947174678701 ) ) ;
#17521 = ADVANCED_FACE ( 'NONE', ( #5357 ), #10997, .T. ) ;
#17522 = DIRECTION ( 'NONE',  ( 1.000000000000000000, 0.000000000000000000, 0.000000000000000000 ) ) ;
#17523 = EDGE_LOOP ( 'NONE', ( #47756, #53921, #18132, #47565 ) ) ;
#17524 = CIRCLE ( 'NONE', #54690, 7.938172270156617749 ) ;
#17525 = CARTESIAN_POINT ( 'NONE',  ( -35.00000000000000000, 10.84030624090606487, 6.711949091238180287 ) ) ;
#17526 = ORIENTED_EDGE ( 'NONE', *, *, #42176, .F. ) ;
#17527 = PRODUCT_DEFINITION_SHAPE ( 'NONE', 'NONE',  #65812 ) ;
#17528 = CARTESIAN_POINT ( 'NONE',  ( 0.2653519789438738008, -6.104019611498650910, 10.61653328464225687 ) ) ;
#17529 = CARTESIAN_POINT ( 'NONE',  ( -35.04709527796842394, 0.01231589140598780829, 0.001082316405371860912 ) ) ;
#17530 = VECTOR ( 'NONE', #57254, 1000.000000000000000 ) ;
#17531 = CARTESIAN_POINT ( 'NONE',  ( -35.00000000000000000, -5.710938531231627202, -11.39945968423477751 ) ) ;
#17532 = DIRECTION ( 'NONE',  ( -1.000000000000000000, 0.000000000000000000, 0.000000000000000000 ) ) ;
#17533 = AXIS2_PLACEMENT_3D ( 'NONE', #48996, #18411, #3453 ) ;
#17534 = ORIENTED_EDGE ( 'NONE', *, *, #36728, .T. ) ;
#17535 = VERTEX_POINT ( 'NONE', #6673 ) ;
#17536 = CARTESIAN_POINT ( 'NONE',  ( 5.514970785353741078, -0.002796696073589895887, -0.003805873180274304147 ) ) ;
#17537 = ORIENTED_EDGE ( 'NONE', *, *, #31386, .F. ) ;
#17538 = CYLINDRICAL_SURFACE ( 'NONE', #51077, 2.899999999999994582 ) ;
#17539 = DIRECTION ( 'NONE',  ( -1.000000000000000000, 0.000000000000000000, 0.000000000000000000 ) ) ;
#17540 = CARTESIAN_POINT ( 'NONE',  ( -35.00000000000000000, 0.000000000000000000, 0.000000000000000000 ) ) ;
#17541 = CARTESIAN_POINT ( 'NONE',  ( 2.253265082352432724, 1.452519439326557249, -7.498995607278123643 ) ) ;
#17542 = ORIENTED_EDGE ( 'NONE', *, *, #832, .T. ) ;
#17543 = CARTESIAN_POINT ( 'NONE',  ( 0.2648978790185584908, -6.008231198268910056, -10.67083876753498117 ) ) ;
#17544 = CARTESIAN_POINT ( 'NONE',  ( 18.31509512384567273, 9.277234456363913750, 9.833198574146647886 ) ) ;
#17545 = CARTESIAN_POINT ( 'NONE',  ( 0.2651627923886310523, -10.56116046379969653, -6.199207987242205675 ) ) ;
#17546 = CARTESIAN_POINT ( 'NONE',  ( -47.76247274761328754, -0.4463159248369971688, 10.36992351718251371 ) ) ;
#17547 = EDGE_CURVE ( 'NONE', #24896, #29925, #22773, .T. ) ;
#17548 = VECTOR ( 'NONE', #44649, 1000.000000000000114 ) ;
#17549 = CARTESIAN_POINT ( 'NONE',  ( 0.2676618633000443781, 6.262131165853879189, -10.52491907319755526 ) ) ;
#17550 = LINE ( 'NONE', #28180, #61643 ) ;
#17551 = ORIENTED_EDGE ( 'NONE', *, *, #47305, .T. ) ;
#17552 = CARTESIAN_POINT ( 'NONE',  ( -27.08426571771018487, 1.845988025802340005, -1.357728109767518454 ) ) ;
#17553 = CARTESIAN_POINT ( 'NONE',  ( 2.245754705088395031, 0.1113317465207851603, -7.635057163463313756 ) ) ;
#17554 = CARTESIAN_POINT ( 'NONE',  ( 35.00000000000000000, 4.705694406421931860E-17, -3.469127814946512892E-15 ) ) ;
#17555 = ORIENTED_EDGE ( 'NONE', *, *, #4952, .T. ) ;
#17556 = CARTESIAN_POINT ( 'NONE',  ( -11.40165637463000436, -7.508992741355388745, -9.360289953322599388 ) ) ;
#17557 = LINE ( 'NONE', #52795, #27824 ) ;
#17558 = CYLINDRICAL_SURFACE ( 'NONE', #57459, 12.75000000000000178 ) ;
#17559 =( GEOMETRIC_REPRESENTATION_CONTEXT ( 3 ) GLOBAL_UNCERTAINTY_ASSIGNED_CONTEXT ( ( #11970 ) ) GLOBAL_UNIT_ASSIGNED_CONTEXT ( ( #60747, #10512, #15507 ) ) REPRESENTATION_CONTEXT ( 'NONE', 'WORKASPACE' ) );
#17560 = CARTESIAN_POINT ( 'NONE',  ( 2.000000000000001776, 0.000000000000000000, 1.499999999999997780 ) ) ;
#17561 = CARTESIAN_POINT ( 'NONE',  ( 25.00000000000000355, -30.00000000000000000, -5.000000000000000888 ) ) ;
#17562 = ADVANCED_FACE ( 'NONE', ( #1021 ), #26607, .T. ) ;
#17563 = ORIENTED_EDGE ( 'NONE', *, *, #43993, .F. ) ;
#17564 = ORIENTED_EDGE ( 'NONE', *, *, #40213, .F. ) ;
#17565 = CARTESIAN_POINT ( 'NONE',  ( -35.00000000000000000, 0.7008968033238767159, 12.16632754454236931 ) ) ;
#17566 = ORIENTED_EDGE ( 'NONE', *, *, #63502, .F. ) ;
#17567 = DIRECTION ( 'NONE',  ( 0.000000000000000000, 0.01356324068817998940, -0.9999080150203989437 ) ) ;
#17569 = AXIS2_PLACEMENT_3D ( 'NONE', #6671, #41563, #10995 ) ;
#17568 = CARTESIAN_POINT ( 'NONE',  ( 2.705197763288546664, 7.410249563424458508, -2.399370654839196870 ) ) ;
#17570 = CARTESIAN_POINT ( 'NONE',  ( 35.00000000000000000, -6.917234959366766134, 9.493370459201765144 ) ) ;
#17571 = CARTESIAN_POINT ( 'NONE',  ( 1.459561108994223533, 3.725588117663211740, -12.08294179906978272 ) ) ;
#17572 = CARTESIAN_POINT ( 'NONE',  ( 0.4626703367447423387, -7.694993290995431501, -9.611037151103516862 ) ) ;
#17573 = EDGE_CURVE ( 'NONE', #32993, #23409, #52428, .T. ) ;
#17574 = CARTESIAN_POINT ( 'NONE',  ( 2.269879328256728002, -1.181008584586007659, 7.552124491910168658 ) ) ;
#17575 = CARTESIAN_POINT ( 'NONE',  ( 145.1370849898475797, 3.309064568108273190E-14, 0.000000000000000000 ) ) ;
#17576 = ORIENTED_EDGE ( 'NONE', *, *, #13485, .T. ) ;
#17577 = EDGE_CURVE ( 'NONE', #8147, #33520, #62986, .T. ) ;
#17578 = VERTEX_POINT ( 'NONE', #17948 ) ;
#17579 = CARTESIAN_POINT ( 'NONE',  ( 1.194176325881342704, -5.827386336992954163, 11.12159247766670767 ) ) ;
#17580 = ORIENTED_EDGE ( 'NONE', *, *, #9714, .F. ) ;
#17582 = CARTESIAN_POINT ( 'NONE',  ( 35.00000000000000000, -0.2661492558802491248, 12.18359334611896116 ) ) ;
#17581 = VECTOR ( 'NONE', #42401, 1000.000000000000000 ) ;
#17583 = CARTESIAN_POINT ( 'NONE',  ( 0.3665391374699467075, 0.2638605131388869762, -12.27992639892678106 ) ) ;
#17584 = EDGE_CURVE ( 'NONE', #57334, #23325, #40730, .T. ) ;
#17585 = CARTESIAN_POINT ( 'NONE',  ( 36.00000000000000711, 11.32068061209303345, 5.865551165830958702 ) ) ;
#17586 = ORIENTED_EDGE ( 'NONE', *, *, #56934, .T. ) ;
#17587 = CARTESIAN_POINT ( 'NONE',  ( 2.000000000000001776, -1.779948802829851129, 6.576141558201223702 ) ) ;
#17588 = DIRECTION ( 'NONE',  ( -0.9688695217174486674, 0.000000000000000000, 0.2475719085175094036 ) ) ;
#17590 = EDGE_CURVE ( 'NONE', #20923, #51040, #1999, .T. ) ;
#17589 = CARTESIAN_POINT ( 'NONE',  ( -22.30625920655495165, -3.783486345733982237, 0.2529928606556808846 ) ) ;
#17591 = ORIENTED_EDGE ( 'NONE', *, *, #35927, .T. ) ;
#17592 = ORIENTED_EDGE ( 'NONE', *, *, #29363, .T. ) ;
#17593 = LINE ( 'NONE', #33532, #26835 ) ;
#17594 = VERTEX_POINT ( 'NONE', #58526 ) ;
#17595 = VERTEX_POINT ( 'NONE', #47554 ) ;
#17596 = CARTESIAN_POINT ( 'NONE',  ( 25.00000000000000355, -9.999999999999998224, 25.00000000000000000 ) ) ;
#17597 = ORIENTED_EDGE ( 'NONE', *, *, #29566, .T. ) ;
#17599 = EDGE_CURVE ( 'NONE', #4304, #52011, #5336, .T. ) ;
#17598 = ORIENTED_EDGE ( 'NONE', *, *, #17374, .F. ) ;
#17600 = DIRECTION ( 'NONE',  ( 1.836970198721029688E-16, -1.000000000000000000, 0.000000000000000000 ) ) ;
#17601 = CARTESIAN_POINT ( 'NONE',  ( -27.01437459610461644, -13.31613970204372421, -2.220455681983950935 ) ) ;
#17602 = CIRCLE ( 'NONE', #65362, 12.75000000000000178 ) ;
#17603 = DIRECTION ( 'NONE',  ( -1.000000000000000000, 0.000000000000000000, 0.000000000000000000 ) ) ;
#17604 = CYLINDRICAL_SURFACE ( 'NONE', #57468, 5.000000000000000888 ) ;
#17605 = CARTESIAN_POINT ( 'NONE',  ( 5.514624014163232779, -0.0001700579043834244742, 0.004137701579365677534 ) ) ;
#17606 = B_SPLINE_CURVE_WITH_KNOTS ( 'NONE', 3,
 ( #47833, #13548, #13242, #33525, #64104, #58143, #28209, #28855, #22569, #8249, #54130, #38502, #3622, #8567, #23886, #38841, #49165, #12250, #44150, #64415, #2292, #32512 ),
 .UNSPECIFIED., .F., .F.,
 ( 4, 3, 3, 3, 3, 3, 3, 4 ),
 ( 0.000000000000000000, 4.447697177976191098E-05, 6.624143997791052778E-05, 8.800576886944171486E-05, 0.0001097699864780878276, 0.0001315341395364365415, 0.0001760120188223252577, 0.0001867971373174704037 ),
 .UNSPECIFIED. ) ;
#17607 = EDGE_CURVE ( 'NONE', #61407, #7317, #8298, .T. ) ;
#17608 = CARTESIAN_POINT ( 'NONE',  ( -35.00000000000000000, -10.54834585426215732, -6.102719229070786788 ) ) ;
#17609 = B_SPLINE_CURVE_WITH_KNOTS ( 'NONE', 3,
 ( #63298, #17769, #58333, #12751, #2824, #49365, #18442, #25049, #38704, #19073 ),
 .UNSPECIFIED., .F., .F.,
 ( 4, 3, 3, 4 ),
 ( 1.084202172485504241E-18, 6.607638129004478041E-05, 9.911389841680565626E-05, 0.0001667630577588619589 ),
 .UNSPECIFIED. ) ;
#17610 = VERTEX_POINT ( 'NONE', #58188 ) ;
#17611 = DIRECTION ( 'NONE',  ( 0.000000000000000000, 0.000000000000000000, 1.000000000000000000 ) ) ;
#17612 = CARTESIAN_POINT ( 'NONE',  ( -22.27722022243424149, 2.798846704197255342, -2.391991868237149710 ) ) ;
#17613 = EDGE_CURVE ( 'NONE', #17080, #55989, #2687, .T. ) ;
#17614 = LINE ( 'NONE', #12586, #61831 ) ;
#17615 = CARTESIAN_POINT ( 'NONE',  ( 29.61270049156755135, 5.476238065135014210, 10.68911382491602424 ) ) ;
#17616 = LINE ( 'NONE', #12935, #10617 ) ;
#17617 = CARTESIAN_POINT ( 'NONE',  ( 2.907497136250764225, -4.235253383576185193, -6.617189382231105199 ) ) ;
#17618 = CARTESIAN_POINT ( 'NONE',  ( 0.3654063281920759687, -11.62642356802259513, -3.951404032559384216 ) ) ;
#17619 = CARTESIAN_POINT ( 'NONE',  ( 37.00000000000000711, 5.143145423404281047, -11.66664283989682005 ) ) ;
#17620 = B_SPLINE_CURVE_WITH_KNOTS ( 'NONE', 3,
 ( #3916, #48813, #59763, #49151, #33513, #60086, #33815, #13850, #14192, #54783, #65058, #44441, #44135, #64092, #14505, #18874, #39134, #34144, #54113 ),
 .UNSPECIFIED., .F., .F.,
 ( 4, 3, 3, 3, 3, 3, 4 ),
 ( 2.168404344971008868E-19, 2.831840207499647868E-05, 4.217266859840459553E-05, 5.602024318396018118E-05, 6.290810167969207911E-05, 9.120440630945170354E-05, 0.0001153103026479764556 ),
 .UNSPECIFIED. ) ;
#17621 = ORIENTED_EDGE ( 'NONE', *, *, #48313, .T. ) ;
#17622 = CARTESIAN_POINT ( 'NONE',  ( -37.00000000000000711, 0.000000000000000000, 0.000000000000000000 ) ) ;
#17623 = AXIS2_PLACEMENT_3D ( 'NONE', #51733, #848, #61678 ) ;
#17624 = ORIENTED_EDGE ( 'NONE', *, *, #20881, .F. ) ;
#17625 = CARTESIAN_POINT ( 'NONE',  ( -35.00000000000000000, 6.950793414699794504, 10.68873102412845100 ) ) ;
#17626 = CARTESIAN_POINT ( 'NONE',  ( -18.01523681890432371, -28.74990419755712878, -8.100995087731224231 ) ) ;
#17627 = DIRECTION ( 'NONE',  ( 1.000000000000000000, 0.000000000000000000, 0.000000000000000000 ) ) ;
#17628 = CARTESIAN_POINT ( 'NONE',  ( -27.10307689719060065, -0.6678239540327197687, -2.250862122746733363 ) ) ;
#17629 = CARTESIAN_POINT ( 'NONE',  ( 2.305787727787084407, -4.792270232040854339, -5.970480882365271746 ) ) ;
#17630 = ORIENTED_EDGE ( 'NONE', *, *, #16454, .F. ) ;
#17631 = CARTESIAN_POINT ( 'NONE',  ( 1.000000000000000888, -7.493043167941588756, -0.3229614270520431152 ) ) ;
#17632 = CARTESIAN_POINT ( 'NONE',  ( 2.000000000000001776, 3.859771122243047081, 5.613913289150030295 ) ) ;
#17633 = CARTESIAN_POINT ( 'NONE',  ( -3.757056674316401779, 9.653459166343935749, 9.445297855425245359 ) ) ;
#17634 = AXIS2_PLACEMENT_3D ( 'NONE', #13087, #49013, #18079 ) ;
#17635 = EDGE_CURVE ( 'NONE', #38476, #10194, #12051, .T. ) ;
#17636 = EDGE_CURVE ( 'NONE', #55391, #26236, #42808, .T. ) ;
#17637 = CARTESIAN_POINT ( 'NONE',  ( -22.35190811654613086, -1.736165297230997995, 3.498661567522999061 ) ) ;
#17638 = ORIENTED_EDGE ( 'NONE', *, *, #15589, .F. ) ;
#17639 = CARTESIAN_POINT ( 'NONE',  ( 5.514624014163232779, -0.001921576324372477156, -0.003668383633201366227 ) ) ;
#17640 = CARTESIAN_POINT ( 'NONE',  ( 3.291290029914074378, 8.250315036047103590, -8.713914264323182834 ) ) ;
#17641 = EDGE_CURVE ( 'NONE', #37431, #40269, #43201, .T. ) ;
#17642 = EDGE_CURVE ( 'NONE', #16592, #60501, #60905, .T. ) ;
#17643 = ORIENTED_EDGE ( 'NONE', *, *, #47390, .F. ) ;
#17644 = CARTESIAN_POINT ( 'NONE',  ( 10.22196962362456851, 7.431669770566725397, -9.426540164465942340 ) ) ;
#17645 = VERTEX_POINT ( 'NONE', #17297 ) ;
#17646 = DIRECTION ( 'NONE',  ( -1.000000000000000000, 0.000000000000000000, 0.000000000000000000 ) ) ;
#17647 = FACE_OUTER_BOUND ( 'NONE', #22386, .T. ) ;
#17648 = DIRECTION ( 'NONE',  ( 1.000000000000000000, 0.000000000000000000, 0.000000000000000000 ) ) ;
#17649 = CARTESIAN_POINT ( 'NONE',  ( -35.00000000000000000, -8.624332853796127907, 9.390600770287958809 ) ) ;
#17650 = DIRECTION ( 'NONE',  ( 0.3939253465568944290, -0.1500280335741476234, -0.9068155327749437555 ) ) ;
#17651 = EDGE_LOOP ( 'NONE', ( #56307, #39256, #38667, #63382 ) ) ;
#17652 = ADVANCED_FACE ( 'NONE', ( #27582 ), #27974, .T. ) ;
#17653 = ORIENTED_EDGE ( 'NONE', *, *, #56920, .F. ) ;
#17655 = ORIENTED_EDGE ( 'NONE', *, *, #35908, .F. ) ;
#17654 = B_SPLINE_CURVE_WITH_KNOTS ( 'NONE', 3,
 ( #65075, #45447, #50134, #60416, #4588, #56082, #35128, #55439, #30164, #9212, #45787, #25497, #14518, #10204, #29497, #44793, #9876, #20842, #50780, #24516, #19550, #5229, #250, #20523 ),
 .UNSPECIFIED., .F., .F.,
 ( 4, 2, 2, 2, 2, 2, 2, 2, 2, 2, 2, 4 ),
 ( 2.168404344971008868E-19, 0.001212199945010031558, 0.001818299917515049614, 0.002424399890020067887, 0.003030499862525085943, 0.003636599835030103998, 0.004848799780040138376, 0.005454899752545154697, 0.006060999725050171018, 0.007273199670060210599, 0.008485399615070249313, 0.009697599560080288894 ),
 .UNSPECIFIED. ) ;
#17656 = CARTESIAN_POINT ( 'NONE',  ( 37.00000000000000711, 4.705694406421931860E-17, -3.469127814946512892E-15 ) ) ;
#17657 = CARTESIAN_POINT ( 'NONE',  ( 0.2646305136544072623, -1.996350543473075945, 12.08286001766534845 ) ) ;
#17658 = ORIENTED_EDGE ( 'NONE', *, *, #45255, .F. ) ;
#17659 = AXIS2_PLACEMENT_3D ( 'NONE', #48672, #23390, #43659 ) ;
#17660 = DIRECTION ( 'NONE',  ( -1.000000000000000000, 0.000000000000000000, -0.000000000000000000 ) ) ;
#17661 = CARTESIAN_POINT ( 'NONE',  ( 2.305787727787083519, -7.566723232958080914, 1.164987321564707967 ) ) ;
#17662 = ORIENTED_EDGE ( 'NONE', *, *, #14697, .F. ) ;
#17663 = VECTOR ( 'NONE', #62332, 1000.000000000000000 ) ;
#17664 = FACE_OUTER_BOUND ( 'NONE', #18001, .T. ) ;
#17666 = ADVANCED_FACE ( 'NONE', ( #59178 ), #2341, .T. ) ;
#17665 = DIRECTION ( 'NONE',  ( 0.2475719085175094591, 0.000000000000000000, -0.9688695217174487784 ) ) ;
#17667 = DIRECTION ( 'NONE',  ( 0.000000000000000000, -0.1764146379942750642, -0.9843159429275484262 ) ) ;
#17668 = ORIENTED_EDGE ( 'NONE', *, *, #45799, .F. ) ;
#17669 = EDGE_LOOP ( 'NONE', ( #29248, #11105, #29572, #43057 ) ) ;
#17670 = CARTESIAN_POINT ( 'NONE',  ( 2.258463476536644698, 2.484972401833245748, 7.224688073723612547 ) ) ;
#17671 = VERTEX_POINT ( 'NONE', #32555 ) ;
#17672 = EDGE_LOOP ( 'NONE', ( #60529, #57729, #29629, #62869 ) ) ;
#17673 = B_SPLINE_CURVE_WITH_KNOTS ( 'NONE', 3,
 ( #39059, #14754, #39726, #29414, #8478, #34712, #49709, #4157, #18494, #13776, #29106, #34067, #19784, #29729, #28762, #39386 ),
 .UNSPECIFIED., .F., .F.,
 ( 4, 3, 3, 3, 3, 4 ),
 ( 0.000000000000000000, 0.0002999043160757236797, 0.0005998071753050783408, 0.0008997092107374227935, 0.001204458948194733715, 0.001510329163474712858 ),
 .UNSPECIFIED. ) ;
#17674 = CARTESIAN_POINT ( 'NONE',  ( 2.262775599886258870, 3.697834000591639914, 6.687241191563670917 ) ) ;
#17675 = EDGE_CURVE ( 'NONE', #47279, #9626, #20564, .T. ) ;
#17676 = CYLINDRICAL_SURFACE ( 'NONE', #5457, 12.18649999999999878 ) ;
#17677 = DIRECTION ( 'NONE',  ( 1.000000000000000000, 0.000000000000000000, 0.000000000000000000 ) ) ;
#17678 = CARTESIAN_POINT ( 'NONE',  ( -22.30861784526115699, 3.671054459752226773, 0.8834205920623279251 ) ) ;
#17679 = FACE_OUTER_BOUND ( 'NONE', #48438, .T. ) ;
#17680 = CYLINDRICAL_SURFACE ( 'NONE', #9025, 4.999999999999999112 ) ;
#17681 = CARTESIAN_POINT ( 'NONE',  ( -35.00000000000000000, -10.30098186818253758, 5.644643009979033899 ) ) ;
#17682 = ORIENTED_EDGE ( 'NONE', *, *, #47728, .F. ) ;
#17683 = EDGE_CURVE ( 'NONE', #60562, #65410, #55597, .T. ) ;
#17684 = CYLINDRICAL_SURFACE ( 'NONE', #21582, 12.18650000000000055 ) ;
#17685 =( BOUNDED_SURFACE ( )  B_SPLINE_SURFACE ( 3, 1, ( 
 ( #10866, #41775 ),
 ( #1879, #62072 ),
 ( #57406, #26479 ),
 ( #57754, #2209 ) ),
 .UNSPECIFIED., .F., .F., .F. ) 
 B_SPLINE_SURFACE_WITH_KNOTS ( ( 4, 4 ),
 ( 2, 2 ),
 ( 0.000000000000000000, 1.000000000000000000 ),
 ( 0.000000000000000000, 1.000000000000000000 ),
 .UNSPECIFIED. ) 
 GEOMETRIC_REPRESENTATION_ITEM ( )  RATIONAL_B_SPLINE_SURFACE ( (
 ( 1.000000000000000000, 1.000000000000000000),
 ( 0.9856612449720755231, 0.9999558406602322425),
 ( 0.9856612449720755231, 0.9999558406602322425),
 ( 1.000000000000000000, 1.000000000000000000) ) ) 
 REPRESENTATION_ITEM ( '' )  SURFACE ( )  );
#17686 = VERTEX_POINT ( 'NONE', #63476 ) ;
#17687 = DIRECTION ( 'NONE',  ( -1.000000000000000000, 0.000000000000000000, 0.000000000000000000 ) ) ;
#17688 = CARTESIAN_POINT ( 'NONE',  ( 2.276905613632194569, 6.697548486789856703, 3.688905863353881376 ) ) ;
#17689 = EDGE_CURVE ( 'NONE', #21896, #20774, #58798, .T. ) ;
#17690 = VERTEX_POINT ( 'NONE', #32886 ) ;
#17691 = DIRECTION ( 'NONE',  ( 0.000000000000000000, 0.01356324068818000848, -0.9999080150203990547 ) ) ;
#17692 = CARTESIAN_POINT ( 'NONE',  ( 2.000000000000001776, -4.570217215903394248, 5.218059682435592705 ) ) ;
#17693 = CARTESIAN_POINT ( 'NONE',  ( 0.2648978790185619880, -9.465406350830555482, -7.769924372105300847 ) ) ;
#17694 = B_SPLINE_CURVE_WITH_KNOTS ( 'NONE', 3,
 ( #25286, #17, #55221, #28980, #39602, #60874, #20301, #4369 ),
 .UNSPECIFIED., .F., .F.,
 ( 4, 2, 2, 4 ),
 ( 0.000000000000000000, 0.002295434919525721467, 0.003443152379288585020, 0.004590869839051449006 ),
 .UNSPECIFIED. ) ;
#17695 = VERTEX_POINT ( 'NONE', #43524 ) ;
#17696 = ORIENTED_EDGE ( 'NONE', *, *, #7585, .F. ) ;
#17697 = LINE ( 'NONE', #57611, #47101 ) ;
#17698 = ORIENTED_EDGE ( 'NONE', *, *, #58178, .T. ) ;
#17699 = FACE_OUTER_BOUND ( 'NONE', #30389, .T. ) ;
#17700 = CARTESIAN_POINT ( 'NONE',  ( 5.514624014163232779, 0.002529391395135306177, 0.003278974416024616270 ) ) ;
#17701 = CARTESIAN_POINT ( 'NONE',  ( 2.034671305879538483, 11.60021725667554371, -1.331347915349341049 ) ) ;
#17702 = DIRECTION ( 'NONE',  ( 1.000000000000000000, 0.000000000000000000, 0.000000000000000000 ) ) ;
#17703 = ORIENTED_EDGE ( 'NONE', *, *, #50955, .F. ) ;
#17704 = AXIS2_PLACEMENT_3D ( 'NONE', #15368, #15027, #5746 ) ;
#17705 = FACE_OUTER_BOUND ( 'NONE', #507, .T. ) ;
#17706 = EDGE_CURVE ( 'NONE', #47952, #44565, #52902, .T. ) ;
#17707 = CIRCLE ( 'NONE', #60170, 2.899999999999994582 ) ;
#17708 = EDGE_CURVE ( 'NONE', #817, #3673, #25953, .T. ) ;
#17709 = CARTESIAN_POINT ( 'NONE',  ( 17.75832895199376793, -29.67262258703657807, -8.626345146652873552 ) ) ;
#17710 = CARTESIAN_POINT ( 'NONE',  ( -28.41827485489077532, 3.509237424706437292, 11.47541949982830722 ) ) ;
#17711 = DIRECTION ( 'NONE',  ( 0.000000000000000000, -0.8276889981568840149, -0.5611870653623919347 ) ) ;
#17712 = CARTESIAN_POINT ( 'NONE',  ( 2.000000000000001776, 0.000000000000000000, 0.000000000000000000 ) ) ;
#17713 = DIRECTION ( 'NONE',  ( 0.000000000000000000, 0.000000000000000000, 1.000000000000000000 ) ) ;
#17714 = CARTESIAN_POINT ( 'NONE',  ( -22.27756824490284160, -2.599719761044739119, -2.608445836294064346 ) ) ;
#17715 = EDGE_CURVE ( 'NONE', #8013, #54679, #64080, .T. ) ;
#17716 = ORIENTED_EDGE ( 'NONE', *, *, #64580, .F. ) ;
#17717 = CARTESIAN_POINT ( 'NONE',  ( 2.268878695253352618, -0.1481365927654071657, 7.642144312464380640 ) ) ;
#17718 = ORIENTED_EDGE ( 'NONE', *, *, #3001, .F. ) ;
#17719 = DIRECTION ( 'NONE',  ( -1.000000000000000000, 0.000000000000000000, 0.000000000000000000 ) ) ;
#17720 = DIRECTION ( 'NONE',  ( -1.000000000000000000, 0.000000000000000000, 0.000000000000000000 ) ) ;
#17721 = DIRECTION ( 'NONE',  ( -1.000000000000000000, 0.000000000000000000, 0.000000000000000000 ) ) ;
#17722 = ORIENTED_EDGE ( 'NONE', *, *, #60671, .F. ) ;
#17723 = UNCERTAINTY_MEASURE_WITH_UNIT (LENGTH_MEASURE( 1.000000000000000082E-05 ), #56197, 'distance_accuracy_value', 'NONE');
#17724 = CARTESIAN_POINT ( 'NONE',  ( -37.00000000000000711, 6.657191900728318679, 9.677500615117924809 ) ) ;
#17725 = EDGE_LOOP ( 'NONE', ( #11455, #51832, #8806, #14252 ) ) ;
#17726 = EDGE_CURVE ( 'NONE', #30167, #4485, #48159, .T. ) ;
#17727 = LINE ( 'NONE', #37984, #57219 ) ;
#17728 = ORIENTED_EDGE ( 'NONE', *, *, #56882, .F. ) ;
#17729 = VERTEX_POINT ( 'NONE', #35174 ) ;
#17730 = CARTESIAN_POINT ( 'NONE',  ( -35.00000000000000000, -10.25474254703948418, -6.584150480049660636 ) ) ;
#17731 = ADVANCED_FACE ( 'NONE', ( #55480 ), #34536, .T. ) ;
#17732 = CARTESIAN_POINT ( 'NONE',  ( -22.35190811654612375, 0.2457675311905117566, 3.898012445334706921 ) ) ;
#17733 = B_SPLINE_CURVE_WITH_KNOTS ( 'NONE', 3,
 ( #47302, #1741, #40653, #33629, #13342, #12667, #3060, #37293, #8046, #32949, #23003, #22680, #43260, #37636, #53260, #2747, #28312, #7356, #43585, #42945, #27993, #18009 ),
 .UNSPECIFIED., .F., .F.,
 ( 4, 3, 3, 3, 3, 3, 3, 4 ),
 ( 1.755771606739170543E-18, 4.449119708436529840E-05, 6.626296329539953971E-05, 8.803456484962175158E-05, 0.0001098060367612756628, 0.0001315774408628470331, 0.0001760698110411152600, 0.0001829697163287826703 ),
 .UNSPECIFIED. ) ;
#17734 = ORIENTED_EDGE ( 'NONE', *, *, #33399, .F. ) ;
#17735 = DIRECTION ( 'NONE',  ( -1.000000000000000000, 0.000000000000000000, -0.000000000000000000 ) ) ;
#17736 = CARTESIAN_POINT ( 'NONE',  ( -35.00000000000000000, 0.000000000000000000, 0.000000000000000000 ) ) ;
#17737 = CYLINDRICAL_SURFACE ( 'NONE', #8937, 2.899999999999994582 ) ;
#17738 = CARTESIAN_POINT ( 'NONE',  ( -14.47334165536099881, 4.898587196589412829E-16, -4.000000000000000000 ) ) ;
#17739 = EDGE_LOOP ( 'NONE', ( #54341, #974, #62245, #31885 ) ) ;
#17740 = DIRECTION ( 'NONE',  ( 0.000000000000000000, -0.01356324068817992175, 0.9999080150203990547 ) ) ;
#17741 = DIRECTION ( 'NONE',  ( 0.000000000000000000, 0.01356324068817999808, -0.9999080150203990547 ) ) ;
#17742 = CARTESIAN_POINT ( 'NONE',  ( 5.520433897694421610, -0.01186170453199867497, -0.009283255140285580700 ) ) ;
#17743 = ORIENTED_EDGE ( 'NONE', *, *, #42753, .F. ) ;
#17744 = CYLINDRICAL_SURFACE ( 'NONE', #61761, 5.000000000000000888 ) ;
#17745 = ORIENTED_EDGE ( 'NONE', *, *, #58602, .T. ) ;
#17746 = DIRECTION ( 'NONE',  ( 0.000000000000000000, -0.5155538571770110767, -0.8568571761675957132 ) ) ;
#17747 = ORIENTED_EDGE ( 'NONE', *, *, #30700, .T. ) ;
#17748 = AXIS2_PLACEMENT_3D ( 'NONE', #20692, #737, #41278 ) ;
#17749 = LINE ( 'NONE', #53327, #51828 ) ;
#17750 = FACE_OUTER_BOUND ( 'NONE', #28747, .T. ) ;
#17751 = EDGE_CURVE ( 'NONE', #53297, #46246, #6756, .T. ) ;
#17752 = CARTESIAN_POINT ( 'NONE',  ( -35.00000000000000000, 5.246972444134173408, -10.99909370905151995 ) ) ;
#17753 = CARTESIAN_POINT ( 'NONE',  ( -35.00000000000000000, -9.063649021439015740, 8.146229107149364879 ) ) ;
#17754 = CARTESIAN_POINT ( 'NONE',  ( 0.2739690278137235091, 9.499928778897116288, 7.732471127692628343 ) ) ;
#17755 = CARTESIAN_POINT ( 'NONE',  ( 1.948354844646963180, -11.88693049004113611, -1.364409644999339255 ) ) ;
#17756 = CARTESIAN_POINT ( 'NONE',  ( 13.22184092363782604, 12.92131670040196134, -3.916134364945811352 ) ) ;
#17757 = EDGE_LOOP ( 'NONE', ( #44383, #13870, #29298, #44948 ) ) ;
#17758 = EDGE_CURVE ( 'NONE', #34549, #939, #44193, .T. ) ;
#17759 = ORIENTED_EDGE ( 'NONE', *, *, #2091, .F. ) ;
#17760 = CARTESIAN_POINT ( 'NONE',  ( 35.00000000000000000, 4.705694406421931860E-17, -3.469127814946512892E-15 ) ) ;
#17761 = ORIENTED_EDGE ( 'NONE', *, *, #1083, .T. ) ;
#17762 = EDGE_CURVE ( 'NONE', #9839, #52648, #64461, .T. ) ;
#17763 = EDGE_LOOP ( 'NONE', ( #21811, #26910, #49634, #57538 ) ) ;
#17764 = CARTESIAN_POINT ( 'NONE',  ( -37.00000000000000711, 0.000000000000000000, 0.000000000000000000 ) ) ;
#17765 = CARTESIAN_POINT ( 'NONE',  ( -22.28023996335807411, 3.345627887484369900, 1.558279384310053306 ) ) ;
#17766 = CARTESIAN_POINT ( 'NONE',  ( 5.536195898058073439, -0.008323005098840522212, -0.001726268814999801574 ) ) ;
#17767 = CARTESIAN_POINT ( 'NONE',  ( 0.3474126878361749604, -10.49748369253935998, 6.359473273659659753 ) ) ;
#17768 = DIRECTION ( 'NONE',  ( -0.000000000000000000, -1.000000000000000000, -0.000000000000000000 ) ) ;
#17769 = CARTESIAN_POINT ( 'NONE',  ( 2.241449424704146764, -7.528892370271783818, -1.265244293929165709 ) ) ;
#17770 = CARTESIAN_POINT ( 'NONE',  ( 47.00000000000000711, 4.705694406421931860E-17, -3.469127814946512892E-15 ) ) ;
#17771 = ORIENTED_EDGE ( 'NONE', *, *, #42094, .T. ) ;
#17772 = CARTESIAN_POINT ( 'NONE',  ( 2.276198483117261251, -5.756970692722241267, -5.031786924855536469 ) ) ;
#17773 = CARTESIAN_POINT ( 'NONE',  ( -17.14223920962179548, -7.219260785924160650, 11.41241003048411429 ) ) ;
#17774 = CARTESIAN_POINT ( 'NONE',  ( 35.00000000000000000, 4.705694406421931860E-17, -3.469127814946512892E-15 ) ) ;
#17775 = CARTESIAN_POINT ( 'NONE',  ( -35.00000000000000000, -5.644643009978993931, -10.30098186818255890 ) ) ;
#17776 = EDGE_CURVE ( 'NONE', #6781, #11746, #30094, .T. ) ;
#17777 = CARTESIAN_POINT ( 'NONE',  ( 2.000000000000001776, 0.4129979343798200753, -6.800241778083709221 ) ) ;
#17778 = CARTESIAN_POINT ( 'NONE',  ( -22.31328051695926007, -0.2528478350593797996, -3.781397440874599614 ) ) ;
#17779 = ORIENTED_EDGE ( 'NONE', *, *, #34446, .T. ) ;
#17780 = CARTESIAN_POINT ( 'NONE',  ( 37.00000000000000711, 4.705694406421931860E-17, -3.469127814946512892E-15 ) ) ;
#17781 = LINE ( 'NONE', #52050, #26112 ) ;
#17782 = CARTESIAN_POINT ( 'NONE',  ( -22.27384469013076185, -0.9224151068931482067, -3.564715702084495952 ) ) ;
#17783 = DIRECTION ( 'NONE',  ( 1.000000000000000000, 0.000000000000000000, 0.000000000000000000 ) ) ;
#17784 = AXIS2_PLACEMENT_3D ( 'NONE', #12573, #48202, #26913 ) ;
#17785 = CIRCLE ( 'NONE', #58142, 12.18650000000000233 ) ;
#17786 = B_SPLINE_CURVE_WITH_KNOTS ( 'NONE', 3,
 ( #57414, #57094, #37784, #47124, #11519, #31790, #1577, #27465, #21850, #53076 ),
 .UNSPECIFIED., .F., .F.,
 ( 4, 3, 3, 4 ),
 ( 1.301042606982605321E-18, 6.607638129004456357E-05, 9.911389841680489732E-05, 0.0001667630577588619318 ),
 .UNSPECIFIED. ) ;
#17787 = CARTESIAN_POINT ( 'NONE',  ( 0.000000000000000000, 0.000000000000000000, 0.000000000000000000 ) ) ;
#17788 = CARTESIAN_POINT ( 'NONE',  ( 35.00000000000000000, -12.57916205664482590, -2.080187960898520316 ) ) ;
#17789 = EDGE_LOOP ( 'NONE', ( #34487, #47670, #35636, #35688 ) ) ;
#17790 = CARTESIAN_POINT ( 'NONE',  ( -25.86628395826706850, 25.00000000000000000, 10.84354029019568522 ) ) ;
#17791 = CARTESIAN_POINT ( 'NONE',  ( 35.00000000000000000, 12.74921544981110877, -0.1414404973752607098 ) ) ;
#17792 = CARTESIAN_POINT ( 'NONE',  ( 2.305787727787084407, -4.792270232040854339, -5.970480882365271746 ) ) ;
#17793 = ORIENTED_EDGE ( 'NONE', *, *, #1398, .T. ) ;
#17794 = CARTESIAN_POINT ( 'NONE',  ( 0.3474126878361818438, 2.385599230262039239, 12.03947592323247306 ) ) ;
#17795 = CARTESIAN_POINT ( 'NONE',  ( 1.452237505248552996, 12.08199618361518013, -3.767214359061005435 ) ) ;
#17796 = ORIENTED_EDGE ( 'NONE', *, *, #48916, .F. ) ;
#17797 = EDGE_CURVE ( 'NONE', #886, #24291, #3969, .T. ) ;
#17798 = ORIENTED_EDGE ( 'NONE', *, *, #22087, .F. ) ;
#17799 = DIRECTION ( 'NONE',  ( 1.000000000000000000, 0.000000000000000000, 0.000000000000000000 ) ) ;
#17800 = ADVANCED_FACE ( 'NONE', ( #9253 ), #29535, .T. ) ;
#17801 = DIRECTION ( 'NONE',  ( 1.000000000000000000, 1.836970198721029688E-16, 0.000000000000000000 ) ) ;
#17802 = ORIENTED_EDGE ( 'NONE', *, *, #57090, .T. ) ;
#17803 = DIRECTION ( 'NONE',  ( 1.000000000000000000, 0.000000000000000000, 0.000000000000000000 ) ) ;
#17804 = DIRECTION ( 'NONE',  ( -1.000000000000000000, 0.000000000000000000, 0.000000000000000000 ) ) ;
#17805 = DIRECTION ( 'NONE',  ( -1.000000000000000000, 0.000000000000000000, 0.000000000000000000 ) ) ;
#17806 = CARTESIAN_POINT ( 'NONE',  ( 2.269879328256731554, -7.552124491910167770, -1.181008584586032306 ) ) ;
#17807 = CARTESIAN_POINT ( 'NONE',  ( -27.01437459610461644, 8.723448335974111956, -8.240233560378637634 ) ) ;
#17808 = DIRECTION ( 'NONE',  ( 0.000000000000000000, 0.000000000000000000, 1.000000000000000000 ) ) ;
#17810 = VERTEX_POINT ( 'NONE', #41148 ) ;
#17809 = CARTESIAN_POINT ( 'NONE',  ( -2.672254813960866393, 12.91372982010633841, 3.936302266217769130 ) ) ;
#17811 = CARTESIAN_POINT ( 'NONE',  ( 2.000000000000001776, 5.814643797626986910, -3.550179297009520063 ) ) ;
#17812 = ORIENTED_EDGE ( 'NONE', *, *, #22635, .F. ) ;
#17813 = CARTESIAN_POINT ( 'NONE',  ( -22.70624764888619751, -5.249808673991985586, -0.08990180771019026795 ) ) ;
#17814 = ORIENTED_EDGE ( 'NONE', *, *, #25069, .T. ) ;
#17815 = EDGE_LOOP ( 'NONE', ( #62563, #26879, #33484, #51560 ) ) ;
#17816 = CARTESIAN_POINT ( 'NONE',  ( -16.44683101004208581, 8.250250954730093511, 10.68587204513299582 ) ) ;
#17817 = CARTESIAN_POINT ( 'NONE',  ( -22.27718112499583469, 3.645895996548659035, -0.5110808820053269752 ) ) ;
#17818 = EDGE_CURVE ( 'NONE', #3364, #29286, #34627, .T. ) ;
#17819 = VECTOR ( 'NONE', #56513, 1000.000000000000000 ) ;
#17820 = CARTESIAN_POINT ( 'NONE',  ( -24.45674484725088149, 9.483701336929913239, 9.615580680626223398 ) ) ;
#17821 = CARTESIAN_POINT ( 'NONE',  ( -44.06649112733600759, -1.138262461040779439, -14.66001971352459243 ) ) ;
#17822 = CARTESIAN_POINT ( 'NONE',  ( 22.88594695219327235, 3.421158645304719137, 13.05931366970166962 ) ) ;
#17823 = EDGE_LOOP ( 'NONE', ( #54533, #15593, #46916, #22882 ) ) ;
#17824 = CARTESIAN_POINT ( 'NONE',  ( -25.60701309404801052, -10.48086169146383106, 5.846161800792287977 ) ) ;
#17825 = CARTESIAN_POINT ( 'NONE',  ( 1.019420486327238695, 0.09895457231945321841, -13.50926513763734960 ) ) ;
#17827 = VERTEX_POINT ( 'NONE', #35818 ) ;
#17826 = CARTESIAN_POINT ( 'NONE',  ( 0.2833330754217401881, 11.58086621621913359, -3.999965385632473946 ) ) ;
#17828 = ORIENTED_EDGE ( 'NONE', *, *, #35028, .F. ) ;
#17829 = CARTESIAN_POINT ( 'NONE',  ( 5.536195898058073439, -0.008496323383586770056, 0.0002547682446684717324 ) ) ;
#17830 = ORIENTED_EDGE ( 'NONE', *, *, #2199, .T. ) ;
#17831 = FACE_OUTER_BOUND ( 'NONE', #57690, .T. ) ;
#17832 = CIRCLE ( 'NONE', #16727, 4.999999999999999112 ) ;
#17833 = CARTESIAN_POINT ( 'NONE',  ( 0.2956976708475410054, -10.50256636126823473, -6.317697191869750206 ) ) ;
#17834 = DIRECTION ( 'NONE',  ( 0.000000000000000000, 0.01356324068817998593, -0.9999080150203990547 ) ) ;
#17835 = LINE ( 'NONE', #7871, #2947 ) ;
#17836 = ADVANCED_FACE ( 'NONE', ( #61769 ), #56817, .T. ) ;
#17837 = CARTESIAN_POINT ( 'NONE',  ( -37.25000000000002132, -27.56175630915211272, -1.528111002209142422 ) ) ;
#17838 = DIRECTION ( 'NONE',  ( 1.000000000000000000, 0.000000000000000000, -0.000000000000000000 ) ) ;
#17839 = AXIS2_PLACEMENT_3D ( 'NONE', #54186, #53204, #63486 ) ;
#17840 = CARTESIAN_POINT ( 'NONE',  ( -7.389643752995853632, -8.206056478905798812, -10.72177447465197275 ) ) ;
#17841 = ORIENTED_EDGE ( 'NONE', *, *, #22989, .T. ) ;
#17842 = DIRECTION ( 'NONE',  ( -1.000000000000000000, 0.000000000000000000, 0.000000000000000000 ) ) ;
#17843 = EDGE_LOOP ( 'NONE', ( #3741, #40603, #26148, #53632 ) ) ;
#17844 = CARTESIAN_POINT ( 'NONE',  ( -9.248427021356883770, -11.50593189300519725, -7.070361659645593377 ) ) ;
#17845 = DIRECTION ( 'NONE',  ( -0.000000000000000000, -1.000000000000000000, -0.000000000000000000 ) ) ;
#17846 = B_SPLINE_CURVE_WITH_KNOTS ( 'NONE', 3,
 ( #22261, #32240, #21281, #51890, #47238, #1685, #47875, #21633, #36587, #56890, #37573, #42525, #21951, #37220, #32549, #41558, #17628, #61849, #26601 ),
 .UNSPECIFIED., .F., .F.,
 ( 4, 3, 3, 3, 3, 3, 4 ),
 ( 0.000000000000000000, 2.832085443540606438E-05, 4.217789847394578227E-05, 5.603488375045981523E-05, 6.989180858579043150E-05, 9.821094829918522679E-05, 0.0001178165571465082212 ),
 .UNSPECIFIED. ) ;
#17847 = CARTESIAN_POINT ( 'NONE',  ( -10.48620311856347875, -9.720786832536937538, 7.036071585506805448 ) ) ;
#17848 = ORIENTED_EDGE ( 'NONE', *, *, #62711, .T. ) ;
#17849 = ORIENTED_EDGE ( 'NONE', *, *, #28974, .F. ) ;
#17850 = DIRECTION ( 'NONE',  ( 0.000000000000000000, -0.01356324068817998940, 0.9999080150203990547 ) ) ;
#17851 = EDGE_CURVE ( 'NONE', #40103, #6736, #54514, .T. ) ;
#17852 = ORIENTED_EDGE ( 'NONE', *, *, #62517, .T. ) ;
#17853 = CARTESIAN_POINT ( 'NONE',  ( 0.3109076770649009669, 7.699281309344454982, -9.542672295796739590 ) ) ;
#17854 = CARTESIAN_POINT ( 'NONE',  ( -25.00000000000000355, -28.99999999999999645, 5.000000000000000888 ) ) ;
#17855 = CARTESIAN_POINT ( 'NONE',  ( 2.280717697723836146, 1.481796453660317425, 7.502592193582054314 ) ) ;
#17856 = EDGE_CURVE ( 'NONE', #17595, #31528, #11238, .T. ) ;
#17857 = CARTESIAN_POINT ( 'NONE',  ( 0.000000000000000000, 6.812627895098307462, -0.04423456934727655609 ) ) ;
#17858 = ORIENTED_EDGE ( 'NONE', *, *, #30703, .F. ) ;
#17859 = CARTESIAN_POINT ( 'NONE',  ( 0.2958664285830424623, 12.10650684287254286, 1.910785783655619241 ) ) ;
#17860 = CARTESIAN_POINT ( 'NONE',  ( -22.28073302975500880, -2.595086548180001174, 2.626377654649335813 ) ) ;
#17861 = CARTESIAN_POINT ( 'NONE',  ( -29.11945779004042478, 1.962419008656826502, -13.36268013567996604 ) ) ;
#17862 = CARTESIAN_POINT ( 'NONE',  ( 2.000000000000001776, -4.376687952327290354, -5.220963330856675633 ) ) ;
#17863 = AXIS2_PLACEMENT_3D ( 'NONE', #43842, #64432, #8920 ) ;
#17864 = EDGE_CURVE ( 'NONE', #32570, #38861, #47389, .T. ) ;
#17865 = CARTESIAN_POINT ( 'NONE',  ( 3.152665057735843490, -3.546019893114926713, 7.102135024646879735 ) ) ;
#17866 = CARTESIAN_POINT ( 'NONE',  ( 2.000000000000001776, 6.441884263200815752, 2.217201541069855786 ) ) ;
#17867 = CIRCLE ( 'NONE', #15761, 5.000000000000001776 ) ;
#17868 =( BOUNDED_CURVE ( )  B_SPLINE_CURVE ( 3, ( #45811, #40827, #10225, #40481 ),
 .UNSPECIFIED., .F., .F. ) 
 B_SPLINE_CURVE_WITH_KNOTS ( ( 4, 4 ),
 ( 4.993910677237380469, 5.028906353039236166 ),
 .UNSPECIFIED. ) 
 CURVE ( )  GEOMETRIC_REPRESENTATION_ITEM ( )  RATIONAL_B_SPLINE_CURVE ( ( 1.000000000000000000, 0.9998979444935354177, 0.9998979444935354177, 1.000000000000000000 ) ) 
 REPRESENTATION_ITEM ( '' )  );
#17869 = EDGE_LOOP ( 'NONE', ( #14869, #62201, #57968, #13094 ) ) ;
#17870 = B_SPLINE_CURVE_WITH_KNOTS ( 'NONE', 3,
 ( #9859, #50449, #14502, #35109, #55421, #34477, #50762, #19531, #54778, #46116, #55084, #4895, #563, #41092, #9513, #61371, #40105, #39796, #5556 ),
 .UNSPECIFIED., .F., .F.,
 ( 4, 3, 3, 3, 3, 3, 4 ),
 ( 0.000000000000000000, 2.836829843012687999E-05, 4.224792512550939246E-05, 5.612066614913134463E-05, 6.998859278354717817E-05, 9.832141288087045293E-05, 0.0001178161482478527668 ),
 .UNSPECIFIED. ) ;
#17871 = CARTESIAN_POINT ( 'NONE',  ( -22.27834755396593991, -3.610802913011853743, 0.7418417409069075763 ) ) ;
#17872 = DIRECTION ( 'NONE',  ( 1.000000000000000000, 0.000000000000000000, 0.000000000000000000 ) ) ;
#17873 = CARTESIAN_POINT ( 'NONE',  ( -36.00000000000000711, -4.074242145635922796, -12.08151691381194581 ) ) ;
#17874 = ORIENTED_EDGE ( 'NONE', *, *, #50463, .F. ) ;
#17875 = AXIS2_PLACEMENT_3D ( 'NONE', #19063, #38016, #23394 ) ;
#17876 = CARTESIAN_POINT ( 'NONE',  ( -11.31210385045561573, -8.611009510439803449, -8.362799969824267876 ) ) ;
#17877 = DIRECTION ( 'NONE',  ( 0.000000000000000000, -0.01356324068817991828, 0.9999080150203990547 ) ) ;
#17878 = DIRECTION ( 'NONE',  ( -1.000000000000000000, 0.000000000000000000, 0.000000000000000000 ) ) ;
#17879 = EDGE_CURVE ( 'NONE', #58222, #40199, #22661, .T. ) ;
#17880 = AXIS2_PLACEMENT_3D ( 'NONE', #41957, #16692, #12587 ) ;
#17881 = CARTESIAN_POINT ( 'NONE',  ( -30.04210686634944949, 0.3871513321129805840, -13.50186640917502245 ) ) ;
#17882 = CARTESIAN_POINT ( 'NONE',  ( 0.2834382757447999057, -11.44241760114838691, 4.380429851625286197 ) ) ;
#17883 = ORIENTED_EDGE ( 'NONE', *, *, #9179, .F. ) ;
#17884 = FACE_BOUND ( 'NONE', #25397, .T. ) ;
#17885 = ORIENTED_EDGE ( 'NONE', *, *, #60127, .F. ) ;
#17886 = CARTESIAN_POINT ( 'NONE',  ( -36.00000000000000711, 5.143145423404448913, -11.66664283989674367 ) ) ;
#17887 = CARTESIAN_POINT ( 'NONE',  ( 0.2801149460245153100, -9.509848747524133117, -7.723514566794077219 ) ) ;
#17888 = DIRECTION ( 'NONE',  ( 0.000000000000000000, 0.000000000000000000, 1.000000000000000000 ) ) ;
#17889 = PLANE ( 'NONE',  #30122 ) ;
#17890 = DIRECTION ( 'NONE',  ( 0.000000000000000000, -0.6478160128811839558, 0.7617968321374970486 ) ) ;
#17891 = CARTESIAN_POINT ( 'NONE',  ( 2.260457164927185847, 7.547495527593559572, 1.190240296002696541 ) ) ;
#17892 = DIRECTION ( 'NONE',  ( -1.000000000000000000, 0.000000000000000000, 0.000000000000000000 ) ) ;
#17893 = VERTEX_POINT ( 'NONE', #15236 ) ;
#17894 = ORIENTED_EDGE ( 'NONE', *, *, #5555, .T. ) ;
#17895 = CARTESIAN_POINT ( 'NONE',  ( -27.15525204139121840, 0.7327319213109966256, 2.394850816831278539 ) ) ;
#17896 = EDGE_LOOP ( 'NONE', ( #60333, #11605, #55667, #22310 ) ) ;
#17897 = SHAPE_REPRESENTATION_RELATIONSHIP ( 'NONE' , 'NONE' ,  #45039, #65033 ) ;
#17898 = CARTESIAN_POINT ( 'NONE',  ( -22.28169757117799321, 2.592369810060400237, -2.633129923220806745 ) ) ;
#17899 = CARTESIAN_POINT ( 'NONE',  ( 0.4626703367449477300, 8.128802338754596235, -9.247028139127518642 ) ) ;
#17900 = AXIS2_PLACEMENT_3D ( 'NONE', #28894, #64768, #28245 ) ;
#17901 = DIRECTION ( 'NONE',  ( 1.000000000000000000, 0.000000000000000000, 0.000000000000000000 ) ) ;
#17902 = ORIENTED_EDGE ( 'NONE', *, *, #22107, .F. ) ;
#17903 = CARTESIAN_POINT ( 'NONE',  ( 0.3006302518452036443, 5.932248915294314529, -10.72687985734936333 ) ) ;
#17904 = CARTESIAN_POINT ( 'NONE',  ( 3.100650473569749543, 1.818095316078704560, -7.709402782713593361 ) ) ;
#17905 = CIRCLE ( 'NONE', #55053, 5.000000000000000888 ) ;
#17906 = CARTESIAN_POINT ( 'NONE',  ( 2.994568964204212591, -1.761139509856882945, 7.686291764591503650 ) ) ;
#17907 = ORIENTED_EDGE ( 'NONE', *, *, #36135, .F. ) ;
#17908 = ORIENTED_EDGE ( 'NONE', *, *, #54073, .F. ) ;
#17909 = DIRECTION ( 'NONE',  ( 1.000000000000000000, -0.000000000000000000, -0.000000000000000000 ) ) ;
#17910 = ORIENTED_EDGE ( 'NONE', *, *, #38374, .F. ) ;
#17911 = CARTESIAN_POINT ( 'NONE',  ( -35.00000000000000000, -11.37311665002361494, -2.936739658819992549 ) ) ;
#17912 = ORIENTED_EDGE ( 'NONE', *, *, #60809, .T. ) ;
#17913 = VERTEX_POINT ( 'NONE', #36830 ) ;
#17914 = CARTESIAN_POINT ( 'NONE',  ( -22.27719412087655471, -2.887588494201215994, 2.283949229175420204 ) ) ;
#17916 = AXIS2_PLACEMENT_3D ( 'NONE', #13180, #43761, #36999 ) ;
#17915 = CARTESIAN_POINT ( 'NONE',  ( -27.08485414902845179, -1.620258667553439169, 1.622802444813708167 ) ) ;
#17917 = EDGE_CURVE ( 'NONE', #14308, #49252, #55816, .T. ) ;
#17918 = DIRECTION ( 'NONE',  ( 0.000000000000000000, 0.000000000000000000, 1.000000000000000000 ) ) ;
#17919 = CARTESIAN_POINT ( 'NONE',  ( 0.2956976708475479443, 8.045468685197048941, -9.245952174682468439 ) ) ;
#17920 = DIRECTION ( 'NONE',  ( 0.000000000000000000, 0.000000000000000000, 1.000000000000000000 ) ) ;
#17921 = CARTESIAN_POINT ( 'NONE',  ( 0.3164563675027571854, 11.60369811966062770, 3.967501530099125873 ) ) ;
#17922 = VECTOR ( 'NONE', #13781, 1000.000000000000000 ) ;
#17923 = ORIENTED_EDGE ( 'NONE', *, *, #40778, .F. ) ;
#17924 = CARTESIAN_POINT ( 'NONE',  ( -22.23402523511428086, 1.734723475976807094E-15, -8.673617379884035472E-15 ) ) ;
#17925 = CARTESIAN_POINT ( 'NONE',  ( -35.00000000000000000, -11.23004253107761130, -4.732539170486383284 ) ) ;
#17926 = CIRCLE ( 'NONE', #55073, 6.936499999999989008 ) ;
#17927 = DIRECTION ( 'NONE',  ( -1.000000000000000000, -0.000000000000000000, 0.000000000000000000 ) ) ;
#17928 = CARTESIAN_POINT ( 'NONE',  ( -35.04709527796842394, -0.01231589140598780829, -0.001082316405380534530 ) ) ;
#17929 = DIRECTION ( 'NONE',  ( 0.000000000000000000, 0.8515178078024850938, -0.5243256840888592674 ) ) ;
#17930 = CARTESIAN_POINT ( 'NONE',  ( 35.00000000000000000, 3.213188559034240832, -11.29812557209478285 ) ) ;
#17931 = CARTESIAN_POINT ( 'NONE',  ( -27.08416781016246588, 1.485424708116796166, 1.744495588874922509 ) ) ;
#17932 = LINE ( 'NONE', #8278, #23868 ) ;
#17933 = CARTESIAN_POINT ( 'NONE',  ( 0.000000000000000000, 0.000000000000000000, 0.000000000000000000 ) ) ;
#17934 = EDGE_CURVE ( 'NONE', #14755, #14116, #19478, .T. ) ;
#17935 = ORIENTED_EDGE ( 'NONE', *, *, #1671, .T. ) ;
#17936 = CARTESIAN_POINT ( 'NONE',  ( 2.000000000000001776, -1.779948802829851129, 6.576141558201223702 ) ) ;
#17937 = ORIENTED_EDGE ( 'NONE', *, *, #58173, .F. ) ;
#17938 = EDGE_CURVE ( 'NONE', #28876, #6075, #10242, .T. ) ;
#17939 = LINE ( 'NONE', #33227, #28518 ) ;
#17940 = CARTESIAN_POINT ( 'NONE',  ( -35.00000000000000000, -4.603882218679629545, 10.80631716521665453 ) ) ;
#17941 = CARTESIAN_POINT ( 'NONE',  ( 35.00000000000000000, 4.705694406421931860E-17, -3.469127814946512892E-15 ) ) ;
#17942 = CARTESIAN_POINT ( 'NONE',  ( -25.86628395826706850, -8.041618865309574815, 10.84354029019568522 ) ) ;
#17943 = EDGE_CURVE ( 'NONE', #11296, #64733, #46546, .T. ) ;
#17944 = CARTESIAN_POINT ( 'NONE',  ( 2.556980015512939186, 7.658710847181238179, 1.116161541731872653 ) ) ;
#17945 = ORIENTED_EDGE ( 'NONE', *, *, #44501, .F. ) ;
#17946 = FACE_OUTER_BOUND ( 'NONE', #56994, .T. ) ;
#17947 = DIRECTION ( 'NONE',  ( -1.000000000000000000, 0.000000000000000000, -0.000000000000000000 ) ) ;
#17948 = CARTESIAN_POINT ( 'NONE',  ( 35.00000000000000000, 4.426194442447407340, 11.35427606708800852 ) ) ;
#17949 = CARTESIAN_POINT ( 'NONE',  ( 0.2653519991613831897, -2.104847849998778830, -12.06397323649778031 ) ) ;
#17950 = EDGE_CURVE ( 'NONE', #37639, #26820, #15233, .T. ) ;
#17951 = CARTESIAN_POINT ( 'NONE',  ( -37.00000000000000711, 11.59095880812008161, -1.903127969211228621 ) ) ;
#17952 = ORIENTED_EDGE ( 'NONE', *, *, #40335, .T. ) ;
#17953 = VECTOR ( 'NONE', #46066, 1000.000000000000000 ) ;
#17954 = EDGE_CURVE ( 'NONE', #29381, #37749, #58449, .T. ) ;
#17955 = CARTESIAN_POINT ( 'NONE',  ( 2.524535260911985102, -0.2211075636758263463, -7.725637239510234622 ) ) ;
#17956 = CARTESIAN_POINT ( 'NONE',  ( -22.27384469013076185, -1.508555848190757276, 3.358914544760229326 ) ) ;
#17957 = CARTESIAN_POINT ( 'NONE',  ( 2.288423627607477862, -3.963881558061918664, -6.543055113184263583 ) ) ;
#17958 = AXIS2_PLACEMENT_3D ( 'NONE', #52368, #47376, #30735 ) ;
#17959 = AXIS2_PLACEMENT_3D ( 'NONE', #51175, #5628, #56474 ) ;
#17960 = VERTEX_POINT ( 'NONE', #37485 ) ;
#17962 = EDGE_CURVE ( 'NONE', #35534, #24646, #28293, .T. ) ;
#17961 = CARTESIAN_POINT ( 'NONE',  ( -27.08485414902839494, 2.214586389210143391, -0.5952588087544573581 ) ) ;
#17963 = AXIS2_PLACEMENT_3D ( 'NONE', #65445, #4642, #19908 ) ;
#17964 = VERTEX_POINT ( 'NONE', #43439 ) ;
#17965 = CARTESIAN_POINT ( 'NONE',  ( -10.00000000000000178, 0.000000000000000000, 0.000000000000000000 ) ) ;
#17966 = DIRECTION ( 'NONE',  ( 1.000000000000000000, 0.000000000000000000, 0.000000000000000000 ) ) ;
#17967 = DIRECTION ( 'NONE',  ( 1.000000000000000000, -0.000000000000000000, 0.000000000000000000 ) ) ;
#17968 = CARTESIAN_POINT ( 'NONE',  ( 35.00000000000000000, 4.705694406421931860E-17, -3.469127814946512892E-15 ) ) ;
#17969 = ADVANCED_FACE ( 'NONE', ( #42791 ), #57792, .T. ) ;
#17970 = CARTESIAN_POINT ( 'NONE',  ( -22.27945548916780183, -2.122548946923912716, -3.016427163003911005 ) ) ;
#17971 = ORIENTED_EDGE ( 'NONE', *, *, #36251, .F. ) ;
#17972 = ORIENTED_EDGE ( 'NONE', *, *, #28806, .T. ) ;
#17973 = AXIS2_PLACEMENT_3D ( 'NONE', #42040, #47387, #62637 ) ;
#17974 = EDGE_LOOP ( 'NONE', ( #27967, #48584, #40698, #61844 ) ) ;
#17975 = CARTESIAN_POINT ( 'NONE',  ( 0.2646305136544065406, 11.46223899740605923, -4.312539723326019647 ) ) ;
#17976 = CARTESIAN_POINT ( 'NONE',  ( 47.00000000000000711, 4.705694406421931860E-17, -3.469127814946512892E-15 ) ) ;
#17977 = ORIENTED_EDGE ( 'NONE', *, *, #52293, .F. ) ;
#17978 = CARTESIAN_POINT ( 'NONE',  ( 37.00000000000000711, -12.01765980939840439, 2.021542716731525413 ) ) ;
#17979 = CARTESIAN_POINT ( 'NONE',  ( -22.28236030719477512, -0.3108070568283820556, -3.683993210674382457 ) ) ;
#17980 = ORIENTED_EDGE ( 'NONE', *, *, #22061, .T. ) ;
#17981 = FACE_OUTER_BOUND ( 'NONE', #4800, .T. ) ;
#17982 = CARTESIAN_POINT ( 'NONE',  ( -19.56743653832047514, -33.00000000000000000, -5.000000000000001776 ) ) ;
#17983 = DIRECTION ( 'NONE',  ( 0.000000000000000000, 0.01356324068817998940, -0.9999080150203990547 ) ) ;
#17984 = ORIENTED_EDGE ( 'NONE', *, *, #33750, .F. ) ;
#17985 = ORIENTED_EDGE ( 'NONE', *, *, #28357, .F. ) ;
#17986 = CARTESIAN_POINT ( 'NONE',  ( 0.1901047366177790743, -0.2738782441758320640, 11.99765584512894989 ) ) ;
#17987 = ORIENTED_EDGE ( 'NONE', *, *, #58192, .T. ) ;
#17988 = CARTESIAN_POINT ( 'NONE',  ( 10.63279796331799787, 0.6010364628809637955, -13.48722014042763462 ) ) ;
#17989 = ORIENTED_EDGE ( 'NONE', *, *, #61758, .T. ) ;
#17990 = CARTESIAN_POINT ( 'NONE',  ( 0.3665391374699464300, 0.2638605131388880864, -12.27992639892677929 ) ) ;
#17991 = CARTESIAN_POINT ( 'NONE',  ( 9.160076034422203861, -32.64719971958299283, -12.35384511440537381 ) ) ;
#17992 = CARTESIAN_POINT ( 'NONE',  ( 35.00000000000000000, -8.766823244861932096, 7.817610399097601359 ) ) ;
#17993 = EDGE_CURVE ( 'NONE', #4915, #18413, #62424, .T. ) ;
#17995 = CARTESIAN_POINT ( 'NONE',  ( 2.000000000000001776, 3.805198749487521681, -5.799611601383208637 ) ) ;
#17994 = AXIS2_PLACEMENT_3D ( 'NONE', #50503, #56813, #45828 ) ;
#17996 = CARTESIAN_POINT ( 'NONE',  ( 2.889800649504073782, -4.645655809191389984, 3.986129653162632902 ) ) ;
#17997 = CARTESIAN_POINT ( 'NONE',  ( 1.634816307074789865, -0.7191532042403158131, 12.68239325670730544 ) ) ;
#17998 = CARTESIAN_POINT ( 'NONE',  ( 5.973846796310454010, -8.876357692484395656, -8.083262641105859458 ) ) ;
#17999 = VERTEX_POINT ( 'NONE', #47795 ) ;
#18000 = DIRECTION ( 'NONE',  ( 0.000000000000000000, 0.01356324068817991828, -0.9999080150203990547 ) ) ;
#18001 = EDGE_LOOP ( 'NONE', ( #33672, #5427, #35365, #44159 ) ) ;
#18002 = AXIS2_PLACEMENT_3D ( 'NONE', #59160, #63457, #23915 ) ;
#18003 = CARTESIAN_POINT ( 'NONE',  ( 2.000000000000001776, -2.562706407243680928, 6.312399813420318750 ) ) ;
#18004 = B_SPLINE_CURVE_WITH_KNOTS ( 'NONE', 3,
 ( #4770, #55273, #24357, #25030, #39658, #9713, #9376, #29662, #49968, #60588, #45301, #20030, #40296, #25339, #15026, #35308 ),
 .UNSPECIFIED., .F., .F.,
 ( 4, 3, 3, 3, 3, 4 ),
 ( 5.421010862427522170E-19, 0.0003017745587525283912, 0.0006035491769808814383, 0.0009053241094668286080, 0.001207275924540519938, 0.001510325902534030013 ),
 .UNSPECIFIED. ) ;
#18005 = CARTESIAN_POINT ( 'NONE',  ( 1.937114397841935398, -12.45230409340483391, 3.111612666690036999 ) ) ;
#18006 = ORIENTED_EDGE ( 'NONE', *, *, #28956, .F. ) ;
#18007 = ADVANCED_FACE ( 'NONE', ( #23173 ), #38125, .F. ) ;
#18008 = CARTESIAN_POINT ( 'NONE',  ( 0.2646305136544065406, -6.008537389229341663, -10.67138229758235646 ) ) ;
#18009 = CARTESIAN_POINT ( 'NONE',  ( 0.3675815128205894289, 6.367184624550164429, 10.50067073900654080 ) ) ;
#18010 = CARTESIAN_POINT ( 'NONE',  ( 2.907497136250194902, -7.666666002096546251, 1.716624290781062712 ) ) ;
#18011 = CIRCLE ( 'NONE', #37116, 2.899999999999994582 ) ;
#18012 = ORIENTED_EDGE ( 'NONE', *, *, #60127, .T. ) ;
#18013 = EDGE_CURVE ( 'NONE', #14144, #64495, #63032, .T. ) ;
#18014 = ORIENTED_EDGE ( 'NONE', *, *, #45207, .F. ) ;
#18015 = DIRECTION ( 'NONE',  ( 1.000000000000000000, 0.000000000000000000, -0.000000000000000000 ) ) ;
#18016 = AXIS2_PLACEMENT_3D ( 'NONE', #52876, #56660, #2701 ) ;
#18017 = ORIENTED_EDGE ( 'NONE', *, *, #2025, .F. ) ;
#18018 = CYLINDRICAL_SURFACE ( 'NONE', #12752, 7.499999999999988454 ) ;
#18019 = CARTESIAN_POINT ( 'NONE',  ( 2.241509619876139059, -1.287997509666521045, -7.525055189891920904 ) ) ;
#18020 = CARTESIAN_POINT ( 'NONE',  ( -3.552825562195119247, 9.416395929211306637, 7.449814802983512507 ) ) ;
#18021 = EDGE_CURVE ( 'NONE', #63698, #18517, #65596, .T. ) ;
#18022 = CARTESIAN_POINT ( 'NONE',  ( 2.000000000000001776, 0.000000000000000000, 0.000000000000000000 ) ) ;
#18023 = VERTEX_POINT ( 'NONE', #8524 ) ;
#18024 = CIRCLE ( 'NONE', #19069, 5.000000000000001776 ) ;
#18025 = LINE ( 'NONE', #38286, #34779 ) ;
#18026 = DIRECTION ( 'NONE',  ( 0.000000000000000000, 0.000000000000000000, 1.000000000000000000 ) ) ;
#18027 = ADVANCED_FACE ( 'NONE', ( #65361 ), #15707, .F. ) ;
#18028 = DIRECTION ( 'NONE',  ( 0.000000000000000000, 0.000000000000000000, -1.000000000000000000 ) ) ;
#18029 = CARTESIAN_POINT ( 'NONE',  ( 5.515188684475870851, 0.004322737127823480206, -0.003154373509839912288 ) ) ;
#18030 = EDGE_CURVE ( 'NONE', #18023, #14592, #50091, .T. ) ;
#18031 = CARTESIAN_POINT ( 'NONE',  ( 0.2650492594609233921, 7.786980091309454011, 9.451471004987361368 ) ) ;
#18032 = CARTESIAN_POINT ( 'NONE',  ( -37.25000000000000711, -1.694065894508600678E-18, 0.000000000000000000 ) ) ;
#18033 = CARTESIAN_POINT ( 'NONE',  ( -22.65999102136915155, -0.5917351393135155124, 4.797155153747047152 ) ) ;
#18034 = EDGE_CURVE ( 'NONE', #61175, #22451, #62002, .T. ) ;
#18035 = AXIS2_PLACEMENT_3D ( 'NONE', #24149, #13504, #65027 ) ;
#18036 = VECTOR ( 'NONE', #63067, 1000.000000000000000 ) ;
#18037 = ORIENTED_EDGE ( 'NONE', *, *, #54266, .T. ) ;
#18038 = ADVANCED_FACE ( 'NONE', ( #13823 ), #59737, .T. ) ;
#18039 = CARTESIAN_POINT ( 'NONE',  ( 11.97712667809381770, -9.005688583286994842, -7.937970216750675156 ) ) ;
#18040 = ADVANCED_FACE ( 'NONE', ( #14800 ), #33790, .T. ) ;
#18041 = ORIENTED_EDGE ( 'NONE', *, *, #14214, .F. ) ;
#18042 = CARTESIAN_POINT ( 'NONE',  ( 0.3610902822527229938, 1.873269382026155228, -12.13436647668548929 ) ) ;
#18043 = DIRECTION ( 'NONE',  ( 0.000000000000000000, 0.000000000000000000, 1.000000000000000000 ) ) ;
#18044 = CARTESIAN_POINT ( 'NONE',  ( 1.109979610372368919, -9.281420052101120532, -8.414317452283038179 ) ) ;
#18045 = ORIENTED_EDGE ( 'NONE', *, *, #21290, .T. ) ;
#18046 = ADVANCED_FACE ( 'NONE', ( #54091 ), #49127, .T. ) ;
#18047 = CARTESIAN_POINT ( 'NONE',  ( 2.253265082353314686, 6.549959928642921980, 3.929729351084445099 ) ) ;
#18048 = EDGE_LOOP ( 'NONE', ( #18177, #29647, #7820, #2740 ) ) ;
#18049 = DIRECTION ( 'NONE',  ( -1.000000000000000000, 0.000000000000000000, 0.000000000000000000 ) ) ;
#18050 = ORIENTED_EDGE ( 'NONE', *, *, #59477, .T. ) ;
#18051 = VERTEX_POINT ( 'NONE', #24154 ) ;
#18052 = CARTESIAN_POINT ( 'NONE',  ( -10.84987915304990658, -8.326549988222685883, -8.645316455905160069 ) ) ;
#18053 = CIRCLE ( 'NONE', #26535, 2.899999999999995914 ) ;
#18054 = CARTESIAN_POINT ( 'NONE',  ( -22.28023996335807411, -3.345627887484365903, -1.558279384310083282 ) ) ;
#18055 = ORIENTED_EDGE ( 'NONE', *, *, #64037, .F. ) ;
#18056 = CARTESIAN_POINT ( 'NONE',  ( -37.00000000000000711, 3.916263239775508165, -11.07407352312208459 ) ) ;
#18057 = CARTESIAN_POINT ( 'NONE',  ( 3.831474068947881229, 5.123838571001932962, 12.49171852625460488 ) ) ;
#18058 = AXIS2_PLACEMENT_3D ( 'NONE', #54694, #53378, #58710 ) ;
#18059 = DIRECTION ( 'NONE',  ( -1.000000000000000000, 0.000000000000000000, 0.000000000000000000 ) ) ;
#18060 = FACE_OUTER_BOUND ( 'NONE', #27355, .T. ) ;
#18061 = EDGE_LOOP ( 'NONE', ( #25934, #9092, #45440, #59027 ) ) ;
#18062 =( BOUNDED_SURFACE ( )  B_SPLINE_SURFACE ( 3, 1, ( 
 ( #22195, #942 ),
 ( #41483, #56825 ),
 ( #1926, #31518 ),
 ( #36519, #62118 ) ),
 .UNSPECIFIED., .F., .F., .F. ) 
 B_SPLINE_SURFACE_WITH_KNOTS ( ( 4, 4 ),
 ( 2, 2 ),
 ( 0.000000000000000000, 1.000000000000000000 ),
 ( 0.000000000000000000, 1.000000000000000000 ),
 .UNSPECIFIED. ) 
 GEOMETRIC_REPRESENTATION_ITEM ( )  RATIONAL_B_SPLINE_SURFACE ( (
 ( 1.000000000000000000, 1.000000000000000000),
 ( 0.9932032654565553509, 0.8386279382598740284),
 ( 0.9932032654565553509, 0.8386279382598740284),
 ( 1.000000000000000000, 1.000000000000000000) ) ) 
 REPRESENTATION_ITEM ( '' )  SURFACE ( )  );
#18063 = CYLINDRICAL_SURFACE ( 'NONE', #62824, 5.000000000000000888 ) ;
#18064 = CARTESIAN_POINT ( 'NONE',  ( 12.57831868240780082, -29.25370879966822812, 4.768001503383645812 ) ) ;
#18065 = CARTESIAN_POINT ( 'NONE',  ( -27.05874794189610455, 0.3907329275428126913, 2.180117559290193796 ) ) ;
#18067 = ORIENTED_EDGE ( 'NONE', *, *, #28615, .F. ) ;
#18066 = CARTESIAN_POINT ( 'NONE',  ( 36.00000000000000711, -2.527899948230726057, -12.49688848680883346 ) ) ;
#18068 = DIRECTION ( 'NONE',  ( 0.000000000000000000, 0.000000000000000000, 1.000000000000000000 ) ) ;
#18069 = ORIENTED_EDGE ( 'NONE', *, *, #41184, .T. ) ;
#18070 = CARTESIAN_POINT ( 'NONE',  ( -20.35303972915886561, 13.07716483859543999, -3.365615382918716758 ) ) ;
#18071 = AXIS2_PLACEMENT_3D ( 'NONE', #39231, #65792, #59527 ) ;
#18072 = ORIENTED_EDGE ( 'NONE', *, *, #16922, .T. ) ;
#18073 = CARTESIAN_POINT ( 'NONE',  ( 21.44111281379507261, -11.69236863416677075, -2.731880686291859206 ) ) ;
#18074 = CARTESIAN_POINT ( 'NONE',  ( 0.2872850955227758685, 3.994021792079249789, -11.58431228138434932 ) ) ;
#18075 = DIRECTION ( 'NONE',  ( 0.000000000000000000, -0.01356324068817991828, 0.9999080150203990547 ) ) ;
#18076 = CARTESIAN_POINT ( 'NONE',  ( 0.3675815128205894289, -3.951233083390547129, 11.62724744438064306 ) ) ;
#18077 = EDGE_CURVE ( 'NONE', #21253, #60341, #46065, .T. ) ;
#18078 = CARTESIAN_POINT ( 'NONE',  ( 0.3610902822527287670, 9.572034936626899082, 7.689482111308885592 ) ) ;
#18079 = DIRECTION ( 'NONE',  ( 0.000000000000000000, 0.2149704402110246271, -0.9766205557100866574 ) ) ;
#18080 = CARTESIAN_POINT ( 'NONE',  ( -22.29382655386184453, -3.622626291186075598, -0.8947172055470860030 ) ) ;
#18081 = VERTEX_POINT ( 'NONE', #14481 ) ;
#18082 = FACE_OUTER_BOUND ( 'NONE', #54123, .T. ) ;
#18083 = ORIENTED_EDGE ( 'NONE', *, *, #8692, .F. ) ;
#18084 = VERTEX_POINT ( 'NONE', #4550 ) ;
#18085 = EDGE_CURVE ( 'NONE', #65715, #10582, #21940, .T. ) ;
#18086 = CARTESIAN_POINT ( 'NONE',  ( 1.372161826076905289, 1.607409531431637673, -12.51237317864402954 ) ) ;
#18087 = CYLINDRICAL_SURFACE ( 'NONE', #55977, 12.18649999999999878 ) ;
#18088 = DIRECTION ( 'NONE',  ( 1.000000000000000000, 0.000000000000000000, 0.000000000000000000 ) ) ;
#18089 = CARTESIAN_POINT ( 'NONE',  ( -22.30078715814471835, 2.097357782488240119, 3.111489293522180510 ) ) ;
#18090 = DIRECTION ( 'NONE',  ( 1.000000000000000000, 0.000000000000000000, 0.000000000000000000 ) ) ;
#18091 = CARTESIAN_POINT ( 'NONE',  ( -35.00000000000000000, 0.000000000000000000, 0.000000000000000000 ) ) ;
#18092 = VECTOR ( 'NONE', #6748, 1000.000000000000000 ) ;
#18093 = STYLED_ITEM ( 'NONE', ( #61847 ), #7246 ) ;
#18094 = AXIS2_PLACEMENT_3D ( 'NONE', #39370, #65611, #14101 ) ;
#18095 = CARTESIAN_POINT ( 'NONE',  ( 37.00000000000000711, 5.672855678558685888, -10.28547182238010116 ) ) ;
#18096 = ORIENTED_EDGE ( 'NONE', *, *, #18298, .T. ) ;
#18097 = CARTESIAN_POINT ( 'NONE',  ( 2.000000000000001776, 0.000000000000000000, 0.000000000000000000 ) ) ;
#18098 = CARTESIAN_POINT ( 'NONE',  ( -27.08426504710140392, -1.591094357919260904, -1.649100202714224750 ) ) ;
#18099 = DIRECTION ( 'NONE',  ( 0.000000000000000000, -0.01356324068817999114, 0.9999080150203989437 ) ) ;
#18100 = EDGE_CURVE ( 'NONE', #46798, #63438, #4700, .T. ) ;
#18101 = EDGE_CURVE ( 'NONE', #57337, #20539, #34369, .T. ) ;
#18102 = CARTESIAN_POINT ( 'NONE',  ( -35.00000000000000000, 12.73293890771483206, 0.6593684648220944355 ) ) ;
#18103 = DIRECTION ( 'NONE',  ( 0.000000000000000000, 0.000000000000000000, 1.000000000000000000 ) ) ;
#18104 = AXIS2_PLACEMENT_3D ( 'NONE', #62351, #16806, #37416 ) ;
#18105 = CARTESIAN_POINT ( 'NONE',  ( -6.521449894988646356, -1.136726751579723249, 13.45215267574590889 ) ) ;
#18106 = CARTESIAN_POINT ( 'NONE',  ( -10.84199523828880984, -6.639569374722061212, 11.75613028300089091 ) ) ;
#18107 = EDGE_LOOP ( 'NONE', ( #50495, #3800, #26526, #45886 ) ) ;
#18108 = CARTESIAN_POINT ( 'NONE',  ( 47.00000000000000711, 4.705694406421931860E-17, -3.469127814946512892E-15 ) ) ;
#18109 = CARTESIAN_POINT ( 'NONE',  ( 5.514970785353741078, 0.004588761610584827719, 0.001117786416802128355 ) ) ;
#18110 = DIRECTION ( 'NONE',  ( -1.000000000000000000, 0.000000000000000000, 0.000000000000000000 ) ) ;
#18111 = AXIS2_PLACEMENT_3D ( 'NONE', #46611, #36949, #26994 ) ;
#18112 = EDGE_CURVE ( 'NONE', #4846, #1056, #65172, .T. ) ;
#18113 = ADVANCED_FACE ( 'NONE', ( #29775 ), #45098, .T. ) ;
#18114 = DIRECTION ( 'NONE',  ( 0.000000000000000000, -0.5472293298355330737, 0.8369827122275305120 ) ) ;
#18115 = CARTESIAN_POINT ( 'NONE',  ( 35.00000000000000000, -10.14408668126217350, -5.921969905510321652 ) ) ;
#18116 = AXIS2_PLACEMENT_3D ( 'NONE', #25842, #5228, #10863 ) ;
#18117 = VERTEX_POINT ( 'NONE', #20805 ) ;
#18118 = CARTESIAN_POINT ( 'NONE',  ( 18.99404383257591178, -0.5703370437478472166, 12.04059188870767372 ) ) ;
#18119 = CARTESIAN_POINT ( 'NONE',  ( 2.255723233588630361, -4.808373255829151205, -5.936060085173213707 ) ) ;
#18120 = LINE ( 'NONE', #28413, #49912 ) ;
#18121 = ORIENTED_EDGE ( 'NONE', *, *, #18360, .T. ) ;
#18122 = EDGE_CURVE ( 'NONE', #52452, #63611, #5721, .T. ) ;
#18123 = LINE ( 'NONE', #38393, #35048 ) ;
#18124 = AXIS2_PLACEMENT_3D ( 'NONE', #48079, #64006, #8815 ) ;
#18125 = CYLINDRICAL_SURFACE ( 'NONE', #2229, 6.936499999999988120 ) ;
#18126 = ORIENTED_EDGE ( 'NONE', *, *, #62596, .T. ) ;
#18127 = ORIENTED_EDGE ( 'NONE', *, *, #37443, .T. ) ;
#18128 = DIRECTION ( 'NONE',  ( 0.000000000000000000, -0.1764146379942750087, -0.9843159429275484262 ) ) ;
#18129 = AXIS2_PLACEMENT_3D ( 'NONE', #13281, #33563, #62487 ) ;
#18130 = AXIS2_PLACEMENT_3D ( 'NONE', #10845, #6521, #47737 ) ;
#18131 = ADVANCED_FACE ( 'NONE', ( #203 ), #45408, .T. ) ;
#18132 = ORIENTED_EDGE ( 'NONE', *, *, #50048, .T. ) ;
#18133 = CARTESIAN_POINT ( 'NONE',  ( 1.462291587749892319, -12.32753368892837642, -2.816455204776596499 ) ) ;
#18134 = CARTESIAN_POINT ( 'NONE',  ( -27.35552965826137140, -3.094132632038958608, -0.2619431035392160156 ) ) ;
#18135 = DIRECTION ( 'NONE',  ( 1.000000000000000000, 0.000000000000000000, 0.000000000000000000 ) ) ;
#18136 = DIRECTION ( 'NONE',  ( 0.000000000000000000, -0.9985334138511243740, 0.05413890858540768014 ) ) ;
#18137 = DIRECTION ( 'NONE',  ( 1.000000000000000000, 0.000000000000000000, 0.000000000000000000 ) ) ;
#18138 = CARTESIAN_POINT ( 'NONE',  ( 1.372161826075801283, 12.04315837901262221, 3.755740169579934840 ) ) ;
#18140 = ORIENTED_EDGE ( 'NONE', *, *, #23367, .T. ) ;
#18139 = CARTESIAN_POINT ( 'NONE',  ( 2.000000000000001776, 0.000000000000000000, 0.000000000000000000 ) ) ;
#18141 = FACE_OUTER_BOUND ( 'NONE', #9210, .T. ) ;
#18142 = ORIENTED_EDGE ( 'NONE', *, *, #1379, .F. ) ;
#18143 = CARTESIAN_POINT ( 'NONE',  ( 35.00000000000000000, -0.3025107581130382917, 11.74226168163341022 ) ) ;
#18144 = ORIENTED_EDGE ( 'NONE', *, *, #41135, .F. ) ;
#18145 = ORIENTED_EDGE ( 'NONE', *, *, #53832, .F. ) ;
#18146 = CONTEXT_DEPENDENT_SHAPE_REPRESENTATION ( #63763, #12190 ) ;
#18147 = CARTESIAN_POINT ( 'NONE',  ( -24.81811232574347059, 10.66920234648263488, 8.273232917182683721 ) ) ;
#18148 = CIRCLE ( 'NONE', #55301, 12.18650000000000055 ) ;
#18149 = CARTESIAN_POINT ( 'NONE',  ( -0.9057367950588101069, -28.12814853318038644, 13.89764383195466912 ) ) ;
#18150 = CARTESIAN_POINT ( 'NONE',  ( -24.95274435386256329, 11.81191533060742493, 6.539041355910289788 ) ) ;
#18151 = AXIS2_PLACEMENT_3D ( 'NONE', #33057, #39357, #53363 ) ;
#18152 = LINE ( 'NONE', #28133, #9413 ) ;
#18153 = CARTESIAN_POINT ( 'NONE',  ( -47.77118093457291081, -0.4451837999798801682, -7.743266003128062458 ) ) ;
#18154 = CARTESIAN_POINT ( 'NONE',  ( -35.00000000000000000, 9.493370459201697642, 6.917234959366862057 ) ) ;
#18156 = EDGE_LOOP ( 'NONE', ( #12353, #37693, #27516, #58958 ) ) ;
#18155 = CIRCLE ( 'NONE', #35065, 5.000000000000001776 ) ;
#18157 = EDGE_CURVE ( 'NONE', #40994, #8415, #62030, .T. ) ;
#18158 = CARTESIAN_POINT ( 'NONE',  ( -26.34357995062409330, -10.72024744338163593, 5.392951959879463075 ) ) ;
#18159 = DIRECTION ( 'NONE',  ( 0.000000000000000000, 0.01356324068818000848, -0.9999080150203990547 ) ) ;
#18160 = DIRECTION ( 'NONE',  ( -1.000000000000000000, -1.836970198721029688E-16, -0.000000000000000000 ) ) ;
#18161 = EDGE_LOOP ( 'NONE', ( #9382, #2305, #34863, #52352 ) ) ;
#18162 = AXIS2_PLACEMENT_3D ( 'NONE', #61106, #15538, #24544 ) ;
#18163 = CARTESIAN_POINT ( 'NONE',  ( 0.9232058338315048962, -4.617996777200650271, 11.58467545991552328 ) ) ;
#18164 = ORIENTED_EDGE ( 'NONE', *, *, #25315, .F. ) ;
#18165 = AXIS2_PLACEMENT_3D ( 'NONE', #5006, #25266, #45544 ) ;
#18166 = EDGE_CURVE ( 'NONE', #25415, #60864, #28021, .T. ) ;
#18167 = CARTESIAN_POINT ( 'NONE',  ( 25.00000000000000355, -30.00000000000000000, -25.00000000000000000 ) ) ;
#18168 = CARTESIAN_POINT ( 'NONE',  ( -10.60783295782091074, -9.408442966608031810, 7.467594787374099319 ) ) ;
#18169 = DIRECTION ( 'NONE',  ( -1.000000000000000000, 0.000000000000000000, 0.000000000000000000 ) ) ;
#18170 = CARTESIAN_POINT ( 'NONE',  ( -22.27945548916780183, 3.016427163003909229, -2.122548946923910940 ) ) ;
#18171 = CARTESIAN_POINT ( 'NONE',  ( -37.00000000000000711, 10.14408668126213442, 5.921969905510389154 ) ) ;
#18172 = DIRECTION ( 'NONE',  ( -0.000000000000000000, -0.000000000000000000, -1.000000000000000000 ) ) ;
#18173 = CARTESIAN_POINT ( 'NONE',  ( 2.259830038564998311, 3.938923657569498360, -6.546987858513332093 ) ) ;
#18174 = AXIS2_PLACEMENT_3D ( 'NONE', #25672, #40965, #61244 ) ;
#18175 = VERTEX_POINT ( 'NONE', #15149 ) ;
#18176 = CARTESIAN_POINT ( 'NONE',  ( -35.00000000000000000, 9.700295462048664774, 7.376655759824919834 ) ) ;
#18177 = ORIENTED_EDGE ( 'NONE', *, *, #15168, .T. ) ;
#18178 = CIRCLE ( 'NONE', #5465, 5.000000000000000888 ) ;
#18179 = ADVANCED_FACE ( 'NONE', ( #16140 ), #46725, .T. ) ;
#18180 = CARTESIAN_POINT ( 'NONE',  ( 0.3675815128205912052, 3.951233083390468526, 11.62724744438066971 ) ) ;
#18181 = EDGE_CURVE ( 'NONE', #62557, #63186, #41817, .T. ) ;
#18182 = CARTESIAN_POINT ( 'NONE',  ( -35.00000000000000000, 11.73463472867576129, 3.287724142101457137 ) ) ;
#18183 = DIRECTION ( 'NONE',  ( -1.000000000000000000, 0.000000000000000000, 0.000000000000000000 ) ) ;
#18184 = EDGE_CURVE ( 'NONE', #9014, #28947, #47157, .T. ) ;
#18185 = VERTEX_POINT ( 'NONE', #15479 ) ;
#18186 = CIRCLE ( 'NONE', #94, 5.000000000000000888 ) ;
#18187 = CARTESIAN_POINT ( 'NONE',  ( -27.10128162969864363, 0.1566844438592239763, 2.337214317750524906 ) ) ;
#18188 = VERTEX_POINT ( 'NONE', #50743 ) ;
#18189 = CIRCLE ( 'NONE', #47900, 11.99999999999998579 ) ;
#18190 = CARTESIAN_POINT ( 'NONE',  ( 2.000000000000001776, -1.145812388885072863, -6.715725538143620277 ) ) ;
#18191 = CARTESIAN_POINT ( 'NONE',  ( 8.829757094950462459, 6.323861778933462574, 10.20043549987153497 ) ) ;
#18192 = DIRECTION ( 'NONE',  ( -1.000000000000000000, 0.000000000000000000, 0.000000000000000000 ) ) ;
#18193 = FACE_OUTER_BOUND ( 'NONE', #11409, .T. ) ;
#18194 = ORIENTED_EDGE ( 'NONE', *, *, #19776, .T. ) ;
#18195 = CARTESIAN_POINT ( 'NONE',  ( 2.373367633546869193, 2.455525055524889755, 7.275198254387420072 ) ) ;
#18196 = DIRECTION ( 'NONE',  ( -1.000000000000000000, -0.000000000000000000, -0.000000000000000000 ) ) ;
#18197 = CARTESIAN_POINT ( 'NONE',  ( 2.556980015514224824, -1.116161541731589102, 7.658710847181716019 ) ) ;
#18198 = DIRECTION ( 'NONE',  ( 1.000000000000000000, -0.000000000000000000, -0.000000000000000000 ) ) ;
#18199 = EDGE_CURVE ( 'NONE', #4143, #23433, #46402, .T. ) ;
#18200 = AXIS2_PLACEMENT_3D ( 'NONE', #61945, #41978, #16709 ) ;
#18201 = CIRCLE ( 'NONE', #57456, 2.899999999999994582 ) ;
#18202 = CARTESIAN_POINT ( 'NONE',  ( 2.257661810676422576, -0.1348365785570478925, -7.638648121130928281 ) ) ;
#18203 = CARTESIAN_POINT ( 'NONE',  ( -36.00000000000000711, -12.21925492305359562, -3.640372113593682624 ) ) ;
#18204 = VERTEX_POINT ( 'NONE', #5532 ) ;
#18205 = CARTESIAN_POINT ( 'NONE',  ( -27.08418322526031119, 1.789041206975757747, -1.431535851194440268 ) ) ;
#18206 = AXIS2_PLACEMENT_3D ( 'NONE', #24039, #19043, #23054 ) ;
#18207 = CARTESIAN_POINT ( 'NONE',  ( -2.136460567204509164, -31.12783502484143128, -14.34456412933875846 ) ) ;
#18208 = VERTEX_POINT ( 'NONE', #21463 ) ;
#18209 = CARTESIAN_POINT ( 'NONE',  ( -11.40165637463000614, -7.508992741355387857, -11.21895841913464587 ) ) ;
#18210 = CARTESIAN_POINT ( 'NONE',  ( 1.198791140418975054, -8.460175745278220916, 9.279671759317787760 ) ) ;
#18211 = CARTESIAN_POINT ( 'NONE',  ( 17.48309864844228301, -10.09872697878719627, 8.990776945112616048 ) ) ;
#18212 = AXIS2_PLACEMENT_3D ( 'NONE', #25508, #35794, #56791 ) ;
#18213 = CYLINDRICAL_SURFACE ( 'NONE', #10531, 12.18650000000000055 ) ;
#18214 = CARTESIAN_POINT ( 'NONE',  ( 0.000000000000000000, -2.473437528934089524, -7.080403010455012414 ) ) ;
#18215 = ORIENTED_EDGE ( 'NONE', *, *, #10741, .T. ) ;
#18216 = CYLINDRICAL_SURFACE ( 'NONE', #41430, 12.74999999999999822 ) ;
#18217 = ORIENTED_EDGE ( 'NONE', *, *, #63178, .F. ) ;
#18218 = AXIS2_PLACEMENT_3D ( 'NONE', #15926, #31250, #36210 ) ;
#18219 = DIRECTION ( 'NONE',  ( 1.000000000000000000, 0.000000000000000000, 0.000000000000000000 ) ) ;
#18220 = CYLINDRICAL_SURFACE ( 'NONE', #38557, 5.000000000000000888 ) ;
#18221 = CARTESIAN_POINT ( 'NONE',  ( -27.20102706715914209, 0.5453431011645279991, -2.585824624629319946 ) ) ;
#18222 = LINE ( 'NONE', #38493, #26953 ) ;
#18223 = DIRECTION ( 'NONE',  ( 1.000000000000000000, 0.000000000000000000, -0.000000000000000000 ) ) ;
#18224 = CARTESIAN_POINT ( 'NONE',  ( 2.263328370261526334, -1.186889399881243978, 7.548992860189811971 ) ) ;
#18225 = CARTESIAN_POINT ( 'NONE',  ( 0.3665391374699464300, 7.691255657244292721, 9.576575648339046509 ) ) ;
#18226 = CIRCLE ( 'NONE', #63867, 2.899999999999994582 ) ;
#18227 = VERTEX_POINT ( 'NONE', #35433 ) ;
#18228 = ORIENTED_EDGE ( 'NONE', *, *, #43745, .T. ) ;
#18229 = CARTESIAN_POINT ( 'NONE',  ( 5.515188684475870851, -0.003154373509839893206, 0.004322737127823964194 ) ) ;
#18230 = ORIENTED_EDGE ( 'NONE', *, *, #55344, .T. ) ;
#18231 = SURFACE_STYLE_USAGE ( .BOTH. , #16907 ) ;
#18232 = CARTESIAN_POINT ( 'NONE',  ( -22.27706485742869091, 2.625261754997705310, -2.580541389029900934 ) ) ;
#18234 = CARTESIAN_POINT ( 'NONE',  ( -27.32343372485684796, 0.1402256980610574744, -3.007804754713670814 ) ) ;
#18233 = CIRCLE ( 'NONE', #55383, 2.899999999999994582 ) ;
#18235 = AXIS2_PLACEMENT_3D ( 'NONE', #16012, #20696, #21001 ) ;
#18236 = CIRCLE ( 'NONE', #26674, 5.000000000000000000 ) ;
#18237 = CARTESIAN_POINT ( 'NONE',  ( 2.000000000000001776, 3.152010634611773110, -6.039758645301250617 ) ) ;
#18238 = ORIENTED_EDGE ( 'NONE', *, *, #65269, .F. ) ;
#18239 = CARTESIAN_POINT ( 'NONE',  ( 0.2872850955227734815, 5.944938343726402508, -10.71476594226527190 ) ) ;
#18240 = EDGE_CURVE ( 'NONE', #26911, #48492, #540, .T. ) ;
#18241 = CARTESIAN_POINT ( 'NONE',  ( 2.440552418640496768, 1.531218882877394050, -7.547055375260044663 ) ) ;
#18242 = CARTESIAN_POINT ( 'NONE',  ( 3.100650473569749987, -1.818095316078653267, 7.709402782713603131 ) ) ;
#18243 = EDGE_LOOP ( 'NONE', ( #62608, #36504, #31835, #26174 ) ) ;
#18244 = ORIENTED_EDGE ( 'NONE', *, *, #17105, .T. ) ;
#18245 = FACE_OUTER_BOUND ( 'NONE', #25124, .T. ) ;
#18246 = ORIENTED_EDGE ( 'NONE', *, *, #3925, .T. ) ;
#18247 = DIRECTION ( 'NONE',  ( -1.000000000000000000, 0.000000000000000000, 0.000000000000000000 ) ) ;
#18248 = ORIENTED_EDGE ( 'NONE', *, *, #13511, .T. ) ;
#18249 = B_SPLINE_CURVE_WITH_KNOTS ( 'NONE', 3,
 ( #42476, #42154, #17243, #62443, #64099, #13540, #54789 ),
 .UNSPECIFIED., .F., .F.,
 ( 4, 3, 4 ),
 ( 0.000000000000000000, 0.001700533616330525194, 0.005002426799371280895 ),
 .UNSPECIFIED. ) ;
#18250 = ORIENTED_EDGE ( 'NONE', *, *, #17512, .T. ) ;
#18251 = CIRCLE ( 'NONE', #41578, 5.000000000000001776 ) ;
#18252 = CYLINDRICAL_SURFACE ( 'NONE', #6542, 12.18650000000000055 ) ;
#18253 = CARTESIAN_POINT ( 'NONE',  ( 37.00000000000000711, -10.14408668126217350, -5.921969905510321652 ) ) ;
#18254 = AXIS2_PLACEMENT_3D ( 'NONE', #59497, #9261, #49849 ) ;
#18255 = DIRECTION ( 'NONE',  ( 0.000000000000000000, 0.01356324068817991828, -0.9999080150203990547 ) ) ;
#18257 = ADVANCED_FACE ( 'NONE', ( #15791 ), #45742, .T. ) ;
#18256 = CARTESIAN_POINT ( 'NONE',  ( -35.00000000000000000, -8.854740511458796703, -7.717887834988336415 ) ) ;
#18258 = CARTESIAN_POINT ( 'NONE',  ( -25.00000000000000355, -9.999999999999998224, 1.530808498934191521E-15 ) ) ;
#18259 = AXIS2_PLACEMENT_3D ( 'NONE', #38205, #22946, #29229 ) ;
#18260 = CARTESIAN_POINT ( 'NONE',  ( 145.1370849898475797, 3.309064568108273190E-14, 0.000000000000000000 ) ) ;
#18261 =( BOUNDED_SURFACE ( )  B_SPLINE_SURFACE ( 3, 1, ( 
 ( #5045, #4398 ),
 ( #29324, #40265 ),
 ( #4059, #49619 ),
 ( #34307, #10029 ) ),
 .UNSPECIFIED., .F., .F., .F. ) 
 B_SPLINE_SURFACE_WITH_KNOTS ( ( 4, 4 ),
 ( 2, 2 ),
 ( 0.000000000000000000, 1.000000000000000000 ),
 ( 0.000000000000000000, 1.000000000000000000 ),
 .UNSPECIFIED. ) 
 GEOMETRIC_REPRESENTATION_ITEM ( )  RATIONAL_B_SPLINE_SURFACE ( (
 ( 1.000000000000000000, 1.000000000000000000),
 ( 0.9932032654565553509, 0.8386279382598736953),
 ( 0.9932032654565553509, 0.8386279382598736953),
 ( 1.000000000000000000, 1.000000000000000000) ) ) 
 REPRESENTATION_ITEM ( '' )  SURFACE ( )  );
#18262 = VERTEX_POINT ( 'NONE', #11160 ) ;
#18263 = PLANE ( 'NONE',  #42195 ) ;
#18264 = DIRECTION ( 'NONE',  ( 0.000000000000000000, 0.01356324068817992175, -0.9999080150203990547 ) ) ;
#18265 = AXIS2_PLACEMENT_3D ( 'NONE', #54712, #39728, #14115 ) ;
#18266 = CARTESIAN_POINT ( 'NONE',  ( 2.288423627607770960, 3.684511167348237581, -6.704349683466525711 ) ) ;
#18267 = EDGE_CURVE ( 'NONE', #43036, #25930, #58324, .T. ) ;
#18269 = EDGE_CURVE ( 'NONE', #59550, #50924, #2158, .T. ) ;
#18268 = CARTESIAN_POINT ( 'NONE',  ( 35.00000000000000000, -1.463443770872862482, -12.09831040184923978 ) ) ;
#18270 = CARTESIAN_POINT ( 'NONE',  ( 28.91461756896324786, 10.37982945138888446, 6.039709648425571231 ) ) ;
#18271 = DIRECTION ( 'NONE',  ( -1.000000000000000000, 0.000000000000000000, 0.000000000000000000 ) ) ;
#18272 = CIRCLE ( 'NONE', #55410, 2.899999999999995026 ) ;
#18273 = CARTESIAN_POINT ( 'NONE',  ( -27.08419642509983305, 1.538761233743672241, 1.697757994346396737 ) ) ;
#18274 = CARTESIAN_POINT ( 'NONE',  ( 35.00000000000000000, 4.705694406421931860E-17, -3.469127814946512892E-15 ) ) ;
#18275 = CARTESIAN_POINT ( 'NONE',  ( -4.989057617119011745, -0.9162120371760335003, 11.96497202265570259 ) ) ;
#18276 = ORIENTED_EDGE ( 'NONE', *, *, #38061, .T. ) ;
#18277 = CARTESIAN_POINT ( 'NONE',  ( 3.100650473569752652, -7.276570693048392435, -3.129198107108044802 ) ) ;
#18278 =( BOUNDED_CURVE ( )  B_SPLINE_CURVE ( 3, ( #32472, #7540, #47471, #2907 ),
 .UNSPECIFIED., .F., .F. ) 
 B_SPLINE_CURVE_WITH_KNOTS ( ( 4, 4 ),
 ( 5.009162659680186813, 5.030260039792340265 ),
 .UNSPECIFIED. ) 
 CURVE ( )  GEOMETRIC_REPRESENTATION_ITEM ( )  RATIONAL_B_SPLINE_CURVE ( ( 1.000000000000000000, 0.9999629087233127267, 0.9999629087233127267, 1.000000000000000000 ) ) 
 REPRESENTATION_ITEM ( '' )  );
#18279 = VERTEX_POINT ( 'NONE', #52052 ) ;
#18280 = CARTESIAN_POINT ( 'NONE',  ( 35.00000000000000000, -10.99909370905160699, -5.246972444133983338 ) ) ;
#18281 = DIRECTION ( 'NONE',  ( 0.000000000000000000, -0.9551603052523448545, 0.2960891610144612551 ) ) ;
#18282 = CARTESIAN_POINT ( 'NONE',  ( 12.90917927732748360, -12.48803436428174507, -5.132121098330106435 ) ) ;
#18283 = CARTESIAN_POINT ( 'NONE',  ( -22.27384469013076185, -2.581192766446256837, -2.625926801827886070 ) ) ;
#18284 = CARTESIAN_POINT ( 'NONE',  ( 2.245754705088394587, -6.667819336165968558, 3.721112460996998994 ) ) ;
#18285 = ORIENTED_EDGE ( 'NONE', *, *, #22901, .T. ) ;
#18286 = DIRECTION ( 'NONE',  ( 0.000000000000000000, 0.000000000000000000, 1.000000000000000000 ) ) ;
#18287 = CARTESIAN_POINT ( 'NONE',  ( 22.88594695219327235, -4.822122601967141264, 12.60940655271284427 ) ) ;
#18288 = CARTESIAN_POINT ( 'NONE',  ( -27.09729107899804745, 2.094470452260986271, 1.021938248125897397 ) ) ;
#18289 = DIRECTION ( 'NONE',  ( 0.000000000000000000, 0.01356324068817998940, -0.9999080150203990547 ) ) ;
#18290 = AXIS2_PLACEMENT_3D ( 'NONE', #48404, #12458, #62670 ) ;
#18291 = AXIS2_PLACEMENT_3D ( 'NONE', #17681, #60107, #34502 ) ;
#18292 = VECTOR ( 'NONE', #31671, 1000.000000000000000 ) ;
#18293 = CARTESIAN_POINT ( 'NONE',  ( 2.305787727787084407, -3.682701754025465846, -6.711944854845862451 ) ) ;
#18294 = ORIENTED_EDGE ( 'NONE', *, *, #64112, .T. ) ;
#18295 = DIRECTION ( 'NONE',  ( -1.000000000000000000, -0.000000000000000000, 0.000000000000000000 ) ) ;
#18296 = CARTESIAN_POINT ( 'NONE',  ( 2.000000000000001776, -3.155844197800055539, -6.177028383390492650 ) ) ;
#18297 = CARTESIAN_POINT ( 'NONE',  ( 2.241352910868908754, -3.889181972941404553, -6.569501556381482921 ) ) ;
#18298 = EDGE_CURVE ( 'NONE', #9098, #60526, #23805, .T. ) ;
#18299 = VECTOR ( 'NONE', #4434, 1000.000000000000000 ) ;
#18300 = EDGE_CURVE ( 'NONE', #49629, #57610, #55963, .T. ) ;
#18301 = AXIS2_PLACEMENT_3D ( 'NONE', #54771, #55407, #23863 ) ;
#18302 = ORIENTED_EDGE ( 'NONE', *, *, #2506, .T. ) ;
#18303 = ORIENTED_EDGE ( 'NONE', *, *, #32927, .F. ) ;
#18304 = CARTESIAN_POINT ( 'NONE',  ( 36.00000000000000711, -10.93004082984023029, -6.564808257521734802 ) ) ;
#18305 = ORIENTED_EDGE ( 'NONE', *, *, #14517, .T. ) ;
#18306 = CARTESIAN_POINT ( 'NONE',  ( 5.515188684475870851, 0.002166413411657797106, 0.004893136156458006460 ) ) ;
#18307 = FACE_OUTER_BOUND ( 'NONE', #1498, .T. ) ;
#18308 = CARTESIAN_POINT ( 'NONE',  ( -27.09125059358653331, -1.662156772098235091, -1.607567221344416986 ) ) ;
#18309 = CARTESIAN_POINT ( 'NONE',  ( 0.2958664285830451823, 9.245659426743992881, -8.045892866065264215 ) ) ;
#18310 = CIRCLE ( 'NONE', #52249, 5.000000000000000888 ) ;
#18311 = CARTESIAN_POINT ( 'NONE',  ( 2.000000000000001776, -6.470132594555817462, 2.133363481234057168 ) ) ;
#18312 = ORIENTED_EDGE ( 'NONE', *, *, #25770, .T. ) ;
#18313 = ORIENTED_EDGE ( 'NONE', *, *, #20137, .T. ) ;
#18314 = ORIENTED_EDGE ( 'NONE', *, *, #28077, .T. ) ;
#18315 = CARTESIAN_POINT ( 'NONE',  ( 2.000000000000001776, 6.997684042076949495, -2.698595569414168338 ) ) ;
#18316 = B_SPLINE_CURVE_WITH_KNOTS ( 'NONE', 3,
 ( #8550, #38488, #50112, #13529, #13845, #3260 ),
 .UNSPECIFIED., .F., .F.,
 ( 4, 2, 4 ),
 ( 0.0002637379172192615877, 0.0009975831966643347939, 0.001731428476109407675 ),
 .UNSPECIFIED. ) ;
#18317 = CARTESIAN_POINT ( 'NONE',  ( -37.00000000000000711, 12.57916205664481346, 2.080187960898606470 ) ) ;
#18318 = EDGE_CURVE ( 'NONE', #15421, #27180, #51268, .T. ) ;
#18319 = VERTEX_POINT ( 'NONE', #42054 ) ;
#18320 = DIRECTION ( 'NONE',  ( -1.000000000000000000, 0.000000000000000000, 0.000000000000000000 ) ) ;
#18321 = CIRCLE ( 'NONE', #5606, 6.936499999999989008 ) ;
#18322 = CARTESIAN_POINT ( 'NONE',  ( 2.253265082352431836, -7.543541742286985041, 1.199885753716602999 ) ) ;
#18323 = EDGE_LOOP ( 'NONE', ( #34424, #14605, #50224, #37504 ) ) ;
#18324 = DIRECTION ( 'NONE',  ( 0.000000000000000000, 0.000000000000000000, 1.000000000000000000 ) ) ;
#18325 = ADVANCED_FACE ( 'NONE', ( #63316 ), #62334, .T. ) ;
#18326 = EDGE_CURVE ( 'NONE', #52979, #64920, #16788, .T. ) ;
#18327 = DIRECTION ( 'NONE',  ( -1.000000000000000000, 0.000000000000000000, 0.000000000000000000 ) ) ;
#18328 = DIRECTION ( 'NONE',  ( -1.000000000000000000, 0.000000000000000000, 0.000000000000000000 ) ) ;
#18329 = VERTEX_POINT ( 'NONE', #27417 ) ;
#18330 = VERTEX_POINT ( 'NONE', #22786 ) ;
#18331 = CARTESIAN_POINT ( 'NONE',  ( 19.56743653832047514, -30.00000000000000000, 5.000000000000000888 ) ) ;
#18332 = EDGE_CURVE ( 'NONE', #21834, #29257, #58854, .T. ) ;
#18333 = ORIENTED_EDGE ( 'NONE', *, *, #37130, .T. ) ;
#18334 = CARTESIAN_POINT ( 'NONE',  ( 10.39889529048551964, 0.7502239413564057990, -13.48021515222736966 ) ) ;
#18335 = ORIENTED_EDGE ( 'NONE', *, *, #27853, .F. ) ;
#18336 = VECTOR ( 'NONE', #42227, 1000.000000000000000 ) ;
#18337 = CARTESIAN_POINT ( 'NONE',  ( 0.2653519991613819129, -4.209134909048826145, 11.50013121838206764 ) ) ;
#18338 = CARTESIAN_POINT ( 'NONE',  ( 0.2653519890518172830, 11.50766430042468969, 4.188437879978292422 ) ) ;
#18339 = CARTESIAN_POINT ( 'NONE',  ( -4.578562111161573078, -30.90741127680607292, -14.86059354493461448 ) ) ;
#18340 = CIRCLE ( 'NONE', #3441, 12.75000000000000178 ) ;
#18342 = AXIS2_PLACEMENT_3D ( 'NONE', #8721, #3760, #49614 ) ;
#18341 = CARTESIAN_POINT ( 'NONE',  ( -22.29018399051993882, 3.609810019245840440, 0.9010028109494814252 ) ) ;
#18344 = EDGE_CURVE ( 'NONE', #53824, #41945, #36096, .T. ) ;
#18343 = DIRECTION ( 'NONE',  ( -1.000000000000000000, 0.000000000000000000, 0.000000000000000000 ) ) ;
#18345 = CARTESIAN_POINT ( 'NONE',  ( -22.38932658256920050, -4.011828264158258328, 0.2254938976656627458 ) ) ;
#18346 = ORIENTED_EDGE ( 'NONE', *, *, #36575, .T. ) ;
#18347 = CARTESIAN_POINT ( 'NONE',  ( 0.3675815128205894289, 10.76447900494940235, 5.910255304480483751 ) ) ;
#18348 = ORIENTED_EDGE ( 'NONE', *, *, #60046, .F. ) ;
#18349 = CARTESIAN_POINT ( 'NONE',  ( -37.00000000000000711, -0.6593684648221369571, 12.73293890771483383 ) ) ;
#18350 = ADVANCED_FACE ( 'NONE', ( #57366 ), #10379, .T. ) ;
#18351 = CARTESIAN_POINT ( 'NONE',  ( 5.536195898058073439, -0.001726268814999772300, 0.008323005098840527416 ) ) ;
#18352 = VERTEX_POINT ( 'NONE', #61257 ) ;
#18353 = DIRECTION ( 'NONE',  ( 0.000000000000000000, -0.3807014730195085739, 0.9246979985058777496 ) ) ;
#18354 = CARTESIAN_POINT ( 'NONE',  ( 0.3057689695767480398, 12.03117299329039369, -2.355923806019077915 ) ) ;
#18355 = CARTESIAN_POINT ( 'NONE',  ( 0.3341166715381371222, -2.378838837789017280, -12.03629799686217616 ) ) ;
#18356 = ORIENTED_EDGE ( 'NONE', *, *, #8257, .T. ) ;
#18357 = VECTOR ( 'NONE', #24585, 1000.000000000000000 ) ;
#18358 = EDGE_LOOP ( 'NONE', ( #22000, #26305, #32908, #56490 ) ) ;
#18359 = DIRECTION ( 'NONE',  ( -1.000000000000000000, 0.000000000000000000, 0.000000000000000000 ) ) ;
#18360 = EDGE_CURVE ( 'NONE', #43566, #27530, #32971, .T. ) ;
#18361 = CIRCLE ( 'NONE', #5592, 5.000000000000001776 ) ;
#18362 = VERTEX_POINT ( 'NONE', #62237 ) ;
#18363 = CARTESIAN_POINT ( 'NONE',  ( 2.000000000000001776, -4.376687952327356079, 5.220963330856582374 ) ) ;
#18364 = DIRECTION ( 'NONE',  ( 0.000000000000000000, 0.01356324068817991828, -0.9999080150203990547 ) ) ;
#18365 = VECTOR ( 'NONE', #47520, 1000.000000000000000 ) ;
#18366 = CARTESIAN_POINT ( 'NONE',  ( 2.241352910868908310, -1.407733736974815963, -7.503490710578247125 ) ) ;
#18367 = CARTESIAN_POINT ( 'NONE',  ( -2.747358470950249654, 5.743717875782093252, 10.56616121202656977 ) ) ;
#18368 = DIRECTION ( 'NONE',  ( 1.000000000000000000, 0.000000000000000000, 0.000000000000000000 ) ) ;
#18369 = EDGE_LOOP ( 'NONE', ( #10233, #47812, #45829, #59900 ) ) ;
#18370 = CARTESIAN_POINT ( 'NONE',  ( 35.00000000000000000, 6.303578524887091916, 10.42955799785312720 ) ) ;
#18371 = CIRCLE ( 'NONE', #28846, 7.938172270156617749 ) ;
#18372 = DIRECTION ( 'NONE',  ( 0.000000000000000000, -0.3807014730195285579, 0.9246979985058696450 ) ) ;
#18373 = LINE ( 'NONE', #2074, #23496 ) ;
#18374 = CARTESIAN_POINT ( 'NONE',  ( -35.00000000000000000, -7.817492529713920391, 9.348667969174380588 ) ) ;
#18375 = DIRECTION ( 'NONE',  ( 0.000000000000000000, -0.1118654143051476951, -0.9937233664769775654 ) ) ;
#18376 = CYLINDRICAL_SURFACE ( 'NONE', #11299, 6.936499999999988120 ) ;
#18377 = CARTESIAN_POINT ( 'NONE',  ( 2.770579946183340248, 5.249166435139440701, -5.784075095088735630 ) ) ;
#18378 = VECTOR ( 'NONE', #37248, 1000.000000000000000 ) ;
#18379 = VECTOR ( 'NONE', #2290, 1000.000000000000000 ) ;
#18380 = CIRCLE ( 'NONE', #11989, 5.000000000000000000 ) ;
#18381 = ADVANCED_FACE ( 'NONE', ( #16685 ), #39689, .T. ) ;
#18382 = VECTOR ( 'NONE', #45590, 1000.000000000000000 ) ;
#18383 = ORIENTED_EDGE ( 'NONE', *, *, #55409, .F. ) ;
#18384 = CARTESIAN_POINT ( 'NONE',  ( 2.258463476536644254, -0.1358786215988691815, 7.638896687393373242 ) ) ;
#18385 = VERTEX_POINT ( 'NONE', #51633 ) ;
#18386 = DIRECTION ( 'NONE',  ( 0.000000000000000000, -0.01356324068818000328, 0.9999080150203990547 ) ) ;
#18387 = LINE ( 'NONE', #58960, #19562 ) ;
#18388 = CARTESIAN_POINT ( 'NONE',  ( 2.941278708680199916, -1.198640839021349436, 6.021511413163959325 ) ) ;
#18389 = AXIS2_PLACEMENT_3D ( 'NONE', #25363, #20379, #60953 ) ;
#18390 = EDGE_LOOP ( 'NONE', ( #26310, #5188, #27225, #37214 ) ) ;
#18391 = CARTESIAN_POINT ( 'NONE',  ( 37.91369172636191820, -26.91879662985438415, -4.500000000000000888 ) ) ;
#18392 = CARTESIAN_POINT ( 'NONE',  ( 2.000000000000001776, 7.414200355365271555, -1.131208685655096691 ) ) ;
#18393 = ORIENTED_EDGE ( 'NONE', *, *, #65660, .T. ) ;
#18394 = AXIS2_PLACEMENT_3D ( 'NONE', #60217, #10323, #30600 ) ;
#18395 = ORIENTED_EDGE ( 'NONE', *, *, #8284, .F. ) ;
#18396 = ORIENTED_EDGE ( 'NONE', *, *, #11777, .F. ) ;
#18397 = CARTESIAN_POINT ( 'NONE',  ( 29.58334585860551513, -8.059223888209368525, 10.83973719671545233 ) ) ;
#18398 = CIRCLE ( 'NONE', #49216, 5.000000000000000000 ) ;
#18399 = CARTESIAN_POINT ( 'NONE',  ( -22.27786964138240222, -3.347945419004157763, -1.536369256421360685 ) ) ;
#18400 = EDGE_CURVE ( 'NONE', #2234, #61618, #60963, .T. ) ;
#18401 = ORIENTED_EDGE ( 'NONE', *, *, #61027, .F. ) ;
#18402 = CARTESIAN_POINT ( 'NONE',  ( -22.27722019094931127, -2.374181302998997101, -2.813874087060012741 ) ) ;
#18403 = CARTESIAN_POINT ( 'NONE',  ( 3.152665057734036491, 7.923639299009025194, 0.4801242025592407647 ) ) ;
#18404 = CARTESIAN_POINT ( 'NONE',  ( 0.2647959493198551173, -9.285851961022009604, 7.983607158780296587 ) ) ;
#18405 = DIRECTION ( 'NONE',  ( 1.000000000000000000, 0.000000000000000000, 0.000000000000000000 ) ) ;
#18406 = ORIENTED_EDGE ( 'NONE', *, *, #11568, .F. ) ;
#18407 = DIRECTION ( 'NONE',  ( 0.000000000000000000, 0.01356324068817998940, -0.9999080150203990547 ) ) ;
#18408 = ADVANCED_FACE ( 'NONE', ( #57261 ), #20369, .T. ) ;
#18409 = VECTOR ( 'NONE', #27305, 1000.000000000000000 ) ;
#18410 = CARTESIAN_POINT ( 'NONE',  ( 12.83306155034139096, -29.03814089300163914, 3.459227852998686625 ) ) ;
#18411 = DIRECTION ( 'NONE',  ( -0.000000000000000000, -1.000000000000000000, -0.000000000000000000 ) ) ;
#18413 = VERTEX_POINT ( 'NONE', #6728 ) ;
#18412 = CARTESIAN_POINT ( 'NONE',  ( 1.452237505248552996, 2.778494755359218971, -12.34692280296789235 ) ) ;
#18414 = CARTESIAN_POINT ( 'NONE',  ( -22.27218376572352554, -3.566922835983774576, -0.9173404081777783992 ) ) ;
#18415 = EDGE_CURVE ( 'NONE', #61311, #8578, #35449, .T. ) ;
#18416 = ORIENTED_EDGE ( 'NONE', *, *, #38692, .T. ) ;
#18417 = CARTESIAN_POINT ( 'NONE',  ( -37.00000000000000711, 0.000000000000000000, 0.000000000000000000 ) ) ;
#18418 = VERTEX_POINT ( 'NONE', #35652 ) ;
#18419 = CARTESIAN_POINT ( 'NONE',  ( 21.90174657591892071, -11.97747433400148864, -0.7349207973210698519 ) ) ;
#18420 = CARTESIAN_POINT ( 'NONE',  ( -22.51237073810381517, 2.023441661740732478, -3.933875531624967170 ) ) ;
#18421 = LINE ( 'NONE', #17752, #34045 ) ;
#18422 = CARTESIAN_POINT ( 'NONE',  ( -35.00000000000000000, 11.72195762423408816, 0.7536123767500589876 ) ) ;
#18423 = AXIS2_PLACEMENT_3D ( 'NONE', #62735, #37476, #7207 ) ;
#18424 = CARTESIAN_POINT ( 'NONE',  ( 0.3164563675027678991, 9.546944054903095278, 7.696930404785069513 ) ) ;
#18425 = CARTESIAN_POINT ( 'NONE',  ( -7.165178994131125023, -1.884899025446307830, -13.36804325434021479 ) ) ;
#18426 = CARTESIAN_POINT ( 'NONE',  ( 12.59797654570207293, 10.92525928803750190, -7.940295129871110191 ) ) ;
#18427 = VERTEX_POINT ( 'NONE', #41290 ) ;
#18428 = CYLINDRICAL_SURFACE ( 'NONE', #5112, 12.18649999999999878 ) ;
#18429 = ORIENTED_EDGE ( 'NONE', *, *, #47239, .T. ) ;
#18430 = EDGE_CURVE ( 'NONE', #35879, #56806, #49309, .T. ) ;
#18431 = EDGE_CURVE ( 'NONE', #45226, #22711, #21346, .T. ) ;
#18432 = CIRCLE ( 'NONE', #49191, 12.73084802173761787 ) ;
#18433 = VERTEX_POINT ( 'NONE', #31334 ) ;
#18435 = CIRCLE ( 'NONE', #33314, 12.18650000000000055 ) ;
#18434 = CARTESIAN_POINT ( 'NONE',  ( 1.000000000000000888, 3.937687286050910895, -6.383151168292444666 ) ) ;
#18436 = CARTESIAN_POINT ( 'NONE',  ( -22.28482751661422867, 3.347211412506322592, 1.587261331312464163 ) ) ;
#18437 = CARTESIAN_POINT ( 'NONE',  ( -27.32337605527168378, 2.771816950947482816, -1.175835497774972982 ) ) ;
#18438 = CARTESIAN_POINT ( 'NONE',  ( 0.3057689695767462079, -10.49983108339464266, 6.328747727191149863 ) ) ;
#18439 = EDGE_CURVE ( 'NONE', #56824, #32709, #11017, .T. ) ;
#18440 = CARTESIAN_POINT ( 'NONE',  ( 5.520433897694421610, -0.005630909886752966977, 0.01397038704729857209 ) ) ;
#18441 = CIRCLE ( 'NONE', #43898, 12.18650000000000233 ) ;
#18442 = CARTESIAN_POINT ( 'NONE',  ( 2.241528039335008771, -7.515727438419991024, -1.341200777944226097 ) ) ;
#18443 = B_SPLINE_CURVE_WITH_KNOTS ( 'NONE', 3,
 ( #1558, #6529, #21832, #36778, #52078, #25485, #47103, #31463, #6205, #62059, #25829, #26158, #42079, #61073, #55760, #10192, #56765, #30472, #235, #15503, #35770, #46121 ),
 .UNSPECIFIED., .F., .F.,
 ( 4, 3, 3, 3, 3, 3, 3, 4 ),
 ( 8.741117365843378158E-19, 4.449119708436879495E-05, 6.626296329540436441E-05, 8.803456484962602063E-05, 0.0001098060367612803520, 0.0001315774408628526981, 0.0001760698110411182686, 0.0001829697163287819926 ),
 .UNSPECIFIED. ) ;
#18444 = CARTESIAN_POINT ( 'NONE',  ( 1.283627346226762889, -11.16434663959575957, -5.810034161408871967 ) ) ;
#18445 = ADVANCED_FACE ( 'NONE', ( #30997 ), #26024, .T. ) ;
#18446 = B_SPLINE_CURVE_WITH_KNOTS ( 'NONE', 3,
 ( #14142, #14779, #34433, #14463, #29133, #9469, #35063 ),
 .UNSPECIFIED., .F., .F.,
 ( 4, 3, 4 ),
 ( 4.722362119209427361E-15, 0.002398160485434635940, 0.005002426799381492345 ),
 .UNSPECIFIED. ) ;
#18447 = ORIENTED_EDGE ( 'NONE', *, *, #10450, .T. ) ;
#18448 = CARTESIAN_POINT ( 'NONE',  ( 35.00000000000000000, -8.927548052240835474, 8.295159312811946961 ) ) ;
#18449 = CIRCLE ( 'NONE', #61941, 12.18650000000000411 ) ;
#18450 = EDGE_CURVE ( 'NONE', #22470, #28861, #16338, .T. ) ;
#18451 = CYLINDRICAL_SURFACE ( 'NONE', #2712, 12.18649999999999878 ) ;
#18452 = FACE_OUTER_BOUND ( 'NONE', #55131, .T. ) ;
#18453 = AXIS2_PLACEMENT_3D ( 'NONE', #45833, #21200, #41471 ) ;
#18454 = CIRCLE ( 'NONE', #56714, 12.73084802173761787 ) ;
#18455 = B_SPLINE_CURVE_WITH_KNOTS ( 'NONE', 3,
 ( #59847, #29556, #3988, #59196, #9596, #43889, #39547, #54852, #13936, #34230, #40187, #44210, #35200, #3689, #24252, #18646, #49864, #54199, #8641 ),
 .UNSPECIFIED., .F., .F.,
 ( 4, 3, 3, 3, 3, 3, 4 ),
 ( 6.023423705678515846E-18, 4.457896483014980128E-05, 6.639290541542210437E-05, 8.820687556479006554E-05, 0.0001100173248778921805, 0.0001545671401658128613, 0.0001830328308068609349 ),
 .UNSPECIFIED. ) ;
#18456 = FACE_OUTER_BOUND ( 'NONE', #34334, .T. ) ;
#18457 = DIRECTION ( 'NONE',  ( 0.000000000000000000, 0.01356324068817998940, -0.9999080150203990547 ) ) ;
#18458 = AXIS2_PLACEMENT_3D ( 'NONE', #38984, #24035, #63930 ) ;
#18459 = CARTESIAN_POINT ( 'NONE',  ( -9.958172265059427986, -3.385416999472194544, 13.06986580931351938 ) ) ;
#18460 = AXIS2_PLACEMENT_3D ( 'NONE', #12341, #32606, #7349 ) ;
#18461 = CARTESIAN_POINT ( 'NONE',  ( -9.811405951060844899, -4.024453971883430903, 12.88726659228943028 ) ) ;
#18462 = ORIENTED_EDGE ( 'NONE', *, *, #19108, .T. ) ;
#18463 = FACE_OUTER_BOUND ( 'NONE', #49802, .T. ) ;
#18464 = DIRECTION ( 'NONE',  ( 0.000000000000000000, -0.01356324068817998940, 0.9999080150203990547 ) ) ;
#18465 = CARTESIAN_POINT ( 'NONE',  ( -35.00000000000000000, 12.09831040184926287, -1.463443770872647542 ) ) ;
#18466 = ADVANCED_FACE ( 'NONE', ( #11054 ), #41626, .T. ) ;
#18467 = CARTESIAN_POINT ( 'NONE',  ( -27.10719052120871098, 0.1538293304135379680, 2.355164825213503121 ) ) ;
#18468 = DIRECTION ( 'NONE',  ( 0.000000000000000000, -0.2149704402110317047, 0.9766205557100849921 ) ) ;
#18469 =( BOUNDED_CURVE ( )  B_SPLINE_CURVE ( 3, ( #18275, #54162, #32871, #7973 ),
 .UNSPECIFIED., .F., .F. ) 
 B_SPLINE_CURVE_WITH_KNOTS ( ( 4, 4 ),
 ( 1.647221706219855974, 1.689073584867815336 ),
 .UNSPECIFIED. ) 
 CURVE ( )  GEOMETRIC_REPRESENTATION_ITEM ( )  RATIONAL_B_SPLINE_CURVE ( ( 1.000000000000000000, 0.9998540403475023597, 0.9998540403475023597, 1.000000000000000000 ) ) 
 REPRESENTATION_ITEM ( '' )  );
#18470 = ORIENTED_EDGE ( 'NONE', *, *, #49161, .F. ) ;
#18471 = DIRECTION ( 'NONE',  ( -1.000000000000000000, 0.000000000000000000, 0.000000000000000000 ) ) ;
#18472 = CARTESIAN_POINT ( 'NONE',  ( 10.48620311856346454, 8.250315036047107142, -8.713914264323181058 ) ) ;
#18473 = CARTESIAN_POINT ( 'NONE',  ( -18.58686583997218378, 5.151216734910788908, -10.83812558286602012 ) ) ;
#18474 = EDGE_LOOP ( 'NONE', ( #28215, #61924, #33250, #19666 ) ) ;
#18475 = DIRECTION ( 'NONE',  ( 0.000000000000000000, -0.9937233664769749009, 0.1118654143051720229 ) ) ;
#18476 = CARTESIAN_POINT ( 'NONE',  ( 0.2648978790185593790, -4.063980959784970537, -11.55204314799267884 ) ) ;
#18477 = ORIENTED_EDGE ( 'NONE', *, *, #65233, .T. ) ;
#18478 = VECTOR ( 'NONE', #58341, 1000.000000000000000 ) ;
#18479 = EDGE_CURVE ( 'NONE', #19210, #26974, #5440, .T. ) ;
#18480 = AXIS2_PLACEMENT_3D ( 'NONE', #47845, #7951, #2303 ) ;
#18481 = EDGE_LOOP ( 'NONE', ( #45950, #12376, #10344, #47444, #52441, #4013 ) ) ;
#18482 = FACE_OUTER_BOUND ( 'NONE', #62592, .T. ) ;
#18483 = CIRCLE ( 'NONE', #38634, 5.000000000000000888 ) ;
#18484 = EDGE_CURVE ( 'NONE', #57324, #47803, #13899, .T. ) ;
#18485 = ORIENTED_EDGE ( 'NONE', *, *, #2264, .F. ) ;
#18486 = CARTESIAN_POINT ( 'NONE',  ( 35.00000000000000000, 0.06441628369836321921, -12.18632975068353019 ) ) ;
#18487 = CARTESIAN_POINT ( 'NONE',  ( -20.92021774235402276, -12.94977746786776684, -3.816457577290517822 ) ) ;
#18488 = CARTESIAN_POINT ( 'NONE',  ( 35.00000000000000000, 8.766823244861988940, -7.817610399097547180 ) ) ;
#18489 = CARTESIAN_POINT ( 'NONE',  ( 1.719304012338833676, 3.626341562670448493, 12.20344780066006152 ) ) ;
#18490 = AXIS2_PLACEMENT_3D ( 'NONE', #381, #4730, #20660 ) ;
#18491 = CIRCLE ( 'NONE', #53522, 5.000000000000000888 ) ;
#18492 = CARTESIAN_POINT ( 'NONE',  ( 1.633930747250414317, 12.16309769563548393, 3.662223193116243891 ) ) ;
#18495 = ORIENTED_EDGE ( 'NONE', *, *, #10098, .F. ) ;
#18494 = CARTESIAN_POINT ( 'NONE',  ( 1.020182472821183683, 7.686484208905105753, 9.854645283129331190 ) ) ;
#18493 = B_SPLINE_CURVE_WITH_KNOTS ( 'NONE', 3,
 ( #42407, #17825, #32445, #42749, #17507, #16832, #28138, #7179, #37778, #12486 ),
 .UNSPECIFIED., .F., .F.,
 ( 4, 2, 2, 2, 4 ),
 ( 0.000000000000000000, 0.002646595623854251962, 0.005293191247708503924, 0.007939786871562756754, 0.01058638249541700785 ),
 .UNSPECIFIED. ) ;
#18496 = PRODUCT_DEFINITION_SHAPE ( 'NONE', 'NONE',  #23030 ) ;
#18497 = FACE_OUTER_BOUND ( 'NONE', #64849, .T. ) ;
#18498 = EDGE_CURVE ( 'NONE', #38388, #7386, #58589, .T. ) ;
#18499 = ORIENTED_EDGE ( 'NONE', *, *, #10886, .F. ) ;
#18500 = CARTESIAN_POINT ( 'NONE',  ( -41.00000000000000711, -1.694065894508600678E-18, 0.000000000000000000 ) ) ;
#18501 = AXIS2_PLACEMENT_3D ( 'NONE', #33145, #53454, #7899 ) ;
#18502 = ORIENTED_EDGE ( 'NONE', *, *, #20340, .T. ) ;
#18503 = ORIENTED_EDGE ( 'NONE', *, *, #42335, .F. ) ;
#18504 = CARTESIAN_POINT ( 'NONE',  ( -16.82301864121118484, 8.090309307062092614, 10.80809437597500100 ) ) ;
#18505 = CARTESIAN_POINT ( 'NONE',  ( -5.261125060311115931, -26.86576352283317703, 15.75274798952654187 ) ) ;
#18506 = CARTESIAN_POINT ( 'NONE',  ( -35.00000000000000000, -8.295159312811792418, -8.927548052240984688 ) ) ;
#18507 = CARTESIAN_POINT ( 'NONE',  ( 2.000000000000001776, 4.915517050588478654, -4.717154614762057108 ) ) ;
#18508 = CARTESIAN_POINT ( 'NONE',  ( 37.00000000000000711, 12.12087942037209842, -1.262958560998807656 ) ) ;
#18509 = CARTESIAN_POINT ( 'NONE',  ( -35.00000000000000000, 0.000000000000000000, 0.000000000000000000 ) ) ;
#18510 = EDGE_LOOP ( 'NONE', ( #24558, #11593, #27506, #46936 ) ) ;
#18511 = CARTESIAN_POINT ( 'NONE',  ( -22.27715526084302056, 0.4651416883073989927, 3.652257391294490230 ) ) ;
#18512 = DIRECTION ( 'NONE',  ( 0.000000000000000000, 0.01356324068817998940, -0.9999080150203990547 ) ) ;
#18513 = DIRECTION ( 'NONE',  ( -1.000000000000000000, -0.000000000000000000, 0.000000000000000000 ) ) ;
#18514 = VECTOR ( 'NONE', #19809, 1000.000000000000000 ) ;
#18515 = ORIENTED_EDGE ( 'NONE', *, *, #54412, .F. ) ;
#18516 = CARTESIAN_POINT ( 'NONE',  ( -35.00000000000000000, 0.000000000000000000, 0.000000000000000000 ) ) ;
#18517 = VERTEX_POINT ( 'NONE', #27309 ) ;
#18518 = CARTESIAN_POINT ( 'NONE',  ( 2.241451721903216399, -1.385577012535806229, 7.507681056655371776 ) ) ;
#18519 = CARTESIAN_POINT ( 'NONE',  ( 0.3002738374340788163, -10.50101454678641133, -6.323236184341234356 ) ) ;
#18520 = CARTESIAN_POINT ( 'NONE',  ( 35.00000000000000000, -0.9416912585475287756, -12.71517666308947625 ) ) ;
#18521 = EDGE_CURVE ( 'NONE', #5898, #35815, #37257, .T. ) ;
#18522 = CARTESIAN_POINT ( 'NONE',  ( -22.29479313954897890, 3.090162644873547748, -2.096782908204888773 ) ) ;
#18523 = DIRECTION ( 'NONE',  ( 0.000000000000000000, 0.01356324068817992175, -0.9999080150203990547 ) ) ;
#18524 = CARTESIAN_POINT ( 'NONE',  ( -27.08456565417852602, -1.867985369022540976, 1.328664661355674736 ) ) ;
#18525 = CIRCLE ( 'NONE', #31266, 12.75000000000000178 ) ;
#18526 = EDGE_CURVE ( 'NONE', #40488, #14909, #44704, .T. ) ;
#18527 = CARTESIAN_POINT ( 'NONE',  ( -8.891032880924177206, 12.93614229090409395, -3.860857758255646921 ) ) ;
#18528 = ORIENTED_EDGE ( 'NONE', *, *, #63618, .T. ) ;
#18529 = ORIENTED_EDGE ( 'NONE', *, *, #28088, .T. ) ;
#18530 = EDGE_CURVE ( 'NONE', #11089, #44680, #13892, .T. ) ;
#18531 = CARTESIAN_POINT ( 'NONE',  ( 1.109979610369598912, 3.830786822173106732, 11.92772269523320716 ) ) ;
#18532 = AXIS2_PLACEMENT_3D ( 'NONE', #23871, #9195, #23532 ) ;
#18533 = CARTESIAN_POINT ( 'NONE',  ( 37.00000000000000711, 4.705694406421931860E-17, -3.469127814946512892E-15 ) ) ;
#18534 = AXIS2_PLACEMENT_3D ( 'NONE', #2261, #16235, #41158 ) ;
#18535 = CARTESIAN_POINT ( 'NONE',  ( -10.64440273086533040, -9.782391350870078384, 6.950960968970282927 ) ) ;
#18536 = ORIENTED_EDGE ( 'NONE', *, *, #1398, .F. ) ;
#18537 = CYLINDRICAL_SURFACE ( 'NONE', #2442, 12.18650000000000055 ) ;
#18538 = CARTESIAN_POINT ( 'NONE',  ( -10.41759788416483623, -5.099336898890864056, -10.86981208156591094 ) ) ;
#18539 = CARTESIAN_POINT ( 'NONE',  ( 9.883938789068938746, 7.802108911151313997, 9.123879608504731564 ) ) ;
#18540 = FACE_OUTER_BOUND ( 'NONE', #50210, .T. ) ;
#18541 = DIRECTION ( 'NONE',  ( -0.2034311943119418153, 0.9790892447477997917, 0.000000000000000000 ) ) ;
#18542 = ORIENTED_EDGE ( 'NONE', *, *, #2660, .T. ) ;
#18543 = AXIS2_PLACEMENT_3D ( 'NONE', #23084, #32694, #43344 ) ;
#18544 = DIRECTION ( 'NONE',  ( 1.000000000000000000, -0.000000000000000000, -0.000000000000000000 ) ) ;
#18545 = CARTESIAN_POINT ( 'NONE',  ( 2.941278708680199916, -5.814102272488603340, 1.972702289975983625 ) ) ;
#18546 = CARTESIAN_POINT ( 'NONE',  ( 3.152665057735933640, -5.461013642407022139, -5.761241965768077122 ) ) ;
#18547 = DIRECTION ( 'NONE',  ( -1.000000000000000000, 0.000000000000000000, 0.000000000000000000 ) ) ;
#18548 = CIRCLE ( 'NONE', #23853, 12.18649999999999878 ) ;
#18549 = EDGE_CURVE ( 'NONE', #43866, #18956, #47939, .T. ) ;
#18550 = DIRECTION ( 'NONE',  ( 0.000000000000000000, 0.000000000000000000, 1.000000000000000000 ) ) ;
#18551 = EDGE_CURVE ( 'NONE', #36349, #19607, #15985, .T. ) ;
#18552 = CARTESIAN_POINT ( 'NONE',  ( 2.249013661412228693, -5.926694833810643992, 4.816366775941328449 ) ) ;
#18553 = VERTEX_POINT ( 'NONE', #43256 ) ;
#18554 = CARTESIAN_POINT ( 'NONE',  ( 2.280717697723835702, -2.468022724683509583, 7.238333660707031214 ) ) ;
#18556 = AXIS2_PLACEMENT_3D ( 'NONE', #62204, #16658, #26095 ) ;
#18555 = CARTESIAN_POINT ( 'NONE',  ( 29.52239426923290466, 11.14864943672236564, 7.625421059268382429 ) ) ;
#18557 = CARTESIAN_POINT ( 'NONE',  ( 4.286683309450310730, -28.06227586351231196, -12.00609810331033067 ) ) ;
#18558 = ORIENTED_EDGE ( 'NONE', *, *, #46981, .T. ) ;
#18559 = CARTESIAN_POINT ( 'NONE',  ( -11.34436572679164712, -8.403365156751931409, -8.571542621278755547 ) ) ;
#18560 = CARTESIAN_POINT ( 'NONE',  ( -47.00000000000000711, 0.000000000000000000, 0.000000000000000000 ) ) ;
#18561 = CARTESIAN_POINT ( 'NONE',  ( 3.152665057734128862, 5.461013642405629476, -5.761241965769021256 ) ) ;
#18562 = ADVANCED_FACE ( 'NONE', ( #37947 ), #2398, .T. ) ;
#18563 = LINE ( 'NONE', #23527, #34921 ) ;
#18564 = CARTESIAN_POINT ( 'NONE',  ( 2.903928887688111526, 8.044738195289742322, -3.491800274468887189 ) ) ;
#18565 = AXIS2_PLACEMENT_3D ( 'NONE', #41548, #26272, #46549 ) ;
#18566 = DIRECTION ( 'NONE',  ( -1.000000000000000000, 0.000000000000000000, 0.000000000000000000 ) ) ;
#18567 = VERTEX_POINT ( 'NONE', #32946 ) ;
#18568 = FACE_OUTER_BOUND ( 'NONE', #48951, .T. ) ;
#18569 = CARTESIAN_POINT ( 'NONE',  ( 1.937114397841932290, -3.111612666690160456, 12.45230409340480371 ) ) ;
#18570 = CARTESIAN_POINT ( 'NONE',  ( 2.639814597422737386, 7.382549681340947245, -2.414168779979510848 ) ) ;
#18571 = DIRECTION ( 'NONE',  ( -1.000000000000000000, 0.000000000000000000, 0.000000000000000000 ) ) ;
#18572 = CARTESIAN_POINT ( 'NONE',  ( 0.000000000000000000, 0.000000000000000000, 0.000000000000000000 ) ) ;
#18573 = CARTESIAN_POINT ( 'NONE',  ( 15.69195845145067381, -33.00000000000000000, -4.009712365929972044 ) ) ;
#18574 = CARTESIAN_POINT ( 'NONE',  ( 2.241352910868908754, 7.532448145350508995, 1.243507963608119438 ) ) ;
#18575 = CARTESIAN_POINT ( 'NONE',  ( -17.29244623348158783, 2.525873743887551814, -13.26159725786978072 ) ) ;
#18576 = EDGE_LOOP ( 'NONE', ( #64451, #55677, #58964, #3175 ) ) ;
#18577 = ADVANCED_FACE ( 'NONE', ( #38614 ), #42917, .F. ) ;
#18578 = VECTOR ( 'NONE', #60011, 1000.000000000000000 ) ;
#18579 = ORIENTED_EDGE ( 'NONE', *, *, #65182, .F. ) ;
#18580 = DIRECTION ( 'NONE',  ( 0.000000000000000000, -0.9847383929261634972, 0.1740410799127515284 ) ) ;
#18581 = ORIENTED_EDGE ( 'NONE', *, *, #54044, .F. ) ;
#18582 = EDGE_CURVE ( 'NONE', #57580, #7123, #40433, .T. ) ;
#18583 = FACE_OUTER_BOUND ( 'NONE', #41924, .T. ) ;
#18584 = DIRECTION ( 'NONE',  ( -0.000000000000000000, -0.000000000000000000, -1.000000000000000000 ) ) ;
#18585 = LINE ( 'NONE', #58473, #60620 ) ;
#18586 = EDGE_LOOP ( 'NONE', ( #964, #31883, #16169, #41199 ) ) ;
#18587 = CARTESIAN_POINT ( 'NONE',  ( -37.00000000000000711, 0.000000000000000000, 0.000000000000000000 ) ) ;
#18588 = CIRCLE ( 'NONE', #50419, 12.18649999999999878 ) ;
#18589 = DIRECTION ( 'NONE',  ( 0.000000000000000000, 0.5243256840888502746, 0.8515178078024904229 ) ) ;
#18590 = CARTESIAN_POINT ( 'NONE',  ( 2.305787727787084407, -5.047606869483016290, -5.756228004061508585 ) ) ;
#18591 = VERTEX_POINT ( 'NONE', #37289 ) ;
#18592 = EDGE_LOOP ( 'NONE', ( #32605, #31249, #37165, #211 ) ) ;
#18593 = DIRECTION ( 'NONE',  ( 0.000000000000000000, 0.07632122047556495759, -0.9970832820307038435 ) ) ;
#18594 = CONICAL_SURFACE ( 'NONE', #47254, 7.938172270156617749, 1.280189991382167047 ) ;
#18595 = DIRECTION ( 'NONE',  ( 0.000000000000000000, 0.01356324068817998940, -0.9999080150203990547 ) ) ;
#18596 = EDGE_LOOP ( 'NONE', ( #46623, #53788, #39403, #23222 ) ) ;
#18597 = ORIENTED_EDGE ( 'NONE', *, *, #36575, .F. ) ;
#18598 = CARTESIAN_POINT ( 'NONE',  ( 35.00000000000000000, 11.73555825188276280, -4.983891302653623789 ) ) ;
#18599 = EDGE_CURVE ( 'NONE', #60970, #4245, #23659, .T. ) ;
#18600 = AXIS2_PLACEMENT_3D ( 'NONE', #53803, #13536, #54117 ) ;
#18601 = DIRECTION ( 'NONE',  ( 0.000000000000000000, -0.01356324068817991828, 0.9999080150203990547 ) ) ;
#18602 = CARTESIAN_POINT ( 'NONE',  ( 0.2671309869109501078, 10.52409658627924571, -6.263183022891068319 ) ) ;
#18603 = DIRECTION ( 'NONE',  ( -1.000000000000000000, 0.000000000000000000, 0.000000000000000000 ) ) ;
#18604 = CARTESIAN_POINT ( 'NONE',  ( 0.9232058338315058954, -5.905985151448226667, 10.98407661738926677 ) ) ;
#18605 = ADVANCED_FACE ( 'NONE', ( #24964 ), #34271, .T. ) ;
#18606 = DIRECTION ( 'NONE',  ( 0.000000000000000000, 0.000000000000000000, 1.000000000000000000 ) ) ;
#18607 = EDGE_LOOP ( 'NONE', ( #27241, #3714, #57566, #2394 ) ) ;
#18608 = CARTESIAN_POINT ( 'NONE',  ( 2.247206125382828379, -1.439877054338154050, 7.499376972323892332 ) ) ;
#18609 = CARTESIAN_POINT ( 'NONE',  ( 0.2653141334712560973, 7.837911425448908176, -9.409392642815664232 ) ) ;
#18610 = CARTESIAN_POINT ( 'NONE',  ( 0.2653519890538382775, -0.02202236966336145602, 12.24619734961521544 ) ) ;
#18611 = DIRECTION ( 'NONE',  ( -1.000000000000000000, 0.000000000000000000, 0.000000000000000000 ) ) ;
#18612 = DIRECTION ( 'NONE',  ( 0.000000000000000000, -0.01356324068817998940, 0.9999080150203990547 ) ) ;
#18613 = CARTESIAN_POINT ( 'NONE',  ( 23.12239576763279914, 2.549905108198637915, 13.26000697717500643 ) ) ;
#18614 = DIRECTION ( 'NONE',  ( 0.000000000000000000, 0.01356324068817991481, -0.9999080150203990547 ) ) ;
#18615 = CARTESIAN_POINT ( 'NONE',  ( 0.000000000000000000, 0.000000000000000000, 0.000000000000000000 ) ) ;
#18616 = CARTESIAN_POINT ( 'NONE',  ( -35.00000000000000000, 0.000000000000000000, 0.000000000000000000 ) ) ;
#18617 = ORIENTED_EDGE ( 'NONE', *, *, #28579, .T. ) ;
#18618 = CARTESIAN_POINT ( 'NONE',  ( -35.00000000000000000, -7.608228585767649044, -10.23119532541080901 ) ) ;
#18619 = EDGE_CURVE ( 'NONE', #20061, #58290, #7549, .T. ) ;
#18620 = ORIENTED_EDGE ( 'NONE', *, *, #22215, .F. ) ;
#18621 = CARTESIAN_POINT ( 'NONE',  ( 37.00000000000000711, 8.551552972817191289, 8.052525312709789773 ) ) ;
#18622 = FACE_OUTER_BOUND ( 'NONE', #55861, .T. ) ;
#18623 = CARTESIAN_POINT ( 'NONE',  ( 11.74548640120467979, -10.73597826697111124, -8.184666801472349817 ) ) ;
#18624 = CARTESIAN_POINT ( 'NONE',  ( 3.459614771489464946, -11.09853614738469396, -4.563167253695070258 ) ) ;
#18625 = DIRECTION ( 'NONE',  ( 0.000000000000000000, -0.01356324068817992175, 0.9999080150203990547 ) ) ;
#18626 = ORIENTED_EDGE ( 'NONE', *, *, #14413, .T. ) ;
#18627 = CARTESIAN_POINT ( 'NONE',  ( 1.719304012341273724, 0.7661785589598685275, -12.70777170743938456 ) ) ;
#18628 = DIRECTION ( 'NONE',  ( -1.000000000000000000, 0.000000000000000000, 0.000000000000000000 ) ) ;
#18629 = DIRECTION ( 'NONE',  ( -1.000000000000000000, 0.000000000000000000, 0.000000000000000000 ) ) ;
#18630 = CARTESIAN_POINT ( 'NONE',  ( -22.29570301036918778, 2.696988360630619752, 2.586939527522273963 ) ) ;
#18631 = ADVANCED_FACE ( 'NONE', ( #54582 ), #34590, .T. ) ;
#18632 = CARTESIAN_POINT ( 'NONE',  ( -35.00000000000000000, -0.1652884326465054732, 12.18537902504609249 ) ) ;
#18633 = VERTEX_POINT ( 'NONE', #65187 ) ;
#18634 = DIRECTION ( 'NONE',  ( 0.000000000000000000, -0.6051742151937715697, 0.7960930657056388693 ) ) ;
#18635 = ORIENTED_EDGE ( 'NONE', *, *, #9673, .F. ) ;
#18636 = CARTESIAN_POINT ( 'NONE',  ( 2.524535260911804802, 5.776056274541051749, -5.135322114975449104 ) ) ;
#18637 = CARTESIAN_POINT ( 'NONE',  ( 3.618571554686976999, 8.318316264554045603, -8.649151353875886628 ) ) ;
#18638 = CARTESIAN_POINT ( 'NONE',  ( 6.463891187881699807, -7.979741258536692250, 10.89069007513759324 ) ) ;
#18639 = CIRCLE ( 'NONE', #40880, 12.18650000000000411 ) ;
#18640 = EDGE_CURVE ( 'NONE', #7150, #18591, #16038, .T. ) ;
#18641 = EDGE_LOOP ( 'NONE', ( #57147, #47993, #11922, #18393 ) ) ;
#18642 = ORIENTED_EDGE ( 'NONE', *, *, #45563, .T. ) ;
#18643 = CYLINDRICAL_SURFACE ( 'NONE', #46716, 12.74999999999999822 ) ;
#18644 = CARTESIAN_POINT ( 'NONE',  ( -27.27855387000350262, 25.00000000000000000, 5.631341004100471892 ) ) ;
#18645 = DIRECTION ( 'NONE',  ( 1.000000000000000000, 0.000000000000000000, 0.000000000000000000 ) ) ;
#18646 = CARTESIAN_POINT ( 'NONE',  ( 0.2676618633000457659, 12.24591287309139354, 0.1607051348608056485 ) ) ;
#18647 = CARTESIAN_POINT ( 'NONE',  ( 0.3109076770649061849, 9.239379580302207629, -8.060731492642700502 ) ) ;
#18648 = CARTESIAN_POINT ( 'NONE',  ( -22.28350523959500862, -2.107889123925585473, -3.041489826385515904 ) ) ;
#18649 = EDGE_LOOP ( 'NONE', ( #10336, #33586, #27253, #48587 ) ) ;
#18650 = EDGE_CURVE ( 'NONE', #6128, #42485, #39398, .T. ) ;
#18651 = VERTEX_POINT ( 'NONE', #9639 ) ;
#18652 = ORIENTED_EDGE ( 'NONE', *, *, #3925, .F. ) ;
#18653 = CYLINDRICAL_SURFACE ( 'NONE', #26644, 12.18650000000000055 ) ;
#18654 = EDGE_CURVE ( 'NONE', #45219, #7826, #10730, .T. ) ;
#18655 = CIRCLE ( 'NONE', #45208, 12.18649999999999878 ) ;
#18656 = CARTESIAN_POINT ( 'NONE',  ( 37.00000000000000711, -8.839356091080105671, -8.389074212634254124 ) ) ;
#18657 = ORIENTED_EDGE ( 'NONE', *, *, #46988, .T. ) ;
#18658 = CARTESIAN_POINT ( 'NONE',  ( 2.305787727787085295, -3.971363876084009537, 6.545285700970515208 ) ) ;
#18659 = CARTESIAN_POINT ( 'NONE',  ( 2.261269890822073414, -7.547924622047981202, 1.189259211195918375 ) ) ;
#18660 = VERTEX_POINT ( 'NONE', #13982 ) ;
#18661 =( BOUNDED_SURFACE ( )  B_SPLINE_SURFACE ( 3, 1, ( 
 ( #21535, #6572 ),
 ( #11223, #51142 ),
 ( #51796, #16208 ),
 ( #62396, #36489 ) ),
 .UNSPECIFIED., .F., .F., .F. ) 
 B_SPLINE_SURFACE_WITH_KNOTS ( ( 4, 4 ),
 ( 2, 2 ),
 ( 0.000000000000000000, 1.000000000000000000 ),
 ( 0.000000000000000000, 1.000000000000000000 ),
 .UNSPECIFIED. ) 
 GEOMETRIC_REPRESENTATION_ITEM ( )  RATIONAL_B_SPLINE_SURFACE ( (
 ( 1.000000000000000000, 1.000000000000000000),
 ( 0.6933888150995267674, 0.9895912004443193632),
 ( 0.6933888150995267674, 0.9895912004443193632),
 ( 1.000000000000000000, 1.000000000000000000) ) ) 
 REPRESENTATION_ITEM ( '' )  SURFACE ( )  );
#18662 = CARTESIAN_POINT ( 'NONE',  ( 2.241451721903215955, 6.641849090085004903, -3.764430789729908522 ) ) ;
#18663 = CARTESIAN_POINT ( 'NONE',  ( 2.251152103363646795, -2.729599998984361786, -7.133254101175212192 ) ) ;
#18664 = LINE ( 'NONE', #7681, #14377 ) ;
#18665 = ORIENTED_EDGE ( 'NONE', *, *, #13597, .T. ) ;
#18666 = ORIENTED_EDGE ( 'NONE', *, *, #17993, .F. ) ;
#18667 = CARTESIAN_POINT ( 'NONE',  ( 35.00000000000000000, -10.25474254703957477, -6.584150480049516752 ) ) ;
#18668 = VERTEX_POINT ( 'NONE', #35242 ) ;
#18669 = PRODUCT_DEFINITION_FORMATION_WITH_SPECIFIED_SOURCE ( 'ANY', '', #49305, .NOT_KNOWN. ) ;
#18670 = CARTESIAN_POINT ( 'NONE',  ( 8.555539599251753557, 3.416301611567257979, -13.06349654673114991 ) ) ;
#18671 = EDGE_LOOP ( 'NONE', ( #4340, #50209, #14950, #60090 ) ) ;
#18672 = ORIENTED_EDGE ( 'NONE', *, *, #16582, .T. ) ;
#18673 = CARTESIAN_POINT ( 'NONE',  ( 2.665405856346775071, 7.686816759402975485, -5.696318245876773823 ) ) ;
#18674 = DIRECTION ( 'NONE',  ( -1.000000000000000000, -0.000000000000000000, 0.000000000000000000 ) ) ;
#18675 = EDGE_CURVE ( 'NONE', #18204, #28784, #59581, .T. ) ;
#18676 = DIRECTION ( 'NONE',  ( -1.000000000000000000, 0.000000000000000000, 0.000000000000000000 ) ) ;
#18677 = CARTESIAN_POINT ( 'NONE',  ( -22.27706089016750113, 3.548384797797536905, 0.9798385173595970388 ) ) ;
#18678 = CARTESIAN_POINT ( 'NONE',  ( 35.00000000000000000, 10.91536515067648239, 4.339012074899986970 ) ) ;
#18679 = CARTESIAN_POINT ( 'NONE',  ( 1.287602823386882367, -0.5522659225150480244, 12.57487505104553804 ) ) ;
#18680 = ORIENTED_EDGE ( 'NONE', *, *, #36780, .F. ) ;
#18681 = DIRECTION ( 'NONE',  ( 0.000000000000000000, 0.01356324068817998940, -0.9999080150203989437 ) ) ;
#18682 = AXIS2_PLACEMENT_3D ( 'NONE', #4948, #51159, #20565 ) ;
#18683 = ORIENTED_EDGE ( 'NONE', *, *, #29388, .T. ) ;
#18684 = FACE_OUTER_BOUND ( 'NONE', #53303, .T. ) ;
#18685 = CARTESIAN_POINT ( 'NONE',  ( 20.00005080000000035, 4.898587196589412829E-16, -4.000000000000000000 ) ) ;
#18686 = ORIENTED_EDGE ( 'NONE', *, *, #57346, .F. ) ;
#18687 = CARTESIAN_POINT ( 'NONE',  ( 0.3401186441510235525, -10.75260364139049329, 5.912862694513676409 ) ) ;
#18688 = DIRECTION ( 'NONE',  ( 0.000000000000000000, -0.01356324068817999114, 0.9999080150203989437 ) ) ;
#18689 = CARTESIAN_POINT ( 'NONE',  ( 2.491965175173618707, -7.560994562509134376, 1.548529392253887416 ) ) ;
#18690 = AXIS2_PLACEMENT_3D ( 'NONE', #43909, #8988, #17667 ) ;
#18692 = ADVANCED_FACE ( 'NONE', ( #43935 ), #64213, .T. ) ;
#18691 = ORIENTED_EDGE ( 'NONE', *, *, #48633, .F. ) ;
#18693 = ORIENTED_EDGE ( 'NONE', *, *, #43768, .T. ) ;
#18694 = DIRECTION ( 'NONE',  ( 1.000000000000000000, 0.000000000000000000, -0.000000000000000000 ) ) ;
#18695 = ORIENTED_EDGE ( 'NONE', *, *, #60555, .F. ) ;
#18696 = PLANE ( 'NONE',  #15782 ) ;
#18697 = DIRECTION ( 'NONE',  ( -1.000000000000000000, -0.000000000000000000, -0.000000000000000000 ) ) ;
#18698 = DIRECTION ( 'NONE',  ( 0.9947400562552481951, -0.1024315404614497965, 0.000000000000000000 ) ) ;
#18699 = CARTESIAN_POINT ( 'NONE',  ( 1.194176325881340039, -9.279760592562150023, 8.457794872459091451 ) ) ;
#18700 = ORIENTED_EDGE ( 'NONE', *, *, #50509, .T. ) ;
#18701 = DIRECTION ( 'NONE',  ( 1.000000000000000000, 0.000000000000000000, -0.000000000000000000 ) ) ;
#18702 = DIRECTION ( 'NONE',  ( 0.000000000000000000, 0.000000000000000000, 1.000000000000000000 ) ) ;
#18703 = B_SPLINE_CURVE_WITH_KNOTS ( 'NONE', 3,
 ( #8030, #28297, #13642, #43569, #63853, #18337, #38602, #58915, #13328, #28614, #32597, #64202, #23645 ),
 .UNSPECIFIED., .F., .F.,
 ( 4, 3, 3, 3, 4 ),
 ( 3.878959614448864246E-18, 6.607593386745498512E-05, 0.0001321518677373512412, 0.0001982171734706196671, 0.0002642860854759480666 ),
 .UNSPECIFIED. ) ;
#18704 = EDGE_CURVE ( 'NONE', #10069, #62776, #24491, .T. ) ;
#18705 = CARTESIAN_POINT ( 'NONE',  ( 2.373367633546871858, -7.528269033630144769, -1.511052049479995718 ) ) ;
#18706 = DIRECTION ( 'NONE',  ( -1.000000000000000000, 0.000000000000000000, 0.000000000000000000 ) ) ;
#18707 = EDGE_CURVE ( 'NONE', #62820, #27619, #20272, .T. ) ;
#18708 = CYLINDRICAL_SURFACE ( 'NONE', #38359, 6.936499999999988120 ) ;
#18709 = CARTESIAN_POINT ( 'NONE',  ( 5.126543808314632855, -10.38684015690950169, -6.021752670102713978 ) ) ;
#18710 = LINE ( 'NONE', #54276, #5710 ) ;
#18711 = ADVANCED_FACE ( 'NONE', ( #59889 ), #14311, .T. ) ;
#18712 = CIRCLE ( 'NONE', #28243, 4.999999999999999112 ) ;
#18713 = VERTEX_POINT ( 'NONE', #44905 ) ;
#18714 = CARTESIAN_POINT ( 'NONE',  ( -26.74023318801843629, 1.425982498898183071, 3.035730054944064005 ) ) ;
#18715 = VECTOR ( 'NONE', #23771, 1000.000000000000114 ) ;
#18716 = ORIENTED_EDGE ( 'NONE', *, *, #26056, .T. ) ;
#18717 = CYLINDRICAL_SURFACE ( 'NONE', #21465, 6.936499999999988120 ) ;
#18718 = CARTESIAN_POINT ( 'NONE',  ( -22.27709082389155171, -3.569727173833824985, 0.8996430462092213087 ) ) ;
#18719 = DIRECTION ( 'NONE',  ( 1.000000000000000000, 0.000000000000000000, 0.000000000000000000 ) ) ;
#18720 = CARTESIAN_POINT ( 'NONE',  ( 0.2653519991613825790, -12.24619736885323995, -0.02201648635055044115 ) ) ;
#18721 = ORIENTED_EDGE ( 'NONE', *, *, #7329, .T. ) ;
#18722 = ORIENTED_EDGE ( 'NONE', *, *, #45207, .T. ) ;
#18723 = ORIENTED_EDGE ( 'NONE', *, *, #61672, .T. ) ;
#18724 = DIRECTION ( 'NONE',  ( 0.000000000000000000, -0.4134677391718386552, -0.9105187689796012673 ) ) ;
#18725 = AXIS2_PLACEMENT_3D ( 'NONE', #45305, #45970, #39983 ) ;
#18726 = EDGE_LOOP ( 'NONE', ( #13618, #30551, #463, #44069 ) ) ;
#18727 = ADVANCED_FACE ( 'NONE', ( #12769 ), #64616, .T. ) ;
#18728 = CARTESIAN_POINT ( 'NONE',  ( 2.440552418640495880, 5.770332237304444334, 5.099602138956223385 ) ) ;
#18729 = CARTESIAN_POINT ( 'NONE',  ( 0.2851083653049504285, -0.4107471485392698018, 13.49374991542258151 ) ) ;
#18730 = CARTESIAN_POINT ( 'NONE',  ( 5.515188684475870851, -0.0005703990286340425908, 0.005320786921497679470 ) ) ;
#18731 = CARTESIAN_POINT ( 'NONE',  ( -35.00000000000000000, 4.824807283154122217, 11.80185301892982430 ) ) ;
#18732 = VERTEX_POINT ( 'NONE', #19089 ) ;
#18733 = LINE ( 'NONE', #54641, #186 ) ;
#18734 = CARTESIAN_POINT ( 'NONE',  ( 15.45515798858408907, -34.86679772354910511, 6.222782430144768284 ) ) ;
#18735 = CARTESIAN_POINT ( 'NONE',  ( -37.00000000000000711, -11.29812557209474733, -3.213188559034363401 ) ) ;
#18737 = VERTEX_POINT ( 'NONE', #54012 ) ;
#18736 = CARTESIAN_POINT ( 'NONE',  ( 2.000000000000001776, 0.000000000000000000, 0.000000000000000000 ) ) ;
#18738 = CARTESIAN_POINT ( 'NONE',  ( -35.04709527796842394, 0.005220632201000108275, 0.01120703303051501232 ) ) ;
#18739 = VERTEX_POINT ( 'NONE', #38381 ) ;
#18740 = CARTESIAN_POINT ( 'NONE',  ( 35.00000000000000000, -11.61175578952786758, -1.771820996347120092 ) ) ;
#18741 = ORIENTED_EDGE ( 'NONE', *, *, #42771, .T. ) ;
#18742 = CARTESIAN_POINT ( 'NONE',  ( 0.000000000000000000, -6.812627895098285258, -0.04423456934733380197 ) ) ;
#18743 = DIRECTION ( 'NONE',  ( -1.000000000000000000, -0.000000000000000000, -0.000000000000000000 ) ) ;
#18744 = LINE ( 'NONE', #54317, #9592 ) ;
#18745 = CARTESIAN_POINT ( 'NONE',  ( -35.00000000000000000, -5.556331110570326359, -11.47561260193582733 ) ) ;
#18746 = DIRECTION ( 'NONE',  ( -1.000000000000000000, 0.000000000000000000, 0.000000000000000000 ) ) ;
#18747 = LINE ( 'NONE', #39004, #4907 ) ;
#18748 = CARTESIAN_POINT ( 'NONE',  ( -32.00000000000000000, 5.510910596163098430E-16, 0.000000000000000000 ) ) ;
#18749 = ORIENTED_EDGE ( 'NONE', *, *, #8083, .F. ) ;
#18750 = CARTESIAN_POINT ( 'NONE',  ( -4.979815405451806676, -1.249695498034863350, 13.44307378499100913 ) ) ;
#18751 = VERTEX_POINT ( 'NONE', #8454 ) ;
#18752 = VERTEX_POINT ( 'NONE', #9106 ) ;
#18753 = CARTESIAN_POINT ( 'NONE',  ( 0.2648978790185619880, -9.295532325666501450, 7.972372351882998309 ) ) ;
#18754 = CARTESIAN_POINT ( 'NONE',  ( -17.61421642177270996, -11.57952024119405721, 3.221331910940534726 ) ) ;
#18755 = DIRECTION ( 'NONE',  ( 0.000000000000000000, 0.01356324068817991828, -0.9999080150203990547 ) ) ;
#18756 = CARTESIAN_POINT ( 'NONE',  ( -22.27706485742869091, 0.9221835209182547288, 3.563814065926663499 ) ) ;
#18757 = CARTESIAN_POINT ( 'NONE',  ( 3.152665057734040488, 0.000000000000000000, 0.000000000000000000 ) ) ;
#18758 = EDGE_CURVE ( 'NONE', #5369, #20748, #4125, .T. ) ;
#18759 = CARTESIAN_POINT ( 'NONE',  ( 0.3160775863651080764, 10.73821170199163078, -5.922381034681481360 ) ) ;
#18760 = VECTOR ( 'NONE', #37681, 1000.000000000000000 ) ;
#18761 = CARTESIAN_POINT ( 'NONE',  ( -11.40165637463000436, -7.508992741355388745, -9.360289953322599388 ) ) ;
#18762 = AXIS2_PLACEMENT_3D ( 'NONE', #55579, #34928, #45583 ) ;
#18763 = ORIENTED_EDGE ( 'NONE', *, *, #27584, .T. ) ;
#18764 = CARTESIAN_POINT ( 'NONE',  ( 2.827825597296807825, -6.550135365664038645, -6.207590800588439706 ) ) ;
#18765 = CARTESIAN_POINT ( 'NONE',  ( 2.245754705088395475, -5.777230445738506859, -4.993005209687642498 ) ) ;
#18766 = CARTESIAN_POINT ( 'NONE',  ( 19.28625800530496903, 25.00000000000000000, 11.87904264843580471 ) ) ;
#18767 = EDGE_CURVE ( 'NONE', #11975, #6620, #4346, .T. ) ;
#18768 = CARTESIAN_POINT ( 'NONE',  ( -11.39386375410057539, -7.136722497414110578, 11.46148400915446075 ) ) ;
#18769 = EDGE_CURVE ( 'NONE', #5130, #33557, #7812, .T. ) ;
#18770 = CARTESIAN_POINT ( 'NONE',  ( 11.32119323119160548, 0.8088561146804297275, -11.97325730400089050 ) ) ;
#18771 = ADVANCED_FACE ( 'NONE', ( #18463 ), #3826, .T. ) ;
#18772 = VERTEX_POINT ( 'NONE', #14088 ) ;
#18773 = CYLINDRICAL_SURFACE ( 'NONE', #14942, 12.75000000000000178 ) ;
#18774 = DIRECTION ( 'NONE',  ( 1.000000000000000000, 0.000000000000000000, 0.000000000000000000 ) ) ;
#18775 = CARTESIAN_POINT ( 'NONE',  ( 3.409665710615477963, 3.588105730534572047, 11.45304521538101739 ) ) ;
#18776 = EDGE_CURVE ( 'NONE', #21758, #19892, #1163, .T. ) ;
#18777 = FACE_OUTER_BOUND ( 'NONE', #35506, .T. ) ;
#18778 = DIRECTION ( 'NONE',  ( -1.000000000000000000, 0.000000000000000000, 0.000000000000000000 ) ) ;
#18779 = VERTEX_POINT ( 'NONE', #23421 ) ;
#18780 = CARTESIAN_POINT ( 'NONE',  ( 5.514970785353741078, 0.002093325033903811663, -0.004233694591582961957 ) ) ;
#18781 = ADVANCED_FACE ( 'NONE', ( #58347 ), #63635, .T. ) ;
#18782 = CARTESIAN_POINT ( 'NONE',  ( 0.2911222467163570027, -12.10399882413660855, 1.916522451062495414 ) ) ;
#18783 = DIRECTION ( 'NONE',  ( 1.000000000000000000, 0.000000000000000000, 0.000000000000000000 ) ) ;
#18784 = VERTEX_POINT ( 'NONE', #49046 ) ;
#18785 = CARTESIAN_POINT ( 'NONE',  ( 0.2767916011545370480, 2.313848297676449839, 12.02950149294534654 ) ) ;
#18786 = CARTESIAN_POINT ( 'NONE',  ( -27.15511094194037511, -1.124668417986064650, 2.237231637349069935 ) ) ;
#18787 = ORIENTED_EDGE ( 'NONE', *, *, #14483, .F. ) ;
#18788 = EDGE_LOOP ( 'NONE', ( #5100, #23454, #52299, #31255 ) ) ;
#18789 = AXIS2_PLACEMENT_3D ( 'NONE', #1570, #21844, #32444 ) ;
#18790 = CARTESIAN_POINT ( 'NONE',  ( -35.04834644901396956, 0.01358669851861657799, 0.002604658385688424921 ) ) ;
#18791 = VECTOR ( 'NONE', #54299, 1000.000000000000000 ) ;
#18792 = ORIENTED_EDGE ( 'NONE', *, *, #63079, .T. ) ;
#18793 = EDGE_CURVE ( 'NONE', #26770, #40228, #46810, .T. ) ;
#18794 = DIRECTION ( 'NONE',  ( -1.000000000000000000, 0.000000000000000000, -0.000000000000000000 ) ) ;
#18795 = CARTESIAN_POINT ( 'NONE',  ( -28.66013792860432119, -1.673433383655446249, -0.7552004871165390876 ) ) ;
#18796 = FACE_OUTER_BOUND ( 'NONE', #18888, .T. ) ;
#18797 = CARTESIAN_POINT ( 'NONE',  ( 35.00000000000000000, -6.415447294506781084, -11.01837265713071190 ) ) ;
#18798 = ADVANCED_FACE ( 'NONE', ( #13116 ), #18773, .T. ) ;
#18799 = CARTESIAN_POINT ( 'NONE',  ( -35.00000000000000000, 11.72397916322013600, -0.7214809346827312231 ) ) ;
#18801 = EDGE_LOOP ( 'NONE', ( #64337, #31490, #2613, #31206 ) ) ;
#18800 = DIRECTION ( 'NONE',  ( 0.9582930651793755139, -0.01979360193296142434, -0.2851010602429191465 ) ) ;
#18802 = CARTESIAN_POINT ( 'NONE',  ( -22.27715526084302056, 2.228953214080639622, 2.930376837866810025 ) ) ;
#18803 = ORIENTED_EDGE ( 'NONE', *, *, #3539, .F. ) ;
#18804 = CYLINDRICAL_SURFACE ( 'NONE', #65641, 12.75000000000000178 ) ;
#18805 = ORIENTED_EDGE ( 'NONE', *, *, #54129, .T. ) ;
#18806 = ORIENTED_EDGE ( 'NONE', *, *, #31827, .F. ) ;
#18807 = B_SPLINE_CURVE_WITH_KNOTS ( 'NONE', 3,
 ( #5835, #20770, #41040, #55358, #21427, #20443, #31403, #61323, #21081, #40374, #10447, #15758, #30726, #46373, #61012, #6145 ),
 .UNSPECIFIED., .F., .F.,
 ( 4, 3, 3, 3, 3, 4 ),
 ( 0.000000000000000000, 0.0002999043160757283960, 0.0005998071753050876649, 0.0008997092107374375387, 0.001204458948194999561, 0.001510329163475231107 ),
 .UNSPECIFIED. ) ;
#18808 = CARTESIAN_POINT ( 'NONE',  ( -37.00000000000000711, -8.496612874013226957, 9.506317355798344693 ) ) ;
#18809 = CARTESIAN_POINT ( 'NONE',  ( -8.789023433377586514, -31.87591480792581322, 13.49878314047843020 ) ) ;
#18810 = CARTESIAN_POINT ( 'NONE',  ( -24.31508151051078315, 10.66642090741561510, 8.277493316746310725 ) ) ;
#18811 = CARTESIAN_POINT ( 'NONE',  ( -37.00000000000000711, -8.854740511458796703, -7.717887834988336415 ) ) ;
#18812 = CARTESIAN_POINT ( 'NONE',  ( 3.426183256940671829, -10.95277051985667427, -4.917698437020843194 ) ) ;
#18813 = FACE_OUTER_BOUND ( 'NONE', #46928, .T. ) ;
#18814 = ORIENTED_EDGE ( 'NONE', *, *, #7105, .F. ) ;
#18815 = CARTESIAN_POINT ( 'NONE',  ( 35.00000000000000000, 1.030638227056565048, -12.14284015767850278 ) ) ;
#18816 = VERTEX_POINT ( 'NONE', #24392 ) ;
#18817 = CARTESIAN_POINT ( 'NONE',  ( 0.000000000000000000, 0.000000000000000000, 0.000000000000000000 ) ) ;
#18818 = DIRECTION ( 'NONE',  ( 0.000000000000000000, -0.4935949184179134752, 0.8696919319575254770 ) ) ;
#18819 = ORIENTED_EDGE ( 'NONE', *, *, #6263, .F. ) ;
#18820 = DIRECTION ( 'NONE',  ( 1.000000000000000000, 0.000000000000000000, 0.000000000000000000 ) ) ;
#18821 = CARTESIAN_POINT ( 'NONE',  ( -37.00000000000000711, -9.076753354954062658, 8.954052073409570767 ) ) ;
#18822 = DIRECTION ( 'NONE',  ( 0.000000000000000000, 0.000000000000000000, 1.000000000000000000 ) ) ;
#18823 = CARTESIAN_POINT ( 'NONE',  ( -27.15525204139121840, -2.394850816831292306, 0.7327319213109850793 ) ) ;
#18824 = ADVANCED_FACE ( 'NONE', ( #39035, #48703 ), #59659, .F. ) ;
#18825 = ADVANCED_FACE ( 'NONE', ( #59326 ), #56530, .F. ) ;
#18826 = DIRECTION ( 'NONE',  ( -0.7886918350401329603, -0.6147887355352468219, 0.000000000000000000 ) ) ;
#18827 = CARTESIAN_POINT ( 'NONE',  ( -37.00000000000000711, -7.817492529713920391, 9.348667969174380588 ) ) ;
#18828 = ORIENTED_EDGE ( 'NONE', *, *, #51864, .T. ) ;
#18829 = ORIENTED_EDGE ( 'NONE', *, *, #59501, .F. ) ;
#18830 = CARTESIAN_POINT ( 'NONE',  ( -35.00000000000000000, 0.000000000000000000, 0.000000000000000000 ) ) ;
#18831 = DIRECTION ( 'NONE',  ( 1.000000000000000000, 0.000000000000000000, 0.000000000000000000 ) ) ;
#18832 = EDGE_CURVE ( 'NONE', #14741, #61553, #22638, .T. ) ;
#18833 = AXIS2_PLACEMENT_3D ( 'NONE', #34580, #53903, #54571 ) ;
#18834 = DIRECTION ( 'NONE',  ( 0.000000000000000000, 0.2149704402110178270, 0.9766205557100881007 ) ) ;
#18835 = B_SPLINE_CURVE_WITH_KNOTS ( 'NONE', 3,
 ( #37732, #62650, #36748, #58027, #38043, #52712, #7135, #58348, #47711, #27105, #26772, #22104, #12770, #47070, #37060, #33058, #57042, #42697, #42358 ),
 .UNSPECIFIED., .F., .F.,
 ( 4, 3, 3, 3, 3, 3, 4 ),
 ( 9.072543920006869694E-18, 4.457896483014687393E-05, 6.639290541542043741E-05, 8.820687556478911686E-05, 0.0001100173248778932783, 0.0001545671401658158157, 0.0001830328308068589834 ),
 .UNSPECIFIED. ) ;
#18836 = EDGE_CURVE ( 'NONE', #9845, #37953, #40331, .T. ) ;
#18837 = CARTESIAN_POINT ( 'NONE',  ( -27.45775109278350712, 13.35262336282554152, -1.989333891161978674 ) ) ;
#18838 = VECTOR ( 'NONE', #1224, 1000.000000000000000 ) ;
#18839 =( BOUNDED_SURFACE ( )  B_SPLINE_SURFACE ( 3, 1, ( 
 ( #46342, #4811 ),
 ( #60982, #65300 ),
 ( #45672, #55325 ),
 ( #20080, #15416 ) ),
 .UNSPECIFIED., .F., .F., .F. ) 
 B_SPLINE_SURFACE_WITH_KNOTS ( ( 4, 4 ),
 ( 2, 2 ),
 ( 0.000000000000000000, 1.000000000000000000 ),
 ( 0.000000000000000000, 1.000000000000000000 ),
 .UNSPECIFIED. ) 
 GEOMETRIC_REPRESENTATION_ITEM ( )  RATIONAL_B_SPLINE_SURFACE ( (
 ( 1.000000000000000000, 1.000000000000000000),
 ( 0.6933888150995267674, 0.9895912004443193632),
 ( 0.6933888150995267674, 0.9895912004443193632),
 ( 1.000000000000000000, 1.000000000000000000) ) ) 
 REPRESENTATION_ITEM ( '' )  SURFACE ( )  );
#18840 = CARTESIAN_POINT ( 'NONE',  ( -9.082173403709882464, -3.146272781168804045, -11.58446707970393774 ) ) ;
#18841 = CARTESIAN_POINT ( 'NONE',  ( 35.00000000000000000, -5.428340790341627198, 10.91072401419415883 ) ) ;
#18842 = CARTESIAN_POINT ( 'NONE',  ( 2.247112776671467582, 1.440655381229470233, 7.499199956301994874 ) ) ;
#18843 = DIRECTION ( 'NONE',  ( 0.000000000000000000, -0.6745969609292717939, -0.7381862504171901040 ) ) ;
#18844 = EDGE_CURVE ( 'NONE', #52522, #39065, #14409, .T. ) ;
#18845 = ORIENTED_EDGE ( 'NONE', *, *, #13824, .F. ) ;
#18846 = CARTESIAN_POINT ( 'NONE',  ( -37.00000000000000711, -12.12087942037210553, 1.262958560998716617 ) ) ;
#18847 = CARTESIAN_POINT ( 'NONE',  ( -22.29195009621226475, -2.585382421603431347, 2.682867222693514186 ) ) ;
#18848 = CARTESIAN_POINT ( 'NONE',  ( 1.948354844646123629, -8.228891433296906754, -8.685970062895197685 ) ) ;
#18849 = CARTESIAN_POINT ( 'NONE',  ( 2.273267844204867938, -0.1513603614829975852, -7.643541951623947561 ) ) ;
#18850 = CARTESIAN_POINT ( 'NONE',  ( 1.372161826076866653, -4.864129100816962925, -11.63973780005257019 ) ) ;
#18851 = ORIENTED_EDGE ( 'NONE', *, *, #396, .F. ) ;
#18852 = CARTESIAN_POINT ( 'NONE',  ( 0.2655924914740778187, -7.905499957109299203, 9.352877839710574293 ) ) ;
#18853 = CARTESIAN_POINT ( 'NONE',  ( 0.9232058338315058954, 10.98407661738928631, 5.905985151448186699 ) ) ;
#18854 = EDGE_CURVE ( 'NONE', #19934, #65334, #56393, .T. ) ;
#18855 = CARTESIAN_POINT ( 'NONE',  ( -4.228765754682470401, -25.91303510919334485, -15.38236557491807766 ) ) ;
#18856 = ORIENTED_EDGE ( 'NONE', *, *, #43704, .F. ) ;
#18857 = CARTESIAN_POINT ( 'NONE',  ( -9.961160847258154760, -3.372123831127339155, -13.07617202219271135 ) ) ;
#18858 = CARTESIAN_POINT ( 'NONE',  ( 35.00000000000000000, 4.705694406421931860E-17, -3.469127814946512892E-15 ) ) ;
#18859 = FACE_OUTER_BOUND ( 'NONE', #63851, .T. ) ;
#18860 = ADVANCED_FACE ( 'NONE', ( #65595 ), #35002, .T. ) ;
#18861 = CARTESIAN_POINT ( 'NONE',  ( 0.3278977287071183633, -8.073566434006636428, 9.235688435081703673 ) ) ;
#18862 = CARTESIAN_POINT ( 'NONE',  ( 1.719304012341202004, 11.67935079956989775, -5.066286238790292273 ) ) ;
#18863 = EDGE_CURVE ( 'NONE', #3903, #6328, #36150, .T. ) ;
#18864 = AXIS2_PLACEMENT_3D ( 'NONE', #63277, #39313, #17746 ) ;
#18865 = CARTESIAN_POINT ( 'NONE',  ( 2.000000000000001776, 0.000000000000000000, 0.000000000000000000 ) ) ;
#18866 = EDGE_CURVE ( 'NONE', #49313, #55012, #24738, .T. ) ;
#18867 = B_SPLINE_CURVE_WITH_KNOTS ( 'NONE', 3,
 ( #10375, #744, #35959, #50322, #39078, #16015, #5087 ),
 .UNSPECIFIED., .F., .F.,
 ( 4, 3, 4 ),
 ( 2.185848306064139164E-15, 0.002398160485434442518, 0.005002426799378964853 ),
 .UNSPECIFIED. ) ;
#18868 = ORIENTED_EDGE ( 'NONE', *, *, #20961, .F. ) ;
#18869 = CARTESIAN_POINT ( 'NONE',  ( -25.00000000000000355, -30.00000000000000000, 1.530808498934191521E-15 ) ) ;
#18870 = CARTESIAN_POINT ( 'NONE',  ( 5.536195898058073439, -0.008323005098841084262, 0.001726268814999596442 ) ) ;
#18871 = AXIS2_PLACEMENT_3D ( 'NONE', #28546, #63779, #33547 ) ;
#18872 = CARTESIAN_POINT ( 'NONE',  ( 2.000000000000001776, 3.786546189469266466, -5.663561025469129540 ) ) ;
#18873 = CARTESIAN_POINT ( 'NONE',  ( 2.990245332647798016, -6.814589384234918334, 5.049055049623243363 ) ) ;
#18874 = CARTESIAN_POINT ( 'NONE',  ( 2.284126774967664808, 7.558363379199202647, -1.171808575345546721 ) ) ;
#18875 = DIRECTION ( 'NONE',  ( -1.000000000000000000, -1.836970198721029688E-16, -0.000000000000000000 ) ) ;
#18876 = EDGE_CURVE ( 'NONE', #37616, #18330, #45016, .T. ) ;
#18877 = CARTESIAN_POINT ( 'NONE',  ( 2.242418902651939216, 7.535443599794976244, 1.227462051872167725 ) ) ;
#18878 = CYLINDRICAL_SURFACE ( 'NONE', #48872, 12.74999999999999822 ) ;
#18879 = ORIENTED_EDGE ( 'NONE', *, *, #8539, .F. ) ;
#18880 = VERTEX_POINT ( 'NONE', #116 ) ;
#18881 =( LENGTH_UNIT ( ) NAMED_UNIT ( * ) SI_UNIT ( .MILLI., .METRE. ) );
#18882 = EDGE_LOOP ( 'NONE', ( #24019, #62398, #52487, #38402 ) ) ;
#18883 = CIRCLE ( 'NONE', #44344, 5.000000000000000888 ) ;
#18884 = CARTESIAN_POINT ( 'NONE',  ( -22.29382655386184808, 2.586160974799843970, -2.689927793811009771 ) ) ;
#18885 = CARTESIAN_POINT ( 'NONE',  ( 37.00000000000000711, 0.06441628369836321921, -12.18632975068353019 ) ) ;
#18886 = CIRCLE ( 'NONE', #58191, 12.74999999999999822 ) ;
#18887 = CARTESIAN_POINT ( 'NONE',  ( 47.00000000000000711, 4.705694406421931860E-17, -3.469127814946512892E-15 ) ) ;
#18888 = EDGE_LOOP ( 'NONE', ( #34349, #18741, #16001, #39312 ) ) ;
#18889 = CARTESIAN_POINT ( 'NONE',  ( 0.2915757698887277427, 5.940579417090927627, -10.71881693660615475 ) ) ;
#18890 = DIRECTION ( 'NONE',  ( 1.000000000000000000, -0.000000000000000000, 0.000000000000000000 ) ) ;
#18891 = DIRECTION ( 'NONE',  ( 0.000000000000000000, 0.000000000000000000, 1.000000000000000000 ) ) ;
#18892 = ORIENTED_EDGE ( 'NONE', *, *, #63921, .F. ) ;
#18893 = ORIENTED_EDGE ( 'NONE', *, *, #24661, .F. ) ;
#18894 = CYLINDRICAL_SURFACE ( 'NONE', #57615, 6.936499999999988120 ) ;
#18895 = CARTESIAN_POINT ( 'NONE',  ( 0.3665391374699467075, 9.237363111276769345, 8.095513416941262363 ) ) ;
#18896 = ORIENTED_EDGE ( 'NONE', *, *, #60275, .T. ) ;
#18897 = ORIENTED_EDGE ( 'NONE', *, *, #38279, .F. ) ;
#18898 = CARTESIAN_POINT ( 'NONE',  ( 12.51043607184429796, 0.3316456940255351760, 13.49694458083817672 ) ) ;
#18899 = LINE ( 'NONE', #49810, #58139 ) ;
#18900 = EDGE_CURVE ( 'NONE', #55595, #39189, #1204, .T. ) ;
#18901 = CARTESIAN_POINT ( 'NONE',  ( -27.09150307427448112, -2.306459590995638020, 0.1754204729056251799 ) ) ;
#18902 = DIRECTION ( 'NONE',  ( 1.000000000000000000, 0.000000000000000000, 0.000000000000000000 ) ) ;
#18903 = CYLINDRICAL_SURFACE ( 'NONE', #53538, 13.50000000000000178 ) ;
#18904 = EDGE_CURVE ( 'NONE', #22729, #47974, #60675, .T. ) ;
#18905 = ORIENTED_EDGE ( 'NONE', *, *, #50082, .T. ) ;
#18906 = B_SPLINE_CURVE_WITH_KNOTS ( 'NONE', 3,
 ( #39427, #3571, #34104, #4539, #13814, #3884, #33779, #39098, #29447, #53765, #3225, #8201, #34748, #18837 ),
 .UNSPECIFIED., .F., .F.,
 ( 4, 2, 2, 2, 2, 2, 4 ),
 ( 0.000000000000000000, 0.001838460847883235504, 0.002757691271824853040, 0.003676921695766471009, 0.004596152119708088978, 0.005515382543649706079, 0.007353843391532942017 ),
 .UNSPECIFIED. ) ;
#18907 = DIRECTION ( 'NONE',  ( -1.000000000000000000, 0.000000000000000000, 0.000000000000000000 ) ) ;
#18908 = CARTESIAN_POINT ( 'NONE',  ( 0.2648978790185584908, 7.972372351883154629, -9.295532325666371776 ) ) ;
#18909 = CARTESIAN_POINT ( 'NONE',  ( 0.2651627923886356042, -9.437479615842690350, 7.803990550466266995 ) ) ;
#18910 = DIRECTION ( 'NONE',  ( 1.000000000000000000, 0.000000000000000000, -0.000000000000000000 ) ) ;
#18911 = CARTESIAN_POINT ( 'NONE',  ( -22.71097035706202760, 2.846599994298365743, -4.089776368546553798 ) ) ;
#18912 = CARTESIAN_POINT ( 'NONE',  ( -27.08430792439084556, 1.625846845508333027, -1.614882584890335870 ) ) ;
#18913 = CARTESIAN_POINT ( 'NONE',  ( -35.00000000000000000, -8.366449238204298311, -9.621072037177086145 ) ) ;
#18914 = CARTESIAN_POINT ( 'NONE',  ( 37.00000000000000711, 7.238157050195626496, -10.49626516989273384 ) ) ;
#18915 = EDGE_CURVE ( 'NONE', #22151, #43665, #15713, .T. ) ;
#18916 = VECTOR ( 'NONE', #10608, 1000.000000000000000 ) ;
#18917 = ORIENTED_EDGE ( 'NONE', *, *, #46912, .F. ) ;
#18918 = DIRECTION ( 'NONE',  ( -1.000000000000000000, 0.000000000000000000, 0.000000000000000000 ) ) ;
#18919 = AXIS2_PLACEMENT_3D ( 'NONE', #28326, #22696, #52937 ) ;
#18920 = VERTEX_POINT ( 'NONE', #25716 ) ;
#18921 = CARTESIAN_POINT ( 'NONE',  ( 0.9232058338315058954, 8.301689855530167250, 9.306586124266621241 ) ) ;
#18922 = CARTESIAN_POINT ( 'NONE',  ( 2.290907136833250757, -7.504812001538596178, -1.488079974905019309 ) ) ;
#18923 = CARTESIAN_POINT ( 'NONE',  ( -16.15963131418214971, 7.828775782396976801, -10.99875241953665927 ) ) ;
#18924 = AXIS2_PLACEMENT_3D ( 'NONE', #11441, #52995, #22400 ) ;
#18925 = DIRECTION ( 'NONE',  ( 0.000000000000000000, -0.01356324068817992175, 0.9999080150203990547 ) ) ;
#18926 = EDGE_CURVE ( 'NONE', #10959, #35622, #24596, .T. ) ;
#18927 = ORIENTED_EDGE ( 'NONE', *, *, #35390, .F. ) ;
#18928 = DIRECTION ( 'NONE',  ( 1.000000000000000000, 0.000000000000000000, -0.000000000000000000 ) ) ;
#18929 = CARTESIAN_POINT ( 'NONE',  ( 35.00000000000000000, 12.01765980939841683, -2.021542716731445921 ) ) ;
#18930 = CARTESIAN_POINT ( 'NONE',  ( 1.000000000000000888, 7.203928197742101247, 2.086484728383167564 ) ) ;
#18931 = VECTOR ( 'NONE', #31339, 1000.000000000000000 ) ;
#18932 = CARTESIAN_POINT ( 'NONE',  ( -22.28546858134833286, 2.654201075783140684, 2.587024666338633594 ) ) ;
#18933 = EDGE_CURVE ( 'NONE', #12489, #10479, #7611, .T. ) ;
#18934 = DIRECTION ( 'NONE',  ( 0.000000000000000000, 0.9246979985058709772, 0.3807014730195252272 ) ) ;
#18935 = EDGE_LOOP ( 'NONE', ( #50703, #8134, #48127, #35894 ) ) ;
#18936 = FACE_OUTER_BOUND ( 'NONE', #30270, .T. ) ;
#18937 = VERTEX_POINT ( 'NONE', #32634 ) ;
#18938 = CARTESIAN_POINT ( 'NONE',  ( 2.781367136451633471, 5.783466416658805009, -5.255136723410042343 ) ) ;
#18939 = DIRECTION ( 'NONE',  ( 1.000000000000000000, 0.000000000000000000, 0.000000000000000000 ) ) ;
#18940 = DIRECTION ( 'NONE',  ( 1.000000000000000000, 0.000000000000000000, 0.000000000000000000 ) ) ;
#18941 = DIRECTION ( 'NONE',  ( -1.000000000000000000, 0.000000000000000000, 0.000000000000000000 ) ) ;
#18942 = EDGE_CURVE ( 'NONE', #60252, #65370, #47323, .T. ) ;
#18943 = ORIENTED_EDGE ( 'NONE', *, *, #58044, .F. ) ;
#18944 = ORIENTED_EDGE ( 'NONE', *, *, #50552, .F. ) ;
#18945 = DIRECTION ( 'NONE',  ( 0.000000000000000000, -0.8009703041134234036, -0.5987040770935587730 ) ) ;
#18946 = ADVANCED_FACE ( 'NONE', ( #2076 ), #7377, .T. ) ;
#18947 = DIRECTION ( 'NONE',  ( 1.000000000000000000, 0.000000000000000000, 0.000000000000000000 ) ) ;
#18948 = DIRECTION ( 'NONE',  ( 1.000000000000000000, -0.000000000000000000, 0.000000000000000000 ) ) ;
#18949 = FACE_OUTER_BOUND ( 'NONE', #62966, .T. ) ;
#18951 = CARTESIAN_POINT ( 'NONE',  ( 5.516018279890452902, 0.005331956019561711300, -0.004180585980734999839 ) ) ;
#18950 = AXIS2_PLACEMENT_3D ( 'NONE', #2888, #52100, #37451 ) ;
#18952 = EDGE_CURVE ( 'NONE', #32989, #666, #57288, .T. ) ;
#18953 = DIRECTION ( 'NONE',  ( 0.000000000000000000, 0.9796553971857735466, 0.2006870767258926436 ) ) ;
#18954 = ORIENTED_EDGE ( 'NONE', *, *, #22087, .T. ) ;
#18955 = ORIENTED_EDGE ( 'NONE', *, *, #64047, .T. ) ;
#18956 = VERTEX_POINT ( 'NONE', #46646 ) ;
#18957 = CARTESIAN_POINT ( 'NONE',  ( 2.253265082352433168, 7.220580418434058068, -2.491579069691517656 ) ) ;
#18958 = AXIS2_PLACEMENT_3D ( 'NONE', #36216, #41875, #993 ) ;
#18959 = DIRECTION ( 'NONE',  ( 0.3865475372811021382, -0.6075346789811253423, 0.6938894834605981998 ) ) ;
#18961 = ADVANCED_FACE ( 'NONE', ( #22026 ), #31665, .T. ) ;
#18960 = ORIENTED_EDGE ( 'NONE', *, *, #1276, .T. ) ;
#18962 = CARTESIAN_POINT ( 'NONE',  ( 2.000000000000001776, -7.248432822490255667, 1.926193556692974429 ) ) ;
#18963 = CARTESIAN_POINT ( 'NONE',  ( 35.00000000000000000, 12.38385022362085941, 3.033604067594442011 ) ) ;
#18965 = ORIENTED_EDGE ( 'NONE', *, *, #49925, .F. ) ;
#18964 = AXIS2_PLACEMENT_3D ( 'NONE', #9028, #49924, #8706 ) ;
#18966 = AXIS2_PLACEMENT_3D ( 'NONE', #11429, #37019, #27373 ) ;
#18967 = DIRECTION ( 'NONE',  ( 0.000000000000000000, -0.01356324068817998940, 0.9999080150203990547 ) ) ;
#18968 = CARTESIAN_POINT ( 'NONE',  ( -30.18541646480309026, -1.416020129149132334, -13.42553116244734746 ) ) ;
#18969 = CARTESIAN_POINT ( 'NONE',  ( 0.000000000000000000, 7.203928197742132333, -2.086484728383096510 ) ) ;
#18970 = EDGE_LOOP ( 'NONE', ( #25876, #43112, #44831, #19446 ) ) ;
#18971 = ORIENTED_EDGE ( 'NONE', *, *, #47994, .T. ) ;
#18972 = AXIS2_PLACEMENT_3D ( 'NONE', #44557, #64839, #31568 ) ;
#18973 = CARTESIAN_POINT ( 'NONE',  ( 2.247206125382828823, 2.502718378778807207, 7.214589497757592618 ) ) ;
#18974 = ORIENTED_EDGE ( 'NONE', *, *, #63333, .F. ) ;
#18975 = CARTESIAN_POINT ( 'NONE',  ( 10.75853767213705048, 7.830989516993144051, 10.99661780661416088 ) ) ;
#18976 = EDGE_LOOP ( 'NONE', ( #28836, #63931, #23395, #10746 ) ) ;
#18977 = VERTEX_POINT ( 'NONE', #51660 ) ;
#18978 = AXIS2_PLACEMENT_3D ( 'NONE', #27820, #48123, #2580 ) ;
#18979 = ORIENTED_EDGE ( 'NONE', *, *, #6916, .F. ) ;
#18980 = CARTESIAN_POINT ( 'NONE',  ( 0.2648978790185584908, 11.46165506714228322, 4.312320170909275774 ) ) ;
#18981 = CARTESIAN_POINT ( 'NONE',  ( -35.04660725145885891, 0.004999447127077803754, -0.01123650152081124946 ) ) ;
#18982 = DIRECTION ( 'NONE',  ( -1.000000000000000000, 0.000000000000000000, 0.000000000000000000 ) ) ;
#18983 = CARTESIAN_POINT ( 'NONE',  ( 1.719304012339844867, -10.62216384465586216, 7.017415949612814785 ) ) ;
#18984 = FACE_OUTER_BOUND ( 'NONE', #49254, .T. ) ;
#18985 = EDGE_LOOP ( 'NONE', ( #64427, #57665, #63118, #48631 ) ) ;
#18986 = CARTESIAN_POINT ( 'NONE',  ( 0.7400311444011711259, 10.91558650018042620, 5.892391870929054143 ) ) ;
#18987 = EDGE_CURVE ( 'NONE', #63181, #58825, #24547, .T. ) ;
#18988 = EDGE_LOOP ( 'NONE', ( #36204, #16924, #11205, #23249 ) ) ;
#18989 = CYLINDRICAL_SURFACE ( 'NONE', #6252, 13.50000000000000178 ) ;
#18990 = CARTESIAN_POINT ( 'NONE',  ( 2.000000000000001776, 0.000000000000000000, 0.000000000000000000 ) ) ;
#18991 = EDGE_LOOP ( 'NONE', ( #63351, #9501, #61537, #54838 ) ) ;
#18992 = CYLINDRICAL_SURFACE ( 'NONE', #59404, 2.899999999999994582 ) ;
#18993 = CARTESIAN_POINT ( 'NONE',  ( 2.276905613633645853, -6.697548486790738664, -3.688905863353284520 ) ) ;
#18994 = VERTEX_POINT ( 'NONE', #6420 ) ;
#18995 = CIRCLE ( 'NONE', #10472, 5.000000000000000000 ) ;
#18996 = ORIENTED_EDGE ( 'NONE', *, *, #47374, .T. ) ;
#18997 = CARTESIAN_POINT ( 'NONE',  ( 2.276905613633652070, -7.644700064315451904, 0.1540880535620714475 ) ) ;
#18998 = AXIS2_PLACEMENT_3D ( 'NONE', #56017, #31412, #6152 ) ;
#18999 = ORIENTED_EDGE ( 'NONE', *, *, #29515, .T. ) ;
#19000 = CARTESIAN_POINT ( 'NONE',  ( -35.00000000000000000, -0.06441628369844946966, 12.18632975068352842 ) ) ;
#19001 = PLANE ( 'NONE',  #15969 ) ;
#19002 = CARTESIAN_POINT ( 'NONE',  ( -27.08417568107323348, 2.142502990753195835, 0.8117865859100116266 ) ) ;
#19003 = LINE ( 'NONE', #8701, #44709 ) ;
#19004 = CARTESIAN_POINT ( 'NONE',  ( 10.13479916714561568, 11.98071251699297690, -0.6877595805417434649 ) ) ;
#19005 = ADVANCED_FACE ( 'NONE', ( #6103 ), #60787, .F. ) ;
#19006 = VERTEX_POINT ( 'NONE', #16048 ) ;
#19007 = CARTESIAN_POINT ( 'NONE',  ( -35.05012975565874456, -0.01089417657934746084, 0.008684292310210053531 ) ) ;
#19008 = CARTESIAN_POINT ( 'NONE',  ( -30.07634502127111631, -2.989967992425739851, 13.17072238577171106 ) ) ;
#19009 = ADVANCED_FACE ( 'NONE', ( #42614 ), #56646, .T. ) ;
#19010 = VECTOR ( 'NONE', #29559, 1000.000000000000000 ) ;
#19011 = AXIS2_PLACEMENT_3D ( 'NONE', #13204, #3237, #30038 ) ;
#19012 = CARTESIAN_POINT ( 'NONE',  ( -18.06522620542768109, -29.74877956674518131, -8.189528952361769143 ) ) ;
#19014 = CIRCLE ( 'NONE', #27492, 5.000000000000000888 ) ;
#19013 = CARTESIAN_POINT ( 'NONE',  ( -22.46509356695202086, 4.154553862421376920, 0.8809186187925714950 ) ) ;
#19015 = PRODUCT ( 'main drive axle', 'main drive axle', '', ( #11827 ) ) ;
#19016 = DIRECTION ( 'NONE',  ( 0.000000000000000000, 0.000000000000000000, 1.000000000000000000 ) ) ;
#19017 = CARTESIAN_POINT ( 'NONE',  ( 0.000000000000000000, -5.997115278587647147, 3.485633455389469226 ) ) ;
#19018 = CARTESIAN_POINT ( 'NONE',  ( -37.00000000000000711, 6.303578524886947143, 10.42955799785322490 ) ) ;
#19019 = VECTOR ( 'NONE', #27090, 1000.000000000000114 ) ;
#19020 = EDGE_CURVE ( 'NONE', #54027, #65390, #1763, .T. ) ;
#19021 = VERTEX_POINT ( 'NONE', #11082 ) ;
#19022 = CARTESIAN_POINT ( 'NONE',  ( -27.08579483061203064, -1.318128465624909706, -1.879952013015660395 ) ) ;
#19023 =( BOUNDED_CURVE ( )  B_SPLINE_CURVE ( 3, ( #62415, #37150, #57460, #11883 ),
 .UNSPECIFIED., .F., .F. ) 
 B_SPLINE_CURVE_WITH_KNOTS ( ( 4, 4 ),
 ( 1.481266777651250033, 1.521986778384522232 ),
 .UNSPECIFIED. ) 
 CURVE ( )  GEOMETRIC_REPRESENTATION_ITEM ( )  RATIONAL_B_SPLINE_CURVE ( ( 1.000000000000000000, 0.9998618282348130659, 0.9998618282348130659, 1.000000000000000000 ) ) 
 REPRESENTATION_ITEM ( '' )  );
#19024 = EDGE_LOOP ( 'NONE', ( #57865, #15311, #64105, #10898 ) ) ;
#19025 = CARTESIAN_POINT ( 'NONE',  ( 0.2801149460245166978, 1.933835447580789957, -12.09752788490055053 ) ) ;
#19026 = CARTESIAN_POINT ( 'NONE',  ( 36.00000000000000711, -12.49688848680882103, 2.527899948230769578 ) ) ;
#19027 = CARTESIAN_POINT ( 'NONE',  ( 2.573738926104375935, -7.355212866432314200, 2.426778239006430304 ) ) ;
#19028 = CARTESIAN_POINT ( 'NONE',  ( 0.3675815128205894289, 3.951233083390626177, -11.62724744438061641 ) ) ;
#19029 = ORIENTED_EDGE ( 'NONE', *, *, #49913, .T. ) ;
#19030 = VERTEX_POINT ( 'NONE', #26361 ) ;
#19031 = EDGE_LOOP ( 'NONE', ( #5689, #35053, #52510, #21801 ) ) ;
#19032 = CARTESIAN_POINT ( 'NONE',  ( 29.63669315105201463, -8.416703354620286959, 10.56457041555997378 ) ) ;
#19033 = ADVANCED_FACE ( 'NONE', ( #21377 ), #62259, .T. ) ;
#19034 = CIRCLE ( 'NONE', #39195, 4.999999999999999112 ) ;
#19035 = EDGE_LOOP ( 'NONE', ( #46060, #59290, #11440, #64615, #49859, #8574, #8058, #18447, #63575, #62591, #28379, #23221, #30486, #41460, #2053, #6220, #32265, #32891, #58995, #53096, #399, #43487, #21628, #37754, #806, #4926, #19109, #22277, #29362, #23776, #2910, #26204, #21217, #55242 ) ) ;
#19036 = CARTESIAN_POINT ( 'NONE',  ( -22.27722015946438816, -2.356370737780152602, -2.828901469906482724 ) ) ;
#19037 = FACE_OUTER_BOUND ( 'NONE', #40274, .T. ) ;
#19038 = CARTESIAN_POINT ( 'NONE',  ( 0.2648321136542712284, 10.53380804838497475, 6.245325033825767314 ) ) ;
#19039 = CARTESIAN_POINT ( 'NONE',  ( 2.305787727787083519, -2.461236246751120849, 7.249469779319902329 ) ) ;
#19040 = ORIENTED_EDGE ( 'NONE', *, *, #58267, .F. ) ;
#19041 = CARTESIAN_POINT ( 'NONE',  ( -37.00000000000000711, 5.556331110570408960, 11.47561260193578825 ) ) ;
#19042 = AXIS2_PLACEMENT_3D ( 'NONE', #16020, #31000, #36312 ) ;
#19043 = DIRECTION ( 'NONE',  ( 1.000000000000000000, 0.000000000000000000, 0.000000000000000000 ) ) ;
#19045 = ORIENTED_EDGE ( 'NONE', *, *, #5565, .F. ) ;
#19044 = DIRECTION ( 'NONE',  ( -0.9582930651793755139, -0.06744057189511995509, 0.2777159889015688998 ) ) ;
#19046 = ORIENTED_EDGE ( 'NONE', *, *, #62585, .T. ) ;
#19047 = CARTESIAN_POINT ( 'NONE',  ( 0.2648978790185602672, -6.237101853238473659, -10.53870023327869987 ) ) ;
#19048 = ORIENTED_EDGE ( 'NONE', *, *, #48222, .T. ) ;
#19049 = CYLINDRICAL_SURFACE ( 'NONE', #52869, 2.899999999999994582 ) ;
#19050 = B_SPLINE_CURVE_WITH_KNOTS ( 'NONE', 3,
 ( #41415, #51101, #31134, #47098, #46117, #26797, #31457, #46749, #1553, #16811, #10846, #5557, #6859 ),
 .UNSPECIFIED., .F., .F.,
 ( 4, 3, 3, 3, 4 ),
 ( 2.453269466693398698E-18, 6.607593386745200356E-05, 0.0001321518677373506177, 0.0001982171734706192877, 0.0002642860854759468197 ),
 .UNSPECIFIED. ) ;
#19051 = CARTESIAN_POINT ( 'NONE',  ( -35.00000000000000000, -10.80631716521663854, -4.603882218679666849 ) ) ;
#19052 = AXIS2_PLACEMENT_3D ( 'NONE', #39451, #50108, #59415 ) ;
#19053 = DIRECTION ( 'NONE',  ( 0.000000000000000000, -0.01356324068817998940, 0.9999080150203990547 ) ) ;
#19054 = CARTESIAN_POINT ( 'NONE',  ( -2.812214508280806324, 11.36735472963162508, 3.846083643116565920 ) ) ;
#19055 = CARTESIAN_POINT ( 'NONE',  ( 0.3654063281920786332, 9.573804659448660104, 7.689576266239694924 ) ) ;
#19056 = DIRECTION ( 'NONE',  ( -1.000000000000000000, 0.000000000000000000, 0.000000000000000000 ) ) ;
#19057 = CARTESIAN_POINT ( 'NONE',  ( 2.350038591458106119, -4.227970903880792441, 9.744161863086473474 ) ) ;
#19059 = ORIENTED_EDGE ( 'NONE', *, *, #3309, .T. ) ;
#19058 = CARTESIAN_POINT ( 'NONE',  ( -27.10719052120871098, -1.962717903527672059, 1.310802520592011966 ) ) ;
#19060 = AXIS2_PLACEMENT_3D ( 'NONE', #44045, #34389, #59671 ) ;
#19061 = ADVANCED_FACE ( 'NONE', ( #57629 ), #12367, .T. ) ;
#19062 = VERTEX_POINT ( 'NONE', #12048 ) ;
#19063 = CARTESIAN_POINT ( 'NONE',  ( 19.67311005600952711, -0.7004819783312107306, 25.00000000000000000 ) ) ;
#19064 = EDGE_LOOP ( 'NONE', ( #18067, #50932, #60254, #62100 ) ) ;
#19065 = EDGE_CURVE ( 'NONE', #37445, #10053, #30949, .T. ) ;
#19066 = VERTEX_POINT ( 'NONE', #7065 ) ;
#19067 = FACE_OUTER_BOUND ( 'NONE', #1664, .T. ) ;
#19068 = CARTESIAN_POINT ( 'NONE',  ( 37.00000000000000711, 10.62137734850267989, 5.015831474386340361 ) ) ;
#19069 = AXIS2_PLACEMENT_3D ( 'NONE', #52304, #16033, #36327 ) ;
#19070 = CARTESIAN_POINT ( 'NONE',  ( 37.00000000000000711, 4.705694406421931860E-17, -3.469127814946512892E-15 ) ) ;
#19071 = CARTESIAN_POINT ( 'NONE',  ( -22.31328051695926007, 2.109671368890633669, 3.148362328073145200 ) ) ;
#19072 = CARTESIAN_POINT ( 'NONE',  ( -22.30078715814471479, 1.645949880549432365, -3.372109767220907273 ) ) ;
#19073 = CARTESIAN_POINT ( 'NONE',  ( 2.241352910868909643, -7.503490710578223144, -1.407733736974942973 ) ) ;
#19074 = EDGE_CURVE ( 'NONE', #54100, #20923, #61700, .T. ) ;
#19075 = LINE ( 'NONE', #5098, #33275 ) ;
#19076 = AXIS2_PLACEMENT_3D ( 'NONE', #9313, #4360, #14624 ) ;
#19077 = VERTEX_POINT ( 'NONE', #34296 ) ;
#19078 = CARTESIAN_POINT ( 'NONE',  ( -35.00000000000000000, -3.704519465651227694, -11.60979404548638705 ) ) ;
#19079 = DIRECTION ( 'NONE',  ( -1.000000000000000000, 0.000000000000000000, 0.000000000000000000 ) ) ;
#19080 = CARTESIAN_POINT ( 'NONE',  ( -22.30625920655495165, 2.110841417170918000, 3.150098859949304941 ) ) ;
#19081 = ADVANCED_FACE ( 'NONE', ( #7729 ), #42965, .T. ) ;
#19082 = ADVANCED_BREP_SHAPE_REPRESENTATION ( '', ( #6945, #24966 ), #29232 ) ;
#19083 = VERTEX_POINT ( 'NONE', #8379 ) ;
#19084 = CIRCLE ( 'NONE', #9508, 7.499999999999988454 ) ;
#19085 = AXIS2_PLACEMENT_3D ( 'NONE', #29518, #4269, #56799 ) ;
#19086 = CARTESIAN_POINT ( 'NONE',  ( 28.27451930523357504, -3.452175767011101293, -24.83788945613661880 ) ) ;
#19087 = FACE_OUTER_BOUND ( 'NONE', #21833, .T. ) ;
#19088 = ORIENTED_EDGE ( 'NONE', *, *, #33756, .F. ) ;
#19089 = CARTESIAN_POINT ( 'NONE',  ( 35.00000000000000000, -12.05416472667166516, -1.791059740004382617 ) ) ;
#19090 = CARTESIAN_POINT ( 'NONE',  ( 1.000000000000000888, -6.586971819220299729, -3.586335490831473738 ) ) ;
#19091 = LINE ( 'NONE', #59993, #50275 ) ;
#19092 = AXIS2_PLACEMENT_3D ( 'NONE', #57379, #23357, #57722 ) ;
#19093 = CARTESIAN_POINT ( 'NONE',  ( 35.00000000000000000, -5.391785509271032062, -10.43555801961473861 ) ) ;
#19094 = CARTESIAN_POINT ( 'NONE',  ( 3.152665057734121756, -0.4801242025592447060, 7.923639299008720549 ) ) ;
#19095 = CIRCLE ( 'NONE', #1072, 16.19615242270663558 ) ;
#19096 = ORIENTED_EDGE ( 'NONE', *, *, #45550, .T. ) ;
#19097 = DIRECTION ( 'NONE',  ( 0.000000000000000000, 0.01356324068817998940, -0.9999080150203990547 ) ) ;
#19098 = LINE ( 'NONE', #39046, #4527 ) ;
#19099 = CARTESIAN_POINT ( 'NONE',  ( -22.27384469013076185, -2.625926801827875412, 2.581192766446261722 ) ) ;
#19100 = ORIENTED_EDGE ( 'NONE', *, *, #60975, .F. ) ;
#19101 = PLANE ( 'NONE',  #18094 ) ;
#19102 = DIRECTION ( 'NONE',  ( 0.000000000000000000, 0.000000000000000000, 1.000000000000000000 ) ) ;
#19103 = VERTEX_POINT ( 'NONE', #38641 ) ;
#19104 = EDGE_CURVE ( 'NONE', #11231, #6620, #53225, .T. ) ;
#19105 = VECTOR ( 'NONE', #41860, 1000.000000000000000 ) ;
#19106 = VERTEX_POINT ( 'NONE', #2424 ) ;
#19107 = CARTESIAN_POINT ( 'NONE',  ( -35.00000000000000000, -2.185196060783795691, -11.54110654723651486 ) ) ;
#19108 = EDGE_CURVE ( 'NONE', #2190, #9138, #27768, .T. ) ;
#19109 = ORIENTED_EDGE ( 'NONE', *, *, #35072, .T. ) ;
#19110 = DIRECTION ( 'NONE',  ( 1.000000000000000000, 0.000000000000000000, 0.000000000000000000 ) ) ;
#19111 = DIRECTION ( 'NONE',  ( 0.000000000000000000, 0.000000000000000000, -1.000000000000000000 ) ) ;
#19112 = PLANE ( 'NONE',  #35406 ) ;
#19113 = CYLINDRICAL_SURFACE ( 'NONE', #61634, 12.75000000000000178 ) ;
#19114 = CARTESIAN_POINT ( 'NONE',  ( -35.04643116707788408, 0.01204777744935082995, -0.001845126042314057524 ) ) ;
#19116 = ORIENTED_EDGE ( 'NONE', *, *, #65276, .T. ) ;
#19115 = FACE_OUTER_BOUND ( 'NONE', #16190, .T. ) ;
#19117 = DIRECTION ( 'NONE',  ( 0.000000000000000000, 0.01356324068817998940, -0.9999080150203990547 ) ) ;
#19118 = ORIENTED_EDGE ( 'NONE', *, *, #13906, .T. ) ;
#19119 = CARTESIAN_POINT ( 'NONE',  ( -22.51237073810381162, -4.319597983500831795, -0.9543406717316693655 ) ) ;
#19120 = ORIENTED_EDGE ( 'NONE', *, *, #3034, .T. ) ;
#19121 = ORIENTED_EDGE ( 'NONE', *, *, #44997, .F. ) ;
#19122 = CARTESIAN_POINT ( 'NONE',  ( -26.94359064758800670, 12.23578565015750286, 5.704334401058154036 ) ) ;
#19123 = CARTESIAN_POINT ( 'NONE',  ( -10.70822065730263084, -29.54386645810036782, 10.21044671111158664 ) ) ;
#19124 = DIRECTION ( 'NONE',  ( 0.000000000000000000, 0.000000000000000000, 1.000000000000000000 ) ) ;
#19125 = ADVANCED_FACE ( 'NONE', ( #47969 ), #58618, .T. ) ;
#19126 = CIRCLE ( 'NONE', #60512, 4.999999999999999112 ) ;
#19127 = CARTESIAN_POINT ( 'NONE',  ( -35.00000000000000000, 0.000000000000000000, 0.000000000000000000 ) ) ;
#19128 = DIRECTION ( 'NONE',  ( 1.000000000000000000, 0.000000000000000000, 0.000000000000000000 ) ) ;
#19129 = ORIENTED_EDGE ( 'NONE', *, *, #62885, .F. ) ;
#19130 = EDGE_CURVE ( 'NONE', #52731, #4816, #40487, .T. ) ;
#19131 = ORIENTED_EDGE ( 'NONE', *, *, #30198, .T. ) ;
#19132 = ADVANCED_FACE ( 'NONE', ( #59257 ), #18708, .T. ) ;
#19133 = CARTESIAN_POINT ( 'NONE',  ( 37.25000000000000711, -1.694065894508600678E-18, 1.500000000000000222 ) ) ;
#19134 = EDGE_CURVE ( 'NONE', #56264, #13249, #33649, .T. ) ;
#19135 = ORIENTED_EDGE ( 'NONE', *, *, #32590, .T. ) ;
#19136 = CARTESIAN_POINT ( 'NONE',  ( 37.00000000000000711, 4.705694406421931860E-17, -3.469127814946512892E-15 ) ) ;
#19137 = CARTESIAN_POINT ( 'NONE',  ( 2.177405672431479644, -9.343720763424588682, 6.173731551723741440 ) ) ;
#19138 = DIRECTION ( 'NONE',  ( -1.000000000000000000, 0.000000000000000000, 0.000000000000000000 ) ) ;
#19140 = AXIS2_PLACEMENT_3D ( 'NONE', #26548, #42152, #15580 ) ;
#19139 = CARTESIAN_POINT ( 'NONE',  ( -27.27855387000350262, 10.59660315834921640, 5.631341004100471892 ) ) ;
#19141 = DIRECTION ( 'NONE',  ( -0.2475719085175093481, -0.000000000000000000, -0.9688695217174488894 ) ) ;
#19142 = ADVANCED_FACE ( 'NONE', ( #58272 ), #14010, .T. ) ;
#19143 = CARTESIAN_POINT ( 'NONE',  ( -41.00000000000000711, -1.694065894508600678E-18, 0.000000000000000000 ) ) ;
#19144 = AXIS2_PLACEMENT_3D ( 'NONE', #42464, #11899, #58454 ) ;
#19145 = ORIENTED_EDGE ( 'NONE', *, *, #18844, .F. ) ;
#19146 = ADVANCED_FACE ( 'NONE', ( #58952 ), #46797, .F. ) ;
#19147 = ORIENTED_EDGE ( 'NONE', *, *, #45329, .T. ) ;
#19148 = DIRECTION ( 'NONE',  ( -1.000000000000000000, 0.000000000000000000, 0.000000000000000000 ) ) ;
#19149 = CARTESIAN_POINT ( 'NONE',  ( 35.00000000000000000, 4.705694406421931860E-17, -3.469127814946512892E-15 ) ) ;
#19150 = AXIS2_PLACEMENT_3D ( 'NONE', #58397, #11837, #12822 ) ;
#19151 = CARTESIAN_POINT ( 'NONE',  ( 6.511276587883020106, -4.283181266385641450, -12.80273922584868629 ) ) ;
#19152 = CARTESIAN_POINT ( 'NONE',  ( -18.25006854224444908, -9.443202773001939221, -7.404452808139720510 ) ) ;
#19153 = CARTESIAN_POINT ( 'NONE',  ( 5.530133899448235191, -0.004396748047611511757, 0.01536822665454945329 ) ) ;
#19154 = EDGE_CURVE ( 'NONE', #28687, #62520, #56518, .T. ) ;
#19155 = CONICAL_SURFACE ( 'NONE', #61625, 7.938172270156617749, 1.280189991382167047 ) ;
#19156 = CARTESIAN_POINT ( 'NONE',  ( 7.238144804251998465, -5.479122853610516763, -12.33991764455425866 ) ) ;
#19157 = DIRECTION ( 'NONE',  ( 0.000000000000000000, 0.5155538571770230671, -0.8568571761675883858 ) ) ;
#19158 = CARTESIAN_POINT ( 'NONE',  ( 35.00000000000000000, 4.705694406421931860E-17, -3.469127814946512892E-15 ) ) ;
#19159 = CARTESIAN_POINT ( 'NONE',  ( -37.00000000000000711, -6.711949091238219367, 10.84030624090604356 ) ) ;
#19160 = AXIS2_PLACEMENT_3D ( 'NONE', #35765, #60400, #55423 ) ;
#19161 = EDGE_LOOP ( 'NONE', ( #7350, #16655, #23521, #65801 ) ) ;
#19162 = CARTESIAN_POINT ( 'NONE',  ( 0.2653519991613847440, 12.05632699103097494, 2.148211862902952074 ) ) ;
#19163 = CARTESIAN_POINT ( 'NONE',  ( 5.515188684475870851, -0.005194992164431471750, -0.001283816547384778904 ) ) ;
#19164 = CARTESIAN_POINT ( 'NONE',  ( 2.655192694323472047, -6.604353705985011480, -6.969384012965773145 ) ) ;
#19165 = CIRCLE ( 'NONE', #27655, 2.899999999999997691 ) ;
#19166 = CIRCLE ( 'NONE', #35046, 12.18650000000000055 ) ;
#19167 = AXIS2_PLACEMENT_3D ( 'NONE', #41170, #31217, #638 ) ;
#19168 = CARTESIAN_POINT ( 'NONE',  ( 2.373367633546871414, -6.557448619657612277, -3.994744114396157286 ) ) ;
#19169 = CARTESIAN_POINT ( 'NONE',  ( 1.104777566491150553, -4.729982681549460999, -11.59867774809549701 ) ) ;
#19170 = EDGE_LOOP ( 'NONE', ( #7243, #55004, #13299, #31394 ) ) ;
#19171 = FACE_OUTER_BOUND ( 'NONE', #37070, .T. ) ;
#19172 = CARTESIAN_POINT ( 'NONE',  ( 0.3665391374699467075, -0.2638605131388012115, 12.27992639892678284 ) ) ;
#19173 = CARTESIAN_POINT ( 'NONE',  ( -2.112161198359963521, -25.77267402162640408, -15.59357793625674660 ) ) ;
#19174 = VERTEX_POINT ( 'NONE', #13362 ) ;
#19175 = DIRECTION ( 'NONE',  ( 0.000000000000000000, 0.01356324068818000848, -0.9999080150203990547 ) ) ;
#19176 = CARTESIAN_POINT ( 'NONE',  ( -27.74257803791718402, -13.27121782910951353, -2.535736602234749171 ) ) ;
#19177 = CARTESIAN_POINT ( 'NONE',  ( -35.00000000000000000, 12.17626345777664376, -0.4993900848166082374 ) ) ;
#19178 = DIRECTION ( 'NONE',  ( 0.000000000000000000, -0.01356324068817998940, 0.9999080150203990547 ) ) ;
#19179 = CARTESIAN_POINT ( 'NONE',  ( -9.843523776114507129, -12.00711794201791172, -6.183557206441264498 ) ) ;
#19180 = AXIS2_PLACEMENT_3D ( 'NONE', #30068, #54384, #13457 ) ;
#19181 = EDGE_CURVE ( 'NONE', #30137, #2564, #17142, .T. ) ;
#19182 = CARTESIAN_POINT ( 'NONE',  ( 1.104777566491141449, 12.24382064406183268, -2.644034362100568192 ) ) ;
#19183 = ORIENTED_EDGE ( 'NONE', *, *, #8866, .T. ) ;
#19184 = CIRCLE ( 'NONE', #35106, 12.18650000000000055 ) ;
#19185 = CARTESIAN_POINT ( 'NONE',  ( 2.242819959140646358, -7.208832857235893954, 2.514828506625046423 ) ) ;
#19186 = VECTOR ( 'NONE', #37618, 1000.000000000000114 ) ;
#19187 = CARTESIAN_POINT ( 'NONE',  ( 1.000000000000000888, 6.997684042076945055, -2.698595569414161677 ) ) ;
#19188 = CARTESIAN_POINT ( 'NONE',  ( -14.79101291032822019, 8.427946710105242545, -10.54609284329090535 ) ) ;
#19189 = CARTESIAN_POINT ( 'NONE',  ( 2.000000000000001776, 0.000000000000000000, 0.000000000000000000 ) ) ;
#19190 = FACE_OUTER_BOUND ( 'NONE', #10067, .T. ) ;
#19191 = CARTESIAN_POINT ( 'NONE',  ( 3.152665057734127529, -7.281573230474269742, -3.161213418913537687 ) ) ;
#19192 = AXIS2_PLACEMENT_3D ( 'NONE', #63962, #13416, #14070 ) ;
#19193 = CARTESIAN_POINT ( 'NONE',  ( 37.00000000000000711, 12.49688848680884234, -2.527899948230686977 ) ) ;
#19194 = CARTESIAN_POINT ( 'NONE',  ( 2.247112776669946133, 1.211104213049043032, -7.539676020704888515 ) ) ;
#19195 = ORIENTED_EDGE ( 'NONE', *, *, #5471, .F. ) ;
#19196 = EDGE_LOOP ( 'NONE', ( #39225, #47840, #47941, #25065 ) ) ;
#19197 = DIRECTION ( 'NONE',  ( 1.000000000000000000, 0.000000000000000000, 0.000000000000000000 ) ) ;
#19198 = AXIS2_PLACEMENT_3D ( 'NONE', #60856, #15296, #35572 ) ;
#19199 = ORIENTED_EDGE ( 'NONE', *, *, #42241, .F. ) ;
#19200 = DIRECTION ( 'NONE',  ( -0.3865475372811021937, 0.9114221272958270559, 0.1410344188397433807 ) ) ;
#19201 = ADVANCED_FACE ( 'NONE', ( #59918 ), #60015, .F. ) ;
#19202 = FACE_OUTER_BOUND ( 'NONE', #38041, .T. ) ;
#19203 = ORIENTED_EDGE ( 'NONE', *, *, #51971, .F. ) ;
#19205 = CARTESIAN_POINT ( 'NONE',  ( 3.152665057734126197, -1.848755561852092333, 7.719888720907804647 ) ) ;
#19204 = VECTOR ( 'NONE', #53902, 999.9999999999998863 ) ;
#19206 = CARTESIAN_POINT ( 'NONE',  ( 3.152665057734119536, 1.848755561852129858, -7.719888720907784219 ) ) ;
#19207 = EDGE_CURVE ( 'NONE', #20112, #395, #34115, .T. ) ;
#19208 = CARTESIAN_POINT ( 'NONE',  ( 24.52718794524056278, -2.675527299323683383, 13.23708621095143201 ) ) ;
#19209 = VERTEX_POINT ( 'NONE', #29312 ) ;
#19210 = VERTEX_POINT ( 'NONE', #9669 ) ;
#19211 = CARTESIAN_POINT ( 'NONE',  ( 2.269879328256730222, -7.232310762824150530, -2.474479066008294037 ) ) ;
#19212 = VECTOR ( 'NONE', #29091, 1000.000000000000000 ) ;
#19213 = EDGE_CURVE ( 'NONE', #14308, #45693, #12105, .T. ) ;
#19214 = CARTESIAN_POINT ( 'NONE',  ( -22.00000000000000711, -20.00000000000000000, 2.449293598294706907E-15 ) ) ;
#19215 = ORIENTED_EDGE ( 'NONE', *, *, #28704, .T. ) ;
#19216 = DIRECTION ( 'NONE',  ( 1.000000000000000000, -0.000000000000000000, 0.000000000000000000 ) ) ;
#19217 = ORIENTED_EDGE ( 'NONE', *, *, #51064, .T. ) ;
#19218 = CARTESIAN_POINT ( 'NONE',  ( -35.00000000000000000, 11.10408318471068512, -6.265926637539371846 ) ) ;
#19219 = CIRCLE ( 'NONE', #13878, 7.499999999999988454 ) ;
#19220 = CARTESIAN_POINT ( 'NONE',  ( 0.000000000000000000, -6.936109781200648250, -2.853135311045116307 ) ) ;
#19221 = DIRECTION ( 'NONE',  ( 0.000000000000000000, 0.01356324068817992001, -0.9999080150203990547 ) ) ;
#19222 = TOROIDAL_SURFACE ( 'NONE', #9665, 5.000000000000000888, 19.00000000000000000 ) ;
#19223 = DIRECTION ( 'NONE',  ( -1.000000000000000000, 0.000000000000000000, 0.000000000000000000 ) ) ;
#19224 = VERTEX_POINT ( 'NONE', #380 ) ;
#19225 =( BOUNDED_CURVE ( )  B_SPLINE_CURVE ( 3, ( #48658, #13391, #33675, #59947 ),
 .UNSPECIFIED., .F., .F. ) 
 B_SPLINE_CURVE_WITH_KNOTS ( ( 4, 4 ),
 ( 5.020709631077181712, 5.030260039792340265 ),
 .UNSPECIFIED. ) 
 CURVE ( )  GEOMETRIC_REPRESENTATION_ITEM ( )  RATIONAL_B_SPLINE_CURVE ( ( 1.000000000000000000, 0.9999923991555577096, 0.9999923991555577096, 1.000000000000000000 ) ) 
 REPRESENTATION_ITEM ( '' )  );
#19226 = CARTESIAN_POINT ( 'NONE',  ( 2.256373768223414622, 7.638251659827605344, -0.1329433694244546993 ) ) ;
#19227 = VECTOR ( 'NONE', #61022, 1000.000000000000114 ) ;
#19228 = EDGE_CURVE ( 'NONE', #40566, #7359, #9675, .T. ) ;
#19229 = CARTESIAN_POINT ( 'NONE',  ( 0.2653519789438759102, 7.854827495960937433, -9.395292406847850941 ) ) ;
#19230 = CARTESIAN_POINT ( 'NONE',  ( 0.2653519890518156177, -9.381125756446625275, 7.871710682401878323 ) ) ;
#19231 = EDGE_CURVE ( 'NONE', #24479, #13166, #49024, .T. ) ;
#19232 = DIRECTION ( 'NONE',  ( -0.3865475372811021382, -0.4442537292684440309, 0.8082200352954602707 ) ) ;
#19233 = DIRECTION ( 'NONE',  ( 0.000000000000000000, 0.1764146379942750087, 0.9843159429275484262 ) ) ;
#19234 = CARTESIAN_POINT ( 'NONE',  ( 0.7446945582528475827, 0.3561743995939678498, -12.40088838630016888 ) ) ;
#19235 = CARTESIAN_POINT ( 'NONE',  ( 1.719304012338199517, 12.70777170743846796, 0.7661785589580254463 ) ) ;
#19236 = CARTESIAN_POINT ( 'NONE',  ( 1.000000000000000888, -5.217815162096861137, 5.387430271863535403 ) ) ;
#19237 = CARTESIAN_POINT ( 'NONE',  ( -35.00000000000000000, 5.391785509270962784, 10.43555801961477236 ) ) ;
#19238 = ADVANCED_FACE ( 'NONE', ( #64869 ), #3899, .F. ) ;
#19239 = CIRCLE ( 'NONE', #46865, 12.18650000000000055 ) ;
#19240 = AXIS2_PLACEMENT_3D ( 'NONE', #48391, #43358, #54683 ) ;
#19241 = EDGE_LOOP ( 'NONE', ( #30416, #52508, #2523, #38093 ) ) ;
#19242 = CARTESIAN_POINT ( 'NONE',  ( -37.00000000000000711, 5.143145423404449801, -11.66664283989674367 ) ) ;
#19244 = EDGE_CURVE ( 'NONE', #49413, #55105, #30299, .T. ) ;
#19243 = AXIS2_PLACEMENT_3D ( 'NONE', #34444, #8851, #4190 ) ;
#19245 = AXIS2_PLACEMENT_3D ( 'NONE', #13082, #18743, #34002 ) ;
#19246 = ORIENTED_EDGE ( 'NONE', *, *, #35481, .T. ) ;
#19247 = DIRECTION ( 'NONE',  ( 1.000000000000000000, 0.000000000000000000, 0.000000000000000000 ) ) ;
#19248 = LINE ( 'NONE', #9914, #58492 ) ;
#19249 = CARTESIAN_POINT ( 'NONE',  ( 5.515539859299206427, -0.005142293699651846045, 0.003193223631739306942 ) ) ;
#19250 = CIRCLE ( 'NONE', #14953, 5.000000000000002665 ) ;
#19251 = EDGE_CURVE ( 'NONE', #21398, #58025, #2309, .T. ) ;
#19252 = CARTESIAN_POINT ( 'NONE',  ( 0.2652384770603654629, 9.338499095996429133, 7.922175044417011591 ) ) ;
#19253 = DIRECTION ( 'NONE',  ( -1.000000000000000000, 0.000000000000000000, 0.000000000000000000 ) ) ;
#19254 = VERTEX_POINT ( 'NONE', #30606 ) ;
#19255 = CARTESIAN_POINT ( 'NONE',  ( -11.40165637463000614, -7.508992741355387857, -11.21895841913464587 ) ) ;
#19257 = CIRCLE ( 'NONE', #38370, 5.000000000000001776 ) ;
#19256 = CARTESIAN_POINT ( 'NONE',  ( -35.00000000000000000, -11.35427606708809556, 4.426194442447198618 ) ) ;
#19258 = CARTESIAN_POINT ( 'NONE',  ( -27.08430418657510685, 2.086666645150422994, 0.9470735946412616180 ) ) ;
#19259 = DIRECTION ( 'NONE',  ( -1.000000000000000000, 0.000000000000000000, 0.000000000000000000 ) ) ;
#19260 = CIRCLE ( 'NONE', #64895, 5.000000000000000000 ) ;
#19261 = CARTESIAN_POINT ( 'NONE',  ( -47.00000000000000711, 0.000000000000000000, 0.000000000000000000 ) ) ;
#19262 = ORIENTED_EDGE ( 'NONE', *, *, #20837, .T. ) ;
#19263 = DIRECTION ( 'NONE',  ( 0.000000000000000000, 0.000000000000000000, -1.000000000000000000 ) ) ;
#19264 = ORIENTED_EDGE ( 'NONE', *, *, #53695, .F. ) ;
#19265 = CIRCLE ( 'NONE', #50073, 5.000000000000000000 ) ;
#19266 = CARTESIAN_POINT ( 'NONE',  ( 2.907497136250074554, 5.781215374755592329, -5.319973245618017543 ) ) ;
#19267 = DIRECTION ( 'NONE',  ( -1.000000000000000000, -0.000000000000000000, -0.000000000000000000 ) ) ;
#19268 = CYLINDRICAL_SURFACE ( 'NONE', #27822, 12.18649999999999878 ) ;
#19269 = FACE_OUTER_BOUND ( 'NONE', #55831, .T. ) ;
#19270 = CIRCLE ( 'NONE', #44736, 12.74999999999999822 ) ;
#19271 = EDGE_CURVE ( 'NONE', #16301, #25549, #19308, .T. ) ;
#19272 = VECTOR ( 'NONE', #47075, 1000.000000000000000 ) ;
#19273 = ORIENTED_EDGE ( 'NONE', *, *, #21341, .F. ) ;
#19274 = ORIENTED_EDGE ( 'NONE', *, *, #7991, .F. ) ;
#19275 = DIRECTION ( 'NONE',  ( 0.000000000000000000, 0.01356324068817998940, -0.9999080150203990547 ) ) ;
#19276 = LINE ( 'NONE', #39544, #47856 ) ;
#19277 = LINE ( 'NONE', #20243, #51296 ) ;
#19278 = DIRECTION ( 'NONE',  ( 0.3939253465568944290, 0.7103112711423489323, -0.5833358547425069318 ) ) ;
#19279 = CARTESIAN_POINT ( 'NONE',  ( 2.969415267405009384, 6.619534278261656191, -4.269695207293545458 ) ) ;
#19280 = LINE ( 'NONE', #49866, #56154 ) ;
#19281 = CARTESIAN_POINT ( 'NONE',  ( 0.9296196016834407105, -12.46069139398445103, -0.4155906739600075950 ) ) ;
#19282 = VERTEX_POINT ( 'NONE', #27270 ) ;
#19283 = EDGE_CURVE ( 'NONE', #14292, #61981, #46868, .T. ) ;
#19284 = EDGE_LOOP ( 'NONE', ( #60584, #6041, #29875, #58984 ) ) ;
#19285 = ORIENTED_EDGE ( 'NONE', *, *, #7792, .F. ) ;
#19286 = CARTESIAN_POINT ( 'NONE',  ( 2.177405672431599992, -8.997150696569100603, -6.668684901899186279 ) ) ;
#19287 = CIRCLE ( 'NONE', #62796, 5.000000000000000888 ) ;
#19288 = AXIS2_PLACEMENT_3D ( 'NONE', #28653, #48963, #18375 ) ;
#19289 = CARTESIAN_POINT ( 'NONE',  ( 2.903928887688913107, 8.753847148604096517, -0.5297564406060942810 ) ) ;
#19290 = EDGE_LOOP ( 'NONE', ( #45139, #39332, #17759, #63534 ) ) ;
#19291 = DIRECTION ( 'NONE',  ( -1.000000000000000000, 0.000000000000000000, 0.000000000000000000 ) ) ;
#19292 = FACE_BOUND ( 'NONE', #64168, .T. ) ;
#19293 = ORIENTED_EDGE ( 'NONE', *, *, #47441, .F. ) ;
#19294 = CARTESIAN_POINT ( 'NONE',  ( 3.152665057734119536, 7.281573230474295499, 3.161213418913482620 ) ) ;
#19295 = FACE_OUTER_BOUND ( 'NONE', #13393, .T. ) ;
#19296 = CARTESIAN_POINT ( 'NONE',  ( 5.887998910375843664, -9.753598045600698541, 7.002626515174585897 ) ) ;
#19297 = ORIENTED_EDGE ( 'NONE', *, *, #29269, .T. ) ;
#19298 = AXIS2_PLACEMENT_3D ( 'NONE', #34714, #63665, #13150 ) ;
#19299 = VERTEX_POINT ( 'NONE', #36915 ) ;
#19300 = LINE ( 'NONE', #50225, #19347 ) ;
#19301 = ADVANCED_FACE ( 'NONE', ( #11646 ), #21646, .T. ) ;
#19302 = VERTEX_POINT ( 'NONE', #1028 ) ;
#19303 = DIRECTION ( 'NONE',  ( 1.000000000000000000, 0.000000000000000000, 0.000000000000000000 ) ) ;
#19304 = ORIENTED_EDGE ( 'NONE', *, *, #8004, .T. ) ;
#19305 = AXIS2_PLACEMENT_3D ( 'NONE', #18171, #12184, #38441 ) ;
#19306 = ORIENTED_EDGE ( 'NONE', *, *, #6020, .F. ) ;
#19307 = ORIENTED_EDGE ( 'NONE', *, *, #60490, .F. ) ;
#19308 = B_SPLINE_CURVE_WITH_KNOTS ( 'NONE', 3,
 ( #20313, #40598, #50917, #40933, #15330, #5362, #47253, #30944, #21295, #31593, #32252, #16966, #17309 ),
 .UNSPECIFIED., .F., .F.,
 ( 4, 3, 3, 3, 4 ),
 ( 2.168404344971008868E-18, 6.607593386745438881E-05, 0.0001321518677373503738, 0.0001982171734706192063, 0.0002642860854759491508 ),
 .UNSPECIFIED. ) ;
#19309 = CARTESIAN_POINT ( 'NONE',  ( 0.2653141334712562083, 11.52266042163707560, 4.147025708564464175 ) ) ;
#19310 = CARTESIAN_POINT ( 'NONE',  ( -35.00000000000000000, 2.696588552979059639, 12.46157735505190089 ) ) ;
#19311 = LINE ( 'NONE', #44899, #47880 ) ;
#19312 = FACE_OUTER_BOUND ( 'NONE', #21841, .T. ) ;
#19313 = VERTEX_POINT ( 'NONE', #52572 ) ;
#19314 = CARTESIAN_POINT ( 'NONE',  ( 2.253265082352433168, -7.132841660187145827, -2.732639326785877731 ) ) ;
#19315 = AXIS2_PLACEMENT_3D ( 'NONE', #42341, #22082, #26421 ) ;
#19316 = EDGE_LOOP ( 'NONE', ( #32143, #61466, #62175, #14355 ) ) ;
#19317 = DIRECTION ( 'NONE',  ( 0.000000000000000000, 0.01356324068817998940, -0.9999080150203989437 ) ) ;
#19318 = CARTESIAN_POINT ( 'NONE',  ( 0.000000000000000000, -6.164400007374799095, 2.900694413976478536 ) ) ;
#19319 = AXIS2_PLACEMENT_3D ( 'NONE', #29024, #44961, #18407 ) ;
#19320 = CIRCLE ( 'NONE', #16123, 7.499999999999988454 ) ;
#19321 = VERTEX_POINT ( 'NONE', #5706 ) ;
#19322 = DIRECTION ( 'NONE',  ( 0.000000000000000000, 0.01356324068817992175, -0.9999080150203990547 ) ) ;
#19323 = CARTESIAN_POINT ( 'NONE',  ( -35.00000000000000000, 0.000000000000000000, 0.000000000000000000 ) ) ;
#19324 = DIRECTION ( 'NONE',  ( -1.000000000000000000, -0.000000000000000000, -0.000000000000000000 ) ) ;
#19325 = ADVANCED_FACE ( 'NONE', ( #56562 ), #23498, .F. ) ;
#19326 = VERTEX_POINT ( 'NONE', #31918 ) ;
#19327 = CIRCLE ( 'NONE', #37337, 6.936499999999993449 ) ;
#19328 = AXIS2_PLACEMENT_3D ( 'NONE', #30265, #56178, #10616 ) ;
#19329 = VECTOR ( 'NONE', #5791, 1000.000000000000000 ) ;
#19330 = ORIENTED_EDGE ( 'NONE', *, *, #32193, .F. ) ;
#19331 = CARTESIAN_POINT ( 'NONE',  ( 2.242418902651940549, -7.634109827927228586, 0.09970190380430356270 ) ) ;
#19332 = ADVANCED_FACE ( 'NONE', ( #42537 ), #15965, .T. ) ;
#19333 = ORIENTED_EDGE ( 'NONE', *, *, #54609, .T. ) ;
#19334 = CARTESIAN_POINT ( 'NONE',  ( -36.00000000000000711, 9.913596905230114942, 8.017674001891819557 ) ) ;
#19335 = CARTESIAN_POINT ( 'NONE',  ( 37.00000000000000711, -11.66953048682396954, 3.511814412392239682 ) ) ;
#19336 = CARTESIAN_POINT ( 'NONE',  ( -12.53824232977090603, -28.27004406456470775, 13.15159876983787335 ) ) ;
#19337 = EDGE_CURVE ( 'NONE', #30904, #7231, #52238, .T. ) ;
#19338 = CARTESIAN_POINT ( 'NONE',  ( 0.2648978790185584908, -9.295532325666394868, -7.972372351883127095 ) ) ;
#19339 = CARTESIAN_POINT ( 'NONE',  ( 0.8320506296491624321, -9.275353261146591421, 8.282532257448787405 ) ) ;
#19340 = VERTEX_POINT ( 'NONE', #704 ) ;
#19341 = CARTESIAN_POINT ( 'NONE',  ( 2.241537034860907163, 3.821322318518465266, -6.609284473755296929 ) ) ;
#19342 = CARTESIAN_POINT ( 'NONE',  ( 0.9296196016828991437, 1.754499435240217453, 12.34355205587671200 ) ) ;
#19343 = AXIS2_PLACEMENT_3D ( 'NONE', #39324, #9722, #34656 ) ;
#19344 = CIRCLE ( 'NONE', #56498, 12.75000000000000178 ) ;
#19345 = CIRCLE ( 'NONE', #64974, 12.18649999999999878 ) ;
#19346 = CARTESIAN_POINT ( 'NONE',  ( -10.77421046970567708, -27.84620353580639218, -14.04190754122875973 ) ) ;
#19347 = VECTOR ( 'NONE', #4684, 1000.000000000000000 ) ;
#19348 = CARTESIAN_POINT ( 'NONE',  ( -22.59969328935894239, 4.594269189967342015, 0.7214993884004420321 ) ) ;
#19349 = CARTESIAN_POINT ( 'NONE',  ( -22.27384469013076185, 1.508555848190777926, -3.358914544760239540 ) ) ;
#19350 = DIRECTION ( 'NONE',  ( 1.000000000000000000, -0.000000000000000000, 0.000000000000000000 ) ) ;
#19351 = CARTESIAN_POINT ( 'NONE',  ( -35.00000000000000000, 9.348667969174405457, 7.817492529713891081 ) ) ;
#19352 = ADVANCED_FACE ( 'NONE', ( #20962, #56902 ), #26952, .F. ) ;
#19353 = B_SPLINE_CURVE_WITH_KNOTS ( 'NONE', 3,
 ( #48009, #44307, #27704, #43004, #63279, #28370, #3121, #43653, #38685, #8416 ),
 .UNSPECIFIED., .F., .F.,
 ( 4, 3, 3, 4 ),
 ( 0.000000000000000000, 6.607638129004453646E-05, 9.911389841680473469E-05, 0.0001667630577588630702 ),
 .UNSPECIFIED. ) ;
#19354 = ORIENTED_EDGE ( 'NONE', *, *, #21724, .T. ) ;
#19355 = CARTESIAN_POINT ( 'NONE',  ( -27.08430418657512107, -1.333569526608691991, -1.863523114788429691 ) ) ;
#19356 = AXIS2_PLACEMENT_3D ( 'NONE', #22250, #42511, #17275 ) ;
#19357 = EDGE_CURVE ( 'NONE', #44256, #5538, #52644, .T. ) ;
#19358 = ORIENTED_EDGE ( 'NONE', *, *, #25830, .F. ) ;
#19359 = CARTESIAN_POINT ( 'NONE',  ( 0.2834382757448032919, 1.927645269571043984, -12.09963924911732391 ) ) ;
#19360 = DIRECTION ( 'NONE',  ( -1.000000000000000000, -0.000000000000000000, 0.000000000000000000 ) ) ;
#19361 = DIRECTION ( 'NONE',  ( 0.000000000000000000, -0.01356324068817998940, 0.9999080150203990547 ) ) ;
#19362 = CARTESIAN_POINT ( 'NONE',  ( 2.284126774969132523, -1.171808575344847503, -7.558363379199810161 ) ) ;
#19363 = VERTEX_POINT ( 'NONE', #51587 ) ;
#19364 = EDGE_CURVE ( 'NONE', #52959, #44677, #46572, .T. ) ;
#19365 = ORIENTED_EDGE ( 'NONE', *, *, #42176, .T. ) ;
#19366 = ORIENTED_EDGE ( 'NONE', *, *, #44004, .F. ) ;
#19367 = CARTESIAN_POINT ( 'NONE',  ( 29.61403717302718519, -5.490544854489863624, 10.71644165484303457 ) ) ;
#19368 = CIRCLE ( 'NONE', #34208, 5.000000000000000888 ) ;
#19370 = CIRCLE ( 'NONE', #56541, 19.00000000000000000 ) ;
#19369 = CARTESIAN_POINT ( 'NONE',  ( -27.73962451255497541, 10.56031772329400731, -5.706676279454582890 ) ) ;
#19371 = B_SPLINE_CURVE_WITH_KNOTS ( 'NONE', 3,
 ( #24900, #15237, #40848, #293, #41149, #30211 ),
 .UNSPECIFIED., .F., .F.,
 ( 4, 2, 4 ),
 ( 0.000000000000000000, 0.0004528561986909433257, 0.0009057123973818866514 ),
 .UNSPECIFIED. ) ;
#19372 = ORIENTED_EDGE ( 'NONE', *, *, #30564, .T. ) ;
#19373 = CARTESIAN_POINT ( 'NONE',  ( 2.899286259009677291, 5.780956296532521854, 5.316140236670786834 ) ) ;
#19374 = CARTESIAN_POINT ( 'NONE',  ( 2.241352910868909643, 3.744764251557084922, -6.652881166698471738 ) ) ;
#19375 = DIRECTION ( 'NONE',  ( -1.000000000000000000, 0.000000000000000000, 0.000000000000000000 ) ) ;
#19376 = CARTESIAN_POINT ( 'NONE',  ( 2.589278595513357484, -2.423168677231944734, 7.361833592938436865 ) ) ;
#19377 = ORIENTED_EDGE ( 'NONE', *, *, #50298, .T. ) ;
#19378 = CARTESIAN_POINT ( 'NONE',  ( 37.00000000000000711, 4.705694406421931860E-17, -3.469127814946512892E-15 ) ) ;
#19379 = CARTESIAN_POINT ( 'NONE',  ( 1.845799476742940870, -28.15607794640831330, -13.84328548073280629 ) ) ;
#19380 = DIRECTION ( 'NONE',  ( 1.000000000000000000, 0.000000000000000000, 0.000000000000000000 ) ) ;
#19382 = VERTEX_POINT ( 'NONE', #3007 ) ;
#19381 = DIRECTION ( 'NONE',  ( 0.000000000000000000, 0.000000000000000000, 1.000000000000000000 ) ) ;
#19383 = EDGE_CURVE ( 'NONE', #52549, #23040, #43210, .T. ) ;
#19384 = EDGE_CURVE ( 'NONE', #31007, #62530, #9746, .T. ) ;
#19385 = ORIENTED_EDGE ( 'NONE', *, *, #28077, .F. ) ;
#19386 = CYLINDRICAL_SURFACE ( 'NONE', #64509, 12.75000000000000178 ) ;
#19387 = ORIENTED_EDGE ( 'NONE', *, *, #13417, .F. ) ;
#19388 = CARTESIAN_POINT ( 'NONE',  ( -29.68541646480307605, -0.9852353464181112797, -11.96735172698778626 ) ) ;
#19389 = STYLED_ITEM ( 'NONE', ( #63749 ), #29035 ) ;
#19390 = CARTESIAN_POINT ( 'NONE',  ( 13.03306451323199155, -11.51507849167763631, -3.383716369314965888 ) ) ;
#19391 = EDGE_CURVE ( 'NONE', #44608, #60941, #38563, .T. ) ;
#19392 = FACE_OUTER_BOUND ( 'NONE', #6944, .T. ) ;
#19393 = DIRECTION ( 'NONE',  ( 0.000000000000000000, -0.3193015301359872216, 0.9476531711827999027 ) ) ;
#19394 = CIRCLE ( 'NONE', #58662, 12.18650000000000233 ) ;
#19395 = CARTESIAN_POINT ( 'NONE',  ( 36.00000000000000711, -0.3137578094510115045, -12.74613886779085092 ) ) ;
#19396 = CARTESIAN_POINT ( 'NONE',  ( -8.071794517351818854, -2.346129881092677838, -13.29681922941937344 ) ) ;
#19397 = CARTESIAN_POINT ( 'NONE',  ( 0.3218525148189793628, -3.964374483810575445, -11.60666749448228607 ) ) ;
#19399 = ORIENTED_EDGE ( 'NONE', *, *, #42682, .F. ) ;
#19398 = DIRECTION ( 'NONE',  ( 0.000000000000000000, -0.9718671068226484300, 0.2355298848897411923 ) ) ;
#19400 = ORIENTED_EDGE ( 'NONE', *, *, #51870, .T. ) ;
#19401 = LINE ( 'NONE', #20043, #876 ) ;
#19402 = ORIENTED_EDGE ( 'NONE', *, *, #47300, .F. ) ;
#19403 = CIRCLE ( 'NONE', #35322, 12.74999999999999822 ) ;
#19404 = EDGE_LOOP ( 'NONE', ( #9423, #62304, #59205, #58321 ) ) ;
#19405 = CARTESIAN_POINT ( 'NONE',  ( 1.194176325881338263, 1.672143286119727179, -12.44396189284383070 ) ) ;
#19406 = DIRECTION ( 'NONE',  ( -1.000000000000000000, -0.000000000000000000, -0.000000000000000000 ) ) ;
#19407 = DIRECTION ( 'NONE',  ( 0.000000000000000000, 0.000000000000000000, -1.000000000000000000 ) ) ;
#19408 = CARTESIAN_POINT ( 'NONE',  ( 0.2651627923886311078, 0.08809136839532921703, -12.24583724871548540 ) ) ;
#19409 = CARTESIAN_POINT ( 'NONE',  ( 21.90174657591892071, 13.47998113580524659, -0.7349207973210680755 ) ) ;
#19410 = EDGE_CURVE ( 'NONE', #64921, #33298, #58266, .T. ) ;
#19411 = LINE ( 'NONE', #4788, #14013 ) ;
#19412 = DIRECTION ( 'NONE',  ( -1.000000000000000000, -0.000000000000000000, 0.000000000000000000 ) ) ;
#19413 = EDGE_CURVE ( 'NONE', #10611, #42570, #57512, .T. ) ;
#19414 = AXIS2_PLACEMENT_3D ( 'NONE', #51565, #26269, #46544 ) ;
#19415 = ORIENTED_EDGE ( 'NONE', *, *, #64656, .F. ) ;
#19416 = DIRECTION ( 'NONE',  ( 0.000000000000000000, -0.01356324068817998940, 0.9999080150203990547 ) ) ;
#19417 = DIRECTION ( 'NONE',  ( 1.000000000000000000, 0.000000000000000000, -0.000000000000000000 ) ) ;
#19418 = CARTESIAN_POINT ( 'NONE',  ( 1.634816307074518305, 12.36483956257112204, 2.910502128620317208 ) ) ;
#19419 = ORIENTED_EDGE ( 'NONE', *, *, #2204, .F. ) ;
#19420 = CIRCLE ( 'NONE', #59912, 5.000000000000001776 ) ;
#19421 = AXIS2_PLACEMENT_3D ( 'NONE', #20255, #51538, #41509 ) ;
#19422 = AXIS2_PLACEMENT_3D ( 'NONE', #40084, #4871, #20144 ) ;
#19423 = VECTOR ( 'NONE', #41, 1000.000000000000000 ) ;
#19424 =( BOUNDED_CURVE ( )  B_SPLINE_CURVE ( 3, ( #21643, #26610, #377, #20656 ),
 .UNSPECIFIED., .F., .F. ) 
 B_SPLINE_CURVE_WITH_KNOTS ( ( 4, 4 ),
 ( 4.417647514148206334, 4.442076100497985180 ),
 .UNSPECIFIED. ) 
 CURVE ( )  GEOMETRIC_REPRESENTATION_ITEM ( )  RATIONAL_B_SPLINE_CURVE ( ( 1.000000000000000000, 0.9999502709656691302, 0.9999502709656691302, 1.000000000000000000 ) ) 
 REPRESENTATION_ITEM ( '' )  );
#19425 = CARTESIAN_POINT ( 'NONE',  ( -11.22840640265205892, -5.993912459648431224, 12.09830627065808173 ) ) ;
#19426 = CARTESIAN_POINT ( 'NONE',  ( 35.00000000000000000, -10.63508530065518443, 4.986700593229810963 ) ) ;
#19427 = ORIENTED_EDGE ( 'NONE', *, *, #13297, .F. ) ;
#19428 = DIRECTION ( 'NONE',  ( 0.000000000000000000, 0.01356324068817992175, -0.9999080150203990547 ) ) ;
#19429 = CARTESIAN_POINT ( 'NONE',  ( 0.000000000000000000, 5.107597897712416568, -4.693343793638371508 ) ) ;
#19430 = DIRECTION ( 'NONE',  ( 1.000000000000000000, -0.000000000000000000, 0.000000000000000000 ) ) ;
#19431 = AXIS2_PLACEMENT_3D ( 'NONE', #62020, #28987, #32705 ) ;
#19432 = AXIS2_PLACEMENT_3D ( 'NONE', #3987, #24251, #35198 ) ;
#19433 = CARTESIAN_POINT ( 'NONE',  ( -27.35552965826137140, 1.773915698030573473, -2.548625910254528559 ) ) ;
#19434 = CARTESIAN_POINT ( 'NONE',  ( 2.665405856346786173, -0.5773576323838383040, 9.549966053095403140 ) ) ;
#19435 = ADVANCED_FACE ( 'NONE', ( #13604 ), #22625, .T. ) ;
#19436 = ORIENTED_EDGE ( 'NONE', *, *, #34802, .T. ) ;
#19437 = DIRECTION ( 'NONE',  ( 1.000000000000000000, -0.000000000000000000, -0.000000000000000000 ) ) ;
#19438 = DIRECTION ( 'NONE',  ( 0.000000000000000000, 0.01356324068817991828, -0.9999080150203990547 ) ) ;
#19439 = CIRCLE ( 'NONE', #14098, 12.75000000000000178 ) ;
#19440 = DIRECTION ( 'NONE',  ( 0.000000000000000000, 0.000000000000000000, 1.000000000000000000 ) ) ;
#19441 = ORIENTED_EDGE ( 'NONE', *, *, #59646, .F. ) ;
#19442 = DIRECTION ( 'NONE',  ( 0.000000000000000000, -0.01356324068817991828, 0.9999080150203990547 ) ) ;
#19443 = CARTESIAN_POINT ( 'NONE',  ( -35.00000000000000000, 0.000000000000000000, 0.000000000000000000 ) ) ;
#19444 = EDGE_LOOP ( 'NONE', ( #32542, #16242, #47709, #3931 ) ) ;
#19445 = ORIENTED_EDGE ( 'NONE', *, *, #63752, .T. ) ;
#19446 = ORIENTED_EDGE ( 'NONE', *, *, #5028, .T. ) ;
#19447 = DIRECTION ( 'NONE',  ( 0.000000000000000000, -0.01356324068817992175, 0.9999080150203990547 ) ) ;
#19448 = EDGE_CURVE ( 'NONE', #56955, #25443, #6576, .T. ) ;
#19449 = VERTEX_POINT ( 'NONE', #3339 ) ;
#19450 = CARTESIAN_POINT ( 'NONE',  ( 2.000000000000001776, -6.664893814313753495, 3.439359016433473748 ) ) ;
#19451 = CARTESIAN_POINT ( 'NONE',  ( 0.2653519991613820794, 6.142165520908316800, -10.59450977800975480 ) ) ;
#19452 = DIRECTION ( 'NONE',  ( 0.9946347501772865307, 0.000000000000000000, -0.1034490876700550205 ) ) ;
#19453 = CARTESIAN_POINT ( 'NONE',  ( 0.2648978790185593790, 4.312320170909392125, -11.46165506714223703 ) ) ;
#19454 = CARTESIAN_POINT ( 'NONE',  ( 0.3223008802179273546, -10.74209118105752658, -5.919638939520693199 ) ) ;
#19455 = CARTESIAN_POINT ( 'NONE',  ( 2.241534463349553086, 0.005768439177839456040, 7.634462073473345711 ) ) ;
#19457 = ORIENTED_EDGE ( 'NONE', *, *, #57360, .F. ) ;
#19456 = DIRECTION ( 'NONE',  ( 0.9759340573753173542, 0.2180658516479614117, 0.000000000000000000 ) ) ;
#19458 = CARTESIAN_POINT ( 'NONE',  ( 5.516018279890452902, -0.006440244342253398716, 0.002104829434641079973 ) ) ;
#19459 = ORIENTED_EDGE ( 'NONE', *, *, #22840, .F. ) ;
#19460 = VECTOR ( 'NONE', #65144, 1000.000000000000000 ) ;
#19461 = DIRECTION ( 'NONE',  ( -1.000000000000000000, 0.000000000000000000, -0.000000000000000000 ) ) ;
#19462 = EDGE_LOOP ( 'NONE', ( #18127, #31897, #49857, #16330 ) ) ;
#19463 = ORIENTED_EDGE ( 'NONE', *, *, #64171, .T. ) ;
#19464 = CARTESIAN_POINT ( 'NONE',  ( 0.3675815128205912052, 9.574637318042068301, -7.689697408877177232 ) ) ;
#19465 = CARTESIAN_POINT ( 'NONE',  ( 14.53304282576173634, -29.99999999999999289, 3.713578627762628592 ) ) ;
#19467 = FACE_OUTER_BOUND ( 'NONE', #30017, .T. ) ;
#19466 = VECTOR ( 'NONE', #27747, 1000.000000000000000 ) ;
#19468 = AXIS2_PLACEMENT_3D ( 'NONE', #63185, #7664, #62513 ) ;
#19469 = CARTESIAN_POINT ( 'NONE',  ( 23.11735034598994076, 2.555142731765482456, 11.72821463604131687 ) ) ;
#19470 = DIRECTION ( 'NONE',  ( 0.000000000000000000, 0.01356324068817998940, -0.9999080150203989437 ) ) ;
#19471 = DIRECTION ( 'NONE',  ( 1.000000000000000000, 0.000000000000000000, 0.000000000000000000 ) ) ;
#19472 = ORIENTED_EDGE ( 'NONE', *, *, #16654, .F. ) ;
#19473 = VERTEX_POINT ( 'NONE', #12617 ) ;
#19474 = CARTESIAN_POINT ( 'NONE',  ( -35.00000000000000000, 0.000000000000000000, 0.000000000000000000 ) ) ;
#19475 = ORIENTED_EDGE ( 'NONE', *, *, #15919, .T. ) ;
#19476 = CIRCLE ( 'NONE', #59815, 12.75000000000000178 ) ;
#19477 = VERTEX_POINT ( 'NONE', #38896 ) ;
#19478 = CIRCLE ( 'NONE', #61948, 2.899999999999996358 ) ;
#19479 = CARTESIAN_POINT ( 'NONE',  ( 2.241537034860907163, -1.330359961362336696, 7.517665055736002522 ) ) ;
#19480 = CARTESIAN_POINT ( 'NONE',  ( -22.28284753389937478, 0.9231250029035257265, -3.581493264753382810 ) ) ;
#19481 = CARTESIAN_POINT ( 'NONE',  ( 1.719304012339867516, -12.38166659046446938, 2.961219984258617544 ) ) ;
#19482 = CARTESIAN_POINT ( 'NONE',  ( -22.27715526084302056, 1.423304177213893684, -3.395518526174213569 ) ) ;
#19483 = EDGE_CURVE ( 'NONE', #30093, #5329, #9733, .T. ) ;
#19484 = FACE_OUTER_BOUND ( 'NONE', #25991, .T. ) ;
#19485 = DIRECTION ( 'NONE',  ( 0.9261641133930337277, 0.000000000000000000, -0.3771207168306929813 ) ) ;
#19486 = ORIENTED_EDGE ( 'NONE', *, *, #47038, .F. ) ;
#19487 = AXIS2_PLACEMENT_3D ( 'NONE', #12072, #51363, #6127 ) ;
#19488 = ORIENTED_EDGE ( 'NONE', *, *, #42171, .T. ) ;
#19489 = CIRCLE ( 'NONE', #59831, 12.75000000000000178 ) ;
#19490 = CARTESIAN_POINT ( 'NONE',  ( 0.5572780756280654169, 3.933334466452599987, 11.70006938410048036 ) ) ;
#19491 = DIRECTION ( 'NONE',  ( -1.000000000000000000, 0.000000000000000000, 0.000000000000000000 ) ) ;
#19492 = EDGE_CURVE ( 'NONE', #31440, #3747, #20821, .T. ) ;
#19493 = CYLINDRICAL_SURFACE ( 'NONE', #47249, 1.500000000000000222 ) ;
#19494 = VECTOR ( 'NONE', #30558, 1000.000000000000000 ) ;
#19495 = LINE ( 'NONE', #65353, #3646 ) ;
#19496 = CARTESIAN_POINT ( 'NONE',  ( 4.895484889895522329, -10.53691681195900465, -8.443780401669316760 ) ) ;
#19497 = LINE ( 'NONE', #4867, #24757 ) ;
#19498 = DIRECTION ( 'NONE',  ( 1.000000000000000000, 0.000000000000000000, 0.000000000000000000 ) ) ;
#19499 = CARTESIAN_POINT ( 'NONE',  ( -35.00000000000000000, 12.15823808070322798, 0.8294751490779768144 ) ) ;
#19500 = ORIENTED_EDGE ( 'NONE', *, *, #9979, .F. ) ;
#19501 = CIRCLE ( 'NONE', #44989, 12.75000000000000178 ) ;
#19502 = CARTESIAN_POINT ( 'NONE',  ( 37.00000000000000711, 0.7008968033240532414, 12.16632754454235332 ) ) ;
#19503 = CARTESIAN_POINT ( 'NONE',  ( 5.514970785353741078, -0.004713149585127258956, -0.0003039746380524797073 ) ) ;
#19504 = B_SPLINE_CURVE_WITH_KNOTS ( 'NONE', 3,
 ( #4371, #40921, #15630, #55223, #4718, #24979, #25288, #30929, #5695, #45252, #55565, #15317, #35901, #10006, #5025, #20303, #40585, #60877, #35593 ),
 .UNSPECIFIED., .F., .F.,
 ( 4, 3, 3, 3, 3, 3, 4 ),
 ( 4.336808689942017736E-19, 2.831840207457924380E-05, 4.217266859783480663E-05, 5.602024318339633507E-05, 6.290810167913046238E-05, 9.120440630890213501E-05, 0.0001153103026480247297 ),
 .UNSPECIFIED. ) ;
#19505 = CIRCLE ( 'NONE', #384, 2.999999999999996447 ) ;
#19506 = CARTESIAN_POINT ( 'NONE',  ( 35.00000000000000000, -9.240395740215580744, 7.251710744571670197 ) ) ;
#19507 = AXIS2_PLACEMENT_3D ( 'NONE', #9335, #4051, #59259 ) ;
#19508 = B_SPLINE_CURVE_WITH_KNOTS ( 'NONE', 3,
 ( #59821, #24898, #4636, #25211, #60456, #4949, #55143, #45173, #19901, #65751, #14880, #35171, #55478, #55815, #30840, #39522 ),
 .UNSPECIFIED., .F., .F.,
 ( 4, 3, 3, 3, 3, 4 ),
 ( 1.669781113969282313E-15, 0.0002126834539180026825, 0.0004253519300366890199, 0.0006380165497225110402, 0.0007442707582429369719, 0.0009453531351410801977 ),
 .UNSPECIFIED. ) ;
#19509 = CARTESIAN_POINT ( 'NONE',  ( -13.53218314551040002, -34.21215502346704085, -9.055742533982485298 ) ) ;
#19510 = CARTESIAN_POINT ( 'NONE',  ( -28.25737660011475327, -10.82118954187360949, -5.196380785642891631 ) ) ;
#19511 = EDGE_CURVE ( 'NONE', #38245, #45593, #33134, .T. ) ;
#19512 = AXIS2_PLACEMENT_3D ( 'NONE', #63321, #6842, #47408 ) ;
#19513 = VERTEX_POINT ( 'NONE', #50189 ) ;
#19514 = EDGE_CURVE ( 'NONE', #57971, #6586, #50517, .T. ) ;
#19515 = CARTESIAN_POINT ( 'NONE',  ( -17.54726996257253191, 25.00000000000000000, 3.865003848717349033 ) ) ;
#19516 = DIRECTION ( 'NONE',  ( 0.000000000000000000, 0.01356324068817991828, -0.9999080150203990547 ) ) ;
#19517 = VECTOR ( 'NONE', #50496, 1000.000000000000000 ) ;
#19518 = CARTESIAN_POINT ( 'NONE',  ( -9.974301738911194093, -29.01869747443885927, -8.904338584474109197 ) ) ;
#19519 = VERTEX_POINT ( 'NONE', #65131 ) ;
#19520 = ADVANCED_FACE ( 'NONE', ( #29545 ), #4645, .T. ) ;
#19521 = CARTESIAN_POINT ( 'NONE',  ( 2.241534463349552198, -1.511811348926356884E-18, -7.634462073473343935 ) ) ;
#19522 = CARTESIAN_POINT ( 'NONE',  ( -22.38932658256918984, 4.011828264158244117, -0.2254938976656405414 ) ) ;
#19523 = CARTESIAN_POINT ( 'NONE',  ( -22.28169757117798966, -0.9841724999439904753, -3.561623073126556793 ) ) ;
#19524 = CARTESIAN_POINT ( 'NONE',  ( -36.00000000000000711, 4.983891302653583821, 11.73555825188278590 ) ) ;
#19525 = CARTESIAN_POINT ( 'NONE',  ( -27.08588607604433562, 2.220764381377020147, 0.5840042213196856569 ) ) ;
#19526 = AXIS2_PLACEMENT_3D ( 'NONE', #65619, #65314, #19779 ) ;
#19527 = EDGE_CURVE ( 'NONE', #25443, #37186, #25696, .T. ) ;
#19528 = CARTESIAN_POINT ( 'NONE',  ( 1.372161826078031277, 12.30755118281487981, -2.769012792637354003 ) ) ;
#19529 = ORIENTED_EDGE ( 'NONE', *, *, #56058, .F. ) ;
#19530 = CARTESIAN_POINT ( 'NONE',  ( 9.687175622948609899, 13.48729812737144940, -0.5854820436212360146 ) ) ;
#19531 = CARTESIAN_POINT ( 'NONE',  ( -27.09364415740165910, 1.303410551736471801, 1.918701019213880032 ) ) ;
#19532 = CARTESIAN_POINT ( 'NONE',  ( 0.3474126878361833981, -9.566300984424350062, -7.689340002166830779 ) ) ;
#19533 = CARTESIAN_POINT ( 'NONE',  ( 8.937200413559443390, 4.476360154859203355, 11.13383131558893346 ) ) ;
#19534 = DIRECTION ( 'NONE',  ( 0.000000000000000000, -0.8276889981568956722, 0.5611870653623748373 ) ) ;
#19535 = CARTESIAN_POINT ( 'NONE',  ( -22.51237073810381517, 4.319597983500838012, 0.9543406717316287313 ) ) ;
#19536 = CARTESIAN_POINT ( 'NONE',  ( 1.719304012338398469, 8.755325027793414705, 9.242227816402090568 ) ) ;
#19537 = DIRECTION ( 'NONE',  ( 0.000000000000000000, -0.01356324068817999114, 0.9999080150203989437 ) ) ;
#19538 = ORIENTED_EDGE ( 'NONE', *, *, #60290, .T. ) ;
#19539 = EDGE_CURVE ( 'NONE', #11247, #38647, #29243, .T. ) ;
#19540 = ORIENTED_EDGE ( 'NONE', *, *, #29761, .F. ) ;
#19541 = CARTESIAN_POINT ( 'NONE',  ( -37.00000000000000711, -6.657191900728257394, -9.677500615117970995 ) ) ;
#19542 = ORIENTED_EDGE ( 'NONE', *, *, #13089, .F. ) ;
#19543 = B_SPLINE_CURVE_WITH_KNOTS ( 'NONE', 3,
 ( #1178, #26121, #15474, #10477, #41067, #50738, #56728, #5527, #845, #5864, #41387, #46084, #31429, #41728, #198, #11462 ),
 .UNSPECIFIED., .F., .F.,
 ( 4, 3, 3, 3, 3, 4 ),
 ( 0.000000000000000000, 0.0002999043160757425448, 0.0005998071753051165047, 0.0008997092107374801478, 0.001204458948196538044, 0.001510329163478281618 ),
 .UNSPECIFIED. ) ;
#19544 = CARTESIAN_POINT ( 'NONE',  ( 3.386626873725977038, -10.78029969106401253, -8.130803614474327645 ) ) ;
#19545 = CIRCLE ( 'NONE', #10000, 5.000000000000000000 ) ;
#19546 = EDGE_CURVE ( 'NONE', #49777, #29500, #59697, .T. ) ;
#19547 = DIRECTION ( 'NONE',  ( -1.000000000000000000, -0.000000000000000000, -0.000000000000000000 ) ) ;
#19548 = ORIENTED_EDGE ( 'NONE', *, *, #14540, .F. ) ;
#19549 = FACE_OUTER_BOUND ( 'NONE', #27304, .T. ) ;
#19550 = CARTESIAN_POINT ( 'NONE',  ( 12.51045778728196289, 9.694119109124677891, -7.082454569427619973 ) ) ;
#19551 = CARTESIAN_POINT ( 'NONE',  ( 24.54836029594799385, 1.223829190784184728, 13.44931652200175343 ) ) ;
#19552 = ORIENTED_EDGE ( 'NONE', *, *, #22756, .T. ) ;
#19553 = ORIENTED_EDGE ( 'NONE', *, *, #33129, .T. ) ;
#19554 = CARTESIAN_POINT ( 'NONE',  ( 3.152665057734023613, 0.4801242025591827001, -7.923639299008664594 ) ) ;
#19555 = AXIS2_PLACEMENT_3D ( 'NONE', #14501, #39131, #55083 ) ;
#19556 = VECTOR ( 'NONE', #43834, 1000.000000000000000 ) ;
#19557 = ORIENTED_EDGE ( 'NONE', *, *, #23954, .T. ) ;
#19558 = CARTESIAN_POINT ( 'NONE',  ( 4.622486058658314079, -10.10462791929411530, -6.474617390905248904 ) ) ;
#19559 = ORIENTED_EDGE ( 'NONE', *, *, #22938, .T. ) ;
#19560 = CARTESIAN_POINT ( 'NONE',  ( -35.00000000000000000, 0.000000000000000000, 0.000000000000000000 ) ) ;
#19561 = CARTESIAN_POINT ( 'NONE',  ( 2.305787727787083519, 7.135468203930020792, -2.774453000917077805 ) ) ;
#19562 = VECTOR ( 'NONE', #13371, 1000.000000000000227 ) ;
#19563 = CARTESIAN_POINT ( 'NONE',  ( 2.241352910868908310, -7.633946224498474820, 0.08337961031701579540 ) ) ;
#19564 = LINE ( 'NONE', #14854, #31656 ) ;
#19565 = DIRECTION ( 'NONE',  ( 0.000000000000000000, 0.3807014730195152907, -0.9246979985058750851 ) ) ;
#19566 = VERTEX_POINT ( 'NONE', #59836 ) ;
#19567 = CARTESIAN_POINT ( 'NONE',  ( 2.241317068080781905, 7.633845645378814382, -0.09149433816018485988 ) ) ;
#19568 = CARTESIAN_POINT ( 'NONE',  ( -16.89440222264807190, 7.451370833537603211, 9.406604778602895678 ) ) ;
#19569 = CARTESIAN_POINT ( 'NONE',  ( 37.00000000000000711, 4.705694406421931860E-17, -3.469127814946512892E-15 ) ) ;
#19570 = CARTESIAN_POINT ( 'NONE',  ( 12.16520966156148909, 13.20908209050864457, -2.809526505251493500 ) ) ;
#19571 = AXIS2_PLACEMENT_3D ( 'NONE', #41057, #52376, #62012 ) ;
#19572 = CARTESIAN_POINT ( 'NONE',  ( 1.109979610372149761, 0.4797593171736048157, -12.51859925746178703 ) ) ;
#19573 = LINE ( 'NONE', #49823, #51058 ) ;
#19574 = CARTESIAN_POINT ( 'NONE',  ( -36.00000000000000711, 1.286231064351496922, -12.68495603654570481 ) ) ;
#19575 = DIRECTION ( 'NONE',  ( -1.000000000000000000, 0.000000000000000000, 0.000000000000000000 ) ) ;
#19576 = VECTOR ( 'NONE', #26438, 1000.000000000000000 ) ;
#19577 = EDGE_CURVE ( 'NONE', #2026, #6959, #45845, .T. ) ;
#19578 = ORIENTED_EDGE ( 'NONE', *, *, #51742, .T. ) ;
#19579 = CARTESIAN_POINT ( 'NONE',  ( 5.530133899448235191, 0.006998616117863598260, 0.01437126147332036877 ) ) ;
#19580 = ORIENTED_EDGE ( 'NONE', *, *, #50486, .F. ) ;
#19581 = DIRECTION ( 'NONE',  ( -1.000000000000000000, 0.000000000000000000, 0.000000000000000000 ) ) ;
#19582 = CARTESIAN_POINT ( 'NONE',  ( 2.000000000000001776, -3.795144977083660720, 6.468916029978772464 ) ) ;
#19583 = VECTOR ( 'NONE', #1383, 1000.000000000000000 ) ;
#19584 = CARTESIAN_POINT ( 'NONE',  ( 2.241536586108912932, -4.902521014023369261, 5.852386772940055160 ) ) ;
#19585 = DIRECTION ( 'NONE',  ( -1.000000000000000000, 0.000000000000000000, 0.000000000000000000 ) ) ;
#19586 = LINE ( 'NONE', #14251, #65755 ) ;
#19587 = B_SPLINE_CURVE_WITH_KNOTS ( 'NONE', 3,
 ( #12013, #63213, #12655, #1068, #26655, #46950 ),
 .UNSPECIFIED., .F., .F.,
 ( 4, 2, 4 ),
 ( 5.043579854804842159E-18, 0.0004528561986909453857, 0.0009057123973818857841 ),
 .UNSPECIFIED. ) ;
#19588 = ORIENTED_EDGE ( 'NONE', *, *, #50914, .T. ) ;
#19589 = CARTESIAN_POINT ( 'NONE',  ( -11.39029853170218587, -7.950373430328300906, -10.91384404852269796 ) ) ;
#19590 = CARTESIAN_POINT ( 'NONE',  ( 2.257661810676417691, -3.702552158175651087, 6.682681612748201161 ) ) ;
#19591 = CIRCLE ( 'NONE', #59039, 5.000000000000000888 ) ;
#19592 = CARTESIAN_POINT ( 'NONE',  ( 11.55880380088042969, 0.7131711660007539200, 11.97899817320787363 ) ) ;
#19593 = CARTESIAN_POINT ( 'NONE',  ( 11.92950489380962331, -32.88714273283137857, -11.67197772324075267 ) ) ;
#19594 = AXIS2_PLACEMENT_3D ( 'NONE', #23079, #29054, #63615 ) ;
#19595 = ADVANCED_FACE ( 'NONE', ( #54842 ), #55491, .T. ) ;
#19596 = DIRECTION ( 'NONE',  ( -1.000000000000000000, 0.000000000000000000, -0.000000000000000000 ) ) ;
#19597 = VERTEX_POINT ( 'NONE', #9939 ) ;
#19598 = EDGE_CURVE ( 'NONE', #8078, #7570, #5534, .T. ) ;
#19599 = CARTESIAN_POINT ( 'NONE',  ( 37.00000000000000711, 9.060822531526046220, -7.474872387601039669 ) ) ;
#19600 = EDGE_LOOP ( 'NONE', ( #13090, #26198, #25494, #35224 ) ) ;
#19601 = EDGE_CURVE ( 'NONE', #52455, #15087, #4299, .T. ) ;
#19602 = CARTESIAN_POINT ( 'NONE',  ( -37.00000000000000711, 10.25474254703953036, 6.584150480049589582 ) ) ;
#19603 = CARTESIAN_POINT ( 'NONE',  ( 37.00000000000000711, -1.456211999474423369, -11.65554240571057143 ) ) ;
#19604 = AXIS2_PLACEMENT_3D ( 'NONE', #12795, #16808, #32735 ) ;
#19605 = DIRECTION ( 'NONE',  ( -1.000000000000000000, 0.000000000000000000, 0.000000000000000000 ) ) ;
#19606 = CARTESIAN_POINT ( 'NONE',  ( 0.000000000000000000, -5.814643797626954935, 3.550179297009551149 ) ) ;
#19607 = VERTEX_POINT ( 'NONE', #44853 ) ;
#19609 = ORIENTED_EDGE ( 'NONE', *, *, #52981, .F. ) ;
#19608 = EDGE_CURVE ( 'NONE', #429, #65629, #20376, .T. ) ;
#19610 = CYLINDRICAL_SURFACE ( 'NONE', #36063, 6.936499999999988120 ) ;
#19611 = ORIENTED_EDGE ( 'NONE', *, *, #47390, .T. ) ;
#19612 = CARTESIAN_POINT ( 'NONE',  ( 2.259830038564996979, -6.546987858513350744, -3.938923657569476600 ) ) ;
#19613 = DIRECTION ( 'NONE',  ( 0.000000000000000000, 0.000000000000000000, -1.000000000000000000 ) ) ;
#19614 = DIRECTION ( 'NONE',  ( 0.000000000000000000, 0.2006870767258889243, -0.9796553971857742127 ) ) ;
#19615 = DIRECTION ( 'NONE',  ( 1.000000000000000000, 0.000000000000000000, 0.000000000000000000 ) ) ;
#19616 = DIRECTION ( 'NONE',  ( 0.000000000000000000, 0.000000000000000000, -1.000000000000000000 ) ) ;
#19617 = EDGE_CURVE ( 'NONE', #36553, #22075, #32037, .T. ) ;
#19618 = CARTESIAN_POINT ( 'NONE',  ( -35.00000000000000000, -11.81949347079749124, 2.968224442958359965 ) ) ;
#19619 = CARTESIAN_POINT ( 'NONE',  ( 0.8375941296801611147, -12.43103843094034389, -0.3844307390187421403 ) ) ;
#19620 = ORIENTED_EDGE ( 'NONE', *, *, #29275, .T. ) ;
#19622 = ORIENTED_EDGE ( 'NONE', *, *, #40871, .T. ) ;
#19621 = CARTESIAN_POINT ( 'NONE',  ( 2.241352910868909643, -7.145045428366594287, 2.689314586382326677 ) ) ;
#19623 = ORIENTED_EDGE ( 'NONE', *, *, #5347, .T. ) ;
#19624 = CARTESIAN_POINT ( 'NONE',  ( 0.2851083653049504285, -0.4107471485392698018, 13.49374991542258151 ) ) ;
#19625 = ADVANCED_FACE ( 'NONE', ( #11564 ), #6272, .T. ) ;
#19626 = AXIS2_PLACEMENT_3D ( 'NONE', #58726, #49409, #13147 ) ;
#19627 = DIRECTION ( 'NONE',  ( 0.000000000000000000, -1.000000000000000000, 0.000000000000000000 ) ) ;
#19628 = ORIENTED_EDGE ( 'NONE', *, *, #8242, .T. ) ;
#19629 = EDGE_CURVE ( 'NONE', #18227, #16636, #55396, .T. ) ;
#19630 = DIRECTION ( 'NONE',  ( -1.000000000000000000, -1.836970198721029688E-16, -0.000000000000000000 ) ) ;
#19631 = ORIENTED_EDGE ( 'NONE', *, *, #23754, .T. ) ;
#19632 = CARTESIAN_POINT ( 'NONE',  ( 2.241352910868908310, 6.652881166698564108, -3.744764251556923274 ) ) ;
#19633 =( BOUNDED_SURFACE ( )  B_SPLINE_SURFACE ( 3, 1, ( 
 ( #14129, #54723 ),
 ( #24434, #9144 ),
 ( #29426, #33752 ),
 ( #44707, #49722 ) ),
 .UNSPECIFIED., .F., .F., .F. ) 
 B_SPLINE_SURFACE_WITH_KNOTS ( ( 4, 4 ),
 ( 2, 2 ),
 ( 0.000000000000000000, 1.000000000000000000 ),
 ( 0.000000000000000000, 1.000000000000000000 ),
 .UNSPECIFIED. ) 
 GEOMETRIC_REPRESENTATION_ITEM ( )  RATIONAL_B_SPLINE_SURFACE ( (
 ( 1.000000000000000000, 1.000000000000000000),
 ( 0.6933888150995267674, 0.9895912004443193632),
 ( 0.6933888150995267674, 0.9895912004443193632),
 ( 1.000000000000000000, 1.000000000000000000) ) ) 
 REPRESENTATION_ITEM ( '' )  SURFACE ( )  );
#19634 = FACE_OUTER_BOUND ( 'NONE', #36856, .T. ) ;
#19635 = CARTESIAN_POINT ( 'NONE',  ( 2.781367136452162825, 7.232043329634170625, -2.960151187464861611 ) ) ;
#19636 = ORIENTED_EDGE ( 'NONE', *, *, #15780, .F. ) ;
#19638 = EDGE_CURVE ( 'NONE', #39558, #52452, #11865, .T. ) ;
#19637 = ORIENTED_EDGE ( 'NONE', *, *, #7908, .T. ) ;
#19639 = CARTESIAN_POINT ( 'NONE',  ( -37.00000000000000711, 0.3137578094509230753, 12.74613886779085270 ) ) ;
#19640 = VERTEX_POINT ( 'NONE', #36520 ) ;
#19641 = ORIENTED_EDGE ( 'NONE', *, *, #24463, .F. ) ;
#19642 = B_SPLINE_CURVE_WITH_KNOTS ( 'NONE', 3,
 ( #61690, #61055, #15485, #35751, #56384, #15800, #30766, #51086, #16152, #36078, #36431, #31443, #51430, #11168, #11800, #36758, #43048, #32083, #2522 ),
 .UNSPECIFIED., .F., .F.,
 ( 4, 3, 3, 3, 3, 3, 4 ),
 ( 0.000000000000000000, 2.831840207499679716E-05, 4.217266859840589657E-05, 5.602024318396098078E-05, 6.290810167969312265E-05, 9.120440630945326208E-05, 0.0001153103026479758322 ),
 .UNSPECIFIED. ) ;
#19643 = VERTEX_POINT ( 'NONE', #26531 ) ;
#19644 = VERTEX_POINT ( 'NONE', #1286 ) ;
#19645 = CYLINDRICAL_SURFACE ( 'NONE', #44668, 12.74999999999999822 ) ;
#19646 = LINE ( 'NONE', #60186, #13493 ) ;
#19647 = AXIS2_PLACEMENT_3D ( 'NONE', #25956, #26590, #5686 ) ;
#19648 = DIRECTION ( 'NONE',  ( 1.000000000000000000, -0.000000000000000000, 0.000000000000000000 ) ) ;
#19649 = DIRECTION ( 'NONE',  ( 1.000000000000000000, -0.000000000000000000, -0.000000000000000000 ) ) ;
#19650 = ORIENTED_EDGE ( 'NONE', *, *, #43987, .T. ) ;
#19651 = CARTESIAN_POINT ( 'NONE',  ( -35.00000000000000000, -11.72195762423409349, -0.7536123767499773862 ) ) ;
#19652 = ORIENTED_EDGE ( 'NONE', *, *, #8284, .T. ) ;
#19653 = DIRECTION ( 'NONE',  ( 0.000000000000000000, -0.9246979985058680906, -0.3807014730195321661 ) ) ;
#19654 = DIRECTION ( 'NONE',  ( -1.000000000000000000, 0.000000000000000000, 0.000000000000000000 ) ) ;
#19655 = AXIS2_PLACEMENT_3D ( 'NONE', #44956, #50295, #62139 ) ;
#19656 = ORIENTED_EDGE ( 'NONE', *, *, #44428, .T. ) ;
#19657 = CARTESIAN_POINT ( 'NONE',  ( 0.6511581176972706109, 9.688955459275215176, -7.698038847496603054 ) ) ;
#19658 = CARTESIAN_POINT ( 'NONE',  ( 5.515188684475870851, 0.003154373509839897977, 0.004322737127823491482 ) ) ;
#19659 = CARTESIAN_POINT ( 'NONE',  ( 2.241317068080794783, -6.656851426547295780, -3.737686401540284198 ) ) ;
#19660 = VERTEX_POINT ( 'NONE', #628 ) ;
#19661 = ADVANCED_FACE ( 'NONE', ( #5626 ), #8708, .F. ) ;
#19662 = EDGE_CURVE ( 'NONE', #49910, #63048, #63671, .T. ) ;
#19663 = ORIENTED_EDGE ( 'NONE', *, *, #63538, .F. ) ;
#19664 = CARTESIAN_POINT ( 'NONE',  ( 1.459561108992809331, 6.861308540877414153, 10.62073135189154272 ) ) ;
#19665 = AXIS2_PLACEMENT_3D ( 'NONE', #50588, #28722, #4377 ) ;
#19666 = ORIENTED_EDGE ( 'NONE', *, *, #9196, .T. ) ;
#19667 = DIRECTION ( 'NONE',  ( 0.5417962735734935809, -0.000000000000000000, 0.8405098440481683086 ) ) ;
#19668 = CARTESIAN_POINT ( 'NONE',  ( 1.459561108992595502, 10.08002506399508214, 7.633517148169521427 ) ) ;
#19669 = CARTESIAN_POINT ( 'NONE',  ( 4.028938272669588372, -26.74124408001654984, 15.94258242224534960 ) ) ;
#19670 = DIRECTION ( 'NONE',  ( 0.000000000000000000, 0.000000000000000000, -1.000000000000000000 ) ) ;
#19671 = CARTESIAN_POINT ( 'NONE',  ( 0.6473888112830242791, -9.263269341114842348, 8.203438694127630271 ) ) ;
#19672 = ORIENTED_EDGE ( 'NONE', *, *, #31727, .T. ) ;
#19673 = EDGE_CURVE ( 'NONE', #11283, #5130, #49066, .T. ) ;
#19674 = DIRECTION ( 'NONE',  ( 0.000000000000000000, -0.2960891610144577024, -0.9551603052523457427 ) ) ;
#19675 = CARTESIAN_POINT ( 'NONE',  ( 0.000000000000000000, 0.000000000000000000, 0.000000000000000000 ) ) ;
#19676 = CARTESIAN_POINT ( 'NONE',  ( 35.00000000000000000, 10.01317267707886671, -6.946017217729977489 ) ) ;
#19677 = FACE_OUTER_BOUND ( 'NONE', #17672, .T. ) ;
#19678 = AXIS2_PLACEMENT_3D ( 'NONE', #22379, #52975, #62950 ) ;
#19679 = B_SPLINE_CURVE_WITH_KNOTS ( 'NONE', 3,
 ( #43783, #34110, #29155, #19823, #65030, #28477, #29773, #8211, #28813, #34454, #4202, #48784, #50089, #8863, #4548, #33485 ),
 .UNSPECIFIED., .F., .F.,
 ( 4, 3, 3, 3, 3, 4 ),
 ( 2.158593104248768223E-15, 0.0002126834539180167500, 0.0004253519300367212207, 0.0006380165497225577693, 0.0007442707582429906399, 0.0009453531351407485402 ),
 .UNSPECIFIED. ) ;
#19680 = ADVANCED_FACE ( 'NONE', ( #40857 ), #31837, .T. ) ;
#19681 = CARTESIAN_POINT ( 'NONE',  ( -12.53824232977091491, -28.27004406456470775, -13.15159876983786980 ) ) ;
#19682 = DIRECTION ( 'NONE',  ( 0.000000000000000000, -0.01356324068817991828, 0.9999080150203990547 ) ) ;
#19683 = ADVANCED_FACE ( 'NONE', ( #52150 ), #10574, .T. ) ;
#19684 = CARTESIAN_POINT ( 'NONE',  ( -37.00000000000000711, -11.47758908105692655, -2.497432891016966749 ) ) ;
#19685 = CARTESIAN_POINT ( 'NONE',  ( 2.406456491626453698, -1.188938370543003442, 10.36527681095974707 ) ) ;
#19686 = DIRECTION ( 'NONE',  ( 0.000000000000000000, 0.5155538571770231782, -0.8568571761675882748 ) ) ;
#19687 = AXIS2_PLACEMENT_3D ( 'NONE', #56959, #62559, #32312 ) ;
#19688 = ORIENTED_EDGE ( 'NONE', *, *, #17708, .T. ) ;
#19689 = CARTESIAN_POINT ( 'NONE',  ( -29.92777678363736626, -3.750539801530011985, 11.39883551934754635 ) ) ;
#19690 = ORIENTED_EDGE ( 'NONE', *, *, #63979, .F. ) ;
#19691 = CARTESIAN_POINT ( 'NONE',  ( -14.17299601508879192, 8.097942500480229455, -8.858180248946757374 ) ) ;
#19692 = DIRECTION ( 'NONE',  ( -0.9915282196991074271, 0.000000000000000000, 0.1298914529148032515 ) ) ;
#19693 = CYLINDRICAL_SURFACE ( 'NONE', #57634, 12.18649999999999878 ) ;
#19694 = EDGE_CURVE ( 'NONE', #55015, #24413, #51197, .T. ) ;
#19695 = DIRECTION ( 'NONE',  ( -1.000000000000000000, 0.000000000000000000, 0.000000000000000000 ) ) ;
#19696 = ORIENTED_EDGE ( 'NONE', *, *, #46160, .F. ) ;
#19697 = EDGE_CURVE ( 'NONE', #38454, #37450, #51174, .T. ) ;
#19698 = EDGE_LOOP ( 'NONE', ( #25274, #21418, #24847, #45505 ) ) ;
#19699 = VERTEX_POINT ( 'NONE', #51821 ) ;
#19700 = CARTESIAN_POINT ( 'NONE',  ( 2.573738926104377711, 2.868819712476807560, -7.194322927777922594 ) ) ;
#19701 = EDGE_CURVE ( 'NONE', #40113, #21973, #1260, .T. ) ;
#19702 = CYLINDRICAL_SURFACE ( 'NONE', #17226, 5.000000000000000888 ) ;
#19703 = EDGE_LOOP ( 'NONE', ( #63165, #4713, #1562, #33003 ) ) ;
#19704 = EDGE_CURVE ( 'NONE', #11383, #41793, #3412, .T. ) ;
#19705 = DIRECTION ( 'NONE',  ( 1.000000000000000000, -0.000000000000000000, 0.000000000000000000 ) ) ;
#19706 = DIRECTION ( 'NONE',  ( 0.000000000000000000, -0.6876994588534139918, -0.7259954919231395021 ) ) ;
#19707 = CARTESIAN_POINT ( 'NONE',  ( 0.3040950598368144520, 9.552450779732218678, -7.687624643091335308 ) ) ;
#19708 = CARTESIAN_POINT ( 'NONE',  ( 2.781367136452256084, -2.381060477055441549, 7.442815111163296748 ) ) ;
#19709 = ORIENTED_EDGE ( 'NONE', *, *, #1855, .F. ) ;
#19710 = VECTOR ( 'NONE', #40926, 1000.000000000000000 ) ;
#19711 = DIRECTION ( 'NONE',  ( -0.9915282196991074271, 0.000000000000000000, 0.1298914529148032515 ) ) ;
#19712 = CARTESIAN_POINT ( 'NONE',  ( -1.825668173474439993, -28.16298946971344108, -13.82820292526064776 ) ) ;
#19713 = DIRECTION ( 'NONE',  ( 0.000000000000000000, -0.5472293298355331848, 0.8369827122275305120 ) ) ;
#19715 = ORIENTED_EDGE ( 'NONE', *, *, #61217, .T. ) ;
#19714 = CARTESIAN_POINT ( 'NONE',  ( 36.00000000000000711, -10.39746860227895731, -7.379373053628834889 ) ) ;
#19716 = EDGE_CURVE ( 'NONE', #16620, #30257, #63894, .T. ) ;
#19717 = DIRECTION ( 'NONE',  ( 0.000000000000000000, 0.000000000000000000, 1.000000000000000000 ) ) ;
#19718 = ORIENTED_EDGE ( 'NONE', *, *, #58838, .F. ) ;
#19719 = CARTESIAN_POINT ( 'NONE',  ( 0.4626703367446075021, -9.611037151103436926, 7.694993290995456370 ) ) ;
#19720 = VERTEX_POINT ( 'NONE', #32164 ) ;
#19721 = LINE ( 'NONE', #64908, #31632 ) ;
#19722 = CARTESIAN_POINT ( 'NONE',  ( -22.70624764888619751, 4.097886656202288869, 3.282666355490642118 ) ) ;
#19723 = CIRCLE ( 'NONE', #29246, 7.499999999999988454 ) ;
#19724 = CARTESIAN_POINT ( 'NONE',  ( 37.00000000000000711, -11.61976888909157246, -3.827969819614423841 ) ) ;
#19725 = DIRECTION ( 'NONE',  ( 0.000000000000000000, 0.01356324068817992175, -0.9999080150203990547 ) ) ;
#19726 = DIRECTION ( 'NONE',  ( 1.000000000000000000, 0.000000000000000000, 0.000000000000000000 ) ) ;
#19727 = CARTESIAN_POINT ( 'NONE',  ( 37.00000000000000711, -2.497432891016756251, 11.47758908105696740 ) ) ;
#19728 = LINE ( 'NONE', #49653, #59839 ) ;
#19730 = ORIENTED_EDGE ( 'NONE', *, *, #49533, .T. ) ;
#19729 = CYLINDRICAL_SURFACE ( 'NONE', #6625, 6.936499999999988120 ) ;
#19731 = ORIENTED_EDGE ( 'NONE', *, *, #36834, .F. ) ;
#19732 = DIRECTION ( 'NONE',  ( 1.000000000000000000, 0.000000000000000000, 0.000000000000000000 ) ) ;
#19733 = ORIENTED_EDGE ( 'NONE', *, *, #41457, .F. ) ;
#19734 = ORIENTED_EDGE ( 'NONE', *, *, #1736, .T. ) ;
#19735 = CARTESIAN_POINT ( 'NONE',  ( 0.9232167919969115344, -12.45862789703290652, 0.4134278310082598606 ) ) ;
#19736 = DIRECTION ( 'NONE',  ( 1.000000000000000000, 0.000000000000000000, 0.000000000000000000 ) ) ;
#19737 = CARTESIAN_POINT ( 'NONE',  ( -35.00000000000000000, 3.033604067594749765, -12.38385022362078658 ) ) ;
#19738 = CARTESIAN_POINT ( 'NONE',  ( -28.67667724226168602, -0.4371157725390015791, 1.840944188131422576 ) ) ;
#19739 = DIRECTION ( 'NONE',  ( -1.000000000000000000, 0.000000000000000000, 0.000000000000000000 ) ) ;
#19740 = VECTOR ( 'NONE', #56114, 1000.000000000000000 ) ;
#19741 = ADVANCED_FACE ( 'NONE', ( #943 ), #21211, .T. ) ;
#19742 = CARTESIAN_POINT ( 'NONE',  ( -37.00000000000000711, 7.110831038798280268, 9.896810808925419423 ) ) ;
#19743 = ADVANCED_FACE ( 'NONE', ( #1927 ), #23523, .F. ) ;
#19744 = EDGE_LOOP ( 'NONE', ( #63664, #32718, #23057, #24367 ) ) ;
#19745 = LINE ( 'NONE', #54971, #15878 ) ;
#19746 = CARTESIAN_POINT ( 'NONE',  ( 1.719304012338201737, 9.242227816402087015, 8.755325027793320558 ) ) ;
#19747 = CARTESIAN_POINT ( 'NONE',  ( 0.6511581176956539041, 12.12498040206523875, 2.473966499147935760 ) ) ;
#19748 = EDGE_LOOP ( 'NONE', ( #23957, #60619, #48598, #56741 ) ) ;
#19749 = EDGE_CURVE ( 'NONE', #21040, #49572, #54102, .T. ) ;
#19750 = VECTOR ( 'NONE', #18982, 1000.000000000000000 ) ;
#19751 = AXIS2_PLACEMENT_3D ( 'NONE', #38797, #54434, #8522 ) ;
#19752 = FACE_OUTER_BOUND ( 'NONE', #50896, .T. ) ;
#19753 = CARTESIAN_POINT ( 'NONE',  ( -35.00000000000000000, 11.65150730582932503, 1.488153103997165605 ) ) ;
#19754 = CARTESIAN_POINT ( 'NONE',  ( -49.96127604611442763, -0.007915161567797545511, -1.618137530678320335 ) ) ;
#19756 = ORIENTED_EDGE ( 'NONE', *, *, #30522, .T. ) ;
#19755 = EDGE_CURVE ( 'NONE', #48169, #23887, #19344, .T. ) ;
#19757 = CARTESIAN_POINT ( 'NONE',  ( 2.298277635560276533, 6.709004959608422247, -3.682855706290065090 ) ) ;
#19758 = CARTESIAN_POINT ( 'NONE',  ( -47.00000000000000711, 0.000000000000000000, 0.000000000000000000 ) ) ;
#19759 = DIRECTION ( 'NONE',  ( 1.000000000000000000, 0.000000000000000000, -0.000000000000000000 ) ) ;
#19760 = ADVANCED_FACE ( 'NONE', ( #28829 ), #27508, .T. ) ;
#19761 = VECTOR ( 'NONE', #51301, 1000.000000000000000 ) ;
#19762 = CARTESIAN_POINT ( 'NONE',  ( 2.000000000000001776, -6.997684042076919297, 2.698595569414185658 ) ) ;
#19763 = DIRECTION ( 'NONE',  ( -1.000000000000000000, 0.000000000000000000, 0.000000000000000000 ) ) ;
#19764 = ORIENTED_EDGE ( 'NONE', *, *, #25770, .F. ) ;
#19765 = CARTESIAN_POINT ( 'NONE',  ( -35.00000000000000000, -12.18359334611896472, -0.2661492558804631203 ) ) ;
#19766 = CARTESIAN_POINT ( 'NONE',  ( 0.2869720083484353368, -12.10169797402142500, 1.922200714744121575 ) ) ;
#19767 = FACE_OUTER_BOUND ( 'NONE', #2009, .T. ) ;
#19768 = ORIENTED_EDGE ( 'NONE', *, *, #31297, .T. ) ;
#19769 = CARTESIAN_POINT ( 'NONE',  ( 10.63145532060650744, 0.6018409079247246662, 13.48718478653089647 ) ) ;
#19770 = CARTESIAN_POINT ( 'NONE',  ( 2.000000000000001776, 6.750946897830741200, -1.593658756657007514 ) ) ;
#19771 = VERTEX_POINT ( 'NONE', #47806 ) ;
#19772 = ORIENTED_EDGE ( 'NONE', *, *, #47287, .T. ) ;
#19773 = ORIENTED_EDGE ( 'NONE', *, *, #39993, .F. ) ;
#19774 = EDGE_CURVE ( 'NONE', #24593, #29718, #10563, .T. ) ;
#19775 = EDGE_LOOP ( 'NONE', ( #27765, #17945, #39780, #22475 ) ) ;
#19776 = EDGE_CURVE ( 'NONE', #19299, #20746, #32489, .T. ) ;
#19777 = FACE_OUTER_BOUND ( 'NONE', #4276, .T. ) ;
#19778 = CARTESIAN_POINT ( 'NONE',  ( 0.2651627682582892720, 6.046625184671136743, -10.64925413290587919 ) ) ;
#19779 = DIRECTION ( 'NONE',  ( 0.000000000000000000, -0.5472293298355331848, 0.8369827122275305120 ) ) ;
#19780 = CARTESIAN_POINT ( 'NONE',  ( -35.00000000000000000, 3.473736367725253515, 12.26766708251992810 ) ) ;
#19781 = B_SPLINE_CURVE_WITH_KNOTS ( 'NONE', 3,
 ( #9355, #54925, #43063, #2538, #33088, #27776, #4068, #19369, #58725, #63341, #29642, #48080, #13144, #17807 ),
 .UNSPECIFIED., .F., .F.,
 ( 4, 2, 2, 2, 2, 2, 4 ),
 ( 1.301042606982605321E-18, 0.001757691579725207103, 0.002636537369587810004, 0.003515383159450412905, 0.004394228949313015373, 0.005273074739175619141, 0.007030766318900821474 ),
 .UNSPECIFIED. ) ;
#19782 = CARTESIAN_POINT ( 'NONE',  ( -16.37486794060187734, -28.33944867960597236, 9.978426449060183501 ) ) ;
#19783 = CARTESIAN_POINT ( 'NONE',  ( 23.20048651429565112, 3.175973680696976498, -13.12354496719417085 ) ) ;
#19785 = ORIENTED_EDGE ( 'NONE', *, *, #43211, .T. ) ;
#19784 = CARTESIAN_POINT ( 'NONE',  ( 0.6511581176955547612, 7.698038847496699866, 9.688955459274410487 ) ) ;
#19786 = EDGE_CURVE ( 'NONE', #7570, #2448, #17557, .T. ) ;
#19787 = CARTESIAN_POINT ( 'NONE',  ( 145.1370849898475797, 3.309064568108273190E-14, 0.000000000000000000 ) ) ;
#19788 = ORIENTED_EDGE ( 'NONE', *, *, #1525, .T. ) ;
#19789 = LINE ( 'NONE', #60330, #31659 ) ;
#19790 = EDGE_LOOP ( 'NONE', ( #34276, #63291, #41337, #55312 ) ) ;
#19791 = ORIENTED_EDGE ( 'NONE', *, *, #34736, .F. ) ;
#19792 = DIRECTION ( 'NONE',  ( 0.000000000000000000, 1.000000000000000000, 0.000000000000000000 ) ) ;
#19793 = CARTESIAN_POINT ( 'NONE',  ( 17.33919137821584044, -29.56463768738094089, 9.168593624349419713 ) ) ;
#19794 = CARTESIAN_POINT ( 'NONE',  ( -22.27218376572352554, -0.3046453028544371944, -3.670373711461411670 ) ) ;
#19795 = CARTESIAN_POINT ( 'NONE',  ( 1.000000000000000888, -3.224464355699868889, 6.771471746881965181 ) ) ;
#19796 = CIRCLE ( 'NONE', #20869, 5.000000000000000888 ) ;
#19797 = CARTESIAN_POINT ( 'NONE',  ( 37.00000000000000711, 11.81949347079746637, -2.968224442958448783 ) ) ;
#19798 = CYLINDRICAL_SURFACE ( 'NONE', #21420, 4.999999999999999112 ) ;
#19799 = VERTEX_POINT ( 'NONE', #17224 ) ;
#19800 = ORIENTED_EDGE ( 'NONE', *, *, #11614, .F. ) ;
#19801 = LINE ( 'NONE', #50057, #23144 ) ;
#19802 = VERTEX_POINT ( 'NONE', #12223 ) ;
#19803 = ORIENTED_EDGE ( 'NONE', *, *, #50264, .F. ) ;
#19804 = CARTESIAN_POINT ( 'NONE',  ( 3.347841273039249721, -10.61118957148187825, 8.345816669330455184 ) ) ;
#19805 = CARTESIAN_POINT ( 'NONE',  ( -22.29382655386184453, 0.8947172055470843377, -3.622626291186091141 ) ) ;
#19806 = CARTESIAN_POINT ( 'NONE',  ( 17.93387043762216493, -6.318682511722990114, 10.20511618420410116 ) ) ;
#19807 = CARTESIAN_POINT ( 'NONE',  ( 2.290907136833256086, 7.649199419879180617, 0.1622757685885358181 ) ) ;
#19808 = CARTESIAN_POINT ( 'NONE',  ( -11.24065750081571835, -6.047149079109201075, -10.36726786815886214 ) ) ;
#19809 = DIRECTION ( 'NONE',  ( -1.000000000000000000, 0.000000000000000000, 0.000000000000000000 ) ) ;
#19810 = EDGE_CURVE ( 'NONE', #646, #14018, #27068, .T. ) ;
#19811 = VERTEX_POINT ( 'NONE', #2925 ) ;
#19812 =( BOUNDED_CURVE ( )  B_SPLINE_CURVE ( 3, ( #25171, #29822, #65395, #55101 ),
 .UNSPECIFIED., .F., .F. ) 
 B_SPLINE_CURVE_WITH_KNOTS ( ( 4, 4 ),
 ( 1.140504141920692494, 1.180309962260583934 ),
 .UNSPECIFIED. ) 
 CURVE ( )  GEOMETRIC_REPRESENTATION_ITEM ( )  RATIONAL_B_SPLINE_CURVE ( ( 1.000000000000000000, 0.9998679624143003153, 0.9998679624143003153, 1.000000000000000000 ) ) 
 REPRESENTATION_ITEM ( '' )  );
#19813 = VERTEX_POINT ( 'NONE', #58447 ) ;
#19814 = DIRECTION ( 'NONE',  ( -1.000000000000000000, -0.000000000000000000, 0.000000000000000000 ) ) ;
#19815 = DIRECTION ( 'NONE',  ( 1.000000000000000000, 0.000000000000000000, 0.000000000000000000 ) ) ;
#19816 = DIRECTION ( 'NONE',  ( 0.000000000000000000, 0.3807014730195151797, -0.9246979985058750851 ) ) ;
#19817 = CARTESIAN_POINT ( 'NONE',  ( 3.347841273039249721, -10.61118957148187825, 5.603807266321171987 ) ) ;
#19818 = CARTESIAN_POINT ( 'NONE',  ( 6.681371532684399206, -8.678434492379226484, -10.34286318303527352 ) ) ;
#19819 = CYLINDRICAL_SURFACE ( 'NONE', #60885, 4.999999999999999112 ) ;
#19820 = CARTESIAN_POINT ( 'NONE',  ( 5.516018279890452902, 0.002527316374434305981, 0.006286471671801938804 ) ) ;
#19821 = ADVANCED_FACE ( 'NONE', ( #53467 ), #7912, .T. ) ;
#19822 = ORIENTED_EDGE ( 'NONE', *, *, #54136, .F. ) ;
#19823 = CARTESIAN_POINT ( 'NONE',  ( 2.969415267403833880, -6.276215141898326522, -4.760005747566549594 ) ) ;
#19824 = DIRECTION ( 'NONE',  ( -0.9606638835031802159, -0.1943236796486244866, -0.1984016392583667632 ) ) ;
#19825 = CARTESIAN_POINT ( 'NONE',  ( 1.452237505248555660, 12.64182585313126062, -0.5922625322517459656 ) ) ;
#19826 = AXIS2_PLACEMENT_3D ( 'NONE', #35641, #31630, #40967 ) ;
#19827 = EDGE_CURVE ( 'NONE', #51664, #40551, #21424, .T. ) ;
#19828 = CIRCLE ( 'NONE', #52820, 12.18650000000000233 ) ;
#19829 = CARTESIAN_POINT ( 'NONE',  ( -12.31625042011854454, -33.75886355119538962, -10.24605909438320950 ) ) ;
#19830 = CARTESIAN_POINT ( 'NONE',  ( 0.5547464869798252041, -4.506704303875380013, -11.49049644196207964 ) ) ;
#19831 = ORIENTED_EDGE ( 'NONE', *, *, #64422, .F. ) ;
#19832 = CARTESIAN_POINT ( 'NONE',  ( -35.04834644901396956, -0.002604658385690415082, 0.01358669851862255064 ) ) ;
#19833 = CARTESIAN_POINT ( 'NONE',  ( -37.00000000000000711, 9.040300684349693583, 7.499679039484089316 ) ) ;
#19834 = CARTESIAN_POINT ( 'NONE',  ( 14.05446433506782533, -34.40329588773735736, -8.438602785652603799 ) ) ;
#19835 = EDGE_LOOP ( 'NONE', ( #20905, #58484, #59302, #30450 ) ) ;
#19836 = DIRECTION ( 'NONE',  ( 0.000000000000000000, 0.01356324068817998940, -0.9999080150203990547 ) ) ;
#19837 = FACE_OUTER_BOUND ( 'NONE', #17168, .T. ) ;
#19838 = CYLINDRICAL_SURFACE ( 'NONE', #49300, 6.936499999999988120 ) ;
#19839 = CARTESIAN_POINT ( 'NONE',  ( -35.00000000000000000, 0.000000000000000000, 0.000000000000000000 ) ) ;
#19840 = CARTESIAN_POINT ( 'NONE',  ( -16.98800322446194855, 2.922502605998049674, 11.63868456991315625 ) ) ;
#19841 = ADVANCED_FACE ( 'NONE', ( #43798 ), #64078, .T. ) ;
#19842 = DIRECTION ( 'NONE',  ( 1.000000000000000000, -0.000000000000000000, 0.000000000000000000 ) ) ;
#19843 = ORIENTED_EDGE ( 'NONE', *, *, #4786, .T. ) ;
#19844 = LINE ( 'NONE', #15814, #64113 ) ;
#19845 = CARTESIAN_POINT ( 'NONE',  ( -25.00000000000000355, -9.999999999999998224, 1.530808498934191521E-15 ) ) ;
#19846 = CARTESIAN_POINT ( 'NONE',  ( -17.05724255175752901, 7.953322362475236496, -10.91012176226558417 ) ) ;
#19847 = CYLINDRICAL_SURFACE ( 'NONE', #22383, 4.999999999999999112 ) ;
#19848 = CARTESIAN_POINT ( 'NONE',  ( -37.00000000000000711, -11.35427606708809556, 4.426194442447198618 ) ) ;
#19849 = CARTESIAN_POINT ( 'NONE',  ( 35.00000000000000000, -6.102719229070595830, 10.54834585426226390 ) ) ;
#19850 = DIRECTION ( 'NONE',  ( -1.000000000000000000, -0.000000000000000000, 0.000000000000000000 ) ) ;
#19851 = VERTEX_POINT ( 'NONE', #55075 ) ;
#19852 = ORIENTED_EDGE ( 'NONE', *, *, #30815, .T. ) ;
#19853 = CARTESIAN_POINT ( 'NONE',  ( 2.262775599886257094, -5.019217486251079663, 5.761998514039110120 ) ) ;
#19854 = EDGE_LOOP ( 'NONE', ( #54121, #32338, #7879, #11289 ) ) ;
#19855 = SURFACE_SIDE_STYLE ('',( #49484 ) ) ;
#19856 = EDGE_CURVE ( 'NONE', #11898, #10126, #11913, .T. ) ;
#19857 = CYLINDRICAL_SURFACE ( 'NONE', #11985, 12.18650000000000055 ) ;
#19858 = DIRECTION ( 'NONE',  ( 1.000000000000000000, 0.000000000000000000, 0.000000000000000000 ) ) ;
#19859 = ORIENTED_EDGE ( 'NONE', *, *, #56044, .T. ) ;
#19860 = DIRECTION ( 'NONE',  ( 0.000000000000000000, 0.000000000000000000, -1.000000000000000000 ) ) ;
#19861 = FACE_OUTER_BOUND ( 'NONE', #8959, .T. ) ;
#19862 = AXIS2_PLACEMENT_3D ( 'NONE', #39674, #45637, #44321 ) ;
#19863 = CARTESIAN_POINT ( 'NONE',  ( 35.00000000000000000, -5.391785509271032062, -10.43555801961473861 ) ) ;
#19864 = ORIENTED_EDGE ( 'NONE', *, *, #58022, .F. ) ;
#19865 = ORIENTED_EDGE ( 'NONE', *, *, #55879, .F. ) ;
#19866 = DIRECTION ( 'NONE',  ( 0.000000000000000000, -0.000000000000000000, -1.000000000000000000 ) ) ;
#19867 = ORIENTED_EDGE ( 'NONE', *, *, #53993, .T. ) ;
#19868 = B_SPLINE_CURVE_WITH_KNOTS ( 'NONE', 3,
 ( #15124, #65342, #29752, #46070, #10148, #24445, #15460, #41054, #44724, #9808, #516, #30426, #49737, #25778, #25437, #60043, #19807, #30099, #25121 ),
 .UNSPECIFIED., .F., .F.,
 ( 4, 3, 3, 3, 3, 3, 4 ),
 ( 0.000000000000000000, 2.831840207499482866E-05, 4.217266859840272528E-05, 5.602024318395762653E-05, 6.290810167968828440E-05, 9.120440630944945382E-05, 0.0001153103026479763201 ),
 .UNSPECIFIED. ) ;
#19869 = CIRCLE ( 'NONE', #18833, 5.000000000000000000 ) ;
#19870 = CARTESIAN_POINT ( 'NONE',  ( -27.08702828306175547, 0.5765135930309237544, -2.226264228964716985 ) ) ;
#19871 = ORIENTED_EDGE ( 'NONE', *, *, #54536, .F. ) ;
#19872 = CARTESIAN_POINT ( 'NONE',  ( -27.09602251845210930, 2.320865065108510539, -0.1644056400645273475 ) ) ;
#19873 = CARTESIAN_POINT ( 'NONE',  ( 2.241352910868909643, 7.145045428366612050, -2.689314586382279604 ) ) ;
#19874 = CARTESIAN_POINT ( 'NONE',  ( 2.639814597422733833, -4.103563379978059977, 6.594772041715924793 ) ) ;
#19875 = DIRECTION ( 'NONE',  ( 0.000000000000000000, 0.000000000000000000, 1.000000000000000000 ) ) ;
#19876 = VECTOR ( 'NONE', #25489, 1000.000000000000000 ) ;
#19877 = CARTESIAN_POINT ( 'NONE',  ( -14.29135464769095520, 7.782112657557433089, -11.03126115115966854 ) ) ;
#19878 = EDGE_CURVE ( 'NONE', #41187, #20717, #56557, .T. ) ;
#19879 = ORIENTED_EDGE ( 'NONE', *, *, #50684, .T. ) ;
#19880 = CARTESIAN_POINT ( 'NONE',  ( 1.719304012338836563, -2.961219984258077087, 12.38166659046417095 ) ) ;
#19881 = EDGE_CURVE ( 'NONE', #41694, #31670, #29170, .T. ) ;
#19882 = CARTESIAN_POINT ( 'NONE',  ( 22.22678687964571864, 10.97453491530256464, -4.866768194205650211 ) ) ;
#19883 = CARTESIAN_POINT ( 'NONE',  ( -27.19357181888462094, 12.48377454417557253, 5.138615876886901468 ) ) ;
#19884 = CARTESIAN_POINT ( 'NONE',  ( 35.00000000000000000, 11.56998259273182583, 3.827046518384956020 ) ) ;
#19885 = CARTESIAN_POINT ( 'NONE',  ( -27.09569413923886216, 1.607816962455218102, -1.680421072128820192 ) ) ;
#19886 = DIRECTION ( 'NONE',  ( 0.000000000000000000, -0.9903235168508564001, -0.1387779952735713473 ) ) ;
#19887 = FACE_OUTER_BOUND ( 'NONE', #26706, .T. ) ;
#19888 = DIRECTION ( 'NONE',  ( -0.2475719085175098477, 0.000000000000000000, -0.9688695217174486674 ) ) ;
#19889 = EDGE_LOOP ( 'NONE', ( #30404, #45676, #58155, #24036 ) ) ;
#19890 = EDGE_CURVE ( 'NONE', #42057, #6580, #22334, .T. ) ;
#19891 = CARTESIAN_POINT ( 'NONE',  ( 0.3610902822527202183, 0.2623004149194609336, 12.27530799859938071 ) ) ;
#19892 = VERTEX_POINT ( 'NONE', #29467 ) ;
#19893 = DIRECTION ( 'NONE',  ( 1.000000000000000000, -0.000000000000000000, 0.000000000000000000 ) ) ;
#19894 = CARTESIAN_POINT ( 'NONE',  ( -22.28121537037576871, -3.680034389105489190, 0.3168735205819568357 ) ) ;
#19895 = CARTESIAN_POINT ( 'NONE',  ( 37.00000000000000711, -2.080187960898473687, 12.57916205664483122 ) ) ;
#19896 = CARTESIAN_POINT ( 'NONE',  ( 0.000000000000000000, -3.937687286050851831, 6.383151168292441113 ) ) ;
#19897 = DIRECTION ( 'NONE',  ( 0.000000000000000000, 0.01356324068817998940, -0.9999080150203989437 ) ) ;
#19898 = ADVANCED_FACE ( 'NONE', ( #19837 ), #35447, .T. ) ;
#19899 = VERTEX_POINT ( 'NONE', #49138 ) ;
#19900 = DIRECTION ( 'NONE',  ( -1.000000000000000000, -0.000000000000000000, 0.000000000000000000 ) ) ;
#19901 = CARTESIAN_POINT ( 'NONE',  ( 2.653899356899545037, 2.411250235128249653, -7.388433688587198844 ) ) ;
#19902 = CARTESIAN_POINT ( 'NONE',  ( 8.957194808219908211, 4.011391350595442162, 11.31236870852682941 ) ) ;
#19903 = FACE_OUTER_BOUND ( 'NONE', #62739, .T. ) ;
#19904 = CIRCLE ( 'NONE', #39027, 12.74999999999999822 ) ;
#19905 = CARTESIAN_POINT ( 'NONE',  ( 9.584295231686237315, 6.682444889156122336, -11.73468901934476705 ) ) ;
#19906 = CYLINDRICAL_SURFACE ( 'NONE', #53165, 12.75000000000000178 ) ;
#19907 = ORIENTED_EDGE ( 'NONE', *, *, #42072, .T. ) ;
#19908 = DIRECTION ( 'NONE',  ( 0.000000000000000000, 0.000000000000000000, 1.000000000000000000 ) ) ;
#19909 = VERTEX_POINT ( 'NONE', #60727 ) ;
#19910 = CYLINDRICAL_SURFACE ( 'NONE', #60946, 12.18650000000000055 ) ;
#19911 = CARTESIAN_POINT ( 'NONE',  ( -12.96770491601581021, -33.25366259606034447, 10.81293556751078988 ) ) ;
#19912 = CIRCLE ( 'NONE', #48607, 5.000000000000001776 ) ;
#19913 = CARTESIAN_POINT ( 'NONE',  ( 1.000000000000000888, 2.473437528934240515, -7.080403010454960011 ) ) ;
#19914 = CARTESIAN_POINT ( 'NONE',  ( 2.000000000000001776, 1.225832621831852931, 6.827324998361547159 ) ) ;
#19915 = ORIENTED_EDGE ( 'NONE', *, *, #12462, .F. ) ;
#19916 = AXIS2_PLACEMENT_3D ( 'NONE', #46125, #575, #41101 ) ;
#19917 = ORIENTED_EDGE ( 'NONE', *, *, #64696, .T. ) ;
#19918 = DIRECTION ( 'NONE',  ( -1.000000000000000000, 0.000000000000000000, 0.000000000000000000 ) ) ;
#19919 = ORIENTED_EDGE ( 'NONE', *, *, #58883, .T. ) ;
#19920 = LINE ( 'NONE', #39874, #48904 ) ;
#19921 = DIRECTION ( 'NONE',  ( 0.000000000000000000, 0.6943713148249640588, -0.7196168960969792083 ) ) ;
#19922 = DIRECTION ( 'NONE',  ( 0.000000000000000000, 0.2006870767258819854, -0.9796553971857756560 ) ) ;
#19923 = CARTESIAN_POINT ( 'NONE',  ( -36.00000000000000711, 6.711949091238296639, -10.84030624090599559 ) ) ;
#19924 = FACE_OUTER_BOUND ( 'NONE', #18641, .T. ) ;
#19925 = CYLINDRICAL_SURFACE ( 'NONE', #31702, 6.936499999999988120 ) ;
#19926 = CARTESIAN_POINT ( 'NONE',  ( 3.152665057733834431, -3.161213418913157991, 7.281573230474281289 ) ) ;
#19927 = ORIENTED_EDGE ( 'NONE', *, *, #1384, .T. ) ;
#19929 = ORIENTED_EDGE ( 'NONE', *, *, #46056, .T. ) ;
#19928 = CARTESIAN_POINT ( 'NONE',  ( 0.5572780756284301251, -10.83930267798907288, 5.905274004878299010 ) ) ;
#19930 = ORIENTED_EDGE ( 'NONE', *, *, #35157, .F. ) ;
#19931 = FACE_OUTER_BOUND ( 'NONE', #24350, .T. ) ;
#19932 = ADVANCED_FACE ( 'NONE', ( #3597 ), #49466, .T. ) ;
#19933 = CARTESIAN_POINT ( 'NONE',  ( 2.990245332647754051, 7.587819667496316534, -3.789007530133582602 ) ) ;
#19934 = VERTEX_POINT ( 'NONE', #4215 ) ;
#19935 = DIRECTION ( 'NONE',  ( 0.000000000000000000, 0.01356324068817998940, -0.9999080150203990547 ) ) ;
#19936 = ORIENTED_EDGE ( 'NONE', *, *, #28185, .T. ) ;
#19937 = CARTESIAN_POINT ( 'NONE',  ( 35.00000000000000000, -11.73808581813437613, 0.4353888892049613824 ) ) ;
#19938 = CARTESIAN_POINT ( 'NONE',  ( 5.635198476044180893, -9.293512099126084891, -9.797319838910391709 ) ) ;
#19939 = CYLINDRICAL_SURFACE ( 'NONE', #16968, 4.999999999999999112 ) ;
#19940 = CARTESIAN_POINT ( 'NONE',  ( 4.681985117566611621, -10.64506698050158207, 5.541855235442475269 ) ) ;
#19941 = ORIENTED_EDGE ( 'NONE', *, *, #4956, .T. ) ;
#19942 = ORIENTED_EDGE ( 'NONE', *, *, #39476, .F. ) ;
#19943 = CARTESIAN_POINT ( 'NONE',  ( -35.00000000000000000, -3.213188559034318992, 11.29812557209475798 ) ) ;
#19944 = VERTEX_POINT ( 'NONE', #45111 ) ;
#19945 = DIRECTION ( 'NONE',  ( -1.000000000000000000, 0.000000000000000000, -0.000000000000000000 ) ) ;
#19946 = EDGE_LOOP ( 'NONE', ( #41348, #44396, #37010, #44446 ) ) ;
#19947 = ORIENTED_EDGE ( 'NONE', *, *, #31725, .F. ) ;
#19948 = ORIENTED_EDGE ( 'NONE', *, *, #18987, .F. ) ;
#19949 = CARTESIAN_POINT ( 'NONE',  ( 2.491965175173544100, -5.773748672881963806, 5.121563073453287096 ) ) ;
#19951 = AXIS2_PLACEMENT_3D ( 'NONE', #18817, #39077, #55705 ) ;
#19950 = CARTESIAN_POINT ( 'NONE',  ( -14.48921874744988614, -27.84739049628997876, 11.52341872854555227 ) ) ;
#19952 = ADVANCED_FACE ( 'NONE', ( #29789 ), #39124, .T. ) ;
#19953 = CARTESIAN_POINT ( 'NONE',  ( 2.835339799623985968, -1.035140033449997388, -7.763739326985123590 ) ) ;
#19954 = CARTESIAN_POINT ( 'NONE',  ( -41.00000000000000711, -45.00200000000000244, -4.500000000000000888 ) ) ;
#19955 = DIRECTION ( 'NONE',  ( 0.000000000000000000, -0.01356324068818000328, 0.9999080150203990547 ) ) ;
#19956 = ORIENTED_EDGE ( 'NONE', *, *, #1728, .T. ) ;
#19957 = CARTESIAN_POINT ( 'NONE',  ( 2.242819959140598840, -2.514828506625285787, -7.208832857235797142 ) ) ;
#19958 = AXIS2_PLACEMENT_3D ( 'NONE', #32627, #58261, #17373 ) ;
#19959 = EDGE_LOOP ( 'NONE', ( #19045, #7493, #13222, #37863 ) ) ;
#19960 = LINE ( 'NONE', #60194, #48695 ) ;
#19961 = EDGE_CURVE ( 'NONE', #10662, #31156, #49114, .T. ) ;
#19962 = CARTESIAN_POINT ( 'NONE',  ( -18.54676851533650961, -5.050683831495517140, -12.52189472075509613 ) ) ;
#19963 = ADVANCED_FACE ( 'NONE', ( #44426 ), #60389, .T. ) ;
#19964 = ORIENTED_EDGE ( 'NONE', *, *, #27319, .T. ) ;
#19965 = CARTESIAN_POINT ( 'NONE',  ( 0.2676618633000425462, -10.68562420805846891, 5.983781707237577407 ) ) ;
#19966 = CARTESIAN_POINT ( 'NONE',  ( 0.2911222467163552818, 3.989243506922341531, 11.58731125337560997 ) ) ;
#19967 = CARTESIAN_POINT ( 'NONE',  ( 1.000000000000000888, 3.795144977083636739, 6.468916029978800886 ) ) ;
#19968 = AXIS2_PLACEMENT_3D ( 'NONE', #14703, #9731, #30021 ) ;
#19969 = ORIENTED_EDGE ( 'NONE', *, *, #37619, .T. ) ;
#19970 = EDGE_CURVE ( 'NONE', #12635, #42754, #40601, .T. ) ;
#19971 = DIRECTION ( 'NONE',  ( -0.3939253465568943180, -0.4511294145502819930, 0.8008152550167551009 ) ) ;
#19972 = ORIENTED_EDGE ( 'NONE', *, *, #25103, .F. ) ;
#19973 = EDGE_CURVE ( 'NONE', #61727, #662, #33184, .T. ) ;
#19974 = CARTESIAN_POINT ( 'NONE',  ( -24.53364844038847892, -11.34588198318266095, 7.318208206151304296 ) ) ;
#19975 = SURFACE_SIDE_STYLE ('',( #65506 ) ) ;
#19976 = CARTESIAN_POINT ( 'NONE',  ( -18.85528480568559573, -29.92804508438502609, 6.903306693652388581 ) ) ;
#19977 = CARTESIAN_POINT ( 'NONE',  ( 2.491965175173810998, 4.041154086925143218, 6.575382551509535212 ) ) ;
#19978 = CARTESIAN_POINT ( 'NONE',  ( 11.15383795322125771, 11.94197166349967532, -1.183955411781195011 ) ) ;
#19979 = ORIENTED_EDGE ( 'NONE', *, *, #23807, .F. ) ;
#19980 = CARTESIAN_POINT ( 'NONE',  ( 2.266490820343232127, -4.800466063945415307, 5.947069344280080827 ) ) ;
#19981 = DIRECTION ( 'NONE',  ( 0.000000000000000000, 0.5155538571770171830, 0.8568571761675919385 ) ) ;
#19982 = CARTESIAN_POINT ( 'NONE',  ( -27.20102706715912788, -1.765193291701709688, 1.966718264078082923 ) ) ;
#19983 = DIRECTION ( 'NONE',  ( 0.000000000000000000, 0.4134677391718449835, 0.9105187689795983808 ) ) ;
#19984 = EDGE_CURVE ( 'NONE', #20076, #16407, #28710, .T. ) ;
#19985 = CARTESIAN_POINT ( 'NONE',  ( -7.961359079021525176, -27.27258404549933246, -15.08967732372090609 ) ) ;
#19986 = CIRCLE ( 'NONE', #53983, 6.936499999999989008 ) ;
#19987 = ADVANCED_FACE ( 'NONE', ( #31446 ), #1541, .T. ) ;
#19988 = DIRECTION ( 'NONE',  ( -1.000000000000000000, 0.000000000000000000, 0.000000000000000000 ) ) ;
#19989 = CARTESIAN_POINT ( 'NONE',  ( 5.516018279890452902, -0.005331956019561440684, -0.004180585980734585240 ) ) ;
#19990 = DIRECTION ( 'NONE',  ( 1.000000000000000000, 0.000000000000000000, 0.000000000000000000 ) ) ;
#19991 = CARTESIAN_POINT ( 'NONE',  ( 35.00000000000000000, 0.7214809346830272085, 11.72397916322010936 ) ) ;
#19992 = AXIS2_PLACEMENT_3D ( 'NONE', #30809, #32457, #5925 ) ;
#19993 = VERTEX_POINT ( 'NONE', #58281 ) ;
#19994 = CARTESIAN_POINT ( 'NONE',  ( -27.09048036756591671, -1.306202114107277712, -1.905306051559101377 ) ) ;
#19995 = CIRCLE ( 'NONE', #23180, 12.18650000000000233 ) ;
#19996 = ORIENTED_EDGE ( 'NONE', *, *, #46988, .F. ) ;
#19998 =( BOUNDED_SURFACE ( )  B_SPLINE_SURFACE ( 3, 1, ( 
 ( #195, #36062 ),
 ( #16130, #4864 ),
 ( #51724, #25130 ),
 ( #15471, #35735 ) ),
 .UNSPECIFIED., .F., .F., .F. ) 
 B_SPLINE_SURFACE_WITH_KNOTS ( ( 4, 4 ),
 ( 2, 2 ),
 ( 0.000000000000000000, 1.000000000000000000 ),
 ( 0.000000000000000000, 1.000000000000000000 ),
 .UNSPECIFIED. ) 
 GEOMETRIC_REPRESENTATION_ITEM ( )  RATIONAL_B_SPLINE_SURFACE ( (
 ( 1.000000000000000000, 1.000000000000000000),
 ( 0.8716676215708681896, 0.8964445200148164483),
 ( 0.8716676215708681896, 0.8964445200148164483),
 ( 1.000000000000000000, 1.000000000000000000) ) ) 
 REPRESENTATION_ITEM ( '' )  SURFACE ( )  );
#19997 = CARTESIAN_POINT ( 'NONE',  ( 35.00000000000000000, -3.645068577059948911, 11.16627499335658413 ) ) ;
#19999 = DIRECTION ( 'NONE',  ( 0.000000000000000000, 0.1118654143051615590, 0.9937233664769760111 ) ) ;
#20000 = CARTESIAN_POINT ( 'NONE',  ( 3.152665057734062248, -7.609997527621111146, 2.258875078502258216 ) ) ;
#20001 = AXIS2_PLACEMENT_3D ( 'NONE', #39912, #40229, #10304 ) ;
#20002 = CARTESIAN_POINT ( 'NONE',  ( 0.000000000000000000, -3.786546189469129686, -5.663561025469209476 ) ) ;
#20003 = VERTEX_POINT ( 'NONE', #51432 ) ;
#20004 = ORIENTED_EDGE ( 'NONE', *, *, #13906, .F. ) ;
#20005 = AXIS2_PLACEMENT_3D ( 'NONE', #5596, #14861, #35149 ) ;
#20006 = ORIENTED_EDGE ( 'NONE', *, *, #39789, .T. ) ;
#20007 = CARTESIAN_POINT ( 'NONE',  ( 29.60305162835625126, -8.975199590264201888, 7.980219161752089008 ) ) ;
#20008 = ADVANCED_FACE ( 'NONE', ( #42973 ), #40002, .F. ) ;
#20009 = CARTESIAN_POINT ( 'NONE',  ( -22.27709082389155171, 0.8996430462092437352, 3.569727173833806333 ) ) ;
#20010 = ORIENTED_EDGE ( 'NONE', *, *, #3512, .F. ) ;
#20011 = CARTESIAN_POINT ( 'NONE',  ( 37.00000000000000711, -11.01837265713068703, 6.415447294506815723 ) ) ;
#20012 = DIRECTION ( 'NONE',  ( -1.000000000000000000, 0.000000000000000000, 0.000000000000000000 ) ) ;
#20013 = CARTESIAN_POINT ( 'NONE',  ( 2.000000000000001776, 7.414200355365259121, 1.131208685655164414 ) ) ;
#20014 = ORIENTED_EDGE ( 'NONE', *, *, #58452, .F. ) ;
#20015 = CARTESIAN_POINT ( 'NONE',  ( 2.257661810676953262, 4.806737555285070407, -5.938215228163155501 ) ) ;
#20016 = ADVANCED_FACE ( 'NONE', ( #46736 ), #5545, .T. ) ;
#20017 = CARTESIAN_POINT ( 'NONE',  ( 2.128776824815503677, -26.59425375116049040, -16.16470972310717968 ) ) ;
#20018 = CARTESIAN_POINT ( 'NONE',  ( -4.806344283790351390, -7.508992741355383416, 25.00000000000000000 ) ) ;
#20020 = ORIENTED_EDGE ( 'NONE', *, *, #7883, .T. ) ;
#20019 = CARTESIAN_POINT ( 'NONE',  ( 41.00000000000000711, -25.45369917733758314, 1.516638822270951703 ) ) ;
#20021 = LINE ( 'NONE', #9369, #43726 ) ;
#20022 = ORIENTED_EDGE ( 'NONE', *, *, #26584, .T. ) ;
#20023 = CARTESIAN_POINT ( 'NONE',  ( 0.3474126878361845638, -6.359473273659631332, -10.49748369253938307 ) ) ;
#20024 = EDGE_CURVE ( 'NONE', #63348, #50423, #62895, .T. ) ;
#20025 = ORIENTED_EDGE ( 'NONE', *, *, #62017, .T. ) ;
#20026 = B_SPLINE_CURVE_WITH_KNOTS ( 'NONE', 3,
 ( #60367, #4196, #50083, #19156, #39428, #4542, #9169, #49448, #13500, #49749, #24808, #33782, #24462, #19818, #53767, #44742, #65024, #64053, #40079, #28472, #19496, #54084, #39766, #8517 ),
 .UNSPECIFIED., .F., .F.,
 ( 4, 2, 2, 2, 2, 2, 2, 2, 2, 2, 2, 4 ),
 ( 0.000000000000000000, 0.001281805353653630913, 0.001922708030480444093, 0.002563610707307257489, 0.003204513384134070452, 0.003845416060960883849, 0.005127221414614510642, 0.005768124091441322737, 0.006409026768268135700, 0.007690832121921758156, 0.008972637475575379745, 0.01025444282922900220 ),
 .UNSPECIFIED. ) ;
#20027 = DIRECTION ( 'NONE',  ( 0.000000000000000000, 0.000000000000000000, 1.000000000000000000 ) ) ;
#20028 = CARTESIAN_POINT ( 'NONE',  ( 12.36261888780203222, -8.715147324829775499, -8.257870389522178556 ) ) ;
#20029 = CARTESIAN_POINT ( 'NONE',  ( -37.00000000000000711, -11.53507381115581687, -2.216820770815207897 ) ) ;
#20030 = CARTESIAN_POINT ( 'NONE',  ( 1.372161826076679469, -6.811451307636759545, -10.61825687422748388 ) ) ;
#20031 = CARTESIAN_POINT ( 'NONE',  ( -27.05748184469818440, 3.214204530190199804, 0.2721081511922631146 ) ) ;
#20033 = DIRECTION ( 'NONE',  ( 0.000000000000000000, -0.9246979985058764173, -0.3807014730195119045 ) ) ;
#20032 = CIRCLE ( 'NONE', #41279, 5.000000000000000000 ) ;
#20034 = EDGE_CURVE ( 'NONE', #53922, #31267, #59725, .T. ) ;
#20035 = DIRECTION ( 'NONE',  ( 1.000000000000000000, 0.000000000000000000, 0.000000000000000000 ) ) ;
#20036 = CARTESIAN_POINT ( 'NONE',  ( -27.08418322526030764, 2.265123059255413462, -0.3452258100746935510 ) ) ;
#20037 = CARTESIAN_POINT ( 'NONE',  ( -35.00000000000000000, 0.8294751490781091530, -12.15823808070321732 ) ) ;
#20039 = ORIENTED_EDGE ( 'NONE', *, *, #20655, .T. ) ;
#20038 = CARTESIAN_POINT ( 'NONE',  ( -18.36801285212142432, 3.941043466613568746, -12.91410746298855372 ) ) ;
#20040 = CYLINDRICAL_SURFACE ( 'NONE', #26886, 5.000000000000000888 ) ;
#20041 = ORIENTED_EDGE ( 'NONE', *, *, #20881, .T. ) ;
#20042 = AXIS2_PLACEMENT_3D ( 'NONE', #4848, #25117, #31082 ) ;
#20043 = CARTESIAN_POINT ( 'NONE',  ( -2.952869152607106251, 25.00000000000000000, 3.755417052241485365 ) ) ;
#20044 = ORIENTED_EDGE ( 'NONE', *, *, #20628, .T. ) ;
#20045 = EDGE_CURVE ( 'NONE', #48006, #49701, #37399, .T. ) ;
#20046 = ORIENTED_EDGE ( 'NONE', *, *, #63652, .T. ) ;
#20047 = LINE ( 'NONE', #45636, #31783 ) ;
#20048 = CARTESIAN_POINT ( 'NONE',  ( 36.00000000000000711, -12.71517666308947092, 0.9416912585475705200 ) ) ;
#20049 = CARTESIAN_POINT ( 'NONE',  ( -27.15525204139122550, -0.7327319213109896312, -2.394850816831294527 ) ) ;
#20050 = DIRECTION ( 'NONE',  ( -1.000000000000000000, 0.000000000000000000, 0.000000000000000000 ) ) ;
#20051 = CIRCLE ( 'NONE', #11538, 1.500000000000000444 ) ;
#20052 = DIRECTION ( 'NONE',  ( -0.000000000000000000, -1.000000000000000000, -0.000000000000000000 ) ) ;
#20053 = CIRCLE ( 'NONE', #30667, 12.18650000000000055 ) ;
#20054 = CIRCLE ( 'NONE', #57222, 6.936499999999989008 ) ;
#20055 = ORIENTED_EDGE ( 'NONE', *, *, #29547, .F. ) ;
#20056 = EDGE_CURVE ( 'NONE', #38732, #26571, #7711, .T. ) ;
#20057 = CARTESIAN_POINT ( 'NONE',  ( 2.835339799623973089, -6.206025468804385881, 4.778327228934561965 ) ) ;
#20058 = DIRECTION ( 'NONE',  ( 0.000000000000000000, 0.01356324068817992175, -0.9999080150203990547 ) ) ;
#20059 = FACE_OUTER_BOUND ( 'NONE', #33796, .T. ) ;
#20060 = EDGE_CURVE ( 'NONE', #43097, #15504, #10877, .T. ) ;
#20061 = VERTEX_POINT ( 'NONE', #21477 ) ;
#20062 = AXIS2_PLACEMENT_3D ( 'NONE', #24802, #50729, #34742 ) ;
#20063 = EDGE_CURVE ( 'NONE', #8847, #31243, #20816, .T. ) ;
#20064 = ADVANCED_FACE ( 'NONE', ( #41083 ), #41748, .T. ) ;
#20065 = ADVANCED_FACE ( 'NONE', ( #26787 ), #23352, .T. ) ;
#20066 = CARTESIAN_POINT ( 'NONE',  ( 49.83768944945995827, -0.03330036048198387055, -3.290779520873021724 ) ) ;
#20067 = ADVANCED_FACE ( 'NONE', ( #29322 ), #58627, .T. ) ;
#20068 = DIRECTION ( 'NONE',  ( 0.000000000000000000, -0.6876994588534294239, 0.7259954919231249582 ) ) ;
#20069 = LINE ( 'NONE', #48468, #34873 ) ;
#20070 = VERTEX_POINT ( 'NONE', #28341 ) ;
#20071 = CARTESIAN_POINT ( 'NONE',  ( 37.00000000000000711, 4.705694406421931860E-17, -3.469127814946512892E-15 ) ) ;
#20072 = CYLINDRICAL_SURFACE ( 'NONE', #12321, 12.18650000000000055 ) ;
#20073 = CARTESIAN_POINT ( 'NONE',  ( 3.329269835863156501, 3.383330847102705263, 11.51505321664975412 ) ) ;
#20074 = DIRECTION ( 'NONE',  ( 0.000000000000000000, -0.01356324068817999114, 0.9999080150203989437 ) ) ;
#20075 = CARTESIAN_POINT ( 'NONE',  ( 5.515188684475870851, 0.001485678338381713100, 0.005140903460551141980 ) ) ;
#20076 = VERTEX_POINT ( 'NONE', #13689 ) ;
#20077 = AXIS2_PLACEMENT_3D ( 'NONE', #1983, #22251, #62172 ) ;
#20078 = CARTESIAN_POINT ( 'NONE',  ( 0.000000000000000000, 0.3246585432986198727, 6.805031400696091914 ) ) ;
#20079 = CARTESIAN_POINT ( 'NONE',  ( 3.419514237176616067, 7.633187743098319267, -9.298209040439605388 ) ) ;
#20080 = CARTESIAN_POINT ( 'NONE',  ( 5.516018279890452902, -0.006771744149385265123, 0.0002248006052448276067 ) ) ;
#20081 = ORIENTED_EDGE ( 'NONE', *, *, #46210, .F. ) ;
#20082 = DIRECTION ( 'NONE',  ( -1.000000000000000000, 0.000000000000000000, 0.000000000000000000 ) ) ;
#20083 = CARTESIAN_POINT ( 'NONE',  ( 2.241509619876139059, 6.592435552901117823, 3.850348903238736131 ) ) ;
#20084 = EDGE_LOOP ( 'NONE', ( #41561, #13032, #49398, #51287 ) ) ;
#20085 = ORIENTED_EDGE ( 'NONE', *, *, #40467, .T. ) ;
#20086 = ORIENTED_EDGE ( 'NONE', *, *, #62484, .T. ) ;
#20087 = AXIS2_PLACEMENT_3D ( 'NONE', #6153, #26419, #41369 ) ;
#20088 = EDGE_CURVE ( 'NONE', #52731, #54109, #17247, .T. ) ;
#20089 = ORIENTED_EDGE ( 'NONE', *, *, #19694, .T. ) ;
#20090 = DIRECTION ( 'NONE',  ( 0.000000000000000000, 0.000000000000000000, 1.000000000000000000 ) ) ;
#20091 = CARTESIAN_POINT ( 'NONE',  ( 37.00000000000000711, 4.705694406421931860E-17, -3.469127814946512892E-15 ) ) ;
#20092 = AXIS2_PLACEMENT_3D ( 'NONE', #7468, #17470, #27760 ) ;
#20093 = FACE_OUTER_BOUND ( 'NONE', #13291, .T. ) ;
#20094 = FACE_OUTER_BOUND ( 'NONE', #25895, .T. ) ;
#20095 = CARTESIAN_POINT ( 'NONE',  ( -14.06029564544070531, -34.40539544390912141, 8.431086515739542264 ) ) ;
#20096 = DIRECTION ( 'NONE',  ( 0.000000000000000000, -0.01356324068818000848, 0.9999080150203990547 ) ) ;
#20098 = VERTEX_POINT ( 'NONE', #38305 ) ;
#20097 = CARTESIAN_POINT ( 'NONE',  ( 0.2648978790185593790, -12.03635331166810651, -2.256510822326266652 ) ) ;
#20099 = CYLINDRICAL_SURFACE ( 'NONE', #21435, 13.50000000000000178 ) ;
#20100 = ORIENTED_EDGE ( 'NONE', *, *, #28579, .F. ) ;
#20101 = CARTESIAN_POINT ( 'NONE',  ( 2.000000000000001776, 0.000000000000000000, 0.000000000000000000 ) ) ;
#20102 = ORIENTED_EDGE ( 'NONE', *, *, #23807, .T. ) ;
#20103 = EDGE_CURVE ( 'NONE', #61553, #39884, #1760, .T. ) ;
#20104 = CIRCLE ( 'NONE', #34984, 3.000000000000000444 ) ;
#20105 = VERTEX_POINT ( 'NONE', #28662 ) ;
#20106 = CARTESIAN_POINT ( 'NONE',  ( -22.27878402819507997, -0.9457981527432397506, 3.562981801125739700 ) ) ;
#20107 = CARTESIAN_POINT ( 'NONE',  ( 9.704251177394615624, -29.31945899942111211, 10.96599872320776115 ) ) ;
#20108 = FACE_OUTER_BOUND ( 'NONE', #12053, .T. ) ;
#20109 = CARTESIAN_POINT ( 'NONE',  ( -36.00000000000000711, -4.237174932027141239, -12.02534193257725725 ) ) ;
#20110 = DIRECTION ( 'NONE',  ( -1.000000000000000000, 0.000000000000000000, 0.000000000000000000 ) ) ;
#20111 = LINE ( 'NONE', #25108, #50093 ) ;
#20112 = VERTEX_POINT ( 'NONE', #38972 ) ;
#20113 = VERTEX_POINT ( 'NONE', #48974 ) ;
#20114 = CARTESIAN_POINT ( 'NONE',  ( -26.74023318801844340, -2.752802096869876536, -1.916028097164421906 ) ) ;
#20115 = ORIENTED_EDGE ( 'NONE', *, *, #65433, .F. ) ;
#20116 = B_SPLINE_CURVE_WITH_KNOTS ( 'NONE', 3,
 ( #56506, #10951, #5311, #57169, #51544, #21243, #46215, #30888, #31550, #26563, #51207, #657, #20916, #37185, #51852, #41190 ),
 .UNSPECIFIED., .F., .F.,
 ( 4, 3, 3, 3, 3, 4 ),
 ( 2.342674890740637216E-15, 0.0002126834539179767430, 0.0004253519300366382250, 0.0006380165497224343871, 0.0007442707582428458989, 0.0009453531351416440912 ),
 .UNSPECIFIED. ) ;
#20117 = ADVANCED_FACE ( 'NONE', ( #4058 ), #34306, .T. ) ;
#20118 = ORIENTED_EDGE ( 'NONE', *, *, #29727, .F. ) ;
#20119 = DIRECTION ( 'NONE',  ( -1.000000000000000000, 0.000000000000000000, 0.000000000000000000 ) ) ;
#20120 = DIRECTION ( 'NONE',  ( -1.000000000000000000, 0.000000000000000000, 0.000000000000000000 ) ) ;
#20121 = CARTESIAN_POINT ( 'NONE',  ( -22.28546858134833641, 0.9133285433746859416, -3.592117891549496900 ) ) ;
#20122 = CARTESIAN_POINT ( 'NONE',  ( 18.21295819262132554, -5.177675556671182733, 10.87722373139338572 ) ) ;
#20123 = DIRECTION ( 'NONE',  ( -1.000000000000000000, 0.000000000000000000, 0.000000000000000000 ) ) ;
#20124 = CARTESIAN_POINT ( 'NONE',  ( 37.00000000000000711, 10.70999494708492250, -5.814360711498331113 ) ) ;
#20125 = AXIS2_PLACEMENT_3D ( 'NONE', #28564, #65434, #64772 ) ;
#20126 = DIRECTION ( 'NONE',  ( 1.000000000000000000, 0.000000000000000000, -0.000000000000000000 ) ) ;
#20127 = ORIENTED_EDGE ( 'NONE', *, *, #8853, .T. ) ;
#20128 = AXIS2_PLACEMENT_3D ( 'NONE', #62812, #17278, #36226 ) ;
#20129 = EDGE_LOOP ( 'NONE', ( #24095, #53322, #18303, #58086 ) ) ;
#20130 = DIRECTION ( 'NONE',  ( -1.000000000000000000, 0.000000000000000000, 0.000000000000000000 ) ) ;
#20131 = CARTESIAN_POINT ( 'NONE',  ( 37.00000000000000711, 4.986700593229853595, 10.63508530065516311 ) ) ;
#20132 = DIRECTION ( 'NONE',  ( 0.000000000000000000, 0.000000000000000000, 1.000000000000000000 ) ) ;
#20133 = ADVANCED_FACE ( 'NONE', ( #33972 ), #18717, .T. ) ;
#20134 = ADVANCED_FACE ( 'NONE', ( #29007 ), #7741, .T. ) ;
#20135 = CARTESIAN_POINT ( 'NONE',  ( 6.645030759940484977, -5.062125397348413713, 10.88741911013856267 ) ) ;
#20136 = CARTESIAN_POINT ( 'NONE',  ( -22.31328051695926007, 2.109671368890633669, 3.148362328073145200 ) ) ;
#20137 = EDGE_CURVE ( 'NONE', #7394, #51465, #28919, .T. ) ;
#20138 = CARTESIAN_POINT ( 'NONE',  ( 24.36109623891380949, -0.0007059690029652561632, -13.50466814640359914 ) ) ;
#20139 = DIRECTION ( 'NONE',  ( -1.000000000000000000, -0.000000000000000000, -0.000000000000000000 ) ) ;
#20140 = EDGE_CURVE ( 'NONE', #10101, #41887, #2776, .T. ) ;
#20141 = CARTESIAN_POINT ( 'NONE',  ( -27.08418322526030764, -2.134267017050454296, -0.8335872080609635359 ) ) ;
#20142 = ORIENTED_EDGE ( 'NONE', *, *, #19638, .T. ) ;
#20143 = CARTESIAN_POINT ( 'NONE',  ( 3.100650473569728671, -0.4517506188708464432, 7.907988569972077997 ) ) ;
#20144 = DIRECTION ( 'NONE',  ( 0.000000000000000000, 0.5987040770935622147, -0.8009703041134208501 ) ) ;
#20145 = DIRECTION ( 'NONE',  ( 1.000000000000000000, 0.000000000000000000, 0.000000000000000000 ) ) ;
#20146 = TOROIDAL_SURFACE ( 'NONE', #36071, 20.19615242270663558, 4.000000000000000000 ) ;
#20147 = CARTESIAN_POINT ( 'NONE',  ( -12.63451720668099476, -33.87771254755882921, -9.962109630950775951 ) ) ;
#20148 = CARTESIAN_POINT ( 'NONE',  ( 2.717984159219867468, -7.221467817271594036, 2.930214355830794037 ) ) ;
#20149 = VERTEX_POINT ( 'NONE', #44591 ) ;
#20150 = CARTESIAN_POINT ( 'NONE',  ( 2.241537034860906275, 7.634469414369386087, 0.004719967007703176898 ) ) ;
#20151 = CARTESIAN_POINT ( 'NONE',  ( 35.00000000000000000, -7.146664589317845540, 9.321877890560507751 ) ) ;
#20152 = CARTESIAN_POINT ( 'NONE',  ( 12.83306155034124707, -29.03814089299731549, -3.459227852999859021 ) ) ;
#20153 = ORIENTED_EDGE ( 'NONE', *, *, #18900, .F. ) ;
#20154 = CARTESIAN_POINT ( 'NONE',  ( 1.000000000000000888, 5.769711778877386621, -4.791703871138487614 ) ) ;
#20155 = DIRECTION ( 'NONE',  ( 1.000000000000000000, -0.000000000000000000, 0.000000000000000000 ) ) ;
#20156 = CARTESIAN_POINT ( 'NONE',  ( -22.29382655386184453, -1.036465316386235180, -3.584644999358109985 ) ) ;
#20158 = ORIENTED_EDGE ( 'NONE', *, *, #14547, .T. ) ;
#20157 = CARTESIAN_POINT ( 'NONE',  ( 0.000000000000000000, -3.786546189469212731, 5.663561025469122434 ) ) ;
#20159 = DIRECTION ( 'NONE',  ( 0.000000000000000000, 0.8696919319575200369, 0.4935949184179230786 ) ) ;
#20160 = AXIS2_PLACEMENT_3D ( 'NONE', #11322, #46260, #55895 ) ;
#20161 = EDGE_CURVE ( 'NONE', #17080, #13015, #19394, .T. ) ;
#20162 = VECTOR ( 'NONE', #25868, 1000.000000000000000 ) ;
#20163 = CARTESIAN_POINT ( 'NONE',  ( 35.00000000000000000, 11.71932350927024657, -3.511386971104992760 ) ) ;
#20164 = ORIENTED_EDGE ( 'NONE', *, *, #38512, .F. ) ;
#20165 = CARTESIAN_POINT ( 'NONE',  ( 0.3537226245948358883, 7.688925565305018139, 9.569332148897489176 ) ) ;
#20166 = EDGE_CURVE ( 'NONE', #48019, #9242, #713, .T. ) ;
#20167 = CARTESIAN_POINT ( 'NONE',  ( -2.682146249266192939, -4.811221336669188275, 10.99569137319423007 ) ) ;
#20168 = DIRECTION ( 'NONE',  ( 0.000000000000000000, 0.01356324068817998940, -0.9999080150203990547 ) ) ;
#20169 = CARTESIAN_POINT ( 'NONE',  ( 1.634816307077574971, -1.494046826341809853, -12.61459884933005782 ) ) ;
#20170 = CARTESIAN_POINT ( 'NONE',  ( 0.3106921474978483477, -11.43920276778354328, -4.414111574791946602 ) ) ;
#20171 = CARTESIAN_POINT ( 'NONE',  ( -17.68605346665446731, 2.867042001558842035, 13.19364479757039454 ) ) ;
#20172 = FACE_OUTER_BOUND ( 'NONE', #4133, .T. ) ;
#20173 = ORIENTED_EDGE ( 'NONE', *, *, #33703, .F. ) ;
#20174 = DIRECTION ( 'NONE',  ( 0.000000000000000000, -0.01356324068817991828, 0.9999080150203990547 ) ) ;
#20175 = ORIENTED_EDGE ( 'NONE', *, *, #10532, .F. ) ;
#20176 = ADVANCED_FACE ( 'NONE', ( #14654 ), #45935, .T. ) ;
#20177 = VECTOR ( 'NONE', #49785, 1000.000000000000000 ) ;
#20178 = CARTESIAN_POINT ( 'NONE',  ( 35.00000000000000000, 8.954052073409734192, 9.076753354953893904 ) ) ;
#20179 = CARTESIAN_POINT ( 'NONE',  ( 5.520433897694421610, -0.01473594271720286668, 0.003119431460922364278 ) ) ;
#20181 = ORIENTED_EDGE ( 'NONE', *, *, #50536, .T. ) ;
#20180 = VECTOR ( 'NONE', #55415, 1000.000000000000000 ) ;
#20182 = CARTESIAN_POINT ( 'NONE',  ( 0.2646305136544065406, -10.53923716745242345, -6.237419468587189542 ) ) ;
#20183 =( BOUNDED_SURFACE ( )  B_SPLINE_SURFACE ( 3, 1, ( 
 ( #12192, #41797 ),
 ( #37466, #37126 ),
 ( #11859, #52457 ),
 ( #17529, #47461 ) ),
 .UNSPECIFIED., .F., .F., .F. ) 
 B_SPLINE_SURFACE_WITH_KNOTS ( ( 4, 4 ),
 ( 2, 2 ),
 ( 0.000000000000000000, 1.000000000000000000 ),
 ( 0.000000000000000000, 1.000000000000000000 ),
 .UNSPECIFIED. ) 
 GEOMETRIC_REPRESENTATION_ITEM ( )  RATIONAL_B_SPLINE_SURFACE ( (
 ( 1.000000000000000000, 1.000000000000000000),
 ( 0.9932032654565553509, 0.8386279382598740284),
 ( 0.9932032654565553509, 0.8386279382598740284),
 ( 1.000000000000000000, 1.000000000000000000) ) ) 
 REPRESENTATION_ITEM ( '' )  SURFACE ( )  );
#20184 = CYLINDRICAL_SURFACE ( 'NONE', #35070, 11.99999999999998579 ) ;
#20185 = ORIENTED_EDGE ( 'NONE', *, *, #60748, .T. ) ;
#20186 = ORIENTED_EDGE ( 'NONE', *, *, #15449, .T. ) ;
#20187 = CARTESIAN_POINT ( 'NONE',  ( -36.00000000000000711, -5.300372733891724586, 11.59605747147784882 ) ) ;
#20188 = ADVANCED_FACE ( 'NONE', ( #25985 ), #4739, .T. ) ;
#20189 = ADVANCED_FACE ( 'NONE', ( #10664 ), #39951, .T. ) ;
#20190 = VERTEX_POINT ( 'NONE', #9682 ) ;
#20191 = DIRECTION ( 'NONE',  ( 1.000000000000000000, 0.000000000000000000, -0.000000000000000000 ) ) ;
#20192 = CARTESIAN_POINT ( 'NONE',  ( -37.00000000000000711, 0.000000000000000000, 0.000000000000000000 ) ) ;
#20193 = CARTESIAN_POINT ( 'NONE',  ( -27.08429572838383947, 2.279961732801592422, -0.2296550094122856711 ) ) ;
#20194 = EDGE_CURVE ( 'NONE', #26404, #49976, #60232, .T. ) ;
#20195 = CARTESIAN_POINT ( 'NONE',  ( 2.263328370261530331, 7.131064289852376170, -2.746620058315224711 ) ) ;
#20196 = CARTESIAN_POINT ( 'NONE',  ( -35.00000000000000000, 5.428340790341860789, -10.91072401419405402 ) ) ;
#20197 = CARTESIAN_POINT ( 'NONE',  ( 0.2651627682582926582, -10.56115808354087093, 6.199212018117401968 ) ) ;
#20198 = DIRECTION ( 'NONE',  ( 1.000000000000000000, -0.000000000000000000, 0.000000000000000000 ) ) ;
#20199 = ORIENTED_EDGE ( 'NONE', *, *, #53682, .T. ) ;
#20200 = CARTESIAN_POINT ( 'NONE',  ( 2.273267844204862609, 7.643541951623948449, -0.1513603614830752175 ) ) ;
#20201 = CARTESIAN_POINT ( 'NONE',  ( 3.152665057734119536, 7.281573230474295499, 3.161213418913482620 ) ) ;
#20202 = DIRECTION ( 'NONE',  ( 1.000000000000000000, 0.000000000000000000, 0.000000000000000000 ) ) ;
#20203 = CARTESIAN_POINT ( 'NONE',  ( 10.52156035929954392, 13.42709648837756475, -1.404459109811407203 ) ) ;
#20204 = CARTESIAN_POINT ( 'NONE',  ( -22.71097035706203116, 4.965150228107710006, 0.4203397252017151420 ) ) ;
#20205 = DIRECTION ( 'NONE',  ( 0.000000000000000000, -0.01356324068817991828, 0.9999080150203990547 ) ) ;
#20206 = DIRECTION ( 'NONE',  ( -1.000000000000000000, 0.000000000000000000, 0.000000000000000000 ) ) ;
#20207 = CARTESIAN_POINT ( 'NONE',  ( 35.00000000000000000, 4.705694406421931860E-17, -3.469127814946512892E-15 ) ) ;
#20208 = ADVANCED_FACE ( 'NONE', ( #46270 ), #4397, .T. ) ;
#20209 = AXIS2_PLACEMENT_3D ( 'NONE', #36160, #11243, #41477 ) ;
#20210 = VECTOR ( 'NONE', #45394, 1000.000000000000000 ) ;
#20211 = VERTEX_POINT ( 'NONE', #14992 ) ;
#20212 = CIRCLE ( 'NONE', #13827, 5.000000000000001776 ) ;
#20213 = DIRECTION ( 'NONE',  ( 1.000000000000000000, 0.000000000000000000, 0.000000000000000000 ) ) ;
#20214 = EDGE_CURVE ( 'NONE', #20076, #42325, #5655, .T. ) ;
#20215 = ORIENTED_EDGE ( 'NONE', *, *, #48446, .F. ) ;
#20216 = CARTESIAN_POINT ( 'NONE',  ( 47.00000000000000711, 4.705694406421931860E-17, -3.469127814946512892E-15 ) ) ;
#20217 = CARTESIAN_POINT ( 'NONE',  ( -29.68541646480307250, -1.416020129149132334, 11.91616074890920451 ) ) ;
#20218 = DIRECTION ( 'NONE',  ( -1.000000000000000000, 0.000000000000000000, -0.000000000000000000 ) ) ;
#20219 = CARTESIAN_POINT ( 'NONE',  ( 2.844750968615706199, -7.767336242080769004, -1.031816958530684891 ) ) ;
#20220 = CARTESIAN_POINT ( 'NONE',  ( 2.241317068080789898, 2.524952427345916739, -7.204761327832042817 ) ) ;
#20221 = ORIENTED_EDGE ( 'NONE', *, *, #37159, .T. ) ;
#20222 = DIRECTION ( 'NONE',  ( 0.2235469969004301449, -0.9746931518056330956, 0.000000000000000000 ) ) ;
#20223 = DIRECTION ( 'NONE',  ( -1.000000000000000000, 0.000000000000000000, 0.000000000000000000 ) ) ;
#20224 = DIRECTION ( 'NONE',  ( 1.000000000000000000, 0.000000000000000000, -0.000000000000000000 ) ) ;
#20225 = CARTESIAN_POINT ( 'NONE',  ( 2.241537034860906275, -6.609284473755313805, -3.821322318518443506 ) ) ;
#20226 = VECTOR ( 'NONE', #57432, 1000.000000000000000 ) ;
#20227 = CYLINDRICAL_SURFACE ( 'NONE', #63819, 5.000000000000000888 ) ;
#20228 = LINE ( 'NONE', #10246, #11704 ) ;
#20229 = ORIENTED_EDGE ( 'NONE', *, *, #10667, .T. ) ;
#20230 = CARTESIAN_POINT ( 'NONE',  ( -37.00000000000000711, 0.000000000000000000, 0.000000000000000000 ) ) ;
#20231 = ORIENTED_EDGE ( 'NONE', *, *, #10514, .F. ) ;
#20232 = CARTESIAN_POINT ( 'NONE',  ( 0.2717059086739043727, -0.1760722388997017218, -12.24704971877459592 ) ) ;
#20233 = CARTESIAN_POINT ( 'NONE',  ( -27.35552965826136429, -2.810569013793742688, 1.320216934008381804 ) ) ;
#20234 = AXIS2_PLACEMENT_3D ( 'NONE', #1571, #21845, #48101 ) ;
#20235 = CARTESIAN_POINT ( 'NONE',  ( 0.2648978790185584908, 7.769924372105204036, 9.465406350830633642 ) ) ;
#20236 = DIRECTION ( 'NONE',  ( 1.000000000000000000, -0.000000000000000000, 0.000000000000000000 ) ) ;
#20237 = ORIENTED_EDGE ( 'NONE', *, *, #29753, .T. ) ;
#20238 = ORIENTED_EDGE ( 'NONE', *, *, #64750, .T. ) ;
#20239 = CYLINDRICAL_SURFACE ( 'NONE', #54180, 5.000000000000000888 ) ;
#20240 = ORIENTED_EDGE ( 'NONE', *, *, #65210, .F. ) ;
#20241 = ADVANCED_FACE ( 'NONE', ( #24665 ), #51263, .T. ) ;
#20242 = CARTESIAN_POINT ( 'NONE',  ( 2.261269890822070749, -6.546486799463086648, -3.940687015735715892 ) ) ;
#20243 = CARTESIAN_POINT ( 'NONE',  ( -35.00000000000000000, -11.99999999999998579, 0.000000000000000000 ) ) ;
#20244 = CARTESIAN_POINT ( 'NONE',  ( -22.27720412283625961, -3.493592264983218953, -1.161733799004182721 ) ) ;
#20245 = CARTESIAN_POINT ( 'NONE',  ( 1.719304012338199517, 0.000000000000000000, 0.000000000000000000 ) ) ;
#20246 = CARTESIAN_POINT ( 'NONE',  ( 2.827825597296806492, -4.975864478227457255, 7.528560921609606993 ) ) ;
#20247 = DIRECTION ( 'NONE',  ( 0.000000000000000000, -0.01356324068817992522, 0.9999080150203990547 ) ) ;
#20248 = CARTESIAN_POINT ( 'NONE',  ( -18.22624239770570753, -11.73180942638131086, 2.608750867700459608 ) ) ;
#20249 = ORIENTED_EDGE ( 'NONE', *, *, #5941, .T. ) ;
#20250 = AXIS2_PLACEMENT_3D ( 'NONE', #64640, #3522, #53721 ) ;
#20251 = CARTESIAN_POINT ( 'NONE',  ( 2.573738926104379043, -2.426778239006406324, -7.355212866432320418 ) ) ;
#20252 = ORIENTED_EDGE ( 'NONE', *, *, #28831, .F. ) ;
#20253 = CARTESIAN_POINT ( 'NONE',  ( 1.719304012341273280, -2.961219984259375160, -12.38166659046469675 ) ) ;
#20255 = CARTESIAN_POINT ( 'NONE',  ( -37.00000000000000711, 0.000000000000000000, 0.000000000000000000 ) ) ;
#20254 = AXIS2_PLACEMENT_3D ( 'NONE', #59996, #24085, #38387 ) ;
#20256 = AXIS2_PLACEMENT_3D ( 'NONE', #59170, #13584, #39846 ) ;
#20257 = EDGE_CURVE ( 'NONE', #22753, #28214, #32075, .T. ) ;
#20258 = VECTOR ( 'NONE', #52734, 1000.000000000000000 ) ;
#20259 = ORIENTED_EDGE ( 'NONE', *, *, #60598, .F. ) ;
#20260 = DIRECTION ( 'NONE',  ( -1.000000000000000000, 0.000000000000000000, 0.000000000000000000 ) ) ;
#20261 = ORIENTED_EDGE ( 'NONE', *, *, #50911, .F. ) ;
#20262 = CARTESIAN_POINT ( 'NONE',  ( 36.00000000000000711, 6.711949091238144760, -10.84030624090609152 ) ) ;
#20263 = CARTESIAN_POINT ( 'NONE',  ( 6.806460418408726731, -6.060177178964488043, -12.06934091410146870 ) ) ;
#20264 = CIRCLE ( 'NONE', #36198, 2.899999999999995914 ) ;
#20265 = DIRECTION ( 'NONE',  ( 1.000000000000000000, 0.000000000000000000, -0.000000000000000000 ) ) ;
#20266 = CARTESIAN_POINT ( 'NONE',  ( 7.137024968749563492, -4.954338426407852047, 10.93925397463267757 ) ) ;
#20267 = VERTEX_POINT ( 'NONE', #14348 ) ;
#20268 = ORIENTED_EDGE ( 'NONE', *, *, #6262, .T. ) ;
#20269 = CARTESIAN_POINT ( 'NONE',  ( -10.00000000000000178, 0.000000000000000000, 0.000000000000000000 ) ) ;
#20270 = ORIENTED_EDGE ( 'NONE', *, *, #48461, .T. ) ;
#20271 = EDGE_CURVE ( 'NONE', #18208, #5331, #23667, .T. ) ;
#20272 = B_SPLINE_CURVE_WITH_KNOTS ( 'NONE', 3,
 ( #33937, #60196, #49274, #23987, #19962, #40230, #59549, #8351, #44247, #24293, #64518, #9008, #29291, #49586, #4025, #14620, #64840, #39589 ),
 .UNSPECIFIED., .F., .F.,
 ( 4, 2, 2, 2, 2, 2, 2, 2, 4 ),
 ( 0.000000000000000000, 0.0008755766307286345571, 0.001751153261457269114, 0.002626729892185903671, 0.003502306522914538228, 0.004377883153643172785, 0.005253459784371807342, 0.006129036415100441899, 0.007004613045829076456 ),
 .UNSPECIFIED. ) ;
#20273 = CARTESIAN_POINT ( 'NONE',  ( -37.00000000000000711, 0.000000000000000000, 0.000000000000000000 ) ) ;
#20274 = ORIENTED_EDGE ( 'NONE', *, *, #17636, .F. ) ;
#20275 = ORIENTED_EDGE ( 'NONE', *, *, #9811, .F. ) ;
#20276 = VERTEX_POINT ( 'NONE', #20666 ) ;
#20277 = CIRCLE ( 'NONE', #59580, 12.18649999999999878 ) ;
#20278 = CARTESIAN_POINT ( 'NONE',  ( -37.00000000000000711, -11.73463472867573643, -3.287724142101541958 ) ) ;
#20279 = CARTESIAN_POINT ( 'NONE',  ( 19.22959543997423992, -28.98134239863147599, 5.957279114860654978 ) ) ;
#20280 = VECTOR ( 'NONE', #60301, 1000.000000000000000 ) ;
#20281 = CARTESIAN_POINT ( 'NONE',  ( 25.00000000000000355, -30.00000000000000000, -4.999999999999999112 ) ) ;
#20282 = DIRECTION ( 'NONE',  ( 0.000000000000000000, 0.000000000000000000, 1.000000000000000000 ) ) ;
#20283 = DIRECTION ( 'NONE',  ( -1.000000000000000000, 0.000000000000000000, 0.000000000000000000 ) ) ;
#20284 = VERTEX_POINT ( 'NONE', #55590 ) ;
#20285 = AXIS2_PLACEMENT_3D ( 'NONE', #10637, #45914, #20646 ) ;
#20286 = CARTESIAN_POINT ( 'NONE',  ( 2.241352910868909643, -2.532612177304395029, -7.202080440908765979 ) ) ;
#20287 = AXIS2_PLACEMENT_3D ( 'NONE', #7226, #21212, #57140 ) ;
#20288 = VERTEX_POINT ( 'NONE', #5044 ) ;
#20289 = DIRECTION ( 'NONE',  ( 1.000000000000000000, 0.000000000000000000, 0.000000000000000000 ) ) ;
#20290 = CARTESIAN_POINT ( 'NONE',  ( -27.08850691366480490, 0.6228349286848202659, 2.218359546717751041 ) ) ;
#20291 = CIRCLE ( 'NONE', #51104, 4.999999999999999112 ) ;
#20292 = EDGE_LOOP ( 'NONE', ( #54, #3816, #20055, #44465 ) ) ;
#20293 = CARTESIAN_POINT ( 'NONE',  ( -27.74367520006269672, 12.26553276005925142, -5.646909315955152664 ) ) ;
#20294 = DIRECTION ( 'NONE',  ( 0.000000000000000000, 0.000000000000000000, 1.000000000000000000 ) ) ;
#20295 = CARTESIAN_POINT ( 'NONE',  ( 22.00000000000000711, -20.00000000000000000, 2.449293598294706907E-15 ) ) ;
#20296 = ORIENTED_EDGE ( 'NONE', *, *, #5905, .T. ) ;
#20297 = DIRECTION ( 'NONE',  ( -1.000000000000000000, 0.000000000000000000, 0.000000000000000000 ) ) ;
#20298 = CIRCLE ( 'NONE', #48991, 5.000000000000000000 ) ;
#20299 = VERTEX_POINT ( 'NONE', #20322 ) ;
#20300 = CARTESIAN_POINT ( 'NONE',  ( -40.42380607987477958, -25.46069350086627381, -4.500000000000000888 ) ) ;
#20301 = CARTESIAN_POINT ( 'NONE',  ( -18.63139410836038934, -13.49999999999999645, -0.3569054240395071464 ) ) ;
#20302 = CARTESIAN_POINT ( 'NONE',  ( 2.440552418640497212, 6.765628357760830269, -3.678171968408256998 ) ) ;
#20303 = CARTESIAN_POINT ( 'NONE',  ( 2.284126774967170537, -3.686252397487239651, -6.701756155761708911 ) ) ;
#20304 = CARTESIAN_POINT ( 'NONE',  ( 2.305787727787084407, 2.774453000917148415, 7.135468203929992370 ) ) ;
#20305 = ORIENTED_EDGE ( 'NONE', *, *, #8531, .T. ) ;
#20306 = CARTESIAN_POINT ( 'NONE',  ( 35.00000000000000000, 10.23119532541072552, -7.608228585767763619 ) ) ;
#20307 = DIRECTION ( 'NONE',  ( -0.000000000000000000, -0.000000000000000000, -1.000000000000000000 ) ) ;
#20308 = CARTESIAN_POINT ( 'NONE',  ( 37.00000000000000711, 11.72195762423409704, 0.7536123767498881243 ) ) ;
#20309 = FACE_OUTER_BOUND ( 'NONE', #45222, .T. ) ;
#20310 = EDGE_CURVE ( 'NONE', #47259, #32332, #21522, .T. ) ;
#20311 = CARTESIAN_POINT ( 'NONE',  ( -2.024814117303749494, -26.59886070765378818, -16.15701038285739699 ) ) ;
#20312 = DIRECTION ( 'NONE',  ( -1.000000000000000000, -0.000000000000000000, 0.000000000000000000 ) ) ;
#20313 = CARTESIAN_POINT ( 'NONE',  ( 0.2648978790185593790, -2.256510822326224464, 12.03635331166811540 ) ) ;
#20314 = CARTESIAN_POINT ( 'NONE',  ( -35.00000000000000000, 0.000000000000000000, 0.000000000000000000 ) ) ;
#20315 = CYLINDRICAL_SURFACE ( 'NONE', #61988, 12.18649999999999878 ) ;
#20316 = VECTOR ( 'NONE', #20771, 1000.000000000000000 ) ;
#20317 = EDGE_CURVE ( 'NONE', #50474, #35130, #10337, .T. ) ;
#20318 = ORIENTED_EDGE ( 'NONE', *, *, #39277, .F. ) ;
#20319 = VECTOR ( 'NONE', #31193, 1000.000000000000000 ) ;
#20321 = EDGE_LOOP ( 'NONE', ( #14844, #63255, #56084, #30681 ) ) ;
#20320 = EDGE_CURVE ( 'NONE', #12415, #59008, #390, .T. ) ;
#20322 = CARTESIAN_POINT ( 'NONE',  ( 2.305787727787084407, -5.047606869483016290, -5.756228004061508585 ) ) ;
#20323 = CARTESIAN_POINT ( 'NONE',  ( 37.00000000000000711, 4.237174932027401475, 12.02534193257715600 ) ) ;
#20324 = DIRECTION ( 'NONE',  ( 0.000000000000000000, -0.8696919319575238116, -0.4935949184179166949 ) ) ;
#20325 = CARTESIAN_POINT ( 'NONE',  ( 2.276198483118644145, -1.175725118477902287, -7.555081843355313076 ) ) ;
#20326 = ADVANCED_FACE ( 'NONE', ( #34622 ), #62511, .F. ) ;
#20327 = ORIENTED_EDGE ( 'NONE', *, *, #33201, .F. ) ;
#20328 = ORIENTED_EDGE ( 'NONE', *, *, #53812, .T. ) ;
#20329 = ORIENTED_EDGE ( 'NONE', *, *, #57427, .F. ) ;
#20330 = CARTESIAN_POINT ( 'NONE',  ( 2.305787727787084407, 2.774453000917245671, -7.135468203929955067 ) ) ;
#20331 = DIRECTION ( 'NONE',  ( 1.000000000000000000, 0.000000000000000000, 0.000000000000000000 ) ) ;
#20332 = EDGE_CURVE ( 'NONE', #44597, #28690, #49162, .T. ) ;
#20333 = EDGE_LOOP ( 'NONE', ( #55533, #1882, #50564, #43070 ) ) ;
#20334 = DIRECTION ( 'NONE',  ( -1.000000000000000000, -1.836970198721029688E-16, 0.000000000000000000 ) ) ;
#20335 = CIRCLE ( 'NONE', #36233, 4.999999999999998224 ) ;
#20336 = CARTESIAN_POINT ( 'NONE',  ( 2.844750968615921582, -2.364925124214038998, 7.470159816919260010 ) ) ;
#20337 = VERTEX_POINT ( 'NONE', #1373 ) ;
#20338 = CARTESIAN_POINT ( 'NONE',  ( -27.08429572838383947, -0.2296550094122856711, -2.279961732801603080 ) ) ;
#20340 = EDGE_CURVE ( 'NONE', #48418, #16579, #24743, .T. ) ;
#20339 = B_SPLINE_CURVE_WITH_KNOTS ( 'NONE', 3,
 ( #51185, #46193, #50527, #4970, #25233, #15257, #5636, #30863, #56483, #65456, #19612, #20242, #60818, #25905, #35537, #20896, #10929, #24920, #29890 ),
 .UNSPECIFIED., .F., .F.,
 ( 4, 3, 3, 3, 3, 3, 4 ),
 ( 0.000000000000000000, 2.831840207499450679E-05, 4.217266859840506987E-05, 5.602024318395848712E-05, 6.290810167968935505E-05, 9.120440630944629608E-05, 0.0001153103026479747480 ),
 .UNSPECIFIED. ) ;
#20341 = CARTESIAN_POINT ( 'NONE',  ( -4.536586326000698222, -28.39263410566653789, -13.35746355085865211 ) ) ;
#20342 = CARTESIAN_POINT ( 'NONE',  ( 35.00000000000000000, -12.08151691381186943, 4.074242145636128853 ) ) ;
#20343 = VERTEX_POINT ( 'NONE', #62197 ) ;
#20344 = AXIS2_PLACEMENT_3D ( 'NONE', #26585, #40908, #46236 ) ;
#20345 = DIRECTION ( 'NONE',  ( 0.000000000000000000, -0.01356324068817998767, 0.9999080150203990547 ) ) ;
#20346 = ORIENTED_EDGE ( 'NONE', *, *, #269, .T. ) ;
#20347 = CARTESIAN_POINT ( 'NONE',  ( 0.3675815128205894289, -6.367184624550092487, -10.50067073900658521 ) ) ;
#20348 = B_SPLINE_CURVE_WITH_KNOTS ( 'NONE', 3,
 ( #12203, #2243, #17202, #7891, #12856, #18191, #58774, #37806, #33139, #18539, #3229, #43109 ),
 .UNSPECIFIED., .F., .F.,
 ( 4, 2, 2, 2, 2, 4 ),
 ( 0.006679463946646270120, 0.007945415845128882618, 0.008578391794370190601, 0.009211367743611496850, 0.01047731964209411108, 0.01174327154057672531 ),
 .UNSPECIFIED. ) ;
#20349 = ORIENTED_EDGE ( 'NONE', *, *, #39590, .F. ) ;
#20350 = DIRECTION ( 'NONE',  ( 0.000000000000000000, -0.01356324068817992175, 0.9999080150203990547 ) ) ;
#20351 = CARTESIAN_POINT ( 'NONE',  ( 13.38593951179966623, -10.48414865564773635, -5.855826257454635808 ) ) ;
#20352 = CARTESIAN_POINT ( 'NONE',  ( -35.00000000000000000, -10.32377448871672598, 6.475373545682264975 ) ) ;
#20353 = CARTESIAN_POINT ( 'NONE',  ( 2.241352910868909643, -1.407733736974916772, 7.503490710578227585 ) ) ;
#20354 = LINE ( 'NONE', #20996, #53825 ) ;
#20355 = AXIS2_PLACEMENT_3D ( 'NONE', #52066, #226, #16158 ) ;
#20356 = CIRCLE ( 'NONE', #29941, 7.499999999999988454 ) ;
#20358 = AXIS2_PLACEMENT_3D ( 'NONE', #29390, #9760, #50359 ) ;
#20357 = CARTESIAN_POINT ( 'NONE',  ( -30.18541646480307250, -1.416020129149132112, 11.91616074890920096 ) ) ;
#20359 = CARTESIAN_POINT ( 'NONE',  ( -37.00000000000000711, 10.30098186818257666, -5.644643009978957515 ) ) ;
#20360 = CARTESIAN_POINT ( 'NONE',  ( 35.00000000000000000, -11.13736569743270621, 4.946702696913284569 ) ) ;
#20361 = CARTESIAN_POINT ( 'NONE',  ( 2.990245332647579524, -3.377079998295319907, 7.779904630197314930 ) ) ;
#20363 = ORIENTED_EDGE ( 'NONE', *, *, #60284, .F. ) ;
#20362 = CARTESIAN_POINT ( 'NONE',  ( 7.119412768985514894, -4.899345716645643556, 12.58666189623589382 ) ) ;
#20364 = ADVANCED_FACE ( 'NONE', ( #16331 ), #31601, .T. ) ;
#20365 = DIRECTION ( 'NONE',  ( -1.000000000000000000, -0.000000000000000000, -0.000000000000000000 ) ) ;
#20366 = ORIENTED_EDGE ( 'NONE', *, *, #53754, .F. ) ;
#20367 = DIRECTION ( 'NONE',  ( -1.000000000000000000, 0.000000000000000000, 0.000000000000000000 ) ) ;
#20368 = ORIENTED_EDGE ( 'NONE', *, *, #4307, .F. ) ;
#20369 = CYLINDRICAL_SURFACE ( 'NONE', #32267, 4.999999999999999112 ) ;
#20370 = ORIENTED_EDGE ( 'NONE', *, *, #38834, .F. ) ;
#20371 = CARTESIAN_POINT ( 'NONE',  ( 0.2872850955227739256, 8.035297825011367578, 9.251080475901380495 ) ) ;
#20372 = CARTESIAN_POINT ( 'NONE',  ( 35.00000000000000000, 6.547236723514018308, -9.752226076388918585 ) ) ;
#20373 = DIRECTION ( 'NONE',  ( 1.000000000000000000, 0.000000000000000000, 0.000000000000000000 ) ) ;
#20375 = CIRCLE ( 'NONE', #28866, 12.18649999999999878 ) ;
#20374 = LINE ( 'NONE', #40655, #13593 ) ;
#20376 = CIRCLE ( 'NONE', #57554, 5.000000000000000888 ) ;
#20377 = CARTESIAN_POINT ( 'NONE',  ( 3.618261583105321755, 8.318251859915347879, -10.63289868894575285 ) ) ;
#20378 = VERTEX_POINT ( 'NONE', #62850 ) ;
#20379 = DIRECTION ( 'NONE',  ( -0.4327406564646559262, 0.9015184547431841500, 0.000000000000000000 ) ) ;
#20380 = CIRCLE ( 'NONE', #54377, 5.000000000000000000 ) ;
#20381 = ORIENTED_EDGE ( 'NONE', *, *, #2130, .T. ) ;
#20382 = CARTESIAN_POINT ( 'NONE',  ( 2.430348790456773767, 0.1949172018038413667, 7.694949746373610289 ) ) ;
#20383 = CIRCLE ( 'NONE', #51210, 7.499999999999988454 ) ;
#20384 = FACE_OUTER_BOUND ( 'NONE', #48509, .T. ) ;
#20385 = CARTESIAN_POINT ( 'NONE',  ( -2.682146249266190718, 4.811221336669198045, 10.99569137319423007 ) ) ;
#20386 = ORIENTED_EDGE ( 'NONE', *, *, #25476, .T. ) ;
#20387 = AXIS2_PLACEMENT_3D ( 'NONE', #2892, #23151, #63693 ) ;
#20388 = DIRECTION ( 'NONE',  ( 0.000000000000000000, 0.000000000000000000, 1.000000000000000000 ) ) ;
#20389 = EDGE_CURVE ( 'NONE', #42450, #43097, #33238, .T. ) ;
#20390 = AXIS2_PLACEMENT_3D ( 'NONE', #36402, #42034, #2135 ) ;
#20391 =( BOUNDED_CURVE ( )  B_SPLINE_CURVE ( 3, ( #39491, #59788, #54806, #7954 ),
 .UNSPECIFIED., .F., .F. ) 
 B_SPLINE_CURVE_WITH_KNOTS ( ( 4, 4 ),
 ( 5.030260039792340265, 5.070137490277369707 ),
 .UNSPECIFIED. ) 
 CURVE ( )  GEOMETRIC_REPRESENTATION_ITEM ( )  RATIONAL_B_SPLINE_CURVE ( ( 1.000000000000000000, 0.9998674868020707152, 0.9998674868020707152, 1.000000000000000000 ) ) 
 REPRESENTATION_ITEM ( '' )  );
#20392 = CARTESIAN_POINT ( 'NONE',  ( 49.84017496522046287, -0.03257330535492963808, 2.852477068595666854 ) ) ;
#20393 = CARTESIAN_POINT ( 'NONE',  ( -6.985495616976492350, -1.802010734008522741, 13.38029624267572082 ) ) ;
#20394 = CARTESIAN_POINT ( 'NONE',  ( -25.00000000000000355, -3.797884998337192286, -24.99999999999999289 ) ) ;
#20395 = ORIENTED_EDGE ( 'NONE', *, *, #47287, .F. ) ;
#20396 = CARTESIAN_POINT ( 'NONE',  ( 0.2653519789438741339, 2.104833950422741129, -12.06397564829375568 ) ) ;
#20397 = CARTESIAN_POINT ( 'NONE',  ( -35.00000000000000000, 6.265926637539494415, 11.10408318471061584 ) ) ;
#20398 = CARTESIAN_POINT ( 'NONE',  ( 2.034671305879974135, -11.65517003033971122, -0.7032348381693538375 ) ) ;
#20399 = AXIS2_PLACEMENT_3D ( 'NONE', #52076, #6525, #47100 ) ;
#20400 = AXIS2_PLACEMENT_3D ( 'NONE', #64744, #31164, #45797 ) ;
#20401 = AXIS2_PLACEMENT_3D ( 'NONE', #45814, #44486, #45160 ) ;
#20402 = EDGE_CURVE ( 'NONE', #51541, #3030, #13620, .T. ) ;
#20403 = CARTESIAN_POINT ( 'NONE',  ( 2.000000000000001776, 1.145812388885215194, -6.715725538143608730 ) ) ;
#20404 = CARTESIAN_POINT ( 'NONE',  ( 5.515539859299206427, 0.0008592514567754854947, 0.005991790098943841278 ) ) ;
#20405 = VERTEX_POINT ( 'NONE', #2360 ) ;
#20406 = EDGE_CURVE ( 'NONE', #56858, #53890, #15150, .T. ) ;
#20407 = DIRECTION ( 'NONE',  ( 0.000000000000000000, -0.01356324068817998940, 0.9999080150203990547 ) ) ;
#20408 = CARTESIAN_POINT ( 'NONE',  ( -1.734723475976807094E-15, -3.469446951953614189E-15, -11.99999999999998934 ) ) ;
#20409 = CARTESIAN_POINT ( 'NONE',  ( -22.29195009621226831, 3.580440466953064949, -1.030739959031443886 ) ) ;
#20410 = ORIENTED_EDGE ( 'NONE', *, *, #56976, .F. ) ;
#20411 = FACE_OUTER_BOUND ( 'NONE', #63646, .T. ) ;
#20412 = CARTESIAN_POINT ( 'NONE',  ( 2.241536586108913820, 6.614789707676462349, 3.811784405792373764 ) ) ;
#20413 = EDGE_CURVE ( 'NONE', #11115, #24280, #8117, .T. ) ;
#20414 = ORIENTED_EDGE ( 'NONE', *, *, #60444, .F. ) ;
#20415 = ORIENTED_EDGE ( 'NONE', *, *, #48537, .F. ) ;
#20416 = ORIENTED_EDGE ( 'NONE', *, *, #39526, .F. ) ;
#20417 = AXIS2_PLACEMENT_3D ( 'NONE', #50459, #25487, #15505 ) ;
#20418 = EDGE_CURVE ( 'NONE', #51873, #65690, #47566, .T. ) ;
#20419 = ORIENTED_EDGE ( 'NONE', *, *, #35390, .T. ) ;
#20420 = CYLINDRICAL_SURFACE ( 'NONE', #25968, 12.74999999999999822 ) ;
#20421 = DIRECTION ( 'NONE',  ( 0.000000000000000000, -0.6051742151937556935, -0.7960930657056508597 ) ) ;
#20422 = LINE ( 'NONE', #40702, #32231 ) ;
#20423 = CARTESIAN_POINT ( 'NONE',  ( 8.937200413559443390, 4.476360154859203355, 11.13383131558893346 ) ) ;
#20424 = CIRCLE ( 'NONE', #63988, 12.18649999999999878 ) ;
#20425 = DIRECTION ( 'NONE',  ( 0.000000000000000000, 0.9718671068226450993, -0.2355298848897551256 ) ) ;
#20426 = EDGE_CURVE ( 'NONE', #59359, #54096, #33421, .T. ) ;
#20427 = CIRCLE ( 'NONE', #28928, 5.000000000000000000 ) ;
#20428 = CARTESIAN_POINT ( 'NONE',  ( -7.016966734453155219, -28.45964332336963665, 10.94381053768247547 ) ) ;
#20429 = CARTESIAN_POINT ( 'NONE',  ( -17.54726996257253191, 11.36053454945672847, 3.865003848717349033 ) ) ;
#20431 = ORIENTED_EDGE ( 'NONE', *, *, #63899, .F. ) ;
#20430 = CARTESIAN_POINT ( 'NONE',  ( -35.00000000000000000, -11.66953048682402283, 3.511814412392074480 ) ) ;
#20432 = CARTESIAN_POINT ( 'NONE',  ( -35.00000000000000000, -5.130401251914653571, -11.05394794832835359 ) ) ;
#20433 = ADVANCED_FACE ( 'NONE', ( #17647 ), #8970, .T. ) ;
#20434 = EDGE_LOOP ( 'NONE', ( #50785, #5128, #64150, #44966 ) ) ;
#20435 = DIRECTION ( 'NONE',  ( 0.000000000000000000, 0.01356324068817992175, -0.9999080150203990547 ) ) ;
#20436 = ORIENTED_EDGE ( 'NONE', *, *, #26646, .F. ) ;
#20437 = VERTEX_POINT ( 'NONE', #27945 ) ;
#20438 = DIRECTION ( 'NONE',  ( -1.000000000000000000, 0.000000000000000000, 0.000000000000000000 ) ) ;
#20439 = EDGE_CURVE ( 'NONE', #47144, #55517, #37909, .T. ) ;
#20440 = CARTESIAN_POINT ( 'NONE',  ( 14.27815883903102900, -30.09651741059085595, 4.806648824293995759 ) ) ;
#20441 = DIRECTION ( 'NONE',  ( 0.000000000000000000, 0.01356324068817998940, -0.9999080150203990547 ) ) ;
#20442 = DIRECTION ( 'NONE',  ( 0.2475719085175094591, 6.192417051524157726E-18, -0.9688695217174487784 ) ) ;
#20443 = CARTESIAN_POINT ( 'NONE',  ( 1.287602823385630479, -2.727479899220070170, 12.28793447239686287 ) ) ;
#20444 = CARTESIAN_POINT ( 'NONE',  ( 0.3057689695767489280, -12.03117299329037593, 2.355923806019164957 ) ) ;
#20446 = VERTEX_POINT ( 'NONE', #3348 ) ;
#20445 = EDGE_CURVE ( 'NONE', #21752, #14146, #12624, .T. ) ;
#20447 = VECTOR ( 'NONE', #24879, 1000.000000000000000 ) ;
#20448 = ORIENTED_EDGE ( 'NONE', *, *, #57584, .T. ) ;
#20449 = DIRECTION ( 'NONE',  ( 1.000000000000000000, -0.000000000000000000, 0.000000000000000000 ) ) ;
#20450 = ORIENTED_EDGE ( 'NONE', *, *, #39872, .F. ) ;
#20451 = EDGE_CURVE ( 'NONE', #45693, #45313, #39775, .T. ) ;
#20452 = EDGE_LOOP ( 'NONE', ( #9080, #44546, #41098, #25730 ) ) ;
#20454 = AXIS2_PLACEMENT_3D ( 'NONE', #23959, #38583, #44874 ) ;
#20453 = CARTESIAN_POINT ( 'NONE',  ( -36.00000000000000711, 0.3137578094509230753, 12.74613886779085270 ) ) ;
#20455 = LINE ( 'NONE', #64122, #54358 ) ;
#20456 = CARTESIAN_POINT ( 'NONE',  ( 34.00000000000000000, 1.267509437117510519E-14, 0.000000000000000000 ) ) ;
#20457 = B_SPLINE_CURVE_WITH_KNOTS ( 'NONE', 3,
 ( #42006, #32026, #17066, #52345, #12393, #7409 ),
 .UNSPECIFIED., .F., .F.,
 ( 4, 2, 4 ),
 ( 0.0002637379172192473305, 0.0009975831966643154951, 0.001731428476109383822 ),
 .UNSPECIFIED. ) ;
#20458 = CARTESIAN_POINT ( 'NONE',  ( 0.8320506296491581022, -12.17395768195217975, 2.535206712041412569 ) ) ;
#20459 = CARTESIAN_POINT ( 'NONE',  ( 2.000000000000001776, 3.230174184210159893, -5.998318953995314118 ) ) ;
#20460 = CARTESIAN_POINT ( 'NONE',  ( -37.00000000000000711, 0.000000000000000000, 0.000000000000000000 ) ) ;
#20461 = AXIS2_PLACEMENT_3D ( 'NONE', #37980, #17048, #58283 ) ;
#20462 = ORIENTED_EDGE ( 'NONE', *, *, #61756, .T. ) ;
#20463 = VERTEX_POINT ( 'NONE', #23277 ) ;
#20464 = CARTESIAN_POINT ( 'NONE',  ( -37.00000000000000711, 0.000000000000000000, 0.000000000000000000 ) ) ;
#20465 = CARTESIAN_POINT ( 'NONE',  ( 2.251152103363643242, 7.498874008626774668, -1.449454666117645507 ) ) ;
#20466 = AXIS2_PLACEMENT_3D ( 'NONE', #56033, #26430, #65665 ) ;
#20467 = CARTESIAN_POINT ( 'NONE',  ( 2.000000000000001776, 6.935703035393448346, -0.1051458740707923722 ) ) ;
#20468 = CIRCLE ( 'NONE', #62939, 5.000000000000000000 ) ;
#20469 = ADVANCED_FACE ( 'NONE', ( #18307 ), #7662, .T. ) ;
#20470 = CARTESIAN_POINT ( 'NONE',  ( 4.631701379227551207, -10.10996076783195008, 6.470577568759368070 ) ) ;
#20471 = DIRECTION ( 'NONE',  ( -1.000000000000000000, 0.000000000000000000, 0.000000000000000000 ) ) ;
#20472 = DIRECTION ( 'NONE',  ( -1.000000000000000000, 0.000000000000000000, -0.000000000000000000 ) ) ;
#20473 = CARTESIAN_POINT ( 'NONE',  ( 2.102182802109547666, 1.287158751533839629, -11.93215772323105561 ) ) ;
#20474 = VECTOR ( 'NONE', #25684, 1000.000000000000000 ) ;
#20475 = LINE ( 'NONE', #55389, #12927 ) ;
#20476 = ORIENTED_EDGE ( 'NONE', *, *, #34591, .F. ) ;
#20477 = APPLICATION_CONTEXT ( 'automotive_design' ) ;
#20478 = CYLINDRICAL_SURFACE ( 'NONE', #59015, 4.999999999999999112 ) ;
#20479 = DIRECTION ( 'NONE',  ( -1.000000000000000000, 0.000000000000000000, 0.000000000000000000 ) ) ;
#20480 = EDGE_CURVE ( 'NONE', #36604, #22476, #49231, .T. ) ;
#20481 = CARTESIAN_POINT ( 'NONE',  ( 47.00000000000000711, 4.705694406421931860E-17, -3.469127814946512892E-15 ) ) ;
#20482 = EDGE_CURVE ( 'NONE', #27103, #5815, #23950, .T. ) ;
#20483 = CARTESIAN_POINT ( 'NONE',  ( -7.228961821833054024, -32.07041743672399292, -13.19626196499568316 ) ) ;
#20484 = DIRECTION ( 'NONE',  ( 1.000000000000000000, 0.000000000000000000, -0.000000000000000000 ) ) ;
#20485 = ORIENTED_EDGE ( 'NONE', *, *, #56058, .T. ) ;
#20486 = CARTESIAN_POINT ( 'NONE',  ( 2.241528039335008327, 7.634443721858077403, 0.01573255094244493946 ) ) ;
#20487 = DIRECTION ( 'NONE',  ( 1.000000000000000000, 0.000000000000000000, 0.000000000000000000 ) ) ;
#20488 = CARTESIAN_POINT ( 'NONE',  ( 12.19204271345157586, -29.31683997938284136, -5.830637565203153905 ) ) ;
#20489 = VERTEX_POINT ( 'NONE', #33900 ) ;
#20490 = CARTESIAN_POINT ( 'NONE',  ( -36.00000000000000711, -12.49688848680886011, 2.527899948230591942 ) ) ;
#20491 = CARTESIAN_POINT ( 'NONE',  ( -14.51259464223477735, 7.865023325494275852, -9.063844199178094030 ) ) ;
#20492 = CARTESIAN_POINT ( 'NONE',  ( -22.27706089016750113, -0.9256273512588407693, -3.562910635974996243 ) ) ;
#20493 = EDGE_CURVE ( 'NONE', #22257, #43258, #35310, .T. ) ;
#20494 = VECTOR ( 'NONE', #15826, 1000.000000000000000 ) ;
#20496 = ORIENTED_EDGE ( 'NONE', *, *, #33081, .F. ) ;
#20495 = CARTESIAN_POINT ( 'NONE',  ( 3.100650473569713128, 0.9283202922945034130, 7.866294126167251655 ) ) ;
#20497 = FACE_OUTER_BOUND ( 'NONE', #47763, .T. ) ;
#20498 = VECTOR ( 'NONE', #34298, 1000.000000000000000 ) ;
#20499 = VECTOR ( 'NONE', #42150, 1000.000000000000000 ) ;
#20500 = CARTESIAN_POINT ( 'NONE',  ( 2.844750968615974873, -7.470159816919274220, -2.364925124214049212 ) ) ;
#20501 = ORIENTED_EDGE ( 'NONE', *, *, #53688, .T. ) ;
#20502 = CARTESIAN_POINT ( 'NONE',  ( 0.2851083653049504285, -0.4107471485392698018, -11.99296822225284131 ) ) ;
#20503 = DIRECTION ( 'NONE',  ( -1.000000000000000000, -0.000000000000000000, 0.000000000000000000 ) ) ;
#20504 = CARTESIAN_POINT ( 'NONE',  ( -17.65816380191525425, 7.464113067668815660, -11.25126181107559553 ) ) ;
#20505 = DIRECTION ( 'NONE',  ( 0.000000000000000000, -0.01356324068817998940, 0.9999080150203990547 ) ) ;
#20506 = LINE ( 'NONE', #15818, #11890 ) ;
#20507 = CIRCLE ( 'NONE', #22655, 5.000000000000000000 ) ;
#20508 = DIRECTION ( 'NONE',  ( 0.000000000000000000, 0.9796553971857735466, 0.2006870767258926436 ) ) ;
#20509 = CARTESIAN_POINT ( 'NONE',  ( 37.00000000000000711, -12.14284015767850455, -1.030638227056526413 ) ) ;
#20510 = VERTEX_POINT ( 'NONE', #3015 ) ;
#20511 = DIRECTION ( 'NONE',  ( 1.000000000000000000, 0.000000000000000000, 0.000000000000000000 ) ) ;
#20512 = AXIS2_PLACEMENT_3D ( 'NONE', #64776, #14255, #8952 ) ;
#20513 = ORIENTED_EDGE ( 'NONE', *, *, #30165, .T. ) ;
#20514 = DIRECTION ( 'NONE',  ( 1.000000000000000000, 0.000000000000000000, 0.000000000000000000 ) ) ;
#20515 = DIRECTION ( 'NONE',  ( 1.000000000000000000, 0.000000000000000000, 0.000000000000000000 ) ) ;
#20516 = EDGE_CURVE ( 'NONE', #31372, #13725, #58701, .T. ) ;
#20517 = AXIS2_PLACEMENT_3D ( 'NONE', #25159, #60738, #59761 ) ;
#20518 = CARTESIAN_POINT ( 'NONE',  ( 2.907497136251038228, 1.716624290781495699, 7.666666002096734545 ) ) ;
#20519 = EDGE_CURVE ( 'NONE', #36611, #62352, #25789, .T. ) ;
#20520 = CARTESIAN_POINT ( 'NONE',  ( 0.2646305136544072623, 4.312539723326286989, -11.46223899740595797 ) ) ;
#20521 = ORIENTED_EDGE ( 'NONE', *, *, #8060, .T. ) ;
#20522 = DIRECTION ( 'NONE',  ( -1.000000000000000000, 0.000000000000000000, 0.000000000000000000 ) ) ;
#20523 = CARTESIAN_POINT ( 'NONE',  ( 11.74548640120467979, 8.775604215601129354, -8.184666801472349817 ) ) ;
#20524 = CYLINDRICAL_SURFACE ( 'NONE', #54189, 11.99999999999999289 ) ;
#20525 = ORIENTED_EDGE ( 'NONE', *, *, #20847, .F. ) ;
#20526 = AXIS2_PLACEMENT_3D ( 'NONE', #56526, #10302, #15933 ) ;
#20527 = ORIENTED_EDGE ( 'NONE', *, *, #55500, .F. ) ;
#20528 = EDGE_CURVE ( 'NONE', #37925, #65184, #44912, .T. ) ;
#20529 = CARTESIAN_POINT ( 'NONE',  ( 35.00000000000000000, -6.018036132182079889, 11.24036214326526562 ) ) ;
#20530 = EDGE_LOOP ( 'NONE', ( #12564, #10257, #28164, #22682 ) ) ;
#20531 = CARTESIAN_POINT ( 'NONE',  ( 22.22762455518017433, -10.97323854681321897, -4.869946340165640208 ) ) ;
#20532 = CARTESIAN_POINT ( 'NONE',  ( -27.10719052120871098, -2.261993590776032459, 0.6736837626858792616 ) ) ;
#20533 = CARTESIAN_POINT ( 'NONE',  ( 5.516018279890452902, -0.002104829434641057422, -0.006440244342253404787 ) ) ;
#20534 = CARTESIAN_POINT ( 'NONE',  ( 2.269879328256731110, 7.130835954829884749, -2.753278809616039879 ) ) ;
#20535 = LINE ( 'NONE', #61095, #34085 ) ;
#20536 = DIRECTION ( 'NONE',  ( -0.000000000000000000, -1.000000000000000000, -0.000000000000000000 ) ) ;
#20537 = CIRCLE ( 'NONE', #26895, 2.899999999999995026 ) ;
#20538 = CARTESIAN_POINT ( 'NONE',  ( -35.00000000000000000, -7.745827850122939395, -10.12742074351904975 ) ) ;
#20539 = VERTEX_POINT ( 'NONE', #34228 ) ;
#20540 = CARTESIAN_POINT ( 'NONE',  ( 1.547277799337429594, 12.65564732076229681, -0.6737945300318757269 ) ) ;
#20541 = FACE_OUTER_BOUND ( 'NONE', #48572, .T. ) ;
#20542 = DIRECTION ( 'NONE',  ( 1.000000000000000000, 0.000000000000000000, 0.000000000000000000 ) ) ;
#20544 = DIRECTION ( 'NONE',  ( 1.000000000000000000, 0.000000000000000000, 0.000000000000000000 ) ) ;
#20543 = AXIS2_PLACEMENT_3D ( 'NONE', #52163, #6615, #13227 ) ;
#20545 = CARTESIAN_POINT ( 'NONE',  ( 35.00000000000000000, 6.584150480049550502, -10.25474254703955701 ) ) ;
#20546 = DIRECTION ( 'NONE',  ( -0.000000000000000000, -0.000000000000000000, -1.000000000000000000 ) ) ;
#20547 = CARTESIAN_POINT ( 'NONE',  ( -35.00000000000000000, 0.000000000000000000, 0.000000000000000000 ) ) ;
#20548 = AXIS2_PLACEMENT_3D ( 'NONE', #2807, #23388, #43656 ) ;
#20549 = DIRECTION ( 'NONE',  ( 0.000000000000000000, -0.5155538571770109657, -0.8568571761675956022 ) ) ;
#20550 = CIRCLE ( 'NONE', #57725, 5.000000000000000888 ) ;
#20551 = AXIS2_PLACEMENT_3D ( 'NONE', #39135, #58462, #48488 ) ;
#20552 = EDGE_CURVE ( 'NONE', #23557, #42938, #60813, .T. ) ;
#20553 = EDGE_LOOP ( 'NONE', ( #45351, #57503, #61757, #41261 ) ) ;
#20554 = CARTESIAN_POINT ( 'NONE',  ( 37.00000000000000711, 11.90598845858539967, 4.561791185930283099 ) ) ;
#20555 = EDGE_CURVE ( 'NONE', #53879, #29231, #30002, .T. ) ;
#20556 = ORIENTED_EDGE ( 'NONE', *, *, #32039, .T. ) ;
#20557 = CARTESIAN_POINT ( 'NONE',  ( -35.00000000000000000, -7.474872387600942858, -9.060822531526127932 ) ) ;
#20558 = LINE ( 'NONE', #21543, #24529 ) ;
#20559 = FACE_OUTER_BOUND ( 'NONE', #20967, .T. ) ;
#20560 = AXIS2_PLACEMENT_3D ( 'NONE', #13579, #29525, #33868 ) ;
#20561 = DIRECTION ( 'NONE',  ( -1.000000000000000000, -0.000000000000000000, -0.000000000000000000 ) ) ;
#20562 = CARTESIAN_POINT ( 'NONE',  ( 2.280717697723675386, 2.468022724683634372, -7.238333660706929074 ) ) ;
#20563 = ORIENTED_EDGE ( 'NONE', *, *, #12500, .F. ) ;
#20564 = CIRCLE ( 'NONE', #14135, 5.000000000000000888 ) ;
#20565 = DIRECTION ( 'NONE',  ( 0.000000000000000000, 0.2960891610144510966, 0.9551603052523478521 ) ) ;
#20566 = LINE ( 'NONE', #30209, #37384 ) ;
#20567 = EDGE_CURVE ( 'NONE', #48396, #10868, #55496, .T. ) ;
#20568 = CARTESIAN_POINT ( 'NONE',  ( 2.941278708680199916, 6.068329152486391820, -0.9331242451664371051 ) ) ;
#20569 = CARTESIAN_POINT ( 'NONE',  ( 2.241506898688418126, -6.631235260227141382, -3.783130304541498123 ) ) ;
#20570 = VECTOR ( 'NONE', #11108, 1000.000000000000000 ) ;
#20571 = CARTESIAN_POINT ( 'NONE',  ( -17.72572367302459639, -5.320256682235254608, 10.76019785545453722 ) ) ;
#20572 = CARTESIAN_POINT ( 'NONE',  ( 2.257661810676420355, 2.739276463085679403, 7.131864446283232795 ) ) ;
#20573 = AXIS2_PLACEMENT_3D ( 'NONE', #56675, #52339, #6780 ) ;
#20574 = ORIENTED_EDGE ( 'NONE', *, *, #56212, .F. ) ;
#20575 = VECTOR ( 'NONE', #10881, 1000.000000000000000 ) ;
#20576 = CARTESIAN_POINT ( 'NONE',  ( -37.00000000000000711, 10.32377448871677039, -6.475373545682194809 ) ) ;
#20577 = EDGE_LOOP ( 'NONE', ( #2544, #45392, #64805, #64566 ) ) ;
#20578 = CARTESIAN_POINT ( 'NONE',  ( 0.000000000000000000, -29.00000000000000000, 0.000000000000000000 ) ) ;
#20579 = CARTESIAN_POINT ( 'NONE',  ( 2.241536586108912932, 7.176205604390212045, 2.605228657247374180 ) ) ;
#20580 = EDGE_CURVE ( 'NONE', #15890, #52774, #19277, .T. ) ;
#20581 = CARTESIAN_POINT ( 'NONE',  ( -22.28506771379528573, -3.575989816848462510, 1.050362426369334079 ) ) ;
#20582 = ADVANCED_FACE ( 'NONE', ( #40524 ), #48958, .F. ) ;
#20583 = CARTESIAN_POINT ( 'NONE',  ( -9.606767908028034597, -3.747519102173751282, 11.40110431394993640 ) ) ;
#20584 = CIRCLE ( 'NONE', #30115, 12.75000000000000178 ) ;
#20585 = ORIENTED_EDGE ( 'NONE', *, *, #59834, .F. ) ;
#20586 = EDGE_LOOP ( 'NONE', ( #28194, #60247, #5458, #7411 ) ) ;
#20587 = DIRECTION ( 'NONE',  ( -0.000000000000000000, -0.000000000000000000, -1.000000000000000000 ) ) ;
#20588 = ORIENTED_EDGE ( 'NONE', *, *, #31364, .T. ) ;
#20589 = DIRECTION ( 'NONE',  ( -1.000000000000000000, 0.000000000000000000, -0.000000000000000000 ) ) ;
#20591 = DIRECTION ( 'NONE',  ( -1.000000000000000000, -1.836970198721029688E-16, -0.000000000000000000 ) ) ;
#20590 =( BOUNDED_SURFACE ( )  B_SPLINE_SURFACE ( 3, 1, ( 
 ( #37920, #17657 ),
 ( #63192, #58213 ),
 ( #32911, #4324 ),
 ( #39557, #64490 ) ),
 .UNSPECIFIED., .F., .F., .F. ) 
 B_SPLINE_SURFACE_WITH_KNOTS ( ( 4, 4 ),
 ( 2, 2 ),
 ( 0.000000000000000000, 1.000000000000000000 ),
 ( 0.000000000000000000, 1.000000000000000000 ),
 .UNSPECIFIED. ) 
 GEOMETRIC_REPRESENTATION_ITEM ( )  RATIONAL_B_SPLINE_SURFACE ( (
 ( 1.000000000000000000, 1.000000000000000000),
 ( 0.9856612449720755231, 0.9999558406602322425),
 ( 0.9856612449720755231, 0.9999558406602322425),
 ( 1.000000000000000000, 1.000000000000000000) ) ) 
 REPRESENTATION_ITEM ( '' )  SURFACE ( )  );
#20592 = CARTESIAN_POINT ( 'NONE',  ( 0.9232058338315048962, 10.60677148422244365, 6.559496812049697034 ) ) ;
#20593 = CARTESIAN_POINT ( 'NONE',  ( 2.655192694323794456, -8.807900729500619974, 3.822392723567597628 ) ) ;
#20594 = CARTESIAN_POINT ( 'NONE',  ( 1.547277799339725757, 9.261681528764395210, -8.651049845884754674 ) ) ;
#20595 = CARTESIAN_POINT ( 'NONE',  ( 5.515188684475870851, 0.005320786921497679470, 0.0005703990286340230751 ) ) ;
#20596 = DIRECTION ( 'NONE',  ( -1.000000000000000000, 0.000000000000000000, 0.000000000000000000 ) ) ;
#20597 = VERTEX_POINT ( 'NONE', #40867 ) ;
#20598 = CARTESIAN_POINT ( 'NONE',  ( 0.7446945582518260665, -10.91757157182789051, 5.891988114924179065 ) ) ;
#20599 = ORIENTED_EDGE ( 'NONE', *, *, #63233, .F. ) ;
#20600 = DIRECTION ( 'NONE',  ( -1.000000000000000000, 0.000000000000000000, 0.000000000000000000 ) ) ;
#20601 = EDGE_CURVE ( 'NONE', #30121, #22151, #56600, .T. ) ;
#20602 = CYLINDRICAL_SURFACE ( 'NONE', #43854, 5.000000000000000888 ) ;
#20603 = ORIENTED_EDGE ( 'NONE', *, *, #37954, .F. ) ;
#20604 = ADVANCED_FACE ( 'NONE', ( #4971 ), #5292, .T. ) ;
#20605 = CARTESIAN_POINT ( 'NONE',  ( -22.27719412087655471, 3.642699606241628807, -0.5341638063191783692 ) ) ;
#20606 = ORIENTED_EDGE ( 'NONE', *, *, #5156, .F. ) ;
#20607 = CARTESIAN_POINT ( 'NONE',  ( -28.85619398320021745, 3.750539801530000439, -11.39883551934754280 ) ) ;
#20608 = CARTESIAN_POINT ( 'NONE',  ( 6.742208325808031866, -7.058475617584183404, -11.51382290311167722 ) ) ;
#20609 = CYLINDRICAL_SURFACE ( 'NONE', #47782, 12.74999999999999822 ) ;
#20610 = CARTESIAN_POINT ( 'NONE',  ( -27.08850691366480490, -2.232573186527710529, -0.5697889027535691930 ) ) ;
#20611 = ORIENTED_EDGE ( 'NONE', *, *, #55988, .T. ) ;
#20612 = ORIENTED_EDGE ( 'NONE', *, *, #4458, .T. ) ;
#20613 = CARTESIAN_POINT ( 'NONE',  ( 2.507146904658097863, -6.793847219607473953, 3.672650549645643636 ) ) ;
#20614 = VERTEX_POINT ( 'NONE', #29892 ) ;
#20615 = CARTESIAN_POINT ( 'NONE',  ( 0.2706063244538062795, 11.56807224179758720, -4.023948952279145175 ) ) ;
#20616 = ORIENTED_EDGE ( 'NONE', *, *, #65306, .F. ) ;
#20617 = VECTOR ( 'NONE', #60374, 1000.000000000000000 ) ;
#20618 = ORIENTED_EDGE ( 'NONE', *, *, #8120, .T. ) ;
#20619 = B_SPLINE_CURVE_WITH_KNOTS ( 'NONE', 3,
 ( #46884, #684, #45903, #20941, #357, #10628, #20637, #30919, #36229, #16299, #40913, #21622, #6325, #1341, #31573, #6658 ),
 .UNSPECIFIED., .F., .F.,
 ( 4, 3, 3, 3, 3, 4 ),
 ( 0.000000000000000000, 0.0002999043160758303110, 0.0005998071753052896518, 0.0008997092107377380795, 0.001204458948196922069, 0.001510329163478790109 ),
 .UNSPECIFIED. ) ;
#20620 = ORIENTED_EDGE ( 'NONE', *, *, #60552, .T. ) ;
#20621 = CARTESIAN_POINT ( 'NONE',  ( 35.00000000000000000, -5.246972444133939817, 10.99909370905162298 ) ) ;
#20622 = AXIS2_PLACEMENT_3D ( 'NONE', #53145, #7591, #27877 ) ;
#20623 = CARTESIAN_POINT ( 'NONE',  ( -35.00000000000000000, 4.986700593229701717, 10.63508530065523772 ) ) ;
#20624 = CARTESIAN_POINT ( 'NONE',  ( 0.2655924914740778187, -4.229867354073634012, 11.49267051747967017 ) ) ;
#20625 = CYLINDRICAL_SURFACE ( 'NONE', #28735, 7.115568257478080305 ) ;
#20626 = CARTESIAN_POINT ( 'NONE',  ( 2.000000000000001776, -5.888698556700776798, 3.665823448873372747 ) ) ;
#20627 = VERTEX_POINT ( 'NONE', #30864 ) ;
#20628 = EDGE_CURVE ( 'NONE', #23325, #31648, #25235, .T. ) ;
#20629 = CARTESIAN_POINT ( 'NONE',  ( -29.68541646480313645, -1.416020129149148543, -11.91616074890925780 ) ) ;
#20630 = ORIENTED_EDGE ( 'NONE', *, *, #39710, .F. ) ;
#20631 = CARTESIAN_POINT ( 'NONE',  ( -16.98800322446194855, 2.922502605998049674, 13.17987020110344787 ) ) ;
#20632 = VECTOR ( 'NONE', #54924, 1000.000000000000000 ) ;
#20633 = CARTESIAN_POINT ( 'NONE',  ( -2.532614230583026593, 7.965877694534055031, 10.89930238848911337 ) ) ;
#20634 = DIRECTION ( 'NONE',  ( 1.000000000000000000, 0.000000000000000000, 0.000000000000000000 ) ) ;
#20635 = CARTESIAN_POINT ( 'NONE',  ( -27.74685410543621344, 12.59748157192950480, -4.861485140711778286 ) ) ;
#20636 = CARTESIAN_POINT ( 'NONE',  ( 1.452237505248552996, -9.303501428255968264, -8.579708443906842064 ) ) ;
#20637 = CARTESIAN_POINT ( 'NONE',  ( 1.198791140420903512, -10.60778679489422949, -6.720248575444034422 ) ) ;
#20638 = CIRCLE ( 'NONE', #57807, 12.18649999999999878 ) ;
#20639 = ORIENTED_EDGE ( 'NONE', *, *, #31984, .T. ) ;
#20640 = DIRECTION ( 'NONE',  ( 0.000000000000000000, -0.9999080150203989437, -0.01356324068819032662 ) ) ;
#20641 = EDGE_CURVE ( 'NONE', #19302, #52228, #39597, .T. ) ;
#20642 = ORIENTED_EDGE ( 'NONE', *, *, #21061, .F. ) ;
#20643 = PLANE ( 'NONE',  #3063 ) ;
#20644 =( NAMED_UNIT ( * ) PLANE_ANGLE_UNIT ( ) SI_UNIT ( $, .RADIAN. ) );
#20645 = CARTESIAN_POINT ( 'NONE',  ( 3.152665057734004073, 7.102135024645805039, -3.546019893116331811 ) ) ;
#20646 = DIRECTION ( 'NONE',  ( 0.000000000000000000, -0.01356324068817999114, 0.9999080150203989437 ) ) ;
#20647 = CARTESIAN_POINT ( 'NONE',  ( 2.889800649504073782, -0.9965440656174132661, 6.039722463373535355 ) ) ;
#20648 = ORIENTED_EDGE ( 'NONE', *, *, #26977, .F. ) ;
#20649 = CIRCLE ( 'NONE', #24909, 12.74999999999999822 ) ;
#20650 = CIRCLE ( 'NONE', #12128, 12.74999999999999822 ) ;
#20651 = LINE ( 'NONE', #10321, #19710 ) ;
#20652 = CARTESIAN_POINT ( 'NONE',  ( 35.00000000000000000, -12.02534193257717554, 4.237174932027349961 ) ) ;
#20653 = DIRECTION ( 'NONE',  ( 1.000000000000000000, 0.000000000000000000, 0.000000000000000000 ) ) ;
#20654 = DIRECTION ( 'NONE',  ( 0.000000000000000000, 0.000000000000000000, 1.000000000000000000 ) ) ;
#20655 = EDGE_CURVE ( 'NONE', #52583, #62889, #39875, .T. ) ;
#20656 = CARTESIAN_POINT ( 'NONE',  ( -21.17861794710831091, 13.00977982294135593, -3.604945070120774808 ) ) ;
#20657 = FACE_OUTER_BOUND ( 'NONE', #34691, .T. ) ;
#20659 = EDGE_CURVE ( 'NONE', #17610, #43228, #20468, .T. ) ;
#20658 = CARTESIAN_POINT ( 'NONE',  ( 2.259025283528082628, -5.939720477913319918, -4.805599953367722499 ) ) ;
#20660 = DIRECTION ( 'NONE',  ( 0.000000000000000000, 0.01356324068817991828, -0.9999080150203990547 ) ) ;
#20661 = CARTESIAN_POINT ( 'NONE',  ( -14.47334165536099881, 3.872983346207417021, 1.000000000000000000 ) ) ;
#20662 = VECTOR ( 'NONE', #53007, 1000.000000000000000 ) ;
#20663 = EDGE_CURVE ( 'NONE', #33180, #42715, #59845, .T. ) ;
#20664 = ORIENTED_EDGE ( 'NONE', *, *, #35946, .T. ) ;
#20665 = ORIENTED_EDGE ( 'NONE', *, *, #40231, .F. ) ;
#20666 = CARTESIAN_POINT ( 'NONE',  ( 2.000000000000001776, 0.8935325819929771374, -7.446583077151355923 ) ) ;
#20667 = CARTESIAN_POINT ( 'NONE',  ( 0.3040950598368152291, -9.552450779732055253, -7.687624643091528931 ) ) ;
#20668 = LINE ( 'NONE', #40943, #15170 ) ;
#20669 = CARTESIAN_POINT ( 'NONE',  ( 2.241451721903216399, 3.764430789729979132, 6.641849090084966711 ) ) ;
#20670 = EDGE_LOOP ( 'NONE', ( #14134, #28930, #35228, #18856 ) ) ;
#20671 = ORIENTED_EDGE ( 'NONE', *, *, #36251, .T. ) ;
#20672 = ORIENTED_EDGE ( 'NONE', *, *, #36398, .F. ) ;
#20673 = LINE ( 'NONE', #25007, #5781 ) ;
#20674 = EDGE_CURVE ( 'NONE', #43816, #65741, #14092, .T. ) ;
#20675 = CARTESIAN_POINT ( 'NONE',  ( 35.00000000000000000, -8.258652103341374229, 8.352657516904754331 ) ) ;
#20676 = EDGE_LOOP ( 'NONE', ( #29474, #34501, #52262, #50675 ) ) ;
#20677 = CARTESIAN_POINT ( 'NONE',  ( -18.08686583997218733, 5.151216734910788908, -10.83812558286602012 ) ) ;
#20678 = CARTESIAN_POINT ( 'NONE',  ( -35.00000000000000000, -5.644643009978993931, -10.30098186818255890 ) ) ;
#20679 = ORIENTED_EDGE ( 'NONE', *, *, #27620, .F. ) ;
#20680 = CARTESIAN_POINT ( 'NONE',  ( 2.000000000000001776, -0.3246585432985730213, -6.805031400696120336 ) ) ;
#20681 = CARTESIAN_POINT ( 'NONE',  ( -12.89187373143240833, -28.36023352766247996, -12.94763553493058339 ) ) ;
#20682 = CARTESIAN_POINT ( 'NONE',  ( 0.3040950598368152291, -10.49113473328035084, 6.347045025870730939 ) ) ;
#20683 = VERTEX_POINT ( 'NONE', #50845 ) ;
#20684 = DIRECTION ( 'NONE',  ( 1.000000000000000000, 0.000000000000000000, 0.000000000000000000 ) ) ;
#20685 = ORIENTED_EDGE ( 'NONE', *, *, #31704, .T. ) ;
#20686 = CARTESIAN_POINT ( 'NONE',  ( 1.634816307076161879, -10.17753964889841711, 7.601181930721068625 ) ) ;
#20687 = VERTEX_POINT ( 'NONE', #25562 ) ;
#20688 = CARTESIAN_POINT ( 'NONE',  ( -35.00000000000000000, -5.865551165831157654, 11.32068061209293219 ) ) ;
#20689 = CARTESIAN_POINT ( 'NONE',  ( -14.34460386949389665, -34.50739325218034281, 8.058841881770181459 ) ) ;
#20690 = CARTESIAN_POINT ( 'NONE',  ( 2.000000000000001776, 0.000000000000000000, 0.000000000000000000 ) ) ;
#20691 = ADVANCED_FACE ( 'NONE', ( #9272 ), #15258, .F. ) ;
#20692 = CARTESIAN_POINT ( 'NONE',  ( 35.00000000000000000, 5.273331777780336793, -10.49591321039682690 ) ) ;
#20693 = CARTESIAN_POINT ( 'NONE',  ( 0.3006302518452020900, -12.25587491745529967, 0.2259616664571819644 ) ) ;
#20694 = CYLINDRICAL_SURFACE ( 'NONE', #44617, 4.999999999999997335 ) ;
#20695 = CARTESIAN_POINT ( 'NONE',  ( -27.08417473062937120, 2.249064769433619659, -0.4370481938669387723 ) ) ;
#20696 = DIRECTION ( 'NONE',  ( -1.000000000000000000, -0.000000000000000000, -0.000000000000000000 ) ) ;
#20698 = EDGE_LOOP ( 'NONE', ( #25683, #21972, #38766, #33128 ) ) ;
#20697 = LINE ( 'NONE', #40177, #23563 ) ;
#20699 = DIRECTION ( 'NONE',  ( -1.000000000000000000, -0.000000000000000000, 0.000000000000000000 ) ) ;
#20700 = AXIS2_PLACEMENT_3D ( 'NONE', #57697, #7447, #32703 ) ;
#20701 = ORIENTED_EDGE ( 'NONE', *, *, #35983, .T. ) ;
#20702 = CARTESIAN_POINT ( 'NONE',  ( 0.3106921474978441844, -4.414111574791904857, 11.43920276778355927 ) ) ;
#20703 = ORIENTED_EDGE ( 'NONE', *, *, #43095, .F. ) ;
#20704 = DIRECTION ( 'NONE',  ( 0.000000000000000000, -0.01356324068817992175, 0.9999080150203990547 ) ) ;
#20705 = CIRCLE ( 'NONE', #57886, 4.999999999999999112 ) ;
#20706 = EDGE_LOOP ( 'NONE', ( #29045, #17317, #31232, #45650 ) ) ;
#20707 = DIRECTION ( 'NONE',  ( -1.000000000000000000, -0.000000000000000000, 0.000000000000000000 ) ) ;
#20708 = CARTESIAN_POINT ( 'NONE',  ( 0.6511581176972393026, 11.73752429815159815, -3.919972364658484754 ) ) ;
#20709 = DIRECTION ( 'NONE',  ( 0.000000000000000000, 0.9937233664769756780, -0.1118654143051653060 ) ) ;
#20710 = B_SPLINE_CURVE_WITH_KNOTS ( 'NONE', 3,
 ( #50764, #231, #29179, #34478, #54779, #9514, #40440, #20504, #50115, #19846, #5214, #44439, #65697, #55422, #64717, #19188, #40107, #60399, #4572, #15177 ),
 .UNSPECIFIED., .F., .F.,
 ( 4, 2, 2, 2, 2, 2, 2, 2, 2, 4 ),
 ( 0.003127060359999195467, 0.003972907705248850986, 0.004818755050498505638, 0.005664602395748161157, 0.006510449740997816676, 0.007356297086247472194, 0.008202144431497127713, 0.009047991776746791906, 0.009470915449371621400, 0.009893839121996452629 ),
 .UNSPECIFIED. ) ;
#20711 = CARTESIAN_POINT ( 'NONE',  ( -22.51237073810381517, 2.986282257334773149, -3.263711251981915140 ) ) ;
#20712 = CIRCLE ( 'NONE', #57888, 12.74999999999999822 ) ;
#20713 = CARTESIAN_POINT ( 'NONE',  ( 35.00000000000000000, 4.705694406421931860E-17, -3.469127814946512892E-15 ) ) ;
#20714 = ORIENTED_EDGE ( 'NONE', *, *, #48045, .F. ) ;
#20715 = DIRECTION ( 'NONE',  ( 1.000000000000000000, 0.000000000000000000, 0.000000000000000000 ) ) ;
#20716 = EDGE_CURVE ( 'NONE', #22402, #56626, #49862, .T. ) ;
#20717 = VERTEX_POINT ( 'NONE', #44863 ) ;
#20718 = DIRECTION ( 'NONE',  ( 1.000000000000000000, 0.000000000000000000, 0.000000000000000000 ) ) ;
#20719 = ADVANCED_FACE ( 'NONE', ( #65142 ), #60477, .T. ) ;
#20720 = CARTESIAN_POINT ( 'NONE',  ( -41.00000000000000711, 5.493969937218003549E-16, -4.500000000000000888 ) ) ;
#20721 = ORIENTED_EDGE ( 'NONE', *, *, #39904, .F. ) ;
#20722 = CARTESIAN_POINT ( 'NONE',  ( -27.08871896697694481, -0.9878677378266937925, 2.082324523415888695 ) ) ;
#20723 = AXIS2_PLACEMENT_3D ( 'NONE', #63303, #12113, #5255 ) ;
#20724 = ADVANCED_FACE ( 'NONE', ( #11902 ), #639, .T. ) ;
#20725 = LINE ( 'NONE', #40997, #18092 ) ;
#20726 = CARTESIAN_POINT ( 'NONE',  ( 2.305787727787083519, 5.047606869483132641, -5.756228004061408221 ) ) ;
#20727 = DIRECTION ( 'NONE',  ( 0.000000000000000000, -0.01356324068817991828, 0.9999080150203990547 ) ) ;
#20728 = CARTESIAN_POINT ( 'NONE',  ( 0.2648978790185584908, -6.008231198268910056, -10.67083876753498117 ) ) ;
#20729 = VERTEX_POINT ( 'NONE', #25906 ) ;
#20730 = DIRECTION ( 'NONE',  ( 0.000000000000000000, 0.01356324068817991828, -0.9999080150203990547 ) ) ;
#20731 = AXIS2_PLACEMENT_3D ( 'NONE', #61384, #50774, #20514 ) ;
#20732 = CARTESIAN_POINT ( 'NONE',  ( 2.000000000000001776, 0.000000000000000000, 0.000000000000000000 ) ) ;
#20733 = CARTESIAN_POINT ( 'NONE',  ( -22.94572469358971034, -2.792384151940651371, 4.011883207821675512 ) ) ;
#20734 = B_SPLINE_CURVE_WITH_KNOTS ( 'NONE', 3,
 ( #35402, #55711, #15457, #35723, #10459, #52283, #51302, #36951, #16366, #41620, #36639, #5407, #26017, #31326 ),
 .UNSPECIFIED., .F., .F.,
 ( 4, 2, 2, 2, 2, 2, 4 ),
 ( 0.000000000000000000, 0.001263061922348848558, 0.001894592883523271102, 0.002526123844697694080, 0.003789185767046541337, 0.004420716728220965182, 0.005052247689395389027 ),
 .UNSPECIFIED. ) ;
#20735 = EDGE_CURVE ( 'NONE', #19909, #45349, #16241, .T. ) ;
#20736 = CARTESIAN_POINT ( 'NONE',  ( 2.000000000000001776, 6.750946897830712778, 1.593658756657066355 ) ) ;
#20737 = CARTESIAN_POINT ( 'NONE',  ( 17.27839441901508621, -12.20388373500082224, 5.771933972472480967 ) ) ;
#20738 = CIRCLE ( 'NONE', #47295, 12.75000000000000178 ) ;
#20739 = ORIENTED_EDGE ( 'NONE', *, *, #35510, .T. ) ;
#20740 = CARTESIAN_POINT ( 'NONE',  ( 5.516018279890452902, 0.005042957932158584518, -0.004525000489649788973 ) ) ;
#20741 = CARTESIAN_POINT ( 'NONE',  ( 47.00000000000000711, 4.705694406421931860E-17, -3.469127814946512892E-15 ) ) ;
#20742 = DIRECTION ( 'NONE',  ( 1.000000000000000000, 0.000000000000000000, 0.000000000000000000 ) ) ;
#20743 = ORIENTED_EDGE ( 'NONE', *, *, #52465, .F. ) ;
#20744 = CARTESIAN_POINT ( 'NONE',  ( 1.719304012340733934, -11.67935079956419031, -5.066286238786891438 ) ) ;
#20745 = CARTESIAN_POINT ( 'NONE',  ( 2.000000000000001776, 5.396716205731433291, 4.158041573745082431 ) ) ;
#20746 = VERTEX_POINT ( 'NONE', #11576 ) ;
#20747 = ORIENTED_EDGE ( 'NONE', *, *, #1871, .F. ) ;
#20748 = VERTEX_POINT ( 'NONE', #46831 ) ;
#20749 = AXIS2_PLACEMENT_3D ( 'NONE', #13470, #24782, #45060 ) ;
#20750 = ORIENTED_EDGE ( 'NONE', *, *, #23408, .F. ) ;
#20751 = CARTESIAN_POINT ( 'NONE',  ( 2.903928887688637328, 7.845932231840992088, 3.918141038919173536 ) ) ;
#20752 = CARTESIAN_POINT ( 'NONE',  ( -22.27719381268171261, -3.561499689648247369, 0.9326100520993009235 ) ) ;
#20753 = CARTESIAN_POINT ( 'NONE',  ( 3.152665057734131526, -0.9030954876737319337, -7.886634106564212487 ) ) ;
#20754 = CARTESIAN_POINT ( 'NONE',  ( 9.272965915927473546, 6.113671464449896398, 10.33142599188169974 ) ) ;
#20755 = CARTESIAN_POINT ( 'NONE',  ( 1.948354844646335460, 9.982942661982825427, -6.595573209516024882 ) ) ;
#20756 = CARTESIAN_POINT ( 'NONE',  ( -5.901743774574147672, -31.73659747722650692, 13.63115424678022158 ) ) ;
#20757 = DIRECTION ( 'NONE',  ( 0.000000000000000000, 0.4698238015817364777, 0.8827602140260315533 ) ) ;
#20759 = ORIENTED_EDGE ( 'NONE', *, *, #41113, .F. ) ;
#20758 = CARTESIAN_POINT ( 'NONE',  ( 2.000000000000001776, 1.779948802829910193, -6.576141558201243242 ) ) ;
#20760 = CARTESIAN_POINT ( 'NONE',  ( 22.88594695219327235, -4.822122601967141264, 25.00000000000000000 ) ) ;
#20761 = EDGE_LOOP ( 'NONE', ( #32232, #38925, #30207, #62705 ) ) ;
#20762 = FACE_OUTER_BOUND ( 'NONE', #34806, .T. ) ;
#20763 = ORIENTED_EDGE ( 'NONE', *, *, #38799, .T. ) ;
#20764 = EDGE_LOOP ( 'NONE', ( #32696, #23783, #64589, #27701 ) ) ;
#20765 = CARTESIAN_POINT ( 'NONE',  ( -27.10719052120871098, 1.714424047991082389, 1.622102031466668093 ) ) ;
#20766 = CARTESIAN_POINT ( 'NONE',  ( 11.32820571420733557, -29.68697874620739796, 9.642237626533521677 ) ) ;
#20767 = CYLINDRICAL_SURFACE ( 'NONE', #34353, 5.000000000000000888 ) ;
#20768 = EDGE_CURVE ( 'NONE', #65529, #18937, #10924, .T. ) ;
#20769 = CARTESIAN_POINT ( 'NONE',  ( 37.00000000000000711, -12.49688848680882103, 2.527899948230768690 ) ) ;
#20770 = CARTESIAN_POINT ( 'NONE',  ( 1.634816307075119601, -2.910502128620189310, 12.36483956257006511 ) ) ;
#20771 = DIRECTION ( 'NONE',  ( -1.000000000000000000, 0.000000000000000000, 0.000000000000000000 ) ) ;
#20772 = ORIENTED_EDGE ( 'NONE', *, *, #61080, .T. ) ;
#20773 =( BOUNDED_SURFACE ( )  B_SPLINE_SURFACE ( 3, 1, ( 
 ( #65368, #30133 ),
 ( #4210, #25806 ),
 ( #4879, #35441 ),
 ( #65681, #546 ) ),
 .UNSPECIFIED., .F., .F., .F. ) 
 B_SPLINE_SURFACE_WITH_KNOTS ( ( 4, 4 ),
 ( 2, 2 ),
 ( 0.000000000000000000, 1.000000000000000000 ),
 ( 0.000000000000000000, 1.000000000000000000 ),
 .UNSPECIFIED. ) 
 GEOMETRIC_REPRESENTATION_ITEM ( )  RATIONAL_B_SPLINE_SURFACE ( (
 ( 1.000000000000000000, 1.000000000000000000),
 ( 0.6933888150995267674, 0.9895912004443193632),
 ( 0.6933888150995267674, 0.9895912004443193632),
 ( 1.000000000000000000, 1.000000000000000000) ) ) 
 REPRESENTATION_ITEM ( '' )  SURFACE ( )  );
#20774 = VERTEX_POINT ( 'NONE', #15896 ) ;
#20775 = CARTESIAN_POINT ( 'NONE',  ( 0.3106921474978469599, 12.03191800497307895, 2.360654586927831478 ) ) ;
#20776 = VERTEX_POINT ( 'NONE', #6934 ) ;
#20777 = ORIENTED_EDGE ( 'NONE', *, *, #50453, .T. ) ;
#20778 = CARTESIAN_POINT ( 'NONE',  ( -37.00000000000000711, 0.000000000000000000, 0.000000000000000000 ) ) ;
#20779 = CARTESIAN_POINT ( 'NONE',  ( -37.00000000000000711, 11.68758509253248334, -1.171570255487489609 ) ) ;
#20780 = CARTESIAN_POINT ( 'NONE',  ( 2.241352910868908754, 1.243507963608094347, 7.532448145350512547 ) ) ;
#20781 = CARTESIAN_POINT ( 'NONE',  ( 0.000000000000000000, 2.664846396702580833, -6.404188155572981600 ) ) ;
#20782 = CARTESIAN_POINT ( 'NONE',  ( -22.27721688985630522, 1.293557211780076432, -3.446999288411542128 ) ) ;
#20783 = CARTESIAN_POINT ( 'NONE',  ( -7.994277101543554309, -1.718098006006025580, -11.87788732319827822 ) ) ;
#20784 = EDGE_CURVE ( 'NONE', #22075, #13308, #48112, .T. ) ;
#20785 = CARTESIAN_POINT ( 'NONE',  ( 36.00000000000000711, -8.366449238204431538, -9.621072037176967129 ) ) ;
#20786 = AXIS2_PLACEMENT_3D ( 'NONE', #63715, #22528, #11878 ) ;
#20787 =( BOUNDED_SURFACE ( )  B_SPLINE_SURFACE ( 3, 1, ( 
 ( #24480, #44757 ),
 ( #65367, #38807 ),
 ( #29782, #18852 ),
 ( #9841, #23857 ) ),
 .UNSPECIFIED., .F., .F., .F. ) 
 B_SPLINE_SURFACE_WITH_KNOTS ( ( 4, 4 ),
 ( 2, 2 ),
 ( 0.000000000000000000, 1.000000000000000000 ),
 ( 0.000000000000000000, 1.000000000000000000 ),
 .UNSPECIFIED. ) 
 GEOMETRIC_REPRESENTATION_ITEM ( )  RATIONAL_B_SPLINE_SURFACE ( (
 ( 1.000000000000000000, 1.000000000000000000),
 ( 0.9856612449720755231, 0.9999558406602322425),
 ( 0.9856612449720755231, 0.9999558406602322425),
 ( 1.000000000000000000, 1.000000000000000000) ) ) 
 REPRESENTATION_ITEM ( '' )  SURFACE ( )  );
#20788 = ADVANCED_FACE ( 'NONE', ( #41496 ), #44646, .F. ) ;
#20789 = ORIENTED_EDGE ( 'NONE', *, *, #36424, .F. ) ;
#20790 = ADVANCED_FACE ( 'NONE', ( #6282 ), #50292, .T. ) ;
#20791 = DIRECTION ( 'NONE',  ( 1.000000000000000000, 0.000000000000000000, 0.000000000000000000 ) ) ;
#20792 = DIRECTION ( 'NONE',  ( 1.000000000000000000, 0.000000000000000000, 0.000000000000000000 ) ) ;
#20793 = CARTESIAN_POINT ( 'NONE',  ( -3.116620688030298680, -9.325418049453649161, 9.768128050516612149 ) ) ;
#20794 = AXIS2_PLACEMENT_3D ( 'NONE', #6799, #2122, #22748 ) ;
#20795 = CARTESIAN_POINT ( 'NONE',  ( 6.361445718264521432, -4.355102044641763648, 11.18181944858514498 ) ) ;
#20796 = CARTESIAN_POINT ( 'NONE',  ( 1.719304012339893939, -12.38166659046436457, -2.961219984258754767 ) ) ;
#20797 = EDGE_CURVE ( 'NONE', #62352, #10311, #47496, .T. ) ;
#20798 = CARTESIAN_POINT ( 'NONE',  ( 36.00000000000000711, 4.561791185930414549, -11.90598845858535704 ) ) ;
#20799 = EDGE_CURVE ( 'NONE', #61423, #42768, #24795, .T. ) ;
#20800 = FACE_OUTER_BOUND ( 'NONE', #39907, .T. ) ;
#20801 = CYLINDRICAL_SURFACE ( 'NONE', #25700, 12.74999999999999822 ) ;
#20802 = ORIENTED_EDGE ( 'NONE', *, *, #51650, .T. ) ;
#20803 = CARTESIAN_POINT ( 'NONE',  ( 0.2651627682582901602, 10.64925413290593603, 6.046625184671022168 ) ) ;
#20804 = CARTESIAN_POINT ( 'NONE',  ( 5.515188684475870851, 0.003857086913166391916, 0.003709313826049759084 ) ) ;
#20805 = CARTESIAN_POINT ( 'NONE',  ( 35.00000000000000000, -9.217970097227778936, -7.971186206369441862 ) ) ;
#20806 = EDGE_CURVE ( 'NONE', #35321, #24723, #2499, .T. ) ;
#20807 = CARTESIAN_POINT ( 'NONE',  ( -0.8753493882257603609, -31.04850208196563344, -14.43082775300592324 ) ) ;
#20808 = CARTESIAN_POINT ( 'NONE',  ( 0.3675815128205894289, 12.13672785388550324, 1.872154644482125763 ) ) ;
#20809 = ORIENTED_EDGE ( 'NONE', *, *, #44402, .F. ) ;
#20810 = CARTESIAN_POINT ( 'NONE',  ( -18.39961019094981509, -4.493736647258883110, -12.73074473482842883 ) ) ;
#20811 = CARTESIAN_POINT ( 'NONE',  ( -37.00000000000000711, 10.01317267707896441, -6.946017217729827387 ) ) ;
#20813 = EDGE_CURVE ( 'NONE', #9428, #14609, #62767, .T. ) ;
#20812 = CARTESIAN_POINT ( 'NONE',  ( 12.69762816655162574, -29.19309327991418357, -4.289906119468183121 ) ) ;
#20814 = ORIENTED_EDGE ( 'NONE', *, *, #29753, .F. ) ;
#20815 = CARTESIAN_POINT ( 'NONE',  ( 2.000000000000001776, 7.248432822490259220, 1.926193556693033271 ) ) ;
#20816 = LINE ( 'NONE', #5203, #12964 ) ;
#20817 = CARTESIAN_POINT ( 'NONE',  ( -36.00000000000000711, 12.74068829017554094, 0.4871980014161925165 ) ) ;
#20819 = ORIENTED_EDGE ( 'NONE', *, *, #11648, .F. ) ;
#20818 = CARTESIAN_POINT ( 'NONE',  ( -35.00000000000000000, -11.01837265713077585, 6.415447294506668285 ) ) ;
#20820 = DIRECTION ( 'NONE',  ( 0.2475719085175098200, -2.922992529533354589E-16, -0.9688695217174487784 ) ) ;
#20821 = B_SPLINE_CURVE_WITH_KNOTS ( 'NONE', 3,
 ( #7653, #59186, #32894, #7304, #27589, #63487, #47890, #38218, #28264, #49224, #8305, #2349, #33890, #8629, #24241, #19911, #34846, #9581, #45185, #55155, #34544, #50835, #34218, #13924, #30220, #3978 ),
 .UNSPECIFIED., .F., .F.,
 ( 4, 2, 2, 2, 2, 2, 2, 2, 2, 2, 2, 2, 4 ),
 ( 0.02249411442595698057, 0.02389926644164680827, 0.02530441845733663597, 0.02811472248871628790, 0.02951987450440611213, 0.03092502652009593983, 0.03373533055147559523, 0.03654563458285524369, 0.03795078659854507486, 0.03935593861423490603, 0.04076109062992473026, 0.04216624264561455449, 0.04497654667699420294 ),
 .UNSPECIFIED. ) ;
#20822 = VECTOR ( 'NONE', #35951, 1000.000000000000000 ) ;
#20823 = CARTESIAN_POINT ( 'NONE',  ( 3.152665057735546839, 0.4801242025606423658, 7.923639299008859105 ) ) ;
#20824 = VERTEX_POINT ( 'NONE', #42147 ) ;
#20825 = CARTESIAN_POINT ( 'NONE',  ( -22.70624764888619751, 4.891815784104551312, -1.907540768355076688 ) ) ;
#20826 = CARTESIAN_POINT ( 'NONE',  ( -9.342997049464392134, 12.02615817703077283, -6.144013915069329812 ) ) ;
#20827 = CARTESIAN_POINT ( 'NONE',  ( 24.40168093369100433, -0.3774522545360152748, -11.99947585575983844 ) ) ;
#20828 = CARTESIAN_POINT ( 'NONE',  ( 10.16647825512967351, 8.042666982224721650, -10.84593607609787647 ) ) ;
#20829 = DIRECTION ( 'NONE',  ( 0.000000000000000000, -0.01356324068817998940, 0.9999080150203990547 ) ) ;
#20830 = LINE ( 'NONE', #56402, #39776 ) ;
#20831 = CARTESIAN_POINT ( 'NONE',  ( 2.889800649504073782, -5.728825117897692998, -2.156828754871525256 ) ) ;
#20832 = ORIENTED_EDGE ( 'NONE', *, *, #51117, .F. ) ;
#20833 = CARTESIAN_POINT ( 'NONE',  ( -37.00000000000000711, 0.000000000000000000, 0.000000000000000000 ) ) ;
#20834 = ORIENTED_EDGE ( 'NONE', *, *, #46163, .T. ) ;
#20835 = DIRECTION ( 'NONE',  ( -1.000000000000000000, 0.000000000000000000, 0.000000000000000000 ) ) ;
#20836 = DIRECTION ( 'NONE',  ( -1.000000000000000000, 0.000000000000000000, 0.000000000000000000 ) ) ;
#20837 = EDGE_CURVE ( 'NONE', #42300, #44156, #11973, .T. ) ;
#20838 = B_SPLINE_CURVE_WITH_KNOTS ( 'NONE', 3,
 ( #9465, #59376, #13798, #8182, #28786, #19479, #39748, #24442, #18518, #49097 ),
 .UNSPECIFIED., .F., .F.,
 ( 4, 3, 3, 4 ),
 ( 8.673617379884035472E-19, 6.607638129004427896E-05, 9.911389841680530389E-05, 0.0001667630577588622028 ),
 .UNSPECIFIED. ) ;
#20839 = CARTESIAN_POINT ( 'NONE',  ( -35.00000000000000000, 11.37311665002359540, 2.936739658820077370 ) ) ;
#20840 = VERTEX_POINT ( 'NONE', #46503 ) ;
#20841 = CARTESIAN_POINT ( 'NONE',  ( 5.515539859299206427, 0.005618668168217494027, -0.002251761459665947360 ) ) ;
#20842 = CARTESIAN_POINT ( 'NONE',  ( 12.89305137491219710, 10.53990944163839671, -5.751062137880654568 ) ) ;
#20843 = DIRECTION ( 'NONE',  ( 1.000000000000000000, 0.000000000000000000, 0.000000000000000000 ) ) ;
#20844 = ORIENTED_EDGE ( 'NONE', *, *, #28296, .T. ) ;
#20845 = ORIENTED_EDGE ( 'NONE', *, *, #7668, .F. ) ;
#20846 = FACE_OUTER_BOUND ( 'NONE', #44359, .T. ) ;
#20847 = EDGE_CURVE ( 'NONE', #29772, #37649, #61950, .T. ) ;
#20848 = ORIENTED_EDGE ( 'NONE', *, *, #53780, .F. ) ;
#20849 = CARTESIAN_POINT ( 'NONE',  ( 2.000000000000001776, 0.000000000000000000, 0.000000000000000000 ) ) ;
#20850 = CARTESIAN_POINT ( 'NONE',  ( -27.09569413923794556, 0.5521997980586342836, -2.259195818742698592 ) ) ;
#20851 = CARTESIAN_POINT ( 'NONE',  ( -27.08704841010922593, 2.291653842312379563, -0.1930432016059793476 ) ) ;
#20852 = DIRECTION ( 'NONE',  ( 0.000000000000000000, 0.3554799084908970563, 0.9346839223284539866 ) ) ;
#20853 = CARTESIAN_POINT ( 'NONE',  ( 1.000000000000000888, 7.493043167941616289, 0.3229614270519615693 ) ) ;
#20854 = CARTESIAN_POINT ( 'NONE',  ( 26.34661844826604593, -11.53221627053866527, 3.317828791472333005 ) ) ;
#20855 = EDGE_CURVE ( 'NONE', #48474, #54096, #43872, .T. ) ;
#20856 = CARTESIAN_POINT ( 'NONE',  ( 2.298277635560284082, 7.506689984432329155, 1.491234112749218355 ) ) ;
#20857 = ORIENTED_EDGE ( 'NONE', *, *, #48446, .T. ) ;
#20858 = DIRECTION ( 'NONE',  ( 0.000000000000000000, -0.01356324068817999114, 0.9999080150203989437 ) ) ;
#20859 = CARTESIAN_POINT ( 'NONE',  ( 35.00000000000000000, -1.286231064351218478, 12.68495603654572612 ) ) ;
#20860 = EDGE_CURVE ( 'NONE', #13608, #60024, #37501, .T. ) ;
#20861 = CARTESIAN_POINT ( 'NONE',  ( -37.00000000000000711, 8.017674001891920810, -9.913596905230035006 ) ) ;
#20862 = CARTESIAN_POINT ( 'NONE',  ( -9.251009239874910861, 10.88051098239768955, -5.064585925472082195 ) ) ;
#20863 = CARTESIAN_POINT ( 'NONE',  ( -35.00000000000000000, -8.295159312811792418, -8.927548052240984688 ) ) ;
#20864 = CARTESIAN_POINT ( 'NONE',  ( 0.3164563675027660117, -10.73846246126245063, -5.922187299605745636 ) ) ;
#20865 = DIRECTION ( 'NONE',  ( 1.000000000000000000, 0.000000000000000000, 0.000000000000000000 ) ) ;
#20866 = CARTESIAN_POINT ( 'NONE',  ( 5.514970785353741078, 0.001117786416802112525, -0.004588761610584830321 ) ) ;
#20867 = EDGE_LOOP ( 'NONE', ( #32787, #54290, #30702, #9804 ) ) ;
#20868 = CARTESIAN_POINT ( 'NONE',  ( -35.00000000000000000, 0.000000000000000000, 0.000000000000000000 ) ) ;
#20869 = AXIS2_PLACEMENT_3D ( 'NONE', #38669, #52968, #13384 ) ;
#20870 = ORIENTED_EDGE ( 'NONE', *, *, #3879, .T. ) ;
#20871 = CARTESIAN_POINT ( 'NONE',  ( 0.2653141435805182469, 0.04404957080779424439, 12.24612531649369274 ) ) ;
#20872 = EDGE_CURVE ( 'NONE', #11917, #27835, #18398, .T. ) ;
#20873 = CARTESIAN_POINT ( 'NONE',  ( -47.00000000000000711, 0.000000000000000000, 0.000000000000000000 ) ) ;
#20874 = CARTESIAN_POINT ( 'NONE',  ( 0.3675815128205894289, 4.447030445008336663, -11.44679196252404729 ) ) ;
#20875 = DIRECTION ( 'NONE',  ( -0.000000000000000000, -0.000000000000000000, -1.000000000000000000 ) ) ;
#20876 = ADVANCED_FACE ( 'NONE', ( #47816 ), #18220, .T. ) ;
#20877 = ORIENTED_EDGE ( 'NONE', *, *, #64825, .T. ) ;
#20878 = CARTESIAN_POINT ( 'NONE',  ( -35.00000000000000000, 9.557269938331666381, -7.561043153947866635 ) ) ;
#20879 = CARTESIAN_POINT ( 'NONE',  ( 1.283627346226434263, -1.641214790178027405, 12.47820286973605342 ) ) ;
#20880 = LINE ( 'NONE', #50508, #53997 ) ;
#20881 = EDGE_CURVE ( 'NONE', #41793, #50474, #14141, .T. ) ;
#20882 = EDGE_CURVE ( 'NONE', #50607, #22014, #26874, .T. ) ;
#20883 = CARTESIAN_POINT ( 'NONE',  ( 37.00000000000000711, 11.02904044024202967, -4.041347439436060007 ) ) ;
#20884 = DIRECTION ( 'NONE',  ( -1.000000000000000000, 0.000000000000000000, 0.000000000000000000 ) ) ;
#20885 = EDGE_LOOP ( 'NONE', ( #53232, #1283, #64009, #30516 ) ) ;
#20887 = EDGE_CURVE ( 'NONE', #14210, #58632, #23900, .T. ) ;
#20886 = DIRECTION ( 'NONE',  ( 0.000000000000000000, 0.6943713148249640588, -0.7196168960969792083 ) ) ;
#20888 = ORIENTED_EDGE ( 'NONE', *, *, #59713, .F. ) ;
#20889 = CARTESIAN_POINT ( 'NONE',  ( 0.2834382757448011270, -0.2027202995056148482, -12.25055062943084927 ) ) ;
#20890 = CARTESIAN_POINT ( 'NONE',  ( 0.3040950598368152291, -9.229598020917739731, 8.072385578287439856 ) ) ;
#20891 = CARTESIAN_POINT ( 'NONE',  ( 2.000000000000001776, 0.000000000000000000, 0.000000000000000000 ) ) ;
#20892 = ORIENTED_EDGE ( 'NONE', *, *, #52355, .F. ) ;
#20893 = ORIENTED_EDGE ( 'NONE', *, *, #23934, .F. ) ;
#20894 = DIRECTION ( 'NONE',  ( 0.000000000000000000, -0.01356324068817991828, 0.9999080150203990547 ) ) ;
#20895 = ORIENTED_EDGE ( 'NONE', *, *, #15510, .F. ) ;
#20896 = CARTESIAN_POINT ( 'NONE',  ( 2.284126774967656370, -6.543266298866105224, -3.960764882115069607 ) ) ;
#20897 = DIRECTION ( 'NONE',  ( 0.000000000000000000, 0.2618041379715563277, -0.9651210252299813330 ) ) ;
#20898 = CARTESIAN_POINT ( 'NONE',  ( -22.27711653538342773, -3.377206745424988554, -1.465933162149073210 ) ) ;
#20899 = CARTESIAN_POINT ( 'NONE',  ( 1.462291587748165700, 9.267729738232345582, 8.602888600420595111 ) ) ;
#20900 = CARTESIAN_POINT ( 'NONE',  ( 0.9232167919969100911, 9.278116382137485019, -8.324955738482373135 ) ) ;
#20901 = DIRECTION ( 'NONE',  ( 0.000000000000000000, 0.9796553971857748788, 0.2006870767258854826 ) ) ;
#20902 = DIRECTION ( 'NONE',  ( 1.000000000000000000, -0.000000000000000000, 0.000000000000000000 ) ) ;
#20903 = ORIENTED_EDGE ( 'NONE', *, *, #37819, .F. ) ;
#20904 = CARTESIAN_POINT ( 'NONE',  ( 2.994568964204218364, -2.317954327151173555, -7.537093683963818513 ) ) ;
#20905 = ORIENTED_EDGE ( 'NONE', *, *, #33081, .T. ) ;
#20906 = CIRCLE ( 'NONE', #13448, 5.000000000000000000 ) ;
#20907 = CARTESIAN_POINT ( 'NONE',  ( 10.75853767213705048, 7.830989516993144051, 10.99661780661416088 ) ) ;
#20908 = CARTESIAN_POINT ( 'NONE',  ( 0.3632410797595237995, -9.235006602299407064, 8.092233745354604935 ) ) ;
#20909 = CARTESIAN_POINT ( 'NONE',  ( 18.66452593080030198, 6.623341608272929726, 11.78786073385051303 ) ) ;
#20910 = EDGE_CURVE ( 'NONE', #31853, #32709, #22664, .T. ) ;
#20911 = ORIENTED_EDGE ( 'NONE', *, *, #54866, .T. ) ;
#20912 = DIRECTION ( 'NONE',  ( -1.000000000000000000, 0.000000000000000000, 0.000000000000000000 ) ) ;
#20913 = ORIENTED_EDGE ( 'NONE', *, *, #46453, .T. ) ;
#20914 = CARTESIAN_POINT ( 'NONE',  ( 9.687175622948609899, 25.00000000000000000, -0.5854820436212360146 ) ) ;
#20915 = CARTESIAN_POINT ( 'NONE',  ( 1.452237505248555660, 10.65201107290477012, -6.833827325205206193 ) ) ;
#20916 = CARTESIAN_POINT ( 'NONE',  ( 2.491965175174298608, 2.837956678388472653, 7.177226758613711510 ) ) ;
#20917 = CARTESIAN_POINT ( 'NONE',  ( -48.17199526896420991, -0.3660652840184910883, 6.262213226250253228 ) ) ;
#20918 = VERTEX_POINT ( 'NONE', #8552 ) ;
#20919 = ORIENTED_EDGE ( 'NONE', *, *, #17109, .T. ) ;
#20920 = FACE_OUTER_BOUND ( 'NONE', #51884, .T. ) ;
#20921 = ORIENTED_EDGE ( 'NONE', *, *, #49450, .T. ) ;
#20922 = DIRECTION ( 'NONE',  ( -1.000000000000000000, 0.000000000000000000, 0.000000000000000000 ) ) ;
#20923 = VERTEX_POINT ( 'NONE', #38822 ) ;
#20924 = ADVANCED_FACE ( 'NONE', ( #39132 ), #33169, .T. ) ;
#20925 = VERTEX_POINT ( 'NONE', #53799 ) ;
#20926 = VERTEX_POINT ( 'NONE', #8234 ) ;
#20927 = DIRECTION ( 'NONE',  ( -0.3939253465568944290, -0.5833358547425138152, 0.7103112711423431591 ) ) ;
#20928 = CARTESIAN_POINT ( 'NONE',  ( 0.7446945582506530048, 11.53120448859746539, 4.576048078258359020 ) ) ;
#20929 = DIRECTION ( 'NONE',  ( 0.000000000000000000, 0.000000000000000000, 1.000000000000000000 ) ) ;
#20930 = CARTESIAN_POINT ( 'NONE',  ( 5.530133899448235191, -0.01324661008606583569, 0.008946569461392389275 ) ) ;
#20931 = CARTESIAN_POINT ( 'NONE',  ( -35.00000000000000000, 1.903127969211188653, 11.59095880812009227 ) ) ;
#20932 = ORIENTED_EDGE ( 'NONE', *, *, #11523, .T. ) ;
#20933 = CARTESIAN_POINT ( 'NONE',  ( -36.00000000000000711, -8.017674001891851532, 9.913596905230088296 ) ) ;
#20934 = ORIENTED_EDGE ( 'NONE', *, *, #19213, .T. ) ;
#20935 = CARTESIAN_POINT ( 'NONE',  ( 0.000000000000000000, 0.000000000000000000, 0.000000000000000000 ) ) ;
#20936 = CARTESIAN_POINT ( 'NONE',  ( -27.09125059358652265, 0.6356863790372305756, 2.223272438024522124 ) ) ;
#20937 = DIRECTION ( 'NONE',  ( 1.000000000000000000, 0.000000000000000000, 0.000000000000000000 ) ) ;
#20938 = EDGE_CURVE ( 'NONE', #53897, #49252, #1638, .T. ) ;
#20939 = CARTESIAN_POINT ( 'NONE',  ( 37.00000000000000711, -1.113475361586579337, -12.70128625845192616 ) ) ;
#20940 = LINE ( 'NONE', #62173, #64697 ) ;
#20941 = CARTESIAN_POINT ( 'NONE',  ( 1.462291587751777033, -10.62080802716771721, -6.862867011843016840 ) ) ;
#20942 = EDGE_CURVE ( 'NONE', #24055, #54635, #21623, .T. ) ;
#20943 = ORIENTED_EDGE ( 'NONE', *, *, #11869, .T. ) ;
#20944 = DIRECTION ( 'NONE',  ( 1.000000000000000000, 0.000000000000000000, 0.000000000000000000 ) ) ;
#20945 = ORIENTED_EDGE ( 'NONE', *, *, #54934, .F. ) ;
#20946 = DIRECTION ( 'NONE',  ( 0.8405098440481681976, 0.000000000000000000, -0.5417962735734934698 ) ) ;
#20947 = CARTESIAN_POINT ( 'NONE',  ( 0.9972908435452140230, -25.72582856205513835, -15.66294124711422775 ) ) ;
#20948 = CARTESIAN_POINT ( 'NONE',  ( 11.20797324838624220, -27.95044230146133657, 13.82289656124155997 ) ) ;
#20949 = DIRECTION ( 'NONE',  ( -1.000000000000000000, 0.000000000000000000, -0.000000000000000000 ) ) ;
#20950 = CARTESIAN_POINT ( 'NONE',  ( -22.66110217412718342, -1.880032915665386106, -4.573370147466340185 ) ) ;
#20951 = ORIENTED_EDGE ( 'NONE', *, *, #28130, .T. ) ;
#20952 = DIRECTION ( 'NONE',  ( 0.000000000000000000, 0.9718671068226452103, -0.2355298848897551256 ) ) ;
#20953 = CARTESIAN_POINT ( 'NONE',  ( 0.7400311444011689055, 5.892391870929167830, -10.91558650018036225 ) ) ;
#20954 = CARTESIAN_POINT ( 'NONE',  ( 24.48817448996944535, 8.566713351873016080, -8.406659586863929334 ) ) ;
#20955 = CARTESIAN_POINT ( 'NONE',  ( 22.46687615433434004, -12.34696333092269604, -5.470250127934074946 ) ) ;
#20956 = ADVANCED_FACE ( 'NONE', ( #65381 ), #29805, .T. ) ;
#20957 = EDGE_CURVE ( 'NONE', #18937, #49613, #52382, .T. ) ;
#20958 = DIRECTION ( 'NONE',  ( -1.000000000000000000, 0.000000000000000000, 0.000000000000000000 ) ) ;
#20959 =( BOUNDED_SURFACE ( )  B_SPLINE_SURFACE ( 3, 1, ( 
 ( #6761, #469 ),
 ( #56973, #11716 ),
 ( #62580, #61287 ),
 ( #21383, #15718 ) ),
 .UNSPECIFIED., .F., .F., .F. ) 
 B_SPLINE_SURFACE_WITH_KNOTS ( ( 4, 4 ),
 ( 2, 2 ),
 ( 0.000000000000000000, 1.000000000000000000 ),
 ( 0.000000000000000000, 1.000000000000000000 ),
 .UNSPECIFIED. ) 
 GEOMETRIC_REPRESENTATION_ITEM ( )  RATIONAL_B_SPLINE_SURFACE ( (
 ( 1.000000000000000000, 1.000000000000000000),
 ( 0.9856612449720755231, 0.9999558406602322425),
 ( 0.9856612449720755231, 0.9999558406602322425),
 ( 1.000000000000000000, 1.000000000000000000) ) ) 
 REPRESENTATION_ITEM ( '' )  SURFACE ( )  );
#20961 = EDGE_CURVE ( 'NONE', #50893, #45822, #23708, .T. ) ;
#20960 = CARTESIAN_POINT ( 'NONE',  ( 5.520433897694421610, -0.01329351892497966821, 0.007082458259338164468 ) ) ;
#20962 = FACE_BOUND ( 'NONE', #23125, .T. ) ;
#20963 = DIRECTION ( 'NONE',  ( -1.000000000000000000, 0.000000000000000000, 0.000000000000000000 ) ) ;
#20964 = LINE ( 'NONE', #32, #47145 ) ;
#20965 = EDGE_CURVE ( 'NONE', #15192, #46997, #58756, .T. ) ;
#20966 = ORIENTED_EDGE ( 'NONE', *, *, #14335, .T. ) ;
#20967 = EDGE_LOOP ( 'NONE', ( #32524, #61742, #49763, #49789 ) ) ;
#20968 = CARTESIAN_POINT ( 'NONE',  ( 9.687175622948609899, 25.00000000000000000, -0.5854820436212360146 ) ) ;
#20969 = CARTESIAN_POINT ( 'NONE',  ( 35.00000000000000000, -0.4353888892049205261, -11.73808581813437968 ) ) ;
#20970 = DIRECTION ( 'NONE',  ( 0.000000000000000000, 0.01356324068817992175, -0.9999080150203990547 ) ) ;
#20971 = DIRECTION ( 'NONE',  ( 1.000000000000000000, -0.000000000000000000, 0.000000000000000000 ) ) ;
#20972 = VERTEX_POINT ( 'NONE', #34142 ) ;
#20973 = ORIENTED_EDGE ( 'NONE', *, *, #51406, .T. ) ;
#20974 = EDGE_LOOP ( 'NONE', ( #4364, #45871, #61485, #47335 ) ) ;
#20975 = CARTESIAN_POINT ( 'NONE',  ( 2.440552418640498544, 7.698292014589401155, 0.1974238147509528030 ) ) ;
#20976 = VECTOR ( 'NONE', #54564, 1000.000000000000000 ) ;
#20977 = CARTESIAN_POINT ( 'NONE',  ( -35.00000000000000000, -10.64792938439751246, -5.927257550915431494 ) ) ;
#20978 = ORIENTED_EDGE ( 'NONE', *, *, #53978, .T. ) ;
#20979 = CARTESIAN_POINT ( 'NONE',  ( 12.10998784662220729, 25.00000000000000000, -8.526922110106905706 ) ) ;
#20980 = CYLINDRICAL_SURFACE ( 'NONE', #65023, 2.899999999999994582 ) ;
#20981 = EDGE_CURVE ( 'NONE', #15531, #60445, #20710, .T. ) ;
#20983 = ORIENTED_EDGE ( 'NONE', *, *, #58785, .T. ) ;
#20982 = AXIS2_PLACEMENT_3D ( 'NONE', #33315, #6744, #2070 ) ;
#20984 = CYLINDRICAL_SURFACE ( 'NONE', #2470, 2.899999999999994582 ) ;
#20985 = CARTESIAN_POINT ( 'NONE',  ( 11.15801620995752863, -32.62087690405027018, -12.20531625113489227 ) ) ;
#20986 = CARTESIAN_POINT ( 'NONE',  ( -19.47984447937493613, -1.416020129149132334, 25.00000000000000000 ) ) ;
#20987 = ORIENTED_EDGE ( 'NONE', *, *, #10181, .T. ) ;
#20988 = DIRECTION ( 'NONE',  ( -1.000000000000000000, 0.000000000000000000, 0.000000000000000000 ) ) ;
#20989 = VERTEX_POINT ( 'NONE', #49475 ) ;
#20990 = CARTESIAN_POINT ( 'NONE',  ( 1.372161826076962132, 7.648244077827059506, -10.03232826862097760 ) ) ;
#20991 = ORIENTED_EDGE ( 'NONE', *, *, #21503, .T. ) ;
#20992 = AXIS2_PLACEMENT_3D ( 'NONE', #7120, #1821, #36729 ) ;
#20993 = LINE ( 'NONE', #41274, #7504 ) ;
#20994 = CARTESIAN_POINT ( 'NONE',  ( 0.2646305136544072623, -11.55263159009956020, -4.064188116014665120 ) ) ;
#20995 = CARTESIAN_POINT ( 'NONE',  ( 2.241317068080781461, 3.896159243838555941, 6.565357088387183460 ) ) ;
#20996 = CARTESIAN_POINT ( 'NONE',  ( 36.00000000000000711, 5.143145423404280159, -11.66664283989682005 ) ) ;
#20997 = FACE_OUTER_BOUND ( 'NONE', #6805, .T. ) ;
#20998 = CIRCLE ( 'NONE', #24187, 12.74999999999999822 ) ;
#20999 = DIRECTION ( 'NONE',  ( 0.000000000000000000, 0.01356324068817998940, -0.9999080150203990547 ) ) ;
#21000 = CARTESIAN_POINT ( 'NONE',  ( -27.08871896697731785, -0.1856437051692902407, -2.297279805116104967 ) ) ;
#21001 = DIRECTION ( 'NONE',  ( 0.000000000000000000, 0.000000000000000000, 1.000000000000000000 ) ) ;
#21003 = ORIENTED_EDGE ( 'NONE', *, *, #13063, .F. ) ;
#21002 = DIRECTION ( 'NONE',  ( 0.000000000000000000, 0.01356324068817998073, -0.9999080150203990547 ) ) ;
#21004 = LINE ( 'NONE', #35318, #9879 ) ;
#21005 = VERTEX_POINT ( 'NONE', #13848 ) ;
#21006 = CARTESIAN_POINT ( 'NONE',  ( 5.520433897694421610, 0.01505375422439067870, 0.0005131706886599866424 ) ) ;
#21007 = DIRECTION ( 'NONE',  ( -1.000000000000000000, -0.000000000000000000, 0.000000000000000000 ) ) ;
#21008 = ADVANCED_FACE ( 'NONE', ( #9860 ), #49780, .T. ) ;
#21009 = EDGE_CURVE ( 'NONE', #27444, #44984, #50450, .T. ) ;
#21010 = ORIENTED_EDGE ( 'NONE', *, *, #3322, .F. ) ;
#21011 = CARTESIAN_POINT ( 'NONE',  ( -35.00000000000000000, -8.534258022646161734, 8.699265615722952205 ) ) ;
#21012 = CYLINDRICAL_SURFACE ( 'NONE', #30827, 12.18650000000000055 ) ;
#21013 = CARTESIAN_POINT ( 'NONE',  ( -27.10113028276028402, -2.245923868550884439, 0.6639289823109628674 ) ) ;
#21014 = DIRECTION ( 'NONE',  ( 1.000000000000000000, -0.000000000000000000, -0.000000000000000000 ) ) ;
#21015 = EDGE_CURVE ( 'NONE', #18051, #1816, #31148, .T. ) ;
#21016 = B_SPLINE_CURVE_WITH_KNOTS ( 'NONE', 3,
 ( #65293, #39359, #29387, #49682, #55315, #59328, #54984, #45339, #4127, #20073, #18775, #24081, #29702, #9108, #35351, #30042, #30376, #45664, #34688, #50010, #60303, #50356 ),
 .UNSPECIFIED., .F., .F.,
 ( 4, 2, 2, 2, 2, 2, 2, 2, 2, 2, 4 ),
 ( 3.297472175031376986E-18, 0.001351328940859378202, 0.002702657881718753367, 0.004053986822578128750, 0.004729651293007815574, 0.005405315763437503265, 0.006756644704296877781, 0.007432309174726568074, 0.008107973645156257500, 0.009459302586015634617, 0.01081063152687501000 ),
 .UNSPECIFIED. ) ;
#21017 = CARTESIAN_POINT ( 'NONE',  ( 5.514624014163232779, -0.003060352188290566856, 0.002789935220458457377 ) ) ;
#21018 = ORIENTED_EDGE ( 'NONE', *, *, #3563, .F. ) ;
#21019 = CARTESIAN_POINT ( 'NONE',  ( -17.25753826526994317, -6.483132040982834354, -10.09944016160721603 ) ) ;
#21020 = B_SPLINE_CURVE_WITH_KNOTS ( 'NONE', 3,
 ( #11039, #1403, #36945, #52273, #5743, #6713, #22302, #26990, #47284, #1724, #21990, #12006, #62534, #37275, #27297, #47595 ),
 .UNSPECIFIED., .F., .F.,
 ( 4, 2, 2, 2, 2, 2, 2, 4 ),
 ( 1.636534854170084423E-17, 0.001750329107626847226, 0.002625493661440261080, 0.003500658215253675369, 0.004375822769067088357, 0.005250987322880503079, 0.006126151876693916067, 0.007001316430507330789 ),
 .UNSPECIFIED. ) ;
#21021 = EDGE_LOOP ( 'NONE', ( #22491, #8387, #3736, #21018 ) ) ;
#21022 = CARTESIAN_POINT ( 'NONE',  ( 2.368238019614975709, 0.1797502808085061909, 7.674602282635966333 ) ) ;
#21023 = DIRECTION ( 'NONE',  ( 0.000000000000000000, 0.5987040770935622147, -0.8009703041134208501 ) ) ;
#21024 = CARTESIAN_POINT ( 'NONE',  ( -35.00000000000000000, -1.771820996347237331, 11.61175578952785692 ) ) ;
#21025 = VERTEX_POINT ( 'NONE', #24498 ) ;
#21026 = CARTESIAN_POINT ( 'NONE',  ( -27.08954555554372945, -0.9924303381770539501, 2.082904663687279889 ) ) ;
#21027 = EDGE_CURVE ( 'NONE', #2404, #38332, #48164, .T. ) ;
#21028 = TOROIDAL_SURFACE ( 'NONE', #41242, 5.000000000000000888, 20.00000000000000000 ) ;
#21029 = AXIS2_PLACEMENT_3D ( 'NONE', #40591, #60883, #61856 ) ;
#21030 = DIRECTION ( 'NONE',  ( -1.000000000000000000, 0.000000000000000000, -1.224646799147353207E-16 ) ) ;
#21031 = CARTESIAN_POINT ( 'NONE',  ( 26.64924965067720564, -3.627973872667549671, 24.95916750106484727 ) ) ;
#21032 = DIRECTION ( 'NONE',  ( 1.000000000000000000, 0.000000000000000000, 0.000000000000000000 ) ) ;
#21034 = CIRCLE ( 'NONE', #58223, 1.399999999999999911 ) ;
#21033 = CARTESIAN_POINT ( 'NONE',  ( 0.2869720083484383899, -5.945302302873177958, -10.71444492121024616 ) ) ;
#21035 = CARTESIAN_POINT ( 'NONE',  ( -37.00000000000000711, 11.54110654723652196, -2.185196060783755279 ) ) ;
#21036 = DIRECTION ( 'NONE',  ( -1.000000000000000000, 0.000000000000000000, -0.000000000000000000 ) ) ;
#21037 = CARTESIAN_POINT ( 'NONE',  ( -37.00000000000000711, -3.307597835713158130, -12.31350058095526734 ) ) ;
#21038 = CIRCLE ( 'NONE', #17880, 2.899999999999995914 ) ;
#21039 = EDGE_CURVE ( 'NONE', #14797, #58117, #32565, .T. ) ;
#21040 = VERTEX_POINT ( 'NONE', #56760 ) ;
#21041 = CARTESIAN_POINT ( 'NONE',  ( -27.35552965826137140, 0.2619431035392177365, -3.094132632038957276 ) ) ;
#21042 = DIRECTION ( 'NONE',  ( 0.000000000000000000, -0.9289767198167871998, -0.3701381553399246682 ) ) ;
#21043 = EDGE_LOOP ( 'NONE', ( #3178, #5211, #62676, #50587 ) ) ;
#21044 = FACE_OUTER_BOUND ( 'NONE', #7667, .T. ) ;
#21045 = CARTESIAN_POINT ( 'NONE',  ( -35.00000000000000000, 0.000000000000000000, 0.000000000000000000 ) ) ;
#21046 = CARTESIAN_POINT ( 'NONE',  ( 2.889800649504073782, 2.156828754871545240, -5.728825117897685004 ) ) ;
#21047 = VERTEX_POINT ( 'NONE', #10504 ) ;
#21048 = CARTESIAN_POINT ( 'NONE',  ( 2.241317068080774355, -6.565357088387212769, 3.896159243838545283 ) ) ;
#21049 = DIRECTION ( 'NONE',  ( -1.000000000000000000, 0.000000000000000000, 0.000000000000000000 ) ) ;
#21050 = ORIENTED_EDGE ( 'NONE', *, *, #16447, .T. ) ;
#21051 = LINE ( 'NONE', #27681, #28537 ) ;
#21052 = ORIENTED_EDGE ( 'NONE', *, *, #50429, .F. ) ;
#21053 = ORIENTED_EDGE ( 'NONE', *, *, #34613, .T. ) ;
#21054 = CARTESIAN_POINT ( 'NONE',  ( -27.08418322526030764, -1.789041206975751086, 1.431535851194446485 ) ) ;
#21055 = CIRCLE ( 'NONE', #41378, 12.75000000000000178 ) ;
#21056 = VERTEX_POINT ( 'NONE', #51758 ) ;
#21057 = CARTESIAN_POINT ( 'NONE',  ( 1.719304012338200849, 11.38834240361387096, 5.690355757826642602 ) ) ;
#21058 = CARTESIAN_POINT ( 'NONE',  ( 0.4626703367447407289, -11.46957824750463217, -4.475905684073936186 ) ) ;
#21059 = LINE ( 'NONE', #61624, #51399 ) ;
#21060 = CARTESIAN_POINT ( 'NONE',  ( 0.5547464869798232057, -0.3049355384528142365, -12.33891836761636540 ) ) ;
#21061 = EDGE_CURVE ( 'NONE', #40629, #43273, #29405, .T. ) ;
#21062 = ORIENTED_EDGE ( 'NONE', *, *, #28999, .T. ) ;
#21063 = CARTESIAN_POINT ( 'NONE',  ( 2.655192694323322389, 8.010337395400600968, -5.293797899976643073 ) ) ;
#21064 = CARTESIAN_POINT ( 'NONE',  ( -5.484316184572717745, -28.21670571277722672, 11.61674069750055160 ) ) ;
#21065 = CARTESIAN_POINT ( 'NONE',  ( 23.47699541227554931, -4.305096618431536015, -12.79908688602327516 ) ) ;
#21067 = ORIENTED_EDGE ( 'NONE', *, *, #38814, .T. ) ;
#21066 = CARTESIAN_POINT ( 'NONE',  ( 0.2653141617321017054, -12.05243138604824260, -2.169890202573318216 ) ) ;
#21068 = ADVANCED_FACE ( 'NONE', ( #1211 ), #41093, .T. ) ;
#21069 = CARTESIAN_POINT ( 'NONE',  ( 0.3665391374699467075, -11.62960183138730130, 3.952034409876258092 ) ) ;
#21070 = ORIENTED_EDGE ( 'NONE', *, *, #23872, .T. ) ;
#21071 = CARTESIAN_POINT ( 'NONE',  ( -22.71097035706202405, 4.089776368546564456, 2.846599994298306679 ) ) ;
#21072 = ORIENTED_EDGE ( 'NONE', *, *, #9051, .T. ) ;
#21073 = EDGE_LOOP ( 'NONE', ( #50866, #64765, #27390, #11539 ) ) ;
#21074 = DIRECTION ( 'NONE',  ( 0.000000000000000000, 0.01356324068817992175, -0.9999080150203990547 ) ) ;
#21075 = DIRECTION ( 'NONE',  ( -1.000000000000000000, 0.000000000000000000, 0.000000000000000000 ) ) ;
#21076 = AXIS2_PLACEMENT_3D ( 'NONE', #36479, #56792, #11213 ) ;
#21077 = CARTESIAN_POINT ( 'NONE',  ( 2.258463476536644254, -7.638896687393373242, -0.1358786215988950219 ) ) ;
#21078 = ORIENTED_EDGE ( 'NONE', *, *, #53041, .T. ) ;
#21079 = ADVANCED_FACE ( 'NONE', ( #42074 ), #62054, .T. ) ;
#21080 = DIRECTION ( 'NONE',  ( 1.000000000000000000, 0.000000000000000000, 0.000000000000000000 ) ) ;
#21081 = CARTESIAN_POINT ( 'NONE',  ( 1.020182472821638431, -2.608319446514638873, 12.22263240120507355 ) ) ;
#21083 = CARTESIAN_POINT ( 'NONE',  ( -17.83419946441818027, -9.720786832536937538, -9.367833439828872955 ) ) ;
#21082 = B_SPLINE_CURVE_WITH_KNOTS ( 'NONE', 3,
 ( #40474, #51134, #60772, #24874, #15530, #35798 ),
 .UNSPECIFIED., .F., .F.,
 ( 4, 2, 4 ),
 ( 0.0002637379172192671714, 0.0009975831966643365287, 0.001731428476109405940 ),
 .UNSPECIFIED. ) ;
#21084 = ORIENTED_EDGE ( 'NONE', *, *, #19337, .T. ) ;
#21085 = CIRCLE ( 'NONE', #58263, 7.938172270156617749 ) ;
#21086 = AXIS2_PLACEMENT_3D ( 'NONE', #9135, #39063, #48737 ) ;
#21087 = ORIENTED_EDGE ( 'NONE', *, *, #41952, .F. ) ;
#21088 = CARTESIAN_POINT ( 'NONE',  ( -25.42680463514452427, -3.188632951113941516, -2.219378695194090145 ) ) ;
#21089 = ORIENTED_EDGE ( 'NONE', *, *, #58278, .F. ) ;
#21090 = B_SPLINE_CURVE_WITH_KNOTS ( 'NONE', 3,
 ( #11100, #37675, #16067, #16725, #31373, #6435, #51676, #6118, #26377, #16419, #56984, #57304, #31679, #21742, #22043, #46662, #47339, #1780, #52960, #51990, #47647, #47006 ),
 .UNSPECIFIED., .F., .F.,
 ( 4, 3, 3, 3, 3, 3, 3, 4 ),
 ( 5.421010862427521568E-20, 4.449119708437187815E-05, 6.626296329540798293E-05, 8.803456484962904284E-05, 0.0001098060367612821951, 0.0001315774408628530776, 0.0001760698110411187565, 0.0001829697163287827787 ),
 .UNSPECIFIED. ) ;
#21091 = EDGE_CURVE ( 'NONE', #48838, #14758, #15498, .T. ) ;
#21092 = EDGE_CURVE ( 'NONE', #45790, #63543, #41770, .T. ) ;
#21093 = ORIENTED_EDGE ( 'NONE', *, *, #54296, .F. ) ;
#21094 = FACE_OUTER_BOUND ( 'NONE', #7427, .T. ) ;
#21095 = FACE_OUTER_BOUND ( 'NONE', #38435, .T. ) ;
#21096 = CIRCLE ( 'NONE', #60349, 12.18649999999999878 ) ;
#21097 = CARTESIAN_POINT ( 'NONE',  ( 0.000000000000000000, 5.814643797626930954, 3.550179297009575574 ) ) ;
#21098 = DIRECTION ( 'NONE',  ( 0.000000000000000000, 0.9903235168508555120, 0.1387779952735781475 ) ) ;
#21099 = CARTESIAN_POINT ( 'NONE',  ( 0.3040950598368152291, -6.347045025870692747, -10.49113473328036861 ) ) ;
#21100 = DIRECTION ( 'NONE',  ( 1.000000000000000000, 0.000000000000000000, 0.000000000000000000 ) ) ;
#21101 = CARTESIAN_POINT ( 'NONE',  ( -18.58686583997247155, 5.151216734910867068, -12.47858029384659417 ) ) ;
#21102 = ORIENTED_EDGE ( 'NONE', *, *, #35185, .F. ) ;
#21103 = CYLINDRICAL_SURFACE ( 'NONE', #62519, 1.750000000000000000 ) ;
#21104 =( NAMED_UNIT ( * ) PLANE_ANGLE_UNIT ( ) SI_UNIT ( $, .RADIAN. ) );
#21105 = CARTESIAN_POINT ( 'NONE',  ( -14.29135464769095520, 7.782112657557433089, -11.03126115115966854 ) ) ;
#21106 = CIRCLE ( 'NONE', #902, 12.75000000000000178 ) ;
#21107 = DIRECTION ( 'NONE',  ( 1.000000000000000000, 0.000000000000000000, 0.000000000000000000 ) ) ;
#21108 = AXIS2_PLACEMENT_3D ( 'NONE', #20778, #15119, #46379 ) ;
#21109 = CARTESIAN_POINT ( 'NONE',  ( 0.3040950598368144520, -9.229598020917633150, -8.072385578287565977 ) ) ;
#21110 = CARTESIAN_POINT ( 'NONE',  ( -36.00000000000000711, 8.496612874013289129, -9.506317355798284296 ) ) ;
#21111 = FACE_OUTER_BOUND ( 'NONE', #64013, .T. ) ;
#21112 = ORIENTED_EDGE ( 'NONE', *, *, #64985, .F. ) ;
#21113 = EDGE_CURVE ( 'NONE', #56624, #35302, #19050, .T. ) ;
#21114 = CARTESIAN_POINT ( 'NONE',  ( 2.963017218115626239, -0.3847317984105863009, 7.865565884553442189 ) ) ;
#21115 = DIRECTION ( 'NONE',  ( 1.000000000000000000, 0.000000000000000000, 0.000000000000000000 ) ) ;
#21116 = CARTESIAN_POINT ( 'NONE',  ( 12.62425547244847124, -33.87255953084252980, 9.995598718700033913 ) ) ;
#21117 = VECTOR ( 'NONE', #1505, 1000.000000000000000 ) ;
#21118 = VECTOR ( 'NONE', #46781, 1000.000000000000000 ) ;
#21119 = ADVANCED_FACE ( 'NONE', ( #61372 ), #37089, .T. ) ;
#21120 = CARTESIAN_POINT ( 'NONE',  ( 9.634263811864652638, 2.206861042771444126, -13.32010880124498975 ) ) ;
#21121 = CARTESIAN_POINT ( 'NONE',  ( 35.00000000000000000, 2.627174906297071733, 11.44858830469737221 ) ) ;
#21122 = VECTOR ( 'NONE', #62572, 1000.000000000000000 ) ;
#21123 = VERTEX_POINT ( 'NONE', #32096 ) ;
#21124 = CARTESIAN_POINT ( 'NONE',  ( 2.241537034860906275, -3.813147095850935919, -6.614004440763081583 ) ) ;
#21125 = DIRECTION ( 'NONE',  ( 0.000000000000000000, 0.000000000000000000, 1.000000000000000000 ) ) ;
#21126 = CARTESIAN_POINT ( 'NONE',  ( 11.41243050843482187, -29.26822538582705491, -7.243948608349865204 ) ) ;
#21127 = ORIENTED_EDGE ( 'NONE', *, *, #24164, .T. ) ;
#21128 = LINE ( 'NONE', #6846, #39760 ) ;
#21129 = CARTESIAN_POINT ( 'NONE',  ( -18.08686583997219799, 5.369856758749883774, -10.73420889163467606 ) ) ;
#21130 = DIRECTION ( 'NONE',  ( 1.000000000000000000, -0.000000000000000000, -0.000000000000000000 ) ) ;
#21131 = VECTOR ( 'NONE', #22771, 1000.000000000000227 ) ;
#21133 = ORIENTED_EDGE ( 'NONE', *, *, #42215, .F. ) ;
#21132 = DIRECTION ( 'NONE',  ( 0.000000000000000000, -0.01356324068817991828, 0.9999080150203990547 ) ) ;
#21134 = DIRECTION ( 'NONE',  ( -1.000000000000000000, 0.000000000000000000, 0.000000000000000000 ) ) ;
#21135 = ADVANCED_FACE ( 'NONE', ( #5892 ), #36448, .T. ) ;
#21136 = CARTESIAN_POINT ( 'NONE',  ( -35.00000000000000000, -10.80631716521663854, -4.603882218679666849 ) ) ;
#21137 = ORIENTED_EDGE ( 'NONE', *, *, #7443, .F. ) ;
#21138 = CARTESIAN_POINT ( 'NONE',  ( 0.1901047366177758269, -0.2738782441758274011, -11.99765584512894989 ) ) ;
#21139 = CARTESIAN_POINT ( 'NONE',  ( 37.00000000000000711, -10.59380114696464581, 7.094637218249467026 ) ) ;
#21141 = CARTESIAN_POINT ( 'NONE',  ( 23.12237510341146773, 2.549967125219239961, -11.72937603911085347 ) ) ;
#21140 =( BOUNDED_CURVE ( )  B_SPLINE_CURVE ( 3, ( #11764, #2480, #7785, #21438 ),
 .UNSPECIFIED., .F., .F. ) 
 B_SPLINE_CURVE_WITH_KNOTS ( ( 4, 4 ),
 ( 5.788101898619632202, 5.827247932393759378 ),
 .UNSPECIFIED. ) 
 CURVE ( )  GEOMETRIC_REPRESENTATION_ITEM ( )  RATIONAL_B_SPLINE_CURVE ( ( 1.000000000000000000, 0.9998723030801468514, 0.9998723030801468514, 1.000000000000000000 ) ) 
 REPRESENTATION_ITEM ( '' )  );
#21142 = FACE_OUTER_BOUND ( 'NONE', #11019, .T. ) ;
#21143 = EDGE_CURVE ( 'NONE', #26098, #15301, #47061, .T. ) ;
#21144 = CARTESIAN_POINT ( 'NONE',  ( -7.904596692198818886, 5.813930850916539050, -10.52491773401777486 ) ) ;
#21145 = EDGE_CURVE ( 'NONE', #4330, #35715, #54519, .T. ) ;
#21146 = CARTESIAN_POINT ( 'NONE',  ( -17.29244623348158783, 2.525873743887551814, 13.26159725786978960 ) ) ;
#21148 = EDGE_LOOP ( 'NONE', ( #41448, #48353, #61890, #27112 ) ) ;
#21147 = CARTESIAN_POINT ( 'NONE',  ( 0.9232167919969119785, 0.4134278310083039920, 12.45862789703291185 ) ) ;
#21149 = ADVANCED_FACE ( 'NONE', ( #59045 ), #49072, .T. ) ;
#21150 = ORIENTED_EDGE ( 'NONE', *, *, #40905, .T. ) ;
#21151 = CARTESIAN_POINT ( 'NONE',  ( 2.253265082352432280, -5.007416537586561134, 5.768060979107519692 ) ) ;
#21152 = ORIENTED_EDGE ( 'NONE', *, *, #6255, .T. ) ;
#21153 = DIRECTION ( 'NONE',  ( 1.000000000000000000, 0.000000000000000000, 0.000000000000000000 ) ) ;
#21154 = CARTESIAN_POINT ( 'NONE',  ( -2.672254813960873054, -12.91372982010632420, 3.936302266217765577 ) ) ;
#21155 = DIRECTION ( 'NONE',  ( 0.000000000000000000, -0.01356324068817998940, 0.9999080150203990547 ) ) ;
#21156 = VECTOR ( 'NONE', #19581, 1000.000000000000000 ) ;
#21157 = ADVANCED_FACE ( 'NONE', ( #64005 ), #32426, .T. ) ;
#21158 = CARTESIAN_POINT ( 'NONE',  ( -35.00000000000000000, 4.041347439435861943, 11.02904044024210428 ) ) ;
#21159 = VERTEX_POINT ( 'NONE', #17483 ) ;
#21160 = DIRECTION ( 'NONE',  ( -1.000000000000000000, 0.000000000000000000, 0.000000000000000000 ) ) ;
#21161 = CARTESIAN_POINT ( 'NONE',  ( -24.46258210065891703, -7.197801736871879186, 9.604157314396443823 ) ) ;
#21162 =( BOUNDED_SURFACE ( )  B_SPLINE_SURFACE ( 3, 1, ( 
 ( #58698, #14410 ),
 ( #59327, #34040 ),
 ( #28404, #64950 ),
 ( #18109, #54983 ) ),
 .UNSPECIFIED., .F., .F., .F. ) 
 B_SPLINE_SURFACE_WITH_KNOTS ( ( 4, 4 ),
 ( 2, 2 ),
 ( 0.000000000000000000, 1.000000000000000000 ),
 ( 0.000000000000000000, 1.000000000000000000 ),
 .UNSPECIFIED. ) 
 GEOMETRIC_REPRESENTATION_ITEM ( )  RATIONAL_B_SPLINE_SURFACE ( (
 ( 1.000000000000000000, 1.000000000000000000),
 ( 0.9942764183789327692, 0.8450855930916585379),
 ( 0.9942764183789327692, 0.8450855930916585379),
 ( 1.000000000000000000, 1.000000000000000000) ) ) 
 REPRESENTATION_ITEM ( '' )  SURFACE ( )  );
#21163 = AXIS2_PLACEMENT_3D ( 'NONE', #12346, #42589, #36648 ) ;
#21165 = ADVANCED_FACE ( 'NONE', ( #22806 ), #27439, .T. ) ;
#21164 = FACE_BOUND ( 'NONE', #11571, .T. ) ;
#21166 = VERTEX_POINT ( 'NONE', #58374 ) ;
#21167 = EDGE_LOOP ( 'NONE', ( #40979, #59266, #53240, #12056 ) ) ;
#21168 = FACE_OUTER_BOUND ( 'NONE', #43214, .T. ) ;
#21169 = VERTEX_POINT ( 'NONE', #2536 ) ;
#21170 = CARTESIAN_POINT ( 'NONE',  ( 24.44987046108744266, -9.131562448621981076, -7.790012948628247003 ) ) ;
#21171 = CARTESIAN_POINT ( 'NONE',  ( -27.10512513516277977, 0.5469390009826167187, -2.289566223068213890 ) ) ;
#21172 = CYLINDRICAL_SURFACE ( 'NONE', #11833, 7.499999999999988454 ) ;
#21173 = LINE ( 'NONE', #36477, #22045 ) ;
#21174 = CARTESIAN_POINT ( 'NONE',  ( 2.000000000000001776, 2.480520636974283821, -6.345145617221223944 ) ) ;
#21175 = CARTESIAN_POINT ( 'NONE',  ( 2.835339799623985968, -7.763739326985120925, 1.035140033450024699 ) ) ;
#21176 = EDGE_CURVE ( 'NONE', #24505, #9287, #59880, .T. ) ;
#21177 = CARTESIAN_POINT ( 'NONE',  ( -25.00000000000000355, -9.999999999999998224, 24.00000000000000000 ) ) ;
#21178 = AXIS2_PLACEMENT_3D ( 'NONE', #19599, #49537, #39862 ) ;
#21179 = VERTEX_POINT ( 'NONE', #7160 ) ;
#21180 = CARTESIAN_POINT ( 'NONE',  ( 0.4626703367445959003, -11.66326339726744976, 3.943760108616771287 ) ) ;
#21181 = B_SPLINE_CURVE_WITH_KNOTS ( 'NONE', 3,
 ( #20737, #51341, #5792, #26059, #41007, #55974, #46338, #15719, #35995, #56295 ),
 .UNSPECIFIED., .F., .F.,
 ( 4, 2, 2, 2, 4 ),
 ( 8.673617379884035472E-18, 0.002186269455787307001, 0.004372538911574607064, 0.006558808367361907560, 0.008745077823149205454 ),
 .UNSPECIFIED. ) ;
#21182 = CARTESIAN_POINT ( 'NONE',  ( -35.00000000000000000, 2.346765782874606465, -11.95840593935198903 ) ) ;
#21183 = CARTESIAN_POINT ( 'NONE',  ( 2.241537034860906275, 5.845308934728780770, 4.910958050585458423 ) ) ;
#21184 = CARTESIAN_POINT ( 'NONE',  ( -9.318060253344532029, 10.62519452515019402, -5.580531082972568946 ) ) ;
#21185 = DIRECTION ( 'NONE',  ( -1.000000000000000000, 0.000000000000000000, 0.000000000000000000 ) ) ;
#21186 = LINE ( 'NONE', #62095, #17107 ) ;
#21187 = CIRCLE ( 'NONE', #47729, 12.18650000000000055 ) ;
#21188 = DIRECTION ( 'NONE',  ( -1.000000000000000000, -0.000000000000000000, -0.000000000000000000 ) ) ;
#21189 = ORIENTED_EDGE ( 'NONE', *, *, #64229, .T. ) ;
#21190 = VERTEX_POINT ( 'NONE', #63339 ) ;
#21191 = CARTESIAN_POINT ( 'NONE',  ( 0.9232058338315058954, -10.60677148422248983, 6.559496812049624204 ) ) ;
#21192 = ORIENTED_EDGE ( 'NONE', *, *, #39590, .T. ) ;
#21193 = DIRECTION ( 'NONE',  ( 0.000000000000000000, 0.01356324068817998940, -0.9999080150203990547 ) ) ;
#21194 = CARTESIAN_POINT ( 'NONE',  ( 37.00000000000000711, 12.21925492305367200, 3.640372113593418835 ) ) ;
#21195 = CARTESIAN_POINT ( 'NONE',  ( 1.283627346226763999, -9.985833283678418937, -7.660435136228953112 ) ) ;
#21196 = FACE_OUTER_BOUND ( 'NONE', #33167, .T. ) ;
#21197 = ORIENTED_EDGE ( 'NONE', *, *, #3426, .F. ) ;
#21198 = DIRECTION ( 'NONE',  ( -1.000000000000000000, -0.000000000000000000, 0.000000000000000000 ) ) ;
#21199 = CARTESIAN_POINT ( 'NONE',  ( 2.241534463349552198, -0.005768439177821054094, -7.634462073473343935 ) ) ;
#21200 = DIRECTION ( 'NONE',  ( -1.000000000000000000, 0.000000000000000000, 0.000000000000000000 ) ) ;
#21201 = CARTESIAN_POINT ( 'NONE',  ( 2.241352910868908754, -6.652881166698485949, -3.744764251557062718 ) ) ;
#21202 = EDGE_CURVE ( 'NONE', #6107, #46339, #1509, .T. ) ;
#21203 = CIRCLE ( 'NONE', #58390, 12.75000000000000178 ) ;
#21204 = CARTESIAN_POINT ( 'NONE',  ( 2.889800649504073782, -0.9965440656173316647, -6.039722463373548678 ) ) ;
#21205 = DIRECTION ( 'NONE',  ( 0.000000000000000000, 0.01356324068817998940, -0.9999080150203989437 ) ) ;
#21206 = ORIENTED_EDGE ( 'NONE', *, *, #39019, .T. ) ;
#21207 = CIRCLE ( 'NONE', #25442, 4.999999999999999112 ) ;
#21208 = LINE ( 'NONE', #16233, #12674 ) ;
#21209 = VERTEX_POINT ( 'NONE', #48078 ) ;
#21210 = CARTESIAN_POINT ( 'NONE',  ( 22.36482863261543486, -13.46837713145126791, -0.9234811557364140944 ) ) ;
#21211 = CYLINDRICAL_SURFACE ( 'NONE', #31005, 5.000000000000000888 ) ;
#21212 = DIRECTION ( 'NONE',  ( -1.000000000000000000, 0.000000000000000000, 0.000000000000000000 ) ) ;
#21213 = CARTESIAN_POINT ( 'NONE',  ( 27.48158180005687612, -10.97080778372832199, 4.873343154589966808 ) ) ;
#21214 = CARTESIAN_POINT ( 'NONE',  ( -7.194344000760931834, -1.897124946417909408, 11.84942057751005251 ) ) ;
#21215 = AXIS2_PLACEMENT_3D ( 'NONE', #10267, #45513, #5298 ) ;
#21216 = EDGE_CURVE ( 'NONE', #53854, #26580, #43060, .T. ) ;
#21217 = ORIENTED_EDGE ( 'NONE', *, *, #5842, .T. ) ;
#21218 = ORIENTED_EDGE ( 'NONE', *, *, #42958, .T. ) ;
#21219 = CARTESIAN_POINT ( 'NONE',  ( 1.719304012339844867, -11.38834240361479644, 5.690355757826019989 ) ) ;
#21220 = ORIENTED_EDGE ( 'NONE', *, *, #64279, .T. ) ;
#21221 = VECTOR ( 'NONE', #11404, 1000.000000000000000 ) ;
#21222 = CARTESIAN_POINT ( 'NONE',  ( 37.00000000000000711, 1.030638227056565270, -12.14284015767850633 ) ) ;
#21223 = CARTESIAN_POINT ( 'NONE',  ( 35.00000000000000000, 4.705694406421931860E-17, -3.469127814946512892E-15 ) ) ;
#21224 = CARTESIAN_POINT ( 'NONE',  ( -22.27718112499583469, -3.412978993569796504, -1.380338971069148712 ) ) ;
#21225 = CARTESIAN_POINT ( 'NONE',  ( 0.3675815128205912052, 9.235491948680007113, 8.093875121226108860 ) ) ;
#21226 = CARTESIAN_POINT ( 'NONE',  ( -47.00000000000000711, 0.000000000000000000, 0.000000000000000000 ) ) ;
#21227 = EDGE_CURVE ( 'NONE', #49976, #8685, #25888, .T. ) ;
#21228 = DIRECTION ( 'NONE',  ( 0.000000000000000000, -1.000000000000000000, 0.000000000000000000 ) ) ;
#21229 = CARTESIAN_POINT ( 'NONE',  ( 37.00000000000000711, -0.4871980014160605665, 12.74068829017554094 ) ) ;
#21230 = VERTEX_POINT ( 'NONE', #8154 ) ;
#21231 = EDGE_CURVE ( 'NONE', #63997, #40547, #47112, .T. ) ;
#21232 = DIRECTION ( 'NONE',  ( 0.000000000000000000, 0.000000000000000000, 1.000000000000000000 ) ) ;
#21233 = AXIS2_PLACEMENT_3D ( 'NONE', #53892, #3366, #23634 ) ;
#21234 = EDGE_LOOP ( 'NONE', ( #58962, #33196, #18803, #12638 ) ) ;
#21235 = CARTESIAN_POINT ( 'NONE',  ( 35.00000000000000000, -2.968224442958486975, -11.81949347079746282 ) ) ;
#21236 = DIRECTION ( 'NONE',  ( -1.000000000000000000, 0.000000000000000000, 0.000000000000000000 ) ) ;
#21237 = ORIENTED_EDGE ( 'NONE', *, *, #11498, .F. ) ;
#21238 = DIRECTION ( 'NONE',  ( -1.000000000000000000, 0.000000000000000000, 0.000000000000000000 ) ) ;
#21239 = CARTESIAN_POINT ( 'NONE',  ( -16.81745777873098291, -34.49999999816794372, 5.267778333666917945 ) ) ;
#21240 = ORIENTED_EDGE ( 'NONE', *, *, #2823, .T. ) ;
#21241 = FACE_OUTER_BOUND ( 'NONE', #64028, .T. ) ;
#21242 = CARTESIAN_POINT ( 'NONE',  ( 36.00000000000000711, 3.805206332242470957, -12.16893194857551563 ) ) ;
#21244 = EDGE_CURVE ( 'NONE', #29440, #36589, #16691, .T. ) ;
#21243 = CARTESIAN_POINT ( 'NONE',  ( 2.844750968616052145, 2.990088422897422049, 7.242618984642885671 ) ) ;
#21245 = ORIENTED_EDGE ( 'NONE', *, *, #7567, .F. ) ;
#21246 = ORIENTED_EDGE ( 'NONE', *, *, #485, .F. ) ;
#21247 = CARTESIAN_POINT ( 'NONE',  ( -35.00000000000000000, 1.039216533673073206, -11.70009620280410445 ) ) ;
#21249 = ORIENTED_EDGE ( 'NONE', *, *, #12055, .T. ) ;
#21248 = EDGE_CURVE ( 'NONE', #52121, #39182, #53047, .T. ) ;
#21250 = CARTESIAN_POINT ( 'NONE',  ( 37.00000000000000711, 11.17622378668006355, -3.614449339633533764 ) ) ;
#21251 = ORIENTED_EDGE ( 'NONE', *, *, #35626, .F. ) ;
#21252 = ORIENTED_EDGE ( 'NONE', *, *, #32937, .T. ) ;
#21254 = EDGE_CURVE ( 'NONE', #58567, #52575, #15238, .T. ) ;
#21253 = VERTEX_POINT ( 'NONE', #28424 ) ;
#21255 = CARTESIAN_POINT ( 'NONE',  ( 0.2671309869109498303, 4.340541005679527942, 11.45180222993656294 ) ) ;
#21256 = CARTESIAN_POINT ( 'NONE',  ( 35.00000000000000000, -10.32377448871663006, 6.475373545682407972 ) ) ;
#21257 = CIRCLE ( 'NONE', #56282, 12.75000000000000178 ) ;
#21259 = AXIS2_PLACEMENT_3D ( 'NONE', #6166, #26428, #23332 ) ;
#21258 = CARTESIAN_POINT ( 'NONE',  ( 2.000000000000001776, -3.805198749487401777, -5.799611601383285020 ) ) ;
#21260 = LINE ( 'NONE', #62161, #4361 ) ;
#21261 = CARTESIAN_POINT ( 'NONE',  ( -35.00000000000000000, 6.753013023069858178, -10.14433819232427147 ) ) ;
#21262 = VERTEX_POINT ( 'NONE', #43724 ) ;
#21263 = ADVANCED_FACE ( 'NONE', ( #38744 ), #8475, .T. ) ;
#21264 = LINE ( 'NONE', #41538, #39645 ) ;
#21265 = ORIENTED_EDGE ( 'NONE', *, *, #9356, .T. ) ;
#21266 = DIRECTION ( 'NONE',  ( 0.000000000000000000, 0.2149704402110246548, -0.9766205557100865464 ) ) ;
#21267 = CARTESIAN_POINT ( 'NONE',  ( -27.10113028276028757, 0.6639289823109749689, 2.245923868550868896 ) ) ;
#21268 = ADVANCED_FACE ( 'NONE', ( #4494 ), #45358, .T. ) ;
#21269 = DIRECTION ( 'NONE',  ( 0.000000000000000000, 0.000000000000000000, -1.000000000000000000 ) ) ;
#21270 = DIRECTION ( 'NONE',  ( -1.000000000000000000, -0.000000000000000000, -0.000000000000000000 ) ) ;
#21271 = CARTESIAN_POINT ( 'NONE',  ( 2.305787727787083519, 6.711944854845874886, -3.682701754025442753 ) ) ;
#21272 = CARTESIAN_POINT ( 'NONE',  ( 2.305787727787083519, -7.654065630109506913, -0.1666591538753489643 ) ) ;
#21273 = CIRCLE ( 'NONE', #37160, 12.18649999999999878 ) ;
#21274 = ORIENTED_EDGE ( 'NONE', *, *, #14531, .T. ) ;
#21275 = DIRECTION ( 'NONE',  ( -1.000000000000000000, 0.000000000000000000, 0.000000000000000000 ) ) ;
#21276 = CIRCLE ( 'NONE', #42466, 5.000000000000001776 ) ;
#21277 = EDGE_LOOP ( 'NONE', ( #407, #23384, #33075, #58846 ) ) ;
#21278 = CARTESIAN_POINT ( 'NONE',  ( 1.719304012338833676, 5.066286238785588480, 11.67935079956406597 ) ) ;
#21279 = CARTESIAN_POINT ( 'NONE',  ( 5.446351735594772592, -26.05211744559319342, -15.16580142939698028 ) ) ;
#21280 = DIRECTION ( 'NONE',  ( 1.000000000000000000, -0.000000000000000000, 0.000000000000000000 ) ) ;
#21281 = CARTESIAN_POINT ( 'NONE',  ( -27.08485414902839494, -0.5952588087544560258, -2.214586389210155382 ) ) ;
#21282 = CARTESIAN_POINT ( 'NONE',  ( -35.05012975565874456, -0.01377677982613203199, 0.002073729464861247002 ) ) ;
#21283 = VERTEX_POINT ( 'NONE', #64639 ) ;
#21284 = DIRECTION ( 'NONE',  ( 0.000000000000000000, 0.01356324068817992175, -0.9999080150203990547 ) ) ;
#21286 = AXIS2_PLACEMENT_3D ( 'NONE', #32291, #57921, #20999 ) ;
#21285 = DIRECTION ( 'NONE',  ( -1.000000000000000000, 0.000000000000000000, 0.000000000000000000 ) ) ;
#21287 = B_SPLINE_CURVE_WITH_KNOTS ( 'NONE', 3,
 ( #26321, #11353, #36944, #46291, #31624, #62221, #21329, #11673, #1060, #61897, #52603, #20990, #41272, #7026, #1401, #16356 ),
 .UNSPECIFIED., .F., .F.,
 ( 4, 3, 3, 3, 3, 4 ),
 ( 0.000000000000000000, 0.0003017745587525229160, 0.0006035491769808713552, 0.0009053241094668132124, 0.001207275924541012383, 0.001510325902535034634 ),
 .UNSPECIFIED. ) ;
#21288 = CARTESIAN_POINT ( 'NONE',  ( 2.655192694323996072, 2.234846078477681353, 9.337840456948278245 ) ) ;
#21289 = DIRECTION ( 'NONE',  ( 0.000000000000000000, 0.2149704402110178825, 0.9766205557100882118 ) ) ;
#21290 = EDGE_CURVE ( 'NONE', #27894, #23892, #55601, .T. ) ;
#21291 = AXIS2_PLACEMENT_3D ( 'NONE', #5910, #11512, #62070 ) ;
#21292 = CARTESIAN_POINT ( 'NONE',  ( 0.3675815128205894289, 12.27743992903066328, -0.2638082659428851451 ) ) ;
#21293 = CARTESIAN_POINT ( 'NONE',  ( 0.3665391374699465965, -4.447929964102771194, -11.44911061034390976 ) ) ;
#21294 = CIRCLE ( 'NONE', #6452, 4.999999999999999112 ) ;
#21295 = CARTESIAN_POINT ( 'NONE',  ( 0.2653141334712576516, -2.083134085643126188, 12.06772877558522516 ) ) ;
#21296 = DIRECTION ( 'NONE',  ( 0.000000000000000000, 0.01356324068817992175, -0.9999080150203990547 ) ) ;
#21297 = CARTESIAN_POINT ( 'NONE',  ( 2.298277635560277865, 0.1650558796845167375, -7.651596582281724679 ) ) ;
#21298 = ADVANCED_FACE ( 'NONE', ( #18796 ), #19112, .T. ) ;
#21299 = AXIS2_PLACEMENT_3D ( 'NONE', #44503, #38891, #9931 ) ;
#21300 = AXIS2_PLACEMENT_3D ( 'NONE', #41893, #56548, #10989 ) ;
#21301 = CIRCLE ( 'NONE', #44644, 12.75000000000000178 ) ;
#21302 = EDGE_CURVE ( 'NONE', #59550, #3889, #13495, .T. ) ;
#21303 = ORIENTED_EDGE ( 'NONE', *, *, #14302, .F. ) ;
#21304 = ORIENTED_EDGE ( 'NONE', *, *, #48457, .F. ) ;
#21305 = CARTESIAN_POINT ( 'NONE',  ( 0.2653141617321003176, 2.083144498805272526, 12.06772699408309535 ) ) ;
#21306 = CARTESIAN_POINT ( 'NONE',  ( 43.07244751019904072, -1.315220855092162688, 15.87097690372581837 ) ) ;
#21307 = CARTESIAN_POINT ( 'NONE',  ( 2.305787727787084407, -4.792270232040933386, 5.970480882365206909 ) ) ;
#21308 = CARTESIAN_POINT ( 'NONE',  ( -35.00000000000000000, -5.300372733891723698, 11.59605747147784882 ) ) ;
#21309 = ORIENTED_EDGE ( 'NONE', *, *, #1365, .T. ) ;
#21310 = ADVANCED_FACE ( 'NONE', ( #20093 ), #54381, .T. ) ;
#21311 = EDGE_LOOP ( 'NONE', ( #48155, #63133, #34438, #52631 ) ) ;
#21312 = ORIENTED_EDGE ( 'NONE', *, *, #42910, .T. ) ;
#21313 = CARTESIAN_POINT ( 'NONE',  ( -16.21117406328131949, -35.00000000000000000, 4.142385751841757724 ) ) ;
#21314 = VECTOR ( 'NONE', #6785, 1000.000000000000000 ) ;
#21315 = VECTOR ( 'NONE', #52919, 1000.000000000000000 ) ;
#21316 = ORIENTED_EDGE ( 'NONE', *, *, #17573, .F. ) ;
#21317 = CARTESIAN_POINT ( 'NONE',  ( -17.16690145660755817, 3.059820691759368660, -11.60420365748035643 ) ) ;
#21318 = AXIS2_PLACEMENT_3D ( 'NONE', #60052, #19491, #9819 ) ;
#21319 = CIRCLE ( 'NONE', #35108, 5.000000000000000000 ) ;
#21320 = LINE ( 'NONE', #61889, #4541 ) ;
#21321 = ORIENTED_EDGE ( 'NONE', *, *, #4211, .F. ) ;
#21322 = CYLINDRICAL_SURFACE ( 'NONE', #43882, 4.999999999999999112 ) ;
#21323 = CARTESIAN_POINT ( 'NONE',  ( 9.349182579143132443, -29.24123260035265659, -11.20990699596419127 ) ) ;
#21324 = CARTESIAN_POINT ( 'NONE',  ( 2.253265082353312021, 7.132841660186906019, 2.732639326787329903 ) ) ;
#21325 = ORIENTED_EDGE ( 'NONE', *, *, #57047, .T. ) ;
#21326 = AXIS2_PLACEMENT_3D ( 'NONE', #59310, #19739, #9734 ) ;
#21327 = DIRECTION ( 'NONE',  ( -1.000000000000000000, 0.000000000000000000, 0.000000000000000000 ) ) ;
#21328 = ORIENTED_EDGE ( 'NONE', *, *, #47322, .F. ) ;
#21329 = CARTESIAN_POINT ( 'NONE',  ( 0.9232167919969098691, 7.691547553333252019, -9.809608956680790470 ) ) ;
#21330 = AXIS2_PLACEMENT_3D ( 'NONE', #26917, #47216, #57514 ) ;
#21331 = CARTESIAN_POINT ( 'NONE',  ( -35.00000000000000000, -6.584150480049623333, 10.25474254703950905 ) ) ;
#21332 = EDGE_CURVE ( 'NONE', #8491, #45959, #50348, .T. ) ;
#21333 = CARTESIAN_POINT ( 'NONE',  ( 0.2646305136544072623, -11.46223899740597396, -4.312539723326246133 ) ) ;
#21334 = CYLINDRICAL_SURFACE ( 'NONE', #17748, 4.999999999999999112 ) ;
#21335 = DIRECTION ( 'NONE',  ( -1.000000000000000000, 0.000000000000000000, 0.000000000000000000 ) ) ;
#21336 = DIRECTION ( 'NONE',  ( 0.000000000000000000, -0.01356324068817991828, 0.9999080150203990547 ) ) ;
#21337 = CARTESIAN_POINT ( 'NONE',  ( 25.00000000000000355, -30.00000000000000000, 1.530808498934191521E-15 ) ) ;
#21338 = CARTESIAN_POINT ( 'NONE',  ( 0.2652384529303112304, 4.250461213012543205, 11.48485968917275279 ) ) ;
#21340 = ORIENTED_EDGE ( 'NONE', *, *, #5818, .T. ) ;
#21339 = CARTESIAN_POINT ( 'NONE',  ( -18.00928138223606467, 3.265590404870133412, -13.10068440056983796 ) ) ;
#21341 = EDGE_CURVE ( 'NONE', #46591, #43331, #18454, .T. ) ;
#21342 = FACE_OUTER_BOUND ( 'NONE', #14330, .T. ) ;
#21343 = CIRCLE ( 'NONE', #54301, 12.75000000000000178 ) ;
#21344 = ORIENTED_EDGE ( 'NONE', *, *, #53183, .T. ) ;
#21345 = FACE_OUTER_BOUND ( 'NONE', #60022, .T. ) ;
#21346 = LINE ( 'NONE', #748, #37557 ) ;
#21347 = EDGE_CURVE ( 'NONE', #24059, #12311, #26929, .T. ) ;
#21348 = AXIS2_PLACEMENT_3D ( 'NONE', #47084, #21818, #46737 ) ;
#21349 = VERTEX_POINT ( 'NONE', #49407 ) ;
#21350 = CARTESIAN_POINT ( 'NONE',  ( 37.00000000000000711, 10.80631716521673447, 4.603882218679430594 ) ) ;
#21351 = CARTESIAN_POINT ( 'NONE',  ( 0.7446945582530255514, 11.77484212699407884, -3.906659168236647606 ) ) ;
#21352 = CARTESIAN_POINT ( 'NONE',  ( 3.152665057734040488, 0.000000000000000000, 0.000000000000000000 ) ) ;
#21353 = CARTESIAN_POINT ( 'NONE',  ( -35.04643116707788408, 0.008094444324494021181, 0.009112266603801891240 ) ) ;
#21354 = FACE_OUTER_BOUND ( 'NONE', #43551, .T. ) ;
#21355 = AXIS2_PLACEMENT_3D ( 'NONE', #13756, #54990, #54361 ) ;
#21356 = CIRCLE ( 'NONE', #8586, 14.99999999999998757 ) ;
#21357 = ORIENTED_EDGE ( 'NONE', *, *, #28011, .F. ) ;
#21358 = CARTESIAN_POINT ( 'NONE',  ( -17.57571841026333459, -9.333537370853115078, -7.571081700497278355 ) ) ;
#21359 =( BOUNDED_SURFACE ( )  B_SPLINE_SURFACE ( 3, 1, ( 
 ( #61013, #46692 ),
 ( #11129, #62303 ),
 ( #37028, #11437 ),
 ( #50711, #10137 ) ),
 .UNSPECIFIED., .F., .F., .F. ) 
 B_SPLINE_SURFACE_WITH_KNOTS ( ( 4, 4 ),
 ( 2, 2 ),
 ( 0.000000000000000000, 1.000000000000000000 ),
 ( 0.000000000000000000, 1.000000000000000000 ),
 .UNSPECIFIED. ) 
 GEOMETRIC_REPRESENTATION_ITEM ( )  RATIONAL_B_SPLINE_SURFACE ( (
 ( 1.000000000000000000, 1.000000000000000000),
 ( 0.9942764183789327692, 0.8450855930916580938),
 ( 0.9942764183789327692, 0.8450855930916580938),
 ( 1.000000000000000000, 1.000000000000000000) ) ) 
 REPRESENTATION_ITEM ( '' )  SURFACE ( )  );
#21360 = AXIS2_PLACEMENT_3D ( 'NONE', #42671, #18088, #18755 ) ;
#21361 = VERTEX_POINT ( 'NONE', #4823 ) ;
#21362 = FACE_OUTER_BOUND ( 'NONE', #62275, .T. ) ;
#21363 = CYLINDRICAL_SURFACE ( 'NONE', #46228, 7.499999999999988454 ) ;
#21364 = PLANE ( 'NONE',  #10545 ) ;
#21365 = ORIENTED_EDGE ( 'NONE', *, *, #8664, .T. ) ;
#21366 = CARTESIAN_POINT ( 'NONE',  ( -35.00000000000000000, -6.102719229070750373, 10.54834585426218041 ) ) ;
#21367 = AXIS2_PLACEMENT_3D ( 'NONE', #61388, #10518, #11831 ) ;
#21368 = AXIS2_PLACEMENT_3D ( 'NONE', #29621, #45264, #65213 ) ;
#21369 = EDGE_CURVE ( 'NONE', #27612, #48877, #52432, .T. ) ;
#21370 = CIRCLE ( 'NONE', #17104, 12.18650000000000411 ) ;
#21371 = EDGE_CURVE ( 'NONE', #27786, #49417, #10326, .T. ) ;
#21372 = CARTESIAN_POINT ( 'NONE',  ( -35.00000000000000000, 8.699265615722982403, 8.534258022646129760 ) ) ;
#21373 = DIRECTION ( 'NONE',  ( 0.000000000000000000, -0.01356324068817992175, 0.9999080150203990547 ) ) ;
#21374 = AXIS2_PLACEMENT_3D ( 'NONE', #17155, #17492, #30875 ) ;
#21375 = CARTESIAN_POINT ( 'NONE',  ( -35.00000000000000000, 11.96656215839369075, 4.400442035670987018 ) ) ;
#21376 = DIRECTION ( 'NONE',  ( -0.000000000000000000, -0.000000000000000000, -1.000000000000000000 ) ) ;
#21377 = FACE_OUTER_BOUND ( 'NONE', #4965, .T. ) ;
#21378 = CYLINDRICAL_SURFACE ( 'NONE', #36774, 12.74999999999999822 ) ;
#21379 = CARTESIAN_POINT ( 'NONE',  ( -17.83419946441818027, -9.720786832536937538, -7.036071585506806336 ) ) ;
#21380 = AXIS2_PLACEMENT_3D ( 'NONE', #12836, #42761, #47770 ) ;
#21381 = EDGE_CURVE ( 'NONE', #41515, #44894, #54707, .T. ) ;
#21382 = ORIENTED_EDGE ( 'NONE', *, *, #64985, .T. ) ;
#21383 = CARTESIAN_POINT ( 'NONE',  ( 5.514970785353741078, -0.004694330894494713573, -0.0005190732562554920817 ) ) ;
#21384 = CARTESIAN_POINT ( 'NONE',  ( 0.3675815128205912052, -12.27743992903065973, -0.2638082659429707988 ) ) ;
#21385 = CIRCLE ( 'NONE', #17165, 7.499999999999988454 ) ;
#21386 = EDGE_LOOP ( 'NONE', ( #35555, #3657, #7073, #14119 ) ) ;
#21387 = CARTESIAN_POINT ( 'NONE',  ( 5.536195898058073439, 0.008323005098840532620, 0.001726268814999744761 ) ) ;
#21388 = CARTESIAN_POINT ( 'NONE',  ( -22.27721688985630522, 3.446999288411551898, 1.293557211780032246 ) ) ;
#21389 = CARTESIAN_POINT ( 'NONE',  ( 9.586060201835508110, 6.684527016188011039, -9.971514917006311762 ) ) ;
#21390 = ORIENTED_EDGE ( 'NONE', *, *, #55111, .T. ) ;
#21391 = AXIS2_PLACEMENT_3D ( 'NONE', #3779, #39306, #24343 ) ;
#21392 = CARTESIAN_POINT ( 'NONE',  ( 26.17141335727527007, -13.01134923558396572, 3.602278675730974378 ) ) ;
#21393 = CARTESIAN_POINT ( 'NONE',  ( -35.05175862995318425, -0.01253051761586874979, 0.001087818442104329653 ) ) ;
#21394 = ORIENTED_EDGE ( 'NONE', *, *, #46981, .F. ) ;
#21395 = ADVANCED_FACE ( 'NONE', ( #4152 ), #24416, .T. ) ;
#21396 = EDGE_CURVE ( 'NONE', #36553, #14035, #26077, .T. ) ;
#21397 = DIRECTION ( 'NONE',  ( 0.000000000000000000, -0.01356324068817991828, 0.9999080150203990547 ) ) ;
#21398 = VERTEX_POINT ( 'NONE', #51684 ) ;
#21399 = ORIENTED_EDGE ( 'NONE', *, *, #48292, .T. ) ;
#21400 = EDGE_CURVE ( 'NONE', #17474, #52157, #43922, .T. ) ;
#21401 = VECTOR ( 'NONE', #55494, 1000.000000000000000 ) ;
#21402 = CARTESIAN_POINT ( 'NONE',  ( -27.08423805673873375, -1.665498649074237836, 1.573803011992709111 ) ) ;
#21403 = AXIS2_PLACEMENT_3D ( 'NONE', #44414, #2916, #18550 ) ;
#21404 = ORIENTED_EDGE ( 'NONE', *, *, #4374, .T. ) ;
#21405 = DIRECTION ( 'NONE',  ( 0.000000000000000000, -0.01356324068817991828, 0.9999080150203990547 ) ) ;
#21406 = CARTESIAN_POINT ( 'NONE',  ( 1.287602823387594020, -11.62763122279993233, -4.819820779360301621 ) ) ;
#21407 = CARTESIAN_POINT ( 'NONE',  ( -35.00000000000000000, 0.000000000000000000, 0.000000000000000000 ) ) ;
#21408 = CYLINDRICAL_SURFACE ( 'NONE', #16304, 4.000000000000000000 ) ;
#21409 = EDGE_LOOP ( 'NONE', ( #18974, #45679, #47843, #15253 ) ) ;
#21410 = CARTESIAN_POINT ( 'NONE',  ( 34.38695973621796043, 25.00000000000000000, 3.530690241644829364 ) ) ;
#21411 = CARTESIAN_POINT ( 'NONE',  ( 9.079541994506246994, -32.62122108031978485, 12.39463523794014321 ) ) ;
#21412 = CARTESIAN_POINT ( 'NONE',  ( -10.00000000000000178, 0.000000000000000000, 0.000000000000000000 ) ) ;
#21414 = EDGE_LOOP ( 'NONE', ( #35786, #27169, #16098, #32344 ) ) ;
#21413 = CARTESIAN_POINT ( 'NONE',  ( 2.941278708680199916, -4.048809123187903758, -4.615461433467297425 ) ) ;
#21415 = DIRECTION ( 'NONE',  ( 1.000000000000000000, 0.000000000000000000, -0.000000000000000000 ) ) ;
#21416 = VERTEX_POINT ( 'NONE', #56674 ) ;
#21417 = DIRECTION ( 'NONE',  ( 1.000000000000000000, 0.000000000000000000, 0.000000000000000000 ) ) ;
#21418 = ORIENTED_EDGE ( 'NONE', *, *, #57887, .T. ) ;
#21419 = CARTESIAN_POINT ( 'NONE',  ( 35.00000000000000000, 11.86701198550355940, -2.772148766916162188 ) ) ;
#21420 = AXIS2_PLACEMENT_3D ( 'NONE', #49424, #19471, #24783 ) ;
#21421 = FACE_OUTER_BOUND ( 'NONE', #55018, .T. ) ;
#21422 = EDGE_CURVE ( 'NONE', #62530, #20687, #21750, .T. ) ;
#21423 = CARTESIAN_POINT ( 'NONE',  ( -35.00000000000000000, 0.7214809346828596759, 11.72397916322012712 ) ) ;
#21424 = CIRCLE ( 'NONE', #58611, 12.18649999999999878 ) ;
#21425 = VERTEX_POINT ( 'NONE', #32019 ) ;
#21426 = CARTESIAN_POINT ( 'NONE',  ( -22.27706485742869091, 3.662257305743817692, -0.3729136217355926153 ) ) ;
#21427 = CARTESIAN_POINT ( 'NONE',  ( 1.375507693217718597, -2.770709900325616371, 12.30831170622558446 ) ) ;
#21428 = DIRECTION ( 'NONE',  ( 1.000000000000000000, 0.000000000000000000, 0.000000000000000000 ) ) ;
#21430 = ORIENTED_EDGE ( 'NONE', *, *, #22766, .T. ) ;
#21429 = AXIS2_PLACEMENT_3D ( 'NONE', #33481, #37807, #58102 ) ;
#21431 = EDGE_CURVE ( 'NONE', #37186, #3067, #8883, .T. ) ;
#21432 = VERTEX_POINT ( 'NONE', #45684 ) ;
#21433 = DIRECTION ( 'NONE',  ( 0.9582930651793755139, -0.2370079598497639439, 0.1596922922278021517 ) ) ;
#21434 = EDGE_LOOP ( 'NONE', ( #27670, #37765, #46661, #25464 ) ) ;
#21435 = AXIS2_PLACEMENT_3D ( 'NONE', #19787, #40709, #9786 ) ;
#21436 = ORIENTED_EDGE ( 'NONE', *, *, #4315, .T. ) ;
#21437 = CIRCLE ( 'NONE', #50107, 12.75000000000000178 ) ;
#21438 = CARTESIAN_POINT ( 'NONE',  ( 18.84867683979356201, -5.944105725974474730, 12.12095735156416509 ) ) ;
#21439 = CARTESIAN_POINT ( 'NONE',  ( 0.8320506296491625431, -10.57268643647778639, 6.546053790694139174 ) ) ;
#21440 = DIRECTION ( 'NONE',  ( 0.000000000000000000, 0.9970832820307037325, 0.07632122047556839928 ) ) ;
#21441 = B_SPLINE_CURVE_WITH_KNOTS ( 'NONE', 3,
 ( #58405, #64035, #19137, #38437, #14137, #58753, #33458 ),
 .UNSPECIFIED., .F., .F.,
 ( 4, 3, 4 ),
 ( 7.013569501285946009E-15, 0.002398160485434967272, 0.005002426799383816874 ),
 .UNSPECIFIED. ) ;
#21442 = DIRECTION ( 'NONE',  ( -1.000000000000000000, 0.000000000000000000, 0.000000000000000000 ) ) ;
#21443 = CARTESIAN_POINT ( 'NONE',  ( 37.00000000000000711, 9.076753354953998709, -8.954052073409638268 ) ) ;
#21444 = CARTESIAN_POINT ( 'NONE',  ( -6.754644257020094855, -1.192176639353738521, -11.94107717247141132 ) ) ;
#21445 = CARTESIAN_POINT ( 'NONE',  ( 47.00000000000000711, 4.705694406421931860E-17, -3.469127814946512892E-15 ) ) ;
#21446 = VECTOR ( 'NONE', #24444, 1000.000000000000000 ) ;
#21447 = VERTEX_POINT ( 'NONE', #20753 ) ;
#21448 = CYLINDRICAL_SURFACE ( 'NONE', #33864, 4.999999999999999112 ) ;
#21449 =( NAMED_UNIT ( * ) SI_UNIT ( $, .STERADIAN. ) SOLID_ANGLE_UNIT ( ) );
#21450 = AXIS2_PLACEMENT_3D ( 'NONE', #16496, #20820, #10840 ) ;
#21451 = CIRCLE ( 'NONE', #39474, 5.000000000000000888 ) ;
#21452 = CARTESIAN_POINT ( 'NONE',  ( 12.49336350054390365, 0.1658493928153577657, -11.99999999999999645 ) ) ;
#21453 = AXIS2_PLACEMENT_3D ( 'NONE', #60633, #15075, #35355 ) ;
#21454 = DIRECTION ( 'NONE',  ( 0.000000000000000000, 0.8276889981568920085, -0.5611870653623801664 ) ) ;
#21455 = EDGE_CURVE ( 'NONE', #15413, #2234, #41340, .T. ) ;
#21456 = CARTESIAN_POINT ( 'NONE',  ( 0.2638984909335716500, -9.252728947331023690, -8.023974293733274976 ) ) ;
#21457 = CARTESIAN_POINT ( 'NONE',  ( 3.062197852306406620, 2.793213809110397516, -11.67210648529468564 ) ) ;
#21458 = CARTESIAN_POINT ( 'NONE',  ( -35.04582288351658548, -0.006479247284611515389, -0.01092946910274314974 ) ) ;
#21459 = ORIENTED_EDGE ( 'NONE', *, *, #49992, .T. ) ;
#21460 = CARTESIAN_POINT ( 'NONE',  ( -27.08421723179412410, 0.5069555058557477789, 2.234476190936493190 ) ) ;
#21461 = CARTESIAN_POINT ( 'NONE',  ( -35.00000000000000000, 0.000000000000000000, 0.000000000000000000 ) ) ;
#21462 = DIRECTION ( 'NONE',  ( -1.000000000000000000, 0.000000000000000000, 0.000000000000000000 ) ) ;
#21463 = CARTESIAN_POINT ( 'NONE',  ( 2.000000000000001776, 6.664893814313725962, 3.439359016433505278 ) ) ;
#21464 = CIRCLE ( 'NONE', #29957, 5.000000000000000888 ) ;
#21465 = AXIS2_PLACEMENT_3D ( 'NONE', #59267, #54284, #8723 ) ;
#21466 = EDGE_CURVE ( 'NONE', #55606, #26984, #41022, .T. ) ;
#21467 = CIRCLE ( 'NONE', #53335, 5.000000000000001776 ) ;
#21468 = FACE_OUTER_BOUND ( 'NONE', #34234, .T. ) ;
#21469 = DIRECTION ( 'NONE',  ( 0.000000000000000000, 0.9651210252299785575, 0.2618041379715665973 ) ) ;
#21470 = VERTEX_POINT ( 'NONE', #26722 ) ;
#21471 = CARTESIAN_POINT ( 'NONE',  ( -27.35552965826137140, -2.548625910254533888, -1.773915698030580357 ) ) ;
#21472 = DIRECTION ( 'NONE',  ( -1.000000000000000000, 0.000000000000000000, 0.000000000000000000 ) ) ;
#21473 = CIRCLE ( 'NONE', #15096, 2.899999999999995026 ) ;
#21474 = CARTESIAN_POINT ( 'NONE',  ( -37.00000000000000711, -3.473736367725171359, -12.26766708251995475 ) ) ;
#21475 = ORIENTED_EDGE ( 'NONE', *, *, #20768, .F. ) ;
#21476 = CARTESIAN_POINT ( 'NONE',  ( 2.781367136452438604, 6.916275212954706042, 3.637318098960494073 ) ) ;
#21477 = CARTESIAN_POINT ( 'NONE',  ( -37.00000000000000711, -10.68873102412847764, 6.950793414699757200 ) ) ;
#21478 = CARTESIAN_POINT ( 'NONE',  ( 5.530133899448235191, 0.006510401266731618425, 0.01459891979722881261 ) ) ;
#21479 = EDGE_CURVE ( 'NONE', #34180, #25983, #31050, .T. ) ;
#21481 = VERTEX_POINT ( 'NONE', #46353 ) ;
#21480 = DIRECTION ( 'NONE',  ( 0.000000000000000000, 0.01356324068817992175, -0.9999080150203990547 ) ) ;
#21482 = CYLINDRICAL_SURFACE ( 'NONE', #54357, 12.18650000000000055 ) ;
#21483 = EDGE_CURVE ( 'NONE', #9921, #14030, #21059, .T. ) ;
#21484 = EDGE_CURVE ( 'NONE', #28445, #45757, #20422, .T. ) ;
#21485 = B_SPLINE_CURVE_WITH_KNOTS ( 'NONE', 3,
 ( #26943, #42203, #62186, #26286, #52562, #56554, #52230, #31905, #46898, #26605, #57540, #56894, #7296, #16315, #36593, #10996, #31586, #41564, #61854 ),
 .UNSPECIFIED., .F., .F.,
 ( 4, 3, 3, 3, 3, 3, 4 ),
 ( 9.619659766987995311E-18, 4.457896483015182738E-05, 6.639290541542450317E-05, 8.820687556479344011E-05, 0.0001100173248778969103, 0.0001545671401658147586, 0.0001830328308068583057 ),
 .UNSPECIFIED. ) ;
#21486 = DIRECTION ( 'NONE',  ( -1.000000000000000000, -0.000000000000000000, 0.000000000000000000 ) ) ;
#21487 = ORIENTED_EDGE ( 'NONE', *, *, #62040, .F. ) ;
#21488 = CARTESIAN_POINT ( 'NONE',  ( 0.3053067050349154155, -9.538004819224397579, 7.702091166065980765 ) ) ;
#21489 = AXIS2_PLACEMENT_3D ( 'NONE', #5595, #36128, #599 ) ;
#21490 = CARTESIAN_POINT ( 'NONE',  ( 35.00000000000000000, 4.705694406421931860E-17, -3.469127814946512892E-15 ) ) ;
#21491 = CARTESIAN_POINT ( 'NONE',  ( 47.00000000000000711, 4.705694406421931860E-17, -3.469127814946512892E-15 ) ) ;
#21492 = DIRECTION ( 'NONE',  ( -1.000000000000000000, 0.000000000000000000, 0.000000000000000000 ) ) ;
#21493 = CARTESIAN_POINT ( 'NONE',  ( -18.25006854224444908, -9.443202773001939221, 9.647586298549914119 ) ) ;
#21494 = CARTESIAN_POINT ( 'NONE',  ( 2.000000000000001776, -0.08317740279935835479, 7.499538753794344537 ) ) ;
#21496 = ORIENTED_EDGE ( 'NONE', *, *, #40975, .T. ) ;
#21495 = DIRECTION ( 'NONE',  ( -1.000000000000000000, -0.000000000000000000, 0.000000000000000000 ) ) ;
#21497 = EDGE_LOOP ( 'NONE', ( #64630, #27000, #10419, #55942 ) ) ;
#21498 = CARTESIAN_POINT ( 'NONE',  ( 23.98530306424479619, 2.278180183290474226, -11.78598886095566911 ) ) ;
#21499 = ORIENTED_EDGE ( 'NONE', *, *, #11622, .F. ) ;
#21500 = AXIS2_PLACEMENT_3D ( 'NONE', #12634, #62860, #27606 ) ;
#21501 = DIRECTION ( 'NONE',  ( 1.000000000000000000, 0.000000000000000000, 0.000000000000000000 ) ) ;
#21502 = CYLINDRICAL_SURFACE ( 'NONE', #62337, 2.899999999999994582 ) ;
#21503 = EDGE_CURVE ( 'NONE', #11696, #1074, #16079, .T. ) ;
#21505 = CARTESIAN_POINT ( 'NONE',  ( 5.520433897694421610, -0.007971295965052688573, -0.01278034823632013400 ) ) ;
#21504 = AXIS2_PLACEMENT_3D ( 'NONE', #64970, #34397, #64323 ) ;
#21506 = AXIS2_PLACEMENT_3D ( 'NONE', #17933, #22601, #28887 ) ;
#21507 = DIRECTION ( 'NONE',  ( -1.000000000000000000, 0.000000000000000000, 0.000000000000000000 ) ) ;
#21508 = ORIENTED_EDGE ( 'NONE', *, *, #30185, .T. ) ;
#21509 = CARTESIAN_POINT ( 'NONE',  ( -47.00000000000000711, 0.000000000000000000, 0.000000000000000000 ) ) ;
#21510 = DIRECTION ( 'NONE',  ( -1.000000000000000000, -0.000000000000000000, 0.000000000000000000 ) ) ;
#21511 = CARTESIAN_POINT ( 'NONE',  ( -22.27719443589224113, -1.139586749255966147, 3.500848524682618645 ) ) ;
#21512 = VERTEX_POINT ( 'NONE', #42001 ) ;
#21513 = ORIENTED_EDGE ( 'NONE', *, *, #47986, .T. ) ;
#21514 = DIRECTION ( 'NONE',  ( 0.3902440745007897949, -0.000000000000000000, 0.9207114435679737419 ) ) ;
#21515 = ORIENTED_EDGE ( 'NONE', *, *, #23033, .T. ) ;
#21516 = CARTESIAN_POINT ( 'NONE',  ( 22.22080425544861981, -11.93711206880059450, -1.277188082013731574 ) ) ;
#21517 = CARTESIAN_POINT ( 'NONE',  ( -22.38932658256919339, 3.361598243548654441, -2.201197575855948330 ) ) ;
#21518 = AXIS2_PLACEMENT_3D ( 'NONE', #19541, #14511, #18580 ) ;
#21519 = DIRECTION ( 'NONE',  ( -1.000000000000000000, -0.000000000000000000, -0.000000000000000000 ) ) ;
#21520 = CARTESIAN_POINT ( 'NONE',  ( 0.6473888112830253894, 12.23851338376148412, 1.823007254466997074 ) ) ;
#21521 = EDGE_CURVE ( 'NONE', #10081, #49489, #15736, .T. ) ;
#21522 = CIRCLE ( 'NONE', #52333, 2.899999999999995470 ) ;
#21523 = CARTESIAN_POINT ( 'NONE',  ( 2.000000000000001776, -0.2704997240205401221, 6.931223712253438585 ) ) ;
#21524 = CARTESIAN_POINT ( 'NONE',  ( -28.67667724226168602, -0.5419187306520707459, -1.812862320140639749 ) ) ;
#21525 = CYLINDRICAL_SURFACE ( 'NONE', #28029, 4.999999999999999112 ) ;
#21526 = ORIENTED_EDGE ( 'NONE', *, *, #48071, .F. ) ;
#21527 = AXIS2_PLACEMENT_3D ( 'NONE', #16663, #36280, #36934 ) ;
#21528 = CARTESIAN_POINT ( 'NONE',  ( 0.3675815128205912052, -11.62724744438068569, 3.951233083390429446 ) ) ;
#21529 = ORIENTED_EDGE ( 'NONE', *, *, #58231, .T. ) ;
#21530 = AXIS2_PLACEMENT_3D ( 'NONE', #4917, #40461, #35787 ) ;
#21531 = FACE_OUTER_BOUND ( 'NONE', #2589, .T. ) ;
#21532 = CARTESIAN_POINT ( 'NONE',  ( -22.70624764888619751, 4.501516772829880608, 2.702761586319117892 ) ) ;
#21533 = FACE_OUTER_BOUND ( 'NONE', #60669, .T. ) ;
#21534 = CARTESIAN_POINT ( 'NONE',  ( -35.00000000000000000, -10.01317267707891467, 6.946017217729903770 ) ) ;
#21535 = CARTESIAN_POINT ( 'NONE',  ( 5.516018279890452902, -0.006707902355169293243, 0.0009545156522407741585 ) ) ;
#21536 = CYLINDRICAL_SURFACE ( 'NONE', #40394, 250.0000000000000000 ) ;
#21537 = VERTEX_POINT ( 'NONE', #10428 ) ;
#21538 = VERTEX_POINT ( 'NONE', #51362 ) ;
#21539 = CARTESIAN_POINT ( 'NONE',  ( -36.00000000000000711, -12.71517666308948691, 0.9416912585473986574 ) ) ;
#21540 = VECTOR ( 'NONE', #56677, 1000.000000000000000 ) ;
#21541 = EDGE_CURVE ( 'NONE', #25715, #9803, #21668, .T. ) ;
#21542 = EDGE_LOOP ( 'NONE', ( #56274, #61551, #50523, #6710 ) ) ;
#21543 = CARTESIAN_POINT ( 'NONE',  ( 36.00000000000000711, 11.39945968423471534, -5.710938531231754212 ) ) ;
#21544 = FACE_OUTER_BOUND ( 'NONE', #24194, .T. ) ;
#21545 = CARTESIAN_POINT ( 'NONE',  ( 0.3665391374699464300, -3.952034409876219012, -11.62960183138731018 ) ) ;
#21546 = ADVANCED_FACE ( 'NONE', ( #16427 ), #46032, .T. ) ;
#21547 = CARTESIAN_POINT ( 'NONE',  ( 2.290907136833252533, 1.488079974905042180, -7.504812001538589961 ) ) ;
#21548 = ORIENTED_EDGE ( 'NONE', *, *, #64347, .T. ) ;
#21549 = CARTESIAN_POINT ( 'NONE',  ( 0.000000000000000000, -4.976357229393876480, 4.652926418895529714 ) ) ;
#21550 = CARTESIAN_POINT ( 'NONE',  ( 2.241449424704145876, -0.06135604983222692904, -7.634218943782393296 ) ) ;
#21551 = AXIS2_PLACEMENT_3D ( 'NONE', #35854, #10597, #5649 ) ;
#21552 = CARTESIAN_POINT ( 'NONE',  ( 0.3675815128205894289, -1.872154644482166397, 12.13672785388549613 ) ) ;
#21553 = DIRECTION ( 'NONE',  ( 0.000000000000000000, -0.01356324068817991828, 0.9999080150203990547 ) ) ;
#21554 = AXIS2_PLACEMENT_3D ( 'NONE', #34111, #23507, #43784 ) ;
#21555 = EDGE_CURVE ( 'NONE', #2528, #47268, #41822, .T. ) ;
#21556 = B_SPLINE_CURVE_WITH_KNOTS ( 'NONE', 3,
 ( #5014, #61192, #29598, #15619, #30916, #39592, #59891, #14314, #49905, #24630, #44907, #65190, #19657, #16624, #16296, #1340 ),
 .UNSPECIFIED., .F., .F.,
 ( 4, 3, 3, 3, 3, 4 ),
 ( 0.000000000000000000, 0.0002999043160757455806, 0.0005998071753051214920, 0.0008997092107374869783, 0.001204458948196641694, 0.001510329163478484364 ),
 .UNSPECIFIED. ) ;
#21557 = LINE ( 'NONE', #16565, #1245 ) ;
#21558 = CARTESIAN_POINT ( 'NONE',  ( -27.10719052120871098, 1.622102031466687189, -1.714424047991080613 ) ) ;
#21559 =( BOUNDED_CURVE ( )  B_SPLINE_CURVE ( 3, ( #24534, #10535, #65409, #19877 ),
 .UNSPECIFIED., .F., .F. ) 
 B_SPLINE_CURVE_WITH_KNOTS ( ( 4, 4 ),
 ( 4.054895942073102333, 4.098008028811909398 ),
 .UNSPECIFIED. ) 
 CURVE ( )  GEOMETRIC_REPRESENTATION_ITEM ( )  RATIONAL_B_SPLINE_CURVE ( ( 1.000000000000000000, 0.9998451183288734612, 0.9998451183288734612, 1.000000000000000000 ) ) 
 REPRESENTATION_ITEM ( '' )  );
#21560 = ORIENTED_EDGE ( 'NONE', *, *, #6676, .F. ) ;
#21561 = CARTESIAN_POINT ( 'NONE',  ( -16.21117406328131949, -35.00000000000000000, -4.142385751841763053 ) ) ;
#21562 = ORIENTED_EDGE ( 'NONE', *, *, #28431, .F. ) ;
#21563 = CARTESIAN_POINT ( 'NONE',  ( 37.00000000000000711, 4.705694406421931860E-17, -3.469127814946512892E-15 ) ) ;
#21564 = CARTESIAN_POINT ( 'NONE',  ( -35.00000000000000000, 4.986700593229701717, 10.63508530065523772 ) ) ;
#21565 = DIRECTION ( 'NONE',  ( 1.000000000000000000, 0.000000000000000000, 0.000000000000000000 ) ) ;
#21566 = EDGE_CURVE ( 'NONE', #44, #61612, #42866, .T. ) ;
#21567 = AXIS2_PLACEMENT_3D ( 'NONE', #22423, #42689, #21454 ) ;
#21568 = CYLINDRICAL_SURFACE ( 'NONE', #64680, 12.18650000000000055 ) ;
#21569 = B_SPLINE_CURVE_WITH_KNOTS ( 'NONE', 3,
 ( #13747, #44336, #49040, #44031, #38715, #13429, #14085, #39031, #38375, #8786 ),
 .UNSPECIFIED., .F., .F.,
 ( 4, 3, 3, 4 ),
 ( 1.563658610346375187E-18, 6.607638129004402147E-05, 9.911389841680390798E-05, 0.0001667630577588619318 ),
 .UNSPECIFIED. ) ;
#21570 = DIRECTION ( 'NONE',  ( 0.000000000000000000, 0.000000000000000000, 1.000000000000000000 ) ) ;
#21571 = AXIS2_PLACEMENT_3D ( 'NONE', #14189, #60083, #20168 ) ;
#21572 = VERTEX_POINT ( 'NONE', #51999 ) ;
#21573 = VERTEX_POINT ( 'NONE', #6442 ) ;
#21575 = ADVANCED_FACE ( 'NONE', ( #47015 ), #1472, .T. ) ;
#21574 = CARTESIAN_POINT ( 'NONE',  ( -35.00000000000000000, -5.391785509270885512, -10.43555801961481677 ) ) ;
#21576 = ORIENTED_EDGE ( 'NONE', *, *, #23195, .T. ) ;
#21577 = DIRECTION ( 'NONE',  ( -0.000000000000000000, -1.000000000000000000, -0.000000000000000000 ) ) ;
#21578 = DIRECTION ( 'NONE',  ( 1.000000000000000000, 0.000000000000000000, 0.000000000000000000 ) ) ;
#21579 = CARTESIAN_POINT ( 'NONE',  ( -35.00000000000000000, -1.456211999474261054, -11.65554240571058742 ) ) ;
#21580 = CARTESIAN_POINT ( 'NONE',  ( -37.00000000000000711, -4.561791185930498926, 11.90598845858532329 ) ) ;
#21581 = CARTESIAN_POINT ( 'NONE',  ( 2.781367136450317634, 7.808329083462971276, -0.3081277311318336154 ) ) ;
#21582 = AXIS2_PLACEMENT_3D ( 'NONE', #17349, #51947, #57257 ) ;
#21583 = CARTESIAN_POINT ( 'NONE',  ( -9.857392862911050102, -3.262500639785465673, 11.54921333413416207 ) ) ;
#21584 = ORIENTED_EDGE ( 'NONE', *, *, #5938, .F. ) ;
#21585 = CARTESIAN_POINT ( 'NONE',  ( 0.8320506296491628762, -5.883188144889849980, 10.95539209551944815 ) ) ;
#21586 = ORIENTED_EDGE ( 'NONE', *, *, #35984, .T. ) ;
#21587 =( NAMED_UNIT ( * ) SI_UNIT ( $, .STERADIAN. ) SOLID_ANGLE_UNIT ( ) );
#21588 = CYLINDRICAL_SURFACE ( 'NONE', #24886, 12.75000000000000178 ) ;
#21589 = LINE ( 'NONE', #6947, #52367 ) ;
#21590 = CARTESIAN_POINT ( 'NONE',  ( -47.00000000000000711, 0.000000000000000000, 0.000000000000000000 ) ) ;
#21591 = ORIENTED_EDGE ( 'NONE', *, *, #54505, .T. ) ;
#21592 = CYLINDRICAL_SURFACE ( 'NONE', #41790, 2.899999999999994582 ) ;
#21593 = CARTESIAN_POINT ( 'NONE',  ( -22.46225619532222950, 1.978788174090817309, -3.746472695305357981 ) ) ;
#21594 = CARTESIAN_POINT ( 'NONE',  ( 17.27839441901508621, 25.00000000000000000, 5.771933972472480967 ) ) ;
#21595 = EDGE_LOOP ( 'NONE', ( #58634, #65078, #52655, #28975 ) ) ;
#21596 = VERTEX_POINT ( 'NONE', #13385 ) ;
#21597 = CARTESIAN_POINT ( 'NONE',  ( -17.29244623348158783, 2.525873743887551814, -11.73115347397429176 ) ) ;
#21598 = ORIENTED_EDGE ( 'NONE', *, *, #31909, .F. ) ;
#21599 = CARTESIAN_POINT ( 'NONE',  ( 0.6473888112830222807, -11.73602097806018030, -3.920507224439204297 ) ) ;
#21600 = VERTEX_POINT ( 'NONE', #57979 ) ;
#21601 = AXIS2_PLACEMENT_3D ( 'NONE', #12972, #27597, #13304 ) ;
#21602 = VERTEX_POINT ( 'NONE', #7402 ) ;
#21603 = ORIENTED_EDGE ( 'NONE', *, *, #23268, .T. ) ;
#21604 = CARTESIAN_POINT ( 'NONE',  ( -22.27718150314433387, -2.721613812022967593, 2.479231311682832395 ) ) ;
#21605 = CARTESIAN_POINT ( 'NONE',  ( 2.298277635560100229, 5.044791616846937110, -5.755367168477931727 ) ) ;
#21606 = AXIS2_PLACEMENT_3D ( 'NONE', #2512, #32711, #42698 ) ;
#21607 = EDGE_CURVE ( 'NONE', #40174, #43224, #28022, .T. ) ;
#21608 = CIRCLE ( 'NONE', #33161, 12.18649999999999700 ) ;
#21609 = DIRECTION ( 'NONE',  ( 1.000000000000000000, 0.000000000000000000, 0.000000000000000000 ) ) ;
#21610 = CARTESIAN_POINT ( 'NONE',  ( 3.152665057734040488, 0.000000000000000000, 0.000000000000000000 ) ) ;
#21611 = DIRECTION ( 'NONE',  ( 0.000000000000000000, 0.9651210252299803338, 0.2618041379715599914 ) ) ;
#21612 = ORIENTED_EDGE ( 'NONE', *, *, #45998, .F. ) ;
#21613 = CARTESIAN_POINT ( 'NONE',  ( -37.00000000000000711, 3.307597835713245171, 12.31350058095524425 ) ) ;
#21614 = ORIENTED_EDGE ( 'NONE', *, *, #1469, .T. ) ;
#21615 = DIRECTION ( 'NONE',  ( -1.000000000000000000, -1.836970198721029688E-16, -0.000000000000000000 ) ) ;
#21617 = CARTESIAN_POINT ( 'NONE',  ( -2.897877849616106172, 12.67799309120630724, 4.651592531936545427 ) ) ;
#21616 = CIRCLE ( 'NONE', #6708, 2.899999999999994582 ) ;
#21618 = LINE ( 'NONE', #41883, #42722 ) ;
#21619 = CYLINDRICAL_SURFACE ( 'NONE', #8405, 7.499999999999988454 ) ;
#21620 = AXIS2_PLACEMENT_3D ( 'NONE', #58872, #13288, #3328 ) ;
#21621 = CARTESIAN_POINT ( 'NONE',  ( 5.516018279890452902, -0.001397286410094463784, -0.006629829924290467358 ) ) ;
#21622 = CARTESIAN_POINT ( 'NONE',  ( 0.7446945582530906105, -10.56139717223442354, -6.508900271376202085 ) ) ;
#21623 = CIRCLE ( 'NONE', #46010, 15.00000000000000000 ) ;
#21624 = EDGE_CURVE ( 'NONE', #8899, #35815, #13067, .T. ) ;
#21625 = ORIENTED_EDGE ( 'NONE', *, *, #65363, .T. ) ;
#21626 = DIRECTION ( 'NONE',  ( 0.000000000000000000, 0.000000000000000000, -1.000000000000000000 ) ) ;
#21627 = B_SPLINE_CURVE_WITH_KNOTS ( 'NONE', 3,
 ( #47462, #16545, #42426, #57776, #47140, #17192, #38110, #57430, #1592, #26839, #52117, #12194, #41800, #48453, #42773, #52772, #58421, #7199, #12506 ),
 .UNSPECIFIED., .F., .F.,
 ( 4, 3, 3, 3, 3, 3, 4 ),
 ( 4.336808689942017255E-19, 2.831840207499562487E-05, 4.217266859840527316E-05, 5.602024318396039802E-05, 6.290810167969274318E-05, 9.120440630945197459E-05, 0.0001153103026479775127 ),
 .UNSPECIFIED. ) ;
#21628 = ORIENTED_EDGE ( 'NONE', *, *, #32180, .T. ) ;
#21629 = EDGE_CURVE ( 'NONE', #49500, #19944, #53531, .T. ) ;
#21630 = CARTESIAN_POINT ( 'NONE',  ( -35.00000000000000000, 8.052525312710004712, -8.551552972816995890 ) ) ;
#21631 = CIRCLE ( 'NONE', #58811, 7.499999999999988454 ) ;
#21632 = CARTESIAN_POINT ( 'NONE',  ( 2.994568964204208150, 6.289764245798291853, -4.756002438591006687 ) ) ;
#21633 = CARTESIAN_POINT ( 'NONE',  ( -27.08850691366480135, -0.6228349286848144928, -2.218359546717751041 ) ) ;
#21634 = EDGE_CURVE ( 'NONE', #56480, #36936, #3523, .T. ) ;
#21635 = CARTESIAN_POINT ( 'NONE',  ( -27.10719052120871098, 1.962717903527675611, -1.310802520592017295 ) ) ;
#21636 = ORIENTED_EDGE ( 'NONE', *, *, #48794, .F. ) ;
#21637 = CARTESIAN_POINT ( 'NONE',  ( 2.177405672431328210, 5.005033771132237241, -10.01846874165100409 ) ) ;
#21638 = DIRECTION ( 'NONE',  ( 0.000000000000000000, -0.01356324068817992001, 0.9999080150203990547 ) ) ;
#21639 = DIRECTION ( 'NONE',  ( -1.000000000000000000, 0.000000000000000000, 0.000000000000000000 ) ) ;
#21640 = CARTESIAN_POINT ( 'NONE',  ( 0.2653141334712571520, -2.169900597054437608, -12.05242949860146418 ) ) ;
#21641 = VECTOR ( 'NONE', #26561, 1000.000000000000000 ) ;
#21642 = EDGE_CURVE ( 'NONE', #14797, #36936, #12718, .T. ) ;
#21643 = CARTESIAN_POINT ( 'NONE',  ( -20.79170840334646542, 12.91784323155722980, -3.921648409140116698 ) ) ;
#21644 = ADVANCED_FACE ( 'NONE', ( #32659 ), #7758, .T. ) ;
#21645 = CARTESIAN_POINT ( 'NONE',  ( 36.00000000000000711, 12.46157735505189201, -2.696588552979105380 ) ) ;
#21646 = CYLINDRICAL_SURFACE ( 'NONE', #10781, 4.999999999999998224 ) ;
#21647 = CARTESIAN_POINT ( 'NONE',  ( -35.00000000000000000, -6.018036132182240650, 11.24036214326518213 ) ) ;
#21648 = DIRECTION ( 'NONE',  ( 0.000000000000000000, -0.01356324068817998940, 0.9999080150203990547 ) ) ;
#21649 = AXIS2_PLACEMENT_3D ( 'NONE', #19675, #34918, #10011 ) ;
#21650 = EDGE_CURVE ( 'NONE', #25546, #14551, #62009, .T. ) ;
#21651 = AXIS2_PLACEMENT_3D ( 'NONE', #20151, #20487, #61054 ) ;
#21652 = B_SPLINE_CURVE_WITH_KNOTS ( 'NONE', 3,
 ( #48578, #3029, #38588, #22292, #58904, #62864, #37606 ),
 .UNSPECIFIED., .F., .F.,
 ( 4, 3, 4 ),
 ( 0.000000000000000000, 0.001700533616330529530, 0.005002426799371274824 ),
 .UNSPECIFIED. ) ;
#21653 = ORIENTED_EDGE ( 'NONE', *, *, #13976, .F. ) ;
#21654 = ADVANCED_FACE ( 'NONE', ( #22373 ), #17737, .T. ) ;
#21655 = ORIENTED_EDGE ( 'NONE', *, *, #455, .T. ) ;
#21657 = AXIS2_PLACEMENT_3D ( 'NONE', #39117, #50100, #13515 ) ;
#21656 = CARTESIAN_POINT ( 'NONE',  ( 2.653899356900291107, -6.596318473603853150, 4.109946795501455696 ) ) ;
#21658 = CARTESIAN_POINT ( 'NONE',  ( 48.36589927958296187, -0.3279091627047653890, -5.494672883103046246 ) ) ;
#21659 = FACE_OUTER_BOUND ( 'NONE', #47040, .T. ) ;
#21660 = VECTOR ( 'NONE', #47543, 1000.000000000000000 ) ;
#21661 = EDGE_CURVE ( 'NONE', #14466, #51562, #23811, .T. ) ;
#21662 = CARTESIAN_POINT ( 'NONE',  ( 0.2717059086739007645, -1.953280559502777347, 12.09156413799790286 ) ) ;
#21663 = VERTEX_POINT ( 'NONE', #3108 ) ;
#21664 = AXIS2_PLACEMENT_3D ( 'NONE', #11469, #56041, #1184 ) ;
#21665 = ORIENTED_EDGE ( 'NONE', *, *, #38401, .F. ) ;
#21666 = VERTEX_POINT ( 'NONE', #53314 ) ;
#21667 = CARTESIAN_POINT ( 'NONE',  ( 37.00000000000000711, -10.28547182238011715, -5.672855678558653914 ) ) ;
#21668 = CIRCLE ( 'NONE', #58859, 2.899999999999995026 ) ;
#21669 = FACE_OUTER_BOUND ( 'NONE', #29937, .T. ) ;
#21670 = EDGE_LOOP ( 'NONE', ( #34068, #36558, #1018, #24199 ) ) ;
#21671 = CARTESIAN_POINT ( 'NONE',  ( 0.2648978790185584908, -9.465406350830660287, 7.769924372105172949 ) ) ;
#21672 = CARTESIAN_POINT ( 'NONE',  ( -37.00000000000000711, 0.000000000000000000, 0.000000000000000000 ) ) ;
#21673 = ORIENTED_EDGE ( 'NONE', *, *, #44023, .F. ) ;
#21674 = CARTESIAN_POINT ( 'NONE',  ( 37.00000000000000711, -2.346765782874354667, 11.95840593935203522 ) ) ;
#21675 = AXIS2_PLACEMENT_3D ( 'NONE', #45389, #20126, #9812 ) ;
#21676 = CARTESIAN_POINT ( 'NONE',  ( 17.91771366450656444, -29.71233038866040133, -8.402389056493886343 ) ) ;
#21677 = CARTESIAN_POINT ( 'NONE',  ( 0.2646305136544065406, -10.53923716745251049, 6.237419468587042992 ) ) ;
#21678 = EDGE_LOOP ( 'NONE', ( #41438, #37417, #50484, #46817 ) ) ;
#21679 = CARTESIAN_POINT ( 'NONE',  ( 0.2956976708475498317, 12.10637007622315409, -1.911282699793599660 ) ) ;
#21680 = ORIENTED_EDGE ( 'NONE', *, *, #9327, .F. ) ;
#21681 = CARTESIAN_POINT ( 'NONE',  ( 2.000000000000001776, 0.000000000000000000, 0.000000000000000000 ) ) ;
#21682 = DIRECTION ( 'NONE',  ( 0.000000000000000000, 0.01356324068817992175, -0.9999080150203990547 ) ) ;
#21683 = CARTESIAN_POINT ( 'NONE',  ( -15.66937148611438957, -34.93011823067257637, 5.816432770872767222 ) ) ;
#21684 = DIRECTION ( 'NONE',  ( -1.000000000000000000, -0.000000000000000000, 0.000000000000000000 ) ) ;
#21685 = EDGE_CURVE ( 'NONE', #20070, #57232, #28041, .T. ) ;
#21686 = FACE_OUTER_BOUND ( 'NONE', #13009, .T. ) ;
#21687 = CARTESIAN_POINT ( 'NONE',  ( 2.034671305879856895, -10.71175679137336445, -4.647127512369300106 ) ) ;
#21688 = CARTESIAN_POINT ( 'NONE',  ( 37.00000000000000711, 0.4353888892050056802, 11.73808581813437080 ) ) ;
#21689 = CARTESIAN_POINT ( 'NONE',  ( 5.515539859299206427, -0.005336559634876962034, -0.002856745161749523441 ) ) ;
#21690 = ORIENTED_EDGE ( 'NONE', *, *, #27468, .F. ) ;
#21691 = DIRECTION ( 'NONE',  ( -0.000000000000000000, -1.000000000000000000, -0.000000000000000000 ) ) ;
#21692 = ORIENTED_EDGE ( 'NONE', *, *, #17962, .T. ) ;
#21693 = CARTESIAN_POINT ( 'NONE',  ( 0.2869720083484325057, -4.386174336869667734, 11.44147823180129464 ) ) ;
#21694 = CARTESIAN_POINT ( 'NONE',  ( -25.54417658651491863, -4.240019242199836391, 11.22596262356930197 ) ) ;
#21695 = AXIS2_PLACEMENT_3D ( 'NONE', #51897, #6338, #12288 ) ;
#21696 = ORIENTED_EDGE ( 'NONE', *, *, #29620, .F. ) ;
#21697 = ADVANCED_FACE ( 'NONE', ( #42639 ), #42307, .T. ) ;
#21699 = VECTOR ( 'NONE', #15673, 1000.000000000000000 ) ;
#21698 = CYLINDRICAL_SURFACE ( 'NONE', #59383, 4.999999999999999112 ) ;
#21700 = DIRECTION ( 'NONE',  ( -0.000000000000000000, -1.000000000000000000, -0.000000000000000000 ) ) ;
#21701 = FACE_OUTER_BOUND ( 'NONE', #62817, .T. ) ;
#21702 = CARTESIAN_POINT ( 'NONE',  ( -22.00000000000000711, -20.00000000000000000, 1.500000000000002887 ) ) ;
#21703 = VERTEX_POINT ( 'NONE', #12071 ) ;
#21704 = CARTESIAN_POINT ( 'NONE',  ( 3.031336079629464830, -4.304138522350336338, -6.621879275826748845 ) ) ;
#21705 = ADVANCED_FACE ( 'NONE', ( #37682 ), #2791, .T. ) ;
#21706 = ORIENTED_EDGE ( 'NONE', *, *, #59582, .T. ) ;
#21707 = DIRECTION ( 'NONE',  ( -1.000000000000000000, 0.000000000000000000, -0.000000000000000000 ) ) ;
#21708 = VECTOR ( 'NONE', #3224, 1000.000000000000000 ) ;
#21709 = ORIENTED_EDGE ( 'NONE', *, *, #58200, .T. ) ;
#21710 = FACE_OUTER_BOUND ( 'NONE', #22073, .T. ) ;
#21711 = CARTESIAN_POINT ( 'NONE',  ( 35.00000000000000000, -4.237174932027311769, -12.02534193257719508 ) ) ;
#21712 = LINE ( 'NONE', #31346, #39220 ) ;
#21713 = EDGE_CURVE ( 'NONE', #49092, #19473, #38670, .T. ) ;
#21714 = EDGE_LOOP ( 'NONE', ( #34963, #47551, #39965, #19764 ) ) ;
#21715 = AXIS2_PLACEMENT_3D ( 'NONE', #57688, #57029, #46707 ) ;
#21716 = CARTESIAN_POINT ( 'NONE',  ( 0.3341166715381321817, -4.432780143632420788, -11.44035855572979976 ) ) ;
#21717 = AXIS2_PLACEMENT_3D ( 'NONE', #11466, #1526, #42051 ) ;
#21718 = CARTESIAN_POINT ( 'NONE',  ( 28.81837816810347519, 11.51969343814563551, 7.050593228646411248 ) ) ;
#21719 = DIRECTION ( 'NONE',  ( 0.000000000000000000, -0.01356324068817998940, 0.9999080150203990547 ) ) ;
#21720 = AXIS2_PLACEMENT_3D ( 'NONE', #21974, #16979, #57233 ) ;
#21721 = ADVANCED_FACE ( 'NONE', ( #48653 ), #38322, .T. ) ;
#21722 = DIRECTION ( 'NONE',  ( 0.000000000000000000, -0.01356324068817998940, 0.9999080150203990547 ) ) ;
#21723 = LINE ( 'NONE', #38294, #54034 ) ;
#21724 = EDGE_CURVE ( 'NONE', #56447, #24195, #8689, .T. ) ;
#21725 = CARTESIAN_POINT ( 'NONE',  ( 5.514970785353741078, 0.001117786416802112525, -0.004588761610584830321 ) ) ;
#21726 = CARTESIAN_POINT ( 'NONE',  ( 2.269879328256729334, -5.759117113708034807, 5.026125315665188609 ) ) ;
#21727 = LINE ( 'NONE', #61947, #60896 ) ;
#21728 = EDGE_CURVE ( 'NONE', #14627, #41918, #26972, .T. ) ;
#21729 = CIRCLE ( 'NONE', #1566, 12.18650000000000411 ) ;
#21730 = VERTEX_POINT ( 'NONE', #64257 ) ;
#21731 = EDGE_CURVE ( 'NONE', #4063, #33705, #60965, .T. ) ;
#21732 = DIRECTION ( 'NONE',  ( 0.000000000000000000, 0.000000000000000000, 1.000000000000000000 ) ) ;
#21733 = CARTESIAN_POINT ( 'NONE',  ( 0.2911222467163550598, -12.25291251554515704, -0.2144311696656930888 ) ) ;
#21734 = VERTEX_POINT ( 'NONE', #650 ) ;
#21735 = CARTESIAN_POINT ( 'NONE',  ( 0.3665391374699465965, 2.392238720110458239, 12.04754782681758130 ) ) ;
#21736 = CARTESIAN_POINT ( 'NONE',  ( 35.00000000000000000, 4.705694406421931860E-17, -3.469127814946512892E-15 ) ) ;
#21737 = ORIENTED_EDGE ( 'NONE', *, *, #38279, .T. ) ;
#21738 = ADVANCED_FACE ( 'NONE', ( #33670 ), #30297, .F. ) ;
#21739 = CARTESIAN_POINT ( 'NONE',  ( -37.00000000000000711, -0.4993900848166508144, -12.17626345777664554 ) ) ;
#21740 = VERTEX_POINT ( 'NONE', #53961 ) ;
#21741 = VECTOR ( 'NONE', #54032, 1000.000000000000000 ) ;
#21742 = CARTESIAN_POINT ( 'NONE',  ( 0.3109076770649071841, -5.925244271826518805, 10.73466383006819136 ) ) ;
#21743 = ORIENTED_EDGE ( 'NONE', *, *, #26179, .F. ) ;
#21744 = ORIENTED_EDGE ( 'NONE', *, *, #52657, .T. ) ;
#21745 = B_SPLINE_CURVE_WITH_KNOTS ( 'NONE', 3,
 ( #7559, #7906, #12873, #43447, #49134, #3592, #48151, #23858, #18555, #2609, #44119, #63726, #64386, #51085, #60071, #60384, #55742, #50749 ),
 .UNSPECIFIED., .F., .F.,
 ( 4, 2, 2, 2, 2, 2, 2, 2, 4 ),
 ( 4.906538933386797396E-18, 0.002682641281242477155, 0.003353301601553095469, 0.004023961921863713348, 0.005365282562484952576, 0.006706603203106191805, 0.008047923843727428431, 0.009389244484348668526, 0.01073056512496990689 ),
 .UNSPECIFIED. ) ;
#21746 = CARTESIAN_POINT ( 'NONE',  ( 35.00000000000000000, -10.70999494708488520, 5.814360711498399503 ) ) ;
#21747 = B_SPLINE_CURVE_WITH_KNOTS ( 'NONE', 3,
 ( #5181, #50417, #61036, #56032, #194, #30436 ),
 .UNSPECIFIED., .F., .F.,
 ( 4, 2, 4 ),
 ( 0.0001654224980408314249, 0.0006219428995476478528, 0.001078463301054464335 ),
 .UNSPECIFIED. ) ;
#21748 = ORIENTED_EDGE ( 'NONE', *, *, #28671, .T. ) ;
#21749 = CARTESIAN_POINT ( 'NONE',  ( -24.79499881855582188, -8.357637111868410074, 8.619227215508589168 ) ) ;
#21750 = LINE ( 'NONE', #51015, #401 ) ;
#21751 = CARTESIAN_POINT ( 'NONE',  ( 0.3675815128205894289, -0.2638082659427565813, -12.27743992903066328 ) ) ;
#21752 = VERTEX_POINT ( 'NONE', #28678 ) ;
#21753 = AXIS2_PLACEMENT_3D ( 'NONE', #52041, #51722, #43031 ) ;
#21754 = DIRECTION ( 'NONE',  ( 0.000000000000000000, 0.000000000000000000, -1.000000000000000000 ) ) ;
#21755 = CARTESIAN_POINT ( 'NONE',  ( 1.749504362522309897, -27.84680466544767796, 12.51149646090675915 ) ) ;
#21756 = CARTESIAN_POINT ( 'NONE',  ( 0.000000000000000000, -1.956810415765224187, 6.654767106875530303 ) ) ;
#21758 = VERTEX_POINT ( 'NONE', #4072 ) ;
#21757 = CARTESIAN_POINT ( 'NONE',  ( -37.00000000000000711, -10.28547182238004076, -5.672855678558794246 ) ) ;
#21759 = CARTESIAN_POINT ( 'NONE',  ( -27.95874796761056658, 11.60023435971385553, -3.134445752752807568 ) ) ;
#21760 = VERTEX_POINT ( 'NONE', #39963 ) ;
#21761 = CIRCLE ( 'NONE', #14329, 2.899999999999995026 ) ;
#21762 = CARTESIAN_POINT ( 'NONE',  ( 3.152665057734062248, -7.609997527621111146, 2.258875078502258216 ) ) ;
#21763 = EDGE_LOOP ( 'NONE', ( #16724, #65241, #43333, #1413 ) ) ;
#21764 = CARTESIAN_POINT ( 'NONE',  ( 22.22094857615726227, -10.34774274339837419, -6.087373716788684774 ) ) ;
#21765 = CARTESIAN_POINT ( 'NONE',  ( 2.000000000000001776, 5.769711778877384845, -4.791703871138491166 ) ) ;
#21766 = AXIS2_PLACEMENT_3D ( 'NONE', #29810, #23539, #64722 ) ;
#21767 = CARTESIAN_POINT ( 'NONE',  ( 2.305787727787083519, -7.654065630109506913, -0.1666591538753489643 ) ) ;
#21769 = EDGE_CURVE ( 'NONE', #33142, #41836, #31626, .T. ) ;
#21768 = ORIENTED_EDGE ( 'NONE', *, *, #29050, .T. ) ;
#21770 = CARTESIAN_POINT ( 'NONE',  ( -37.00000000000000711, -11.17622378668009020, 3.614449339633449387 ) ) ;
#21771 = FACE_OUTER_BOUND ( 'NONE', #41207, .T. ) ;
#21772 = CARTESIAN_POINT ( 'NONE',  ( 0.3109076770649032984, -12.03190317807025878, 2.361108455562804576 ) ) ;
#21773 = ORIENTED_EDGE ( 'NONE', *, *, #27620, .T. ) ;
#21774 = EDGE_CURVE ( 'NONE', #41285, #26398, #9055, .T. ) ;
#21775 =( BOUNDED_CURVE ( )  B_SPLINE_CURVE ( 3, ( #61648, #36388, #5157, #25424 ),
 .UNSPECIFIED., .F., .T. ) 
 B_SPLINE_CURVE_WITH_KNOTS ( ( 4, 4 ),
 ( 0.8127194087688081048, 0.8598086627273093807 ),
 .UNSPECIFIED. ) 
 CURVE ( )  GEOMETRIC_REPRESENTATION_ITEM ( )  RATIONAL_B_SPLINE_CURVE ( ( 1.000000000000000000, 0.9998152253828482827, 0.9998152253828482827, 1.000000000000000000 ) ) 
 REPRESENTATION_ITEM ( '' )  );
#21776 = ORIENTED_EDGE ( 'NONE', *, *, #20806, .T. ) ;
#21777 = CARTESIAN_POINT ( 'NONE',  ( 3.047904605210369322, 7.698174516567099168, 1.788881754552535286 ) ) ;
#21778 = EDGE_LOOP ( 'NONE', ( #6119, #27121, #39263, #1318 ) ) ;
#21779 = ORIENTED_EDGE ( 'NONE', *, *, #20813, .F. ) ;
#21780 = ADVANCED_FACE ( 'NONE', ( #16910 ), #21910, .T. ) ;
#21781 = CARTESIAN_POINT ( 'NONE',  ( -35.00000000000000000, 0.000000000000000000, 0.000000000000000000 ) ) ;
#21782 = CARTESIAN_POINT ( 'NONE',  ( 0.5547464869798247600, -10.53334899235175470, 6.433541106625056294 ) ) ;
#21783 = DIRECTION ( 'NONE',  ( 1.000000000000000000, 0.000000000000000000, 0.000000000000000000 ) ) ;
#21784 = FACE_OUTER_BOUND ( 'NONE', #34080, .T. ) ;
#21785 = CARTESIAN_POINT ( 'NONE',  ( 35.00000000000000000, 7.718225330433935660, 9.430788938293964918 ) ) ;
#21786 = DIRECTION ( 'NONE',  ( 0.000000000000000000, 0.8835120444460240474, -0.4684084406997878758 ) ) ;
#21787 = AXIS2_PLACEMENT_3D ( 'NONE', #62251, #61586, #1430 ) ;
#21788 = B_SPLINE_CURVE_WITH_KNOTS ( 'NONE', 3,
 ( #39460, #8553, #28841, #14191, #23875, #3263, #2935, #43810, #59762, #48486, #13226, #34479, #4230, #44134, #38824, #33170 ),
 .UNSPECIFIED., .F., .F.,
 ( 4, 3, 3, 3, 3, 4 ),
 ( 2.636225826258666826E-15, 0.0002126834539179618623, 0.0004253519300366071084, 0.0006380165497223882001, 0.0007442707582427911467, 0.0009453531351419972159 ),
 .UNSPECIFIED. ) ;
#21789 = DIRECTION ( 'NONE',  ( -1.000000000000000000, 0.000000000000000000, 0.000000000000000000 ) ) ;
#21790 = VERTEX_POINT ( 'NONE', #37179 ) ;
#21791 = CARTESIAN_POINT ( 'NONE',  ( 0.3040950598368152291, 6.347045025870766466, 10.49113473328032775 ) ) ;
#21792 = ADVANCED_FACE ( 'NONE', ( #57487 ), #1641, .T. ) ;
#21793 = CARTESIAN_POINT ( 'NONE',  ( -4.033241259908380449, -9.046539124021903078, 7.887417314856400630 ) ) ;
#21794 = EDGE_CURVE ( 'NONE', #38173, #52755, #44269, .T. ) ;
#21795 = B_SPLINE_CURVE_WITH_KNOTS ( 'NONE', 3,
 ( #3600, #23866, #34470, #18861, #33805, #55411, #59114, #64081, #4563, #8543, #44127, #24832, #60391, #34133, #24165, #54451, #54773, #14815, #64393 ),
 .UNSPECIFIED., .F., .F.,
 ( 4, 3, 3, 3, 3, 3, 4 ),
 ( 1.039534490390255771E-17, 4.457896483015144114E-05, 6.639290541542309371E-05, 8.820687556479193578E-05, 0.0001100173248778926413, 0.0001545671401658163036, 0.0001830328308068566252 ),
 .UNSPECIFIED. ) ;
#21796 = CARTESIAN_POINT ( 'NONE',  ( 0.3537226245948369985, 4.442821955543956314, -11.44347094181047453 ) ) ;
#21797 = DIRECTION ( 'NONE',  ( 0.000000000000000000, -0.01356324068817998940, 0.9999080150203990547 ) ) ;
#21798 = VECTOR ( 'NONE', #29953, 1000.000000000000000 ) ;
#21799 = CARTESIAN_POINT ( 'NONE',  ( 22.85970942819514917, -4.208613694812052053, -12.82931771421080214 ) ) ;
#21800 = DIRECTION ( 'NONE',  ( 1.000000000000000000, -0.000000000000000000, 0.000000000000000000 ) ) ;
#21801 = ORIENTED_EDGE ( 'NONE', *, *, #54959, .F. ) ;
#21802 = CARTESIAN_POINT ( 'NONE',  ( -27.08416974970326763, 0.4041872645907068629, 2.255186831366090772 ) ) ;
#21803 = LINE ( 'NONE', #47400, #14452 ) ;
#21804 = CARTESIAN_POINT ( 'NONE',  ( 5.515539859299206427, 0.003740028639278282496, 0.004759416711441693572 ) ) ;
#21805 = CARTESIAN_POINT ( 'NONE',  ( 2.491965175174698288, -1.548529392254218040, -7.560994562509435468 ) ) ;
#21806 = EDGE_CURVE ( 'NONE', #9912, #10001, #31228, .T. ) ;
#21807 = AXIS2_PLACEMENT_3D ( 'NONE', #15432, #35699, #55996 ) ;
#21808 = EDGE_CURVE ( 'NONE', #54132, #31390, #10941, .T. ) ;
#21809 = CARTESIAN_POINT ( 'NONE',  ( -37.00000000000000711, 10.70999494708501132, -5.814360711498173018 ) ) ;
#21810 = CARTESIAN_POINT ( 'NONE',  ( -25.86628395826706850, -8.041618865309574815, 10.84354029019568522 ) ) ;
#21811 = ORIENTED_EDGE ( 'NONE', *, *, #42607, .F. ) ;
#21812 = CARTESIAN_POINT ( 'NONE',  ( 2.655192694323436964, 6.969384012965880615, -6.604353705985066547 ) ) ;
#21813 = LINE ( 'NONE', #11167, #64121 ) ;
#21814 = CARTESIAN_POINT ( 'NONE',  ( 0.4613984246114888887, -12.17044190070616061, -1.858723191796595842 ) ) ;
#21815 = ORIENTED_EDGE ( 'NONE', *, *, #61651, .F. ) ;
#21816 = EDGE_CURVE ( 'NONE', #2142, #52203, #2603, .T. ) ;
#21817 = CARTESIAN_POINT ( 'NONE',  ( 0.000000000000000000, -6.606214214351039615, -2.114938770769998477 ) ) ;
#21818 = DIRECTION ( 'NONE',  ( -1.000000000000000000, 0.000000000000000000, 0.000000000000000000 ) ) ;
#21820 = ORIENTED_EDGE ( 'NONE', *, *, #4484, .T. ) ;
#21819 = CARTESIAN_POINT ( 'NONE',  ( 35.00000000000000000, 4.705694406421931860E-17, -3.469127814946512892E-15 ) ) ;
#21821 = DIRECTION ( 'NONE',  ( 0.000000000000000000, -0.01356324068817998940, 0.9999080150203990547 ) ) ;
#21822 = AXIS2_PLACEMENT_3D ( 'NONE', #1014, #21280, #36903 ) ;
#21823 = EDGE_CURVE ( 'NONE', #25967, #3960, #64953, .T. ) ;
#21824 = CARTESIAN_POINT ( 'NONE',  ( -37.00000000000000711, -10.62137734850264614, -5.015831474386418520 ) ) ;
#21825 = ORIENTED_EDGE ( 'NONE', *, *, #52989, .F. ) ;
#21826 = LINE ( 'NONE', #57387, #35429 ) ;
#21827 = LINE ( 'NONE', #42073, #27708 ) ;
#21828 = CARTESIAN_POINT ( 'NONE',  ( -27.35552965826137140, -3.094132632038958608, -0.2619431035392160156 ) ) ;
#21829 = CARTESIAN_POINT ( 'NONE',  ( -10.00000000000000178, 0.000000000000000000, 0.000000000000000000 ) ) ;
#21830 = CARTESIAN_POINT ( 'NONE',  ( 2.000000000000001776, 0.000000000000000000, 0.000000000000000000 ) ) ;
#21831 = CARTESIAN_POINT ( 'NONE',  ( 0.2657645697724688172, 5.991637049003244009, 10.68050050043093258 ) ) ;
#21833 = EDGE_LOOP ( 'NONE', ( #7746, #24938, #25253, #54471 ) ) ;
#21832 = CARTESIAN_POINT ( 'NONE',  ( 0.2671309869109514956, 11.45180222993660379, -4.340541005679410702 ) ) ;
#21834 = VERTEX_POINT ( 'NONE', #57827 ) ;
#21835 = CARTESIAN_POINT ( 'NONE',  ( 24.19827605764011480, 1.944242837392233136, -11.84706149513093365 ) ) ;
#21836 = ORIENTED_EDGE ( 'NONE', *, *, #17114, .T. ) ;
#21837 = ITEM_DEFINED_TRANSFORMATION ( 'NONE', 'NONE', #14354,  #24966 ) ;
#21838 = CARTESIAN_POINT ( 'NONE',  ( 0.000000000000000000, 0.000000000000000000, 0.000000000000000000 ) ) ;
#21839 = CARTESIAN_POINT ( 'NONE',  ( 2.350038591458109227, 1.210550722321025452, 10.55267716396076239 ) ) ;
#21840 = LINE ( 'NONE', #36106, #7607 ) ;
#21841 = EDGE_LOOP ( 'NONE', ( #65478, #65311, #10162, #13183 ) ) ;
#21842 = EDGE_CURVE ( 'NONE', #13989, #61330, #37602, .T. ) ;
#21843 = AXIS2_PLACEMENT_3D ( 'NONE', #49454, #13200, #39772 ) ;
#21844 = DIRECTION ( 'NONE',  ( -1.000000000000000000, 0.000000000000000000, 0.000000000000000000 ) ) ;
#21845 = DIRECTION ( 'NONE',  ( -1.000000000000000000, 0.000000000000000000, -0.000000000000000000 ) ) ;
#21846 = EDGE_LOOP ( 'NONE', ( #40613, #55187, #1988, #749 ) ) ;
#21847 = ORIENTED_EDGE ( 'NONE', *, *, #28869, .T. ) ;
#21848 = CARTESIAN_POINT ( 'NONE',  ( 2.368238019615220402, 7.526794520527660737, -1.509700170844529232 ) ) ;
#21849 = ORIENTED_EDGE ( 'NONE', *, *, #2204, .T. ) ;
#21850 = CARTESIAN_POINT ( 'NONE',  ( 2.241451721903216399, 1.385577012535855523, -7.507681056655362895 ) ) ;
#21851 = CARTESIAN_POINT ( 'NONE',  ( 2.000000000000001776, -1.754183803416586196, 6.711026108862235162 ) ) ;
#21852 = CARTESIAN_POINT ( 'NONE',  ( 35.00000000000000000, 4.705694406421931860E-17, -3.469127814946512892E-15 ) ) ;
#21853 = AXIS2_PLACEMENT_3D ( 'NONE', #49251, #4004, #13957 ) ;
#21854 = CARTESIAN_POINT ( 'NONE',  ( 35.00000000000000000, 4.705694406421931860E-17, -3.469127814946512892E-15 ) ) ;
#21855 = FACE_OUTER_BOUND ( 'NONE', #51460, .T. ) ;
#21856 = CARTESIAN_POINT ( 'NONE',  ( 2.305787727787083519, -7.566723232958080914, 1.164987321564707967 ) ) ;
#21857 = CYLINDRICAL_SURFACE ( 'NONE', #49317, 12.74999999999999822 ) ;
#21858 = VERTEX_POINT ( 'NONE', #12247 ) ;
#21859 = CARTESIAN_POINT ( 'NONE',  ( 1.459561108992491807, 12.62847742794652106, -0.6317018236570858258 ) ) ;
#21860 = VERTEX_POINT ( 'NONE', #966 ) ;
#21861 = DIRECTION ( 'NONE',  ( 1.000000000000000000, 0.000000000000000000, 0.000000000000000000 ) ) ;
#21862 = EDGE_CURVE ( 'NONE', #19083, #2301, #27532, .T. ) ;
#21863 = CARTESIAN_POINT ( 'NONE',  ( -22.30625920655495165, 2.750410778797888867, 2.610366806364660341 ) ) ;
#21864 = CARTESIAN_POINT ( 'NONE',  ( 37.00000000000000711, 10.32377448871667625, -6.475373545682339582 ) ) ;
#21865 = DIRECTION ( 'NONE',  ( -1.000000000000000000, 0.000000000000000000, 0.000000000000000000 ) ) ;
#21866 = CARTESIAN_POINT ( 'NONE',  ( 0.2767916011545370480, -10.70244578860291718, -5.959903879715701791 ) ) ;
#21867 = CARTESIAN_POINT ( 'NONE',  ( 0.2650492594609235031, -11.46945808033130909, -4.291723947796430849 ) ) ;
#21868 = ADVANCED_FACE ( 'NONE', ( #31541 ), #21588, .T. ) ;
#21869 = EDGE_LOOP ( 'NONE', ( #30268, #37403, #11527, #5553 ) ) ;
#21870 = ORIENTED_EDGE ( 'NONE', *, *, #35415, .F. ) ;
#21871 = DIRECTION ( 'NONE',  ( 0.3939253465568944290, -0.5982248387291289049, 0.6978179301705699222 ) ) ;
#21872 = ORIENTED_EDGE ( 'NONE', *, *, #11135, .T. ) ;
#21873 = CARTESIAN_POINT ( 'NONE',  ( 0.2767916011545404897, 7.727819755721592188, -9.504925141026269841 ) ) ;
#21874 = CARTESIAN_POINT ( 'NONE',  ( 37.00000000000000711, 10.59380114696469910, -7.094637218249396859 ) ) ;
#21875 = CARTESIAN_POINT ( 'NONE',  ( 2.305787727787084851, -7.566723232958062262, -1.164987321564809886 ) ) ;
#21876 = CARTESIAN_POINT ( 'NONE',  ( 35.00000000000000000, 3.340853584269691368, 11.26103545359851665 ) ) ;
#21877 = ORIENTED_EDGE ( 'NONE', *, *, #62112, .T. ) ;
#21878 = CARTESIAN_POINT ( 'NONE',  ( 0.2651627923886334393, -6.046629261473261963, -10.64925183219499694 ) ) ;
#21879 = CARTESIAN_POINT ( 'NONE',  ( 35.00000000000000000, -0.3025107581130382917, 11.74226168163341022 ) ) ;
#21880 = CARTESIAN_POINT ( 'NONE',  ( 0.6511581176963316953, -12.23990098761621326, 1.822219471614201725 ) ) ;
#21881 = CARTESIAN_POINT ( 'NONE',  ( -49.83768944945995116, -0.03330036048197439202, 3.290779520873027941 ) ) ;
#21882 = EDGE_CURVE ( 'NONE', #57018, #29075, #46843, .T. ) ;
#21883 = AXIS2_PLACEMENT_3D ( 'NONE', #65563, #45620, #51298 ) ;
#21884 = CARTESIAN_POINT ( 'NONE',  ( 0.3401186441510231639, 6.355596563012454681, -10.49699112323336259 ) ) ;
#21885 = CIRCLE ( 'NONE', #15499, 12.75000000000000178 ) ;
#21886 = ORIENTED_EDGE ( 'NONE', *, *, #23576, .T. ) ;
#21887 = CARTESIAN_POINT ( 'NONE',  ( 0.2646305136544065406, 6.237419468587226845, -10.53923716745240036 ) ) ;
#21888 = VERTEX_POINT ( 'NONE', #36864 ) ;
#21889 = CARTESIAN_POINT ( 'NONE',  ( 10.57567362079633355, 8.112553359107787188, -10.79197710481157557 ) ) ;
#21890 = CARTESIAN_POINT ( 'NONE',  ( 2.241509619876136838, 7.160887714159624551, 2.647089031563595540 ) ) ;
#21891 = CARTESIAN_POINT ( 'NONE',  ( 0.000000000000000000, 0.000000000000000000, 0.000000000000000000 ) ) ;
#21892 = CARTESIAN_POINT ( 'NONE',  ( 5.516018279890452902, 0.006440244342253029219, 0.002104829434640694864 ) ) ;
#21893 = FACE_OUTER_BOUND ( 'NONE', #9577, .T. ) ;
#21894 = CIRCLE ( 'NONE', #14414, 2.899999999999995470 ) ;
#21895 = EDGE_CURVE ( 'NONE', #9063, #50945, #28075, .T. ) ;
#21896 = VERTEX_POINT ( 'NONE', #17582 ) ;
#21897 = VERTEX_POINT ( 'NONE', #33825 ) ;
#21898 = CARTESIAN_POINT ( 'NONE',  ( 0.3278977287071232483, 1.885359334311965895, 12.12129679591847164 ) ) ;
#21899 = VERTEX_POINT ( 'NONE', #13239 ) ;
#21900 = CYLINDRICAL_SURFACE ( 'NONE', #5426, 12.18649999999999878 ) ;
#21901 = CARTESIAN_POINT ( 'NONE',  ( 3.375695012145481400, 5.390482730139837031, -12.38384929327539830 ) ) ;
#21902 = CARTESIAN_POINT ( 'NONE',  ( 22.57855258442564761, -4.427776684447072952, 12.75322679295976691 ) ) ;
#21903 = CARTESIAN_POINT ( 'NONE',  ( 2.241352910868908310, 0.08337961031714861970, -7.633946224498473043 ) ) ;
#21904 = CARTESIAN_POINT ( 'NONE',  ( 1.462291587750753852, -7.633056170897860149, -10.08151577214967709 ) ) ;
#21905 = CYLINDRICAL_SURFACE ( 'NONE', #47256, 6.095312090839646757 ) ;
#21906 = CARTESIAN_POINT ( 'NONE',  ( 2.000000000000001776, 5.814643797626930954, 3.550179297009575574 ) ) ;
#21907 = ORIENTED_EDGE ( 'NONE', *, *, #17762, .T. ) ;
#21908 = CARTESIAN_POINT ( 'NONE',  ( 5.514624014163232779, 0.003946330869975002258, -0.001255375129358090409 ) ) ;
#21909 = ORIENTED_EDGE ( 'NONE', *, *, #49416, .F. ) ;
#21910 = CYLINDRICAL_SURFACE ( 'NONE', #32271, 2.899999999999994582 ) ;
#21911 = CARTESIAN_POINT ( 'NONE',  ( -37.00000000000000711, 11.56998259273177787, 3.827046518385122553 ) ) ;
#21912 = CARTESIAN_POINT ( 'NONE',  ( -20.79170840334646542, 11.34110549087207076, -3.921648409140116698 ) ) ;
#21913 = VERTEX_POINT ( 'NONE', #59133 ) ;
#21914 = CARTESIAN_POINT ( 'NONE',  ( -35.00000000000000000, 0.000000000000000000, 0.000000000000000000 ) ) ;
#21915 = EDGE_CURVE ( 'NONE', #53066, #476, #12108, .T. ) ;
#21916 = FACE_OUTER_BOUND ( 'NONE', #12984, .T. ) ;
#21917 = CARTESIAN_POINT ( 'NONE',  ( 37.00000000000000711, 12.17626345777663488, -0.4993900848167889817 ) ) ;
#21918 = VERTEX_POINT ( 'NONE', #12902 ) ;
#21919 = EDGE_LOOP ( 'NONE', ( #17910, #2168, #57549, #4295, #4691, #5302, #45839, #23472, #31699, #20603, #20845, #33653, #28464, #56946, #10851, #24962, #53982, #1656, #21010, #59536, #44381, #2368, #51004, #20814, #45536, #9003, #25912, #42254, #62390, #24672, #54862, #63917, #62202, #47679, #44952, #11715, #13762, #63530, #14151, #57156, #15288, #38229, #13650, #34786, #24156, #16701, #22813, #11838, #17480, #36847, #54699, #35651, #64571, #14527, #33270, #10210, #4720, #21673, #36755, #18217, #54303, #43166, #53143, #64898, #38308, #9632, #50187, #25861, #48324, #14418, #47658, #32459, #14816, #38001, #9707, #6968, #8635, #12530, #59569, #23103, #35940, #17046, #18495, #37575, #3803, #8051, #16697, #45391, #55998, #9039, #10854, #39972, #36044, #50384, #21394, #31130, #287, #48521, #1307, #39820, #23437, #48021, #23063, #10467, #54513, #43072, #59955, #52037, #36027, #54790, #55931, #55959, #37530, #37929, #43666, #50687, #13820, #17985, #37673, #61220, #17624, #13661, #48939, #13325, #32307, #23111, #51209, #52687, #17231, #44372, #11598, #23327, #51809, #45064, #20585, #32088, #64879, #5768, #6831, #34320, #5632, #32347, #61637, #16305, #17908, #5843, #24581, #38774, #44340, #1905, #34909, #45599, #787, #56193, #27457, #27872, #10288, #48225, #62791, #1600, #14205, #42896, #19419, #63759, #59811, #40454, #45592, #59658, #36629, #42543, #33734, #6881, #60493, #51680, #7596, #22983, #31635, #36390, #43421, #26572, #26065, #58897, #62305, #45888, #11756, #6048, #23320, #38313, #9727, #29428, #45539, #11268, #2586, #6596, #40094, #9790, #44179, #35581, #36515, #36079, #80, #58735, #58209, #25499, #2438, #37366, #14059, #57959, #36925, #61227, #40946, #62702, #62499, #65785, #43902, #22447, #12332, #62937, #20014, #51092, #51120, #1071, #44460, #39899, #2212, #47904, #16420, #43431, #33624, #58277, #32273, #5939, #27071, #24568, #49235, #51452, #8560, #28669, #16978, #42423, #21321, #10660, #65116, #51767, #45292, #50447, #58862, #43126, #32917, #33582, #13462, #41271, #42566, #36965, #39233, #14216, #14649, #47491, #51022, #65323, #58403, #29392, #61605, #45681, #17185, #27698, #24044, #62509, #4490, #12031, #37955, #65452, #65278, #1645, #25189, #38004, #44395, #34732, #6670, #14696, #41829, #58246, #64313, #35761, #20648, #9883, #23011, #6807, #39863, #4856, #7480, #45695, #6768, #1990, #32765, #19293, #2435, #32150, #51517, #37933, #2700, #3233, #41197, #63847, #8282, #34906, #25254, #56949, #46348, #55331, #5058, #63330, #4116, #36897, #6471, #34351, #4626, #53558, #15862, #17537, #5530, #45450, #56572, #38660, #14839, #57433, #42836, #37004, #46438, #58829, #11600, #50806, #65289, #6176, #13447, #44080, #59703, #980, #62615, #6148, #12883, #31612, #45218, #45981, #35213, #24337, #59109, #25003, #13115, #50290, #63760, #62698, #15196, #16726, #2642, #47649, #20893, #58001, #65683, #62074, #21971, #61282, #18395, #49354, #2283, #32122, #17849, #64201, #26724, #16062, #43928, #18652, #31248, #5490, #16607, #496, #54280, #43445, #58055, #9462, #3534, #30367, #40183, #53034, #32943, #56529, #59768, #46374, #28533, #64486, #21612, #46757, #55944, #53326, #20599, #31770, #60698, #54262, #12703, #544, #20363, #44236, #26684, #1868, #63870 ) ) ;
#21920 = CARTESIAN_POINT ( 'NONE',  ( 37.00000000000000711, -6.657191900728386180, -9.677500615117878624 ) ) ;
#21921 = EDGE_CURVE ( 'NONE', #20840, #18772, #15023, .T. ) ;
#21922 = ORIENTED_EDGE ( 'NONE', *, *, #64055, .F. ) ;
#21923 = EDGE_LOOP ( 'NONE', ( #60312, #55174, #27426, #36836 ) ) ;
#21924 = ORIENTED_EDGE ( 'NONE', *, *, #34410, .F. ) ;
#21925 = EDGE_LOOP ( 'NONE', ( #2432, #1559, #15703, #59250 ) ) ;
#21926 = FACE_BOUND ( 'NONE', #8861, .T. ) ;
#21927 = CARTESIAN_POINT ( 'NONE',  ( 2.259830038564650589, 5.015955067335593043, -5.763537486834822587 ) ) ;
#21928 = CYLINDRICAL_SURFACE ( 'NONE', #33120, 4.000030059823568074 ) ;
#21930 = EDGE_CURVE ( 'NONE', #18816, #61317, #49160, .T. ) ;
#21929 = CARTESIAN_POINT ( 'NONE',  ( 2.242819959140644137, 2.707278038035169310, -7.138786956204133283 ) ) ;
#21931 = EDGE_LOOP ( 'NONE', ( #64519, #41363, #21870, #5337 ) ) ;
#21932 = CIRCLE ( 'NONE', #59100, 2.899999999999995026 ) ;
#21933 = CARTESIAN_POINT ( 'NONE',  ( -37.00000000000000711, 8.839356091080043498, 8.389074212634319849 ) ) ;
#21934 = AXIS2_PLACEMENT_3D ( 'NONE', #3754, #44274, #39615 ) ;
#21935 = ORIENTED_EDGE ( 'NONE', *, *, #14250, .F. ) ;
#21936 = CARTESIAN_POINT ( 'NONE',  ( 37.00000000000000711, 10.63508530065521640, -4.986700593229742573 ) ) ;
#21937 = CARTESIAN_POINT ( 'NONE',  ( -22.27719412087655471, 2.887588494201237310, -2.283949229175413098 ) ) ;
#21938 = CARTESIAN_POINT ( 'NONE',  ( 2.269879328257217832, 3.692763753156445894, -6.692746930935887129 ) ) ;
#21939 = ADVANCED_FACE ( 'NONE', ( #18583 ), #3619, .T. ) ;
#21940 = B_SPLINE_CURVE_WITH_KNOTS ( 'NONE', 3,
 ( #23852, #24817, #40085, #44110, #34456, #64379, #29456 ),
 .UNSPECIFIED., .F., .F.,
 ( 4, 3, 4 ),
 ( 0.000000000000000000, 0.001700533616330535819, 0.005002426799371217578 ),
 .UNSPECIFIED. ) ;
#21941 = CARTESIAN_POINT ( 'NONE',  ( 0.2958664285830405194, -8.045892866065303295, -9.245659426743973341 ) ) ;
#21942 = PLANE ( 'NONE',  #33382 ) ;
#21943 = DIRECTION ( 'NONE',  ( -1.000000000000000000, 0.000000000000000000, 0.000000000000000000 ) ) ;
#21944 = VERTEX_POINT ( 'NONE', #12555 ) ;
#21945 = DIRECTION ( 'NONE',  ( -1.000000000000000000, -0.000000000000000000, 0.000000000000000000 ) ) ;
#21946 =( BOUNDED_CURVE ( )  B_SPLINE_CURVE ( 3, ( #34005, #19054, #53331, #48358 ),
 .UNSPECIFIED., .F., .F. ) 
 B_SPLINE_CURVE_WITH_KNOTS ( ( 4, 4 ),
 ( 1.889095289054163906, 1.912960151588308788 ),
 .UNSPECIFIED. ) 
 CURVE ( )  GEOMETRIC_REPRESENTATION_ITEM ( )  RATIONAL_B_SPLINE_CURVE ( ( 1.000000000000000000, 0.9999525395911521564, 0.9999525395911521564, 1.000000000000000000 ) ) 
 REPRESENTATION_ITEM ( '' )  );
#21947 = VERTEX_POINT ( 'NONE', #58471 ) ;
#21948 = DIRECTION ( 'NONE',  ( 0.000000000000000000, 0.5243256840888502746, 0.8515178078024906450 ) ) ;
#21949 = CARTESIAN_POINT ( 'NONE',  ( 17.99690872998901270, -28.74566129397117464, -8.126501682513225688 ) ) ;
#21950 = CARTESIAN_POINT ( 'NONE',  ( 2.827825597296800719, 8.650999012440216518, -2.568788224597678305 ) ) ;
#21951 = CARTESIAN_POINT ( 'NONE',  ( -27.09342121492584710, -0.6436068655225301027, -2.227768580955221012 ) ) ;
#21952 = CARTESIAN_POINT ( 'NONE',  ( 2.253265082352431836, -6.678225412356971091, 3.707567016433793938 ) ) ;
#21953 = VERTEX_POINT ( 'NONE', #13544 ) ;
#21954 = FACE_OUTER_BOUND ( 'NONE', #34215, .T. ) ;
#21955 = CARTESIAN_POINT ( 'NONE',  ( 37.00000000000000711, 4.705694406421931860E-17, -3.469127814946512892E-15 ) ) ;
#21956 = CARTESIAN_POINT ( 'NONE',  ( -18.58686583997218378, 5.151216734910788908, 12.47858029384653555 ) ) ;
#21957 = FACE_OUTER_BOUND ( 'NONE', #46058, .T. ) ;
#21958 = CYLINDRICAL_SURFACE ( 'NONE', #16981, 4.999999999999999112 ) ;
#21959 = VERTEX_POINT ( 'NONE', #54126 ) ;
#21960 = CARTESIAN_POINT ( 'NONE',  ( 5.514970785353741078, -0.0005190732562558867313, -0.004694330894494369230 ) ) ;
#21961 = DIRECTION ( 'NONE',  ( 1.000000000000000000, 0.000000000000000000, 0.000000000000000000 ) ) ;
#21962 = AXIS2_PLACEMENT_3D ( 'NONE', #32599, #62536, #21992 ) ;
#21963 = EDGE_CURVE ( 'NONE', #1294, #2632, #15291, .T. ) ;
#21964 = AXIS2_PLACEMENT_3D ( 'NONE', #7676, #3361, #58559 ) ;
#21965 = EDGE_LOOP ( 'NONE', ( #30795, #32791, #60289, #6277 ) ) ;
#21966 = ORIENTED_EDGE ( 'NONE', *, *, #56963, .F. ) ;
#21967 = DIRECTION ( 'NONE',  ( 1.000000000000000000, 0.000000000000000000, 0.000000000000000000 ) ) ;
#21968 = DIRECTION ( 'NONE',  ( 1.000000000000000000, 0.000000000000000000, 0.000000000000000000 ) ) ;
#21969 = CARTESIAN_POINT ( 'NONE',  ( 35.00000000000000000, 12.05416472667167760, 1.791059740004291578 ) ) ;
#21970 = DIRECTION ( 'NONE',  ( 0.000000000000000000, -0.01356324068817998940, 0.9999080150203990547 ) ) ;
#21971 = ORIENTED_EDGE ( 'NONE', *, *, #29339, .F. ) ;
#21972 = ORIENTED_EDGE ( 'NONE', *, *, #8811, .T. ) ;
#21973 = VERTEX_POINT ( 'NONE', #8564 ) ;
#21974 = CARTESIAN_POINT ( 'NONE',  ( 3.152665057734040488, 0.000000000000000000, 0.000000000000000000 ) ) ;
#21975 = CYLINDRICAL_SURFACE ( 'NONE', #58689, 12.18649999999999878 ) ;
#21976 = EDGE_CURVE ( 'NONE', #14585, #42516, #22764, .T. ) ;
#21977 = EDGE_LOOP ( 'NONE', ( #43497, #36683, #17414, #14370 ) ) ;
#21978 = DIRECTION ( 'NONE',  ( 1.000000000000000000, -0.000000000000000000, 0.000000000000000000 ) ) ;
#21979 = CARTESIAN_POINT ( 'NONE',  ( 2.000000000000001776, 6.777474576704075382, -0.6925993764990371337 ) ) ;
#21980 = VERTEX_POINT ( 'NONE', #53492 ) ;
#21981 = CARTESIAN_POINT ( 'NONE',  ( 0.2653141617321035928, 11.52265685897335068, -4.147035654172604779 ) ) ;
#21982 = EDGE_CURVE ( 'NONE', #25095, #59550, #61782, .T. ) ;
#21983 = CARTESIAN_POINT ( 'NONE',  ( 9.704251177394571215, -29.31945899941926115, -10.96599872320825142 ) ) ;
#21984 = DIRECTION ( 'NONE',  ( 1.000000000000000000, 0.000000000000000000, 0.000000000000000000 ) ) ;
#21985 = VERTEX_POINT ( 'NONE', #32399 ) ;
#21986 = DIRECTION ( 'NONE',  ( -1.000000000000000000, 0.000000000000000000, 0.000000000000000000 ) ) ;
#21987 = ADVANCED_FACE ( 'NONE', ( #52711 ), #43037, .T. ) ;
#21988 = VERTEX_POINT ( 'NONE', #41733 ) ;
#21989 = CARTESIAN_POINT ( 'NONE',  ( 11.92370524553500388, 0.08318608274626294874, -13.49997410565396905 ) ) ;
#21990 = CARTESIAN_POINT ( 'NONE',  ( -18.20967569695231703, -5.494204602085749123, 12.33373156890061395 ) ) ;
#21991 = CARTESIAN_POINT ( 'NONE',  ( 2.827825597296808269, -2.568788224597702730, -8.650999012440189873 ) ) ;
#21992 = DIRECTION ( 'NONE',  ( 0.000000000000000000, -0.2355298848897586228, -0.9718671068226442111 ) ) ;
#21993 = CARTESIAN_POINT ( 'NONE',  ( 0.3040950598368152291, 9.229598020917798351, -8.072385578287377683 ) ) ;
#21995 = EDGE_CURVE ( 'NONE', #7316, #20098, #11076, .T. ) ;
#21994 = CARTESIAN_POINT ( 'NONE',  ( 2.827825597296804716, -8.278234963587674855, -3.592949031604497634 ) ) ;
#21996 = DIRECTION ( 'NONE',  ( 0.000000000000000000, 0.01356324068817998940, -0.9999080150203990547 ) ) ;
#21997 = CARTESIAN_POINT ( 'NONE',  ( 0.2648978790185602672, 4.312320170909236694, 11.46165506714229565 ) ) ;
#21998 = EDGE_LOOP ( 'NONE', ( #26670, #29606, #56459, #26822 ) ) ;
#21999 = DIRECTION ( 'NONE',  ( 0.000000000000000000, 0.3807014730195151797, -0.9246979985058750851 ) ) ;
#22000 = ORIENTED_EDGE ( 'NONE', *, *, #25667, .F. ) ;
#22001 = AXIS2_PLACEMENT_3D ( 'NONE', #34664, #55637, #49662 ) ;
#22002 = DIRECTION ( 'NONE',  ( -1.000000000000000000, 0.000000000000000000, -0.000000000000000000 ) ) ;
#22003 = EDGE_CURVE ( 'NONE', #35347, #32947, #62331, .T. ) ;
#22004 = DIRECTION ( 'NONE',  ( 1.000000000000000000, -0.000000000000000000, 0.000000000000000000 ) ) ;
#22005 = ORIENTED_EDGE ( 'NONE', *, *, #23920, .T. ) ;
#22006 = LINE ( 'NONE', #32303, #29649 ) ;
#22007 = CARTESIAN_POINT ( 'NONE',  ( 0.3610902822527166656, 12.04327049858143539, -2.389900346487964899 ) ) ;
#22008 = CARTESIAN_POINT ( 'NONE',  ( -36.00000000000000711, -10.68873102412847764, 6.950793414699757200 ) ) ;
#22009 = ORIENTED_EDGE ( 'NONE', *, *, #49853, .F. ) ;
#22010 = VERTEX_POINT ( 'NONE', #62025 ) ;
#22011 = CIRCLE ( 'NONE', #47511, 4.999999999999999112 ) ;
#22012 = DIRECTION ( 'NONE',  ( -1.000000000000000000, -0.000000000000000000, 0.000000000000000000 ) ) ;
#22013 = EDGE_CURVE ( 'NONE', #35492, #15725, #16394, .T. ) ;
#22014 = VERTEX_POINT ( 'NONE', #57704 ) ;
#22015 = DIRECTION ( 'NONE',  ( 0.000000000000000000, -0.01356324068817991828, 0.9999080150203990547 ) ) ;
#22016 = EDGE_CURVE ( 'NONE', #11898, #42832, #4733, .T. ) ;
#22017 = CARTESIAN_POINT ( 'NONE',  ( 2.000000000000001776, -2.664846396702537312, 6.404188155572974495 ) ) ;
#22018 = CARTESIAN_POINT ( 'NONE',  ( 0.2648978790185593790, -10.53870023327859151, -6.237101853238657512 ) ) ;
#22019 = DIRECTION ( 'NONE',  ( 0.000000000000000000, -0.01356324068817991828, 0.9999080150203990547 ) ) ;
#22020 = DIRECTION ( 'NONE',  ( 0.000000000000000000, 0.000000000000000000, 1.000000000000000000 ) ) ;
#22021 = EDGE_LOOP ( 'NONE', ( #39554, #47293, #1305, #34094 ) ) ;
#22022 = CARTESIAN_POINT ( 'NONE',  ( 24.82652845881425208, -8.390869743685021476, -8.578654028722157321 ) ) ;
#22023 = LINE ( 'NONE', #27334, #9663 ) ;
#22024 = CARTESIAN_POINT ( 'NONE',  ( -35.00000000000000000, 7.251710744571578715, 9.240395740215660680 ) ) ;
#22025 = CARTESIAN_POINT ( 'NONE',  ( 0.3053067050349174139, -5.928821939311855083, -10.73055518945194819 ) ) ;
#22026 = FACE_OUTER_BOUND ( 'NONE', #6466, .T. ) ;
#22027 = CARTESIAN_POINT ( 'NONE',  ( 1.283627346226426713, 4.817767733507119843, 11.62704807385632044 ) ) ;
#22028 = CARTESIAN_POINT ( 'NONE',  ( 2.440552418640498988, 5.099602138956282893, -5.770332237304396372 ) ) ;
#22029 = VECTOR ( 'NONE', #64574, 1000.000000000000000 ) ;
#22030 = EDGE_CURVE ( 'NONE', #30538, #63048, #63313, .T. ) ;
#22031 = ORIENTED_EDGE ( 'NONE', *, *, #24030, .F. ) ;
#22032 = DIRECTION ( 'NONE',  ( 0.3939253465568943735, 0.3052156353794266974, 0.8669868725995586445 ) ) ;
#22033 = B_SPLINE_CURVE_WITH_KNOTS ( 'NONE', 3,
 ( #18347, #48291, #2738, #22997, #18986, #13010, #59546, #9004, #13977, #34268, #29287, #53596, #10621, #14616, #40564, #24622 ),
 .UNSPECIFIED., .F., .F.,
 ( 4, 3, 3, 3, 3, 4 ),
 ( 0.000000000000000000, 0.0003017745587525249760, 0.0006035491769808762341, 0.0009053241094668206933, 0.001207275924539024173, 0.001510325902531031326 ),
 .UNSPECIFIED. ) ;
#22034 = CARTESIAN_POINT ( 'NONE',  ( 3.347841273039249721, -10.61118957148187825, 8.345816669330455184 ) ) ;
#22035 = ORIENTED_EDGE ( 'NONE', *, *, #921, .T. ) ;
#22036 = EDGE_CURVE ( 'NONE', #30305, #18413, #51732, .T. ) ;
#22037 = CARTESIAN_POINT ( 'NONE',  ( 1.020182472820991837, 10.59341968305504089, 6.631405022218979539 ) ) ;
#22038 = LINE ( 'NONE', #37328, #17282 ) ;
#22039 = ORIENTED_EDGE ( 'NONE', *, *, #60621, .F. ) ;
#22040 = CARTESIAN_POINT ( 'NONE',  ( -22.30625920655495165, -1.672644928563074451, 3.403091720605004866 ) ) ;
#22041 = ORIENTED_EDGE ( 'NONE', *, *, #64055, .T. ) ;
#22042 = EDGE_CURVE ( 'NONE', #63998, #15877, #16575, .T. ) ;
#22043 = CARTESIAN_POINT ( 'NONE',  ( 0.3164563675027631251, -5.922187299605712774, 10.73846246126247550 ) ) ;
#22044 = EDGE_LOOP ( 'NONE', ( #20462, #36546, #31922, #18012 ) ) ;
#22045 = VECTOR ( 'NONE', #11211, 1000.000000000000000 ) ;
#22046 = ORIENTED_EDGE ( 'NONE', *, *, #30555, .T. ) ;
#22047 = CARTESIAN_POINT ( 'NONE',  ( 35.00000000000000000, 4.705694406421931860E-17, -3.469127814946512892E-15 ) ) ;
#22048 = EDGE_CURVE ( 'NONE', #34279, #39829, #65218, .T. ) ;
#22049 = CIRCLE ( 'NONE', #37991, 12.75000000000000178 ) ;
#22050 = ORIENTED_EDGE ( 'NONE', *, *, #22772, .F. ) ;
#22051 = DIRECTION ( 'NONE',  ( -1.000000000000000000, 0.000000000000000000, 0.000000000000000000 ) ) ;
#22052 = CARTESIAN_POINT ( 'NONE',  ( 0.9296196016843242260, -11.56707937094521732, -4.652334946095537660 ) ) ;
#22053 = CARTESIAN_POINT ( 'NONE',  ( 2.000000000000001776, 4.915517050588409376, 4.717154614762108622 ) ) ;
#22054 = FACE_OUTER_BOUND ( 'NONE', #7721, .T. ) ;
#22055 = ORIENTED_EDGE ( 'NONE', *, *, #23660, .T. ) ;
#22056 = CARTESIAN_POINT ( 'NONE',  ( 1.730912674848539366E-15, -30.50000000000000000, 14.13397459621556251 ) ) ;
#22057 = CARTESIAN_POINT ( 'NONE',  ( 7.742519806647712777, -28.58895386040045494, 10.54525737088725101 ) ) ;
#22059 = ORIENTED_EDGE ( 'NONE', *, *, #60555, .T. ) ;
#22058 = CARTESIAN_POINT ( 'NONE',  ( -26.34600911009608382, 10.72077307324429718, 5.391900231479520578 ) ) ;
#22060 = CARTESIAN_POINT ( 'NONE',  ( 25.05309951391468459, 8.823569016628493245, -8.132934882857099979 ) ) ;
#22061 = EDGE_CURVE ( 'NONE', #9614, #48986, #7901, .T. ) ;
#22062 = VERTEX_POINT ( 'NONE', #36747 ) ;
#22063 = CARTESIAN_POINT ( 'NONE',  ( 0.2653141334712584287, 9.352759824582610904, -7.905403790036874767 ) ) ;
#22064 = ORIENTED_EDGE ( 'NONE', *, *, #31349, .F. ) ;
#22065 = CARTESIAN_POINT ( 'NONE',  ( 21.50270529625529647, -11.33978786238144032, -3.930893046708287653 ) ) ;
#22066 = CARTESIAN_POINT ( 'NONE',  ( 35.00000000000000000, 4.309077947445811851, 10.92721691015450780 ) ) ;
#22067 = CARTESIAN_POINT ( 'NONE',  ( -35.00000000000000000, 0.4993900848167411310, 12.17626345777664021 ) ) ;
#22068 = ORIENTED_EDGE ( 'NONE', *, *, #29680, .F. ) ;
#22069 = CARTESIAN_POINT ( 'NONE',  ( 35.00000000000000000, 4.705694406421931860E-17, -3.469127814946512892E-15 ) ) ;
#22070 = CARTESIAN_POINT ( 'NONE',  ( 2.177405672431969919, -11.12610351585405333, -1.276675186593726030 ) ) ;
#22071 = CARTESIAN_POINT ( 'NONE',  ( 2.241451721903217731, -5.887257931662872146, 4.860585618235946370 ) ) ;
#22072 = ORIENTED_EDGE ( 'NONE', *, *, #41479, .T. ) ;
#22073 = EDGE_LOOP ( 'NONE', ( #15613, #59793, #31016, #10775 ) ) ;
#22074 = CARTESIAN_POINT ( 'NONE',  ( 2.963017218115620466, 7.679262289252045015, 1.744728040076931830 ) ) ;
#22075 = VERTEX_POINT ( 'NONE', #22431 ) ;
#22076 = EDGE_CURVE ( 'NONE', #40304, #44716, #62048, .T. ) ;
#22077 = ADVANCED_FACE ( 'NONE', ( #57041 ), #1181, .T. ) ;
#22078 = VERTEX_POINT ( 'NONE', #58026 ) ;
#22079 = CARTESIAN_POINT ( 'NONE',  ( 35.00000000000000000, -6.917234959366766134, 9.493370459201765144 ) ) ;
#22080 = DIRECTION ( 'NONE',  ( -0.9606638835031803270, 0.06908842350339206018, 0.2689826995745341343 ) ) ;
#22081 = CARTESIAN_POINT ( 'NONE',  ( 2.241352910868909643, 7.202080440908774861, -2.532612177304371048 ) ) ;
#22082 = DIRECTION ( 'NONE',  ( 1.000000000000000000, 0.000000000000000000, 0.000000000000000000 ) ) ;
#22083 = ADVANCED_FACE ( 'NONE', ( #12438 ), #55739, .F. ) ;
#22084 = CARTESIAN_POINT ( 'NONE',  ( 2.000000000000001776, 0.000000000000000000, 0.000000000000000000 ) ) ;
#22085 = AXIS2_PLACEMENT_3D ( 'NONE', #33450, #4174, #23471 ) ;
#22086 = DIRECTION ( 'NONE',  ( 1.000000000000000000, 0.000000000000000000, 0.000000000000000000 ) ) ;
#22087 = EDGE_CURVE ( 'NONE', #64733, #28659, #6341, .T. ) ;
#22088 = CARTESIAN_POINT ( 'NONE',  ( -22.27711351828769892, -0.8770428151440446962, -3.575417021793779515 ) ) ;
#22089 = EDGE_CURVE ( 'NONE', #26102, #43663, #9477, .T. ) ;
#22090 = AXIS2_PLACEMENT_3D ( 'NONE', #58414, #38447, #37461 ) ;
#22091 = ORIENTED_EDGE ( 'NONE', *, *, #38212, .F. ) ;
#22092 = ADVANCED_FACE ( 'NONE', ( #1632 ), #21905, .F. ) ;
#22093 = CARTESIAN_POINT ( 'NONE',  ( -11.40165637462999904, -7.508992741355383416, 25.00000000000000000 ) ) ;
#22094 = AXIS2_PLACEMENT_3D ( 'NONE', #3802, #7781, #29361 ) ;
#22095 = CARTESIAN_POINT ( 'NONE',  ( 35.00000000000000000, -11.70009620280412399, -1.039216533672868481 ) ) ;
#22096 = AXIS2_PLACEMENT_3D ( 'NONE', #22084, #42342, #62316 ) ;
#22097 = DIRECTION ( 'NONE',  ( 0.000000000000000000, -0.3807014730195086849, 0.9246979985058776386 ) ) ;
#22098 = CARTESIAN_POINT ( 'NONE',  ( -35.00000000000000000, 9.926225166347114381, -6.280308599560036065 ) ) ;
#22099 = DIRECTION ( 'NONE',  ( 0.000000000000000000, 0.1740410799127612429, 0.9847383929261617208 ) ) ;
#22100 = CARTESIAN_POINT ( 'NONE',  ( 23.11472949692741352, -3.958498414078114092, -12.90974724811009366 ) ) ;
#22101 = DIRECTION ( 'NONE',  ( -1.000000000000000000, 0.000000000000000000, 0.000000000000000000 ) ) ;
#22102 = VERTEX_POINT ( 'NONE', #47501 ) ;
#22103 = CARTESIAN_POINT ( 'NONE',  ( -27.08423805673873375, 0.5302040644010427295, 2.229265646063304018 ) ) ;
#22104 = CARTESIAN_POINT ( 'NONE',  ( 0.2869720083484365580, -1.922200714744079164, -12.10169797402142500 ) ) ;
#22105 = CARTESIAN_POINT ( 'NONE',  ( 0.2638984909335720941, -12.24571285024409129, 0.1991813963113568953 ) ) ;
#22106 = DIRECTION ( 'NONE',  ( 0.000000000000000000, -0.9346839223284501008, 0.3554799084909069928 ) ) ;
#22107 = EDGE_CURVE ( 'NONE', #281, #18433, #13378, .T. ) ;
#22108 = FACE_OUTER_BOUND ( 'NONE', #21021, .T. ) ;
#22109 = CARTESIAN_POINT ( 'NONE',  ( 12.52750123246316072, 0.4973700281276248192, 13.49083477977253764 ) ) ;
#22110 = ORIENTED_EDGE ( 'NONE', *, *, #16641, .F. ) ;
#22111 = CIRCLE ( 'NONE', #27421, 5.000000000000000888 ) ;
#22112 = CARTESIAN_POINT ( 'NONE',  ( 1.948354844646350115, 8.685970062895311372, -8.228891433297251368 ) ) ;
#22113 = CARTESIAN_POINT ( 'NONE',  ( -27.74658222974374411, -12.59936487573947517, -4.856608172635154652 ) ) ;
#22114 = CARTESIAN_POINT ( 'NONE',  ( 2.241311220309522234, -4.835827934491081059, -5.907514893712877857 ) ) ;
#22115 = CARTESIAN_POINT ( 'NONE',  ( 0.7400311444011719031, -12.27261279799597915, -1.803686700615534377 ) ) ;
#22116 = ORIENTED_EDGE ( 'NONE', *, *, #55178, .T. ) ;
#22117 = DIRECTION ( 'NONE',  ( -1.000000000000000000, 0.000000000000000000, -0.000000000000000000 ) ) ;
#22118 = CARTESIAN_POINT ( 'NONE',  ( 5.514624014163232779, 0.003060352188290776324, 0.002789935220458057957 ) ) ;
#22119 = EDGE_CURVE ( 'NONE', #24257, #43073, #15335, .T. ) ;
#22121 = EDGE_LOOP ( 'NONE', ( #38980, #44151, #1705, #26842 ) ) ;
#22120 = CARTESIAN_POINT ( 'NONE',  ( 0.000000000000000000, 5.997115278587632936, 3.485633455389514523 ) ) ;
#22122 = LINE ( 'NONE', #23112, #58637 ) ;
#22123 = CIRCLE ( 'NONE', #30609, 7.499999999999988454 ) ;
#22124 = CARTESIAN_POINT ( 'NONE',  ( 35.00000000000000000, 4.705694406421931860E-17, -3.469127814946512892E-15 ) ) ;
#22125 = EDGE_LOOP ( 'NONE', ( #11203, #28279, #57988, #757 ) ) ;
#22126 = CARTESIAN_POINT ( 'NONE',  ( 37.00000000000000711, 4.705694406421931860E-17, -3.469127814946512892E-15 ) ) ;
#22127 = DIRECTION ( 'NONE',  ( 0.000000000000000000, 0.01356324068817991828, -0.9999080150203990547 ) ) ;
#22128 = AXIS2_PLACEMENT_3D ( 'NONE', #31199, #56464, #16227 ) ;
#22129 = CARTESIAN_POINT ( 'NONE',  ( -37.00000000000000711, 0.000000000000000000, 0.000000000000000000 ) ) ;
#22130 = CIRCLE ( 'NONE', #5161, 5.000000000000000000 ) ;
#22131 = LINE ( 'NONE', #62681, #47842 ) ;
#22132 =( BOUNDED_SURFACE ( )  B_SPLINE_SURFACE ( 3, 1, ( 
 ( #3278, #7942 ),
 ( #53498, #24191 ),
 ( #8251, #35781 ),
 ( #55771, #61390 ) ),
 .UNSPECIFIED., .F., .F., .F. ) 
 B_SPLINE_SURFACE_WITH_KNOTS ( ( 4, 4 ),
 ( 2, 2 ),
 ( 0.000000000000000000, 1.000000000000000000 ),
 ( 0.000000000000000000, 1.000000000000000000 ),
 .UNSPECIFIED. ) 
 GEOMETRIC_REPRESENTATION_ITEM ( )  RATIONAL_B_SPLINE_SURFACE ( (
 ( 1.000000000000000000, 1.000000000000000000),
 ( 0.9932032654565553509, 0.8386279382598740284),
 ( 0.9932032654565553509, 0.8386279382598740284),
 ( 1.000000000000000000, 1.000000000000000000) ) ) 
 REPRESENTATION_ITEM ( '' )  SURFACE ( )  );
#22133 = DIRECTION ( 'NONE',  ( -1.000000000000000000, 0.000000000000000000, 0.000000000000000000 ) ) ;
#22134 = CARTESIAN_POINT ( 'NONE',  ( 0.6473888112830245012, 11.73602097806020517, 3.920507224439127025 ) ) ;
#22136 = ORIENTED_EDGE ( 'NONE', *, *, #22619, .T. ) ;
#22135 = CARTESIAN_POINT ( 'NONE',  ( -35.00000000000000000, -3.827046518385164742, 11.56998259273176188 ) ) ;
#22137 = CARTESIAN_POINT ( 'NONE',  ( 1.198791140420665702, 4.776130053253731411, -11.61358959650694089 ) ) ;
#22138 = ADVANCED_FACE ( 'NONE', ( #60088 ), #24177, .T. ) ;
#22139 = ORIENTED_EDGE ( 'NONE', *, *, #40536, .T. ) ;
#22140 = DIRECTION ( 'NONE',  ( -1.000000000000000000, -0.000000000000000000, 0.000000000000000000 ) ) ;
#22141 = VERTEX_POINT ( 'NONE', #43813 ) ;
#22142 = AXIS2_PLACEMENT_3D ( 'NONE', #6238, #62393, #16851 ) ;
#22143 = CYLINDRICAL_SURFACE ( 'NONE', #28407, 5.000000000000000888 ) ;
#22144 = CYLINDRICAL_SURFACE ( 'NONE', #41750, 12.75000000000000178 ) ;
#22145 = CARTESIAN_POINT ( 'NONE',  ( -39.58329824467849534, -1.898237318462467682, 19.07749194152998484 ) ) ;
#22146 = CARTESIAN_POINT ( 'NONE',  ( -27.08426571771018487, 0.9198084705429482311, -2.098821047392056549 ) ) ;
#22147 = ORIENTED_EDGE ( 'NONE', *, *, #3894, .F. ) ;
#22148 = LINE ( 'NONE', #31476, #36816 ) ;
#22149 = CARTESIAN_POINT ( 'NONE',  ( 0.4613984246114877785, -3.943860067443726525, 11.66278164635733461 ) ) ;
#22150 = ORIENTED_EDGE ( 'NONE', *, *, #47744, .F. ) ;
#22151 = VERTEX_POINT ( 'NONE', #19849 ) ;
#22152 = DIRECTION ( 'NONE',  ( 0.000000000000000000, -0.01356324068817998940, 0.9999080150203990547 ) ) ;
#22153 = EDGE_LOOP ( 'NONE', ( #51963, #54193, #36115, #11900 ) ) ;
#22154 = CARTESIAN_POINT ( 'NONE',  ( 2.000000000000001776, 3.230174184210159893, -5.998318953995314118 ) ) ;
#22155 = DIRECTION ( 'NONE',  ( -0.3865475372811021937, -0.8730852074079720193, -0.2971585806051939005 ) ) ;
#22156 = DIRECTION ( 'NONE',  ( 0.000000000000000000, 0.01356324068817998940, -0.9999080150203990547 ) ) ;
#22157 = EDGE_CURVE ( 'NONE', #48416, #10957, #10078, .T. ) ;
#22158 = DIRECTION ( 'NONE',  ( 1.000000000000000000, -0.000000000000000000, 0.000000000000000000 ) ) ;
#22159 = LINE ( 'NONE', #33767, #29866 ) ;
#22160 = CARTESIAN_POINT ( 'NONE',  ( 3.047904605210428386, -7.845751380824987464, 0.9519317672906529859 ) ) ;
#22161 = AXIS2_PLACEMENT_3D ( 'NONE', #28001, #46971, #56958 ) ;
#22162 = EDGE_CURVE ( 'NONE', #29549, #40046, #57805, .T. ) ;
#22163 = CARTESIAN_POINT ( 'NONE',  ( 35.00000000000000000, 4.705694406421931860E-17, -3.469127814946512892E-15 ) ) ;
#22164 = ORIENTED_EDGE ( 'NONE', *, *, #558, .F. ) ;
#22165 = LINE ( 'NONE', #58762, #46487 ) ;
#22166 = VERTEX_POINT ( 'NONE', #19193 ) ;
#22167 = EDGE_CURVE ( 'NONE', #12197, #58057, #45072, .T. ) ;
#22168 = CYLINDRICAL_SURFACE ( 'NONE', #1335, 4.999999999999999112 ) ;
#22169 = CARTESIAN_POINT ( 'NONE',  ( 0.2648978790185593790, 9.465406350830713578, -7.769924372105106336 ) ) ;
#22170 = FACE_OUTER_BOUND ( 'NONE', #23208, .T. ) ;
#22171 = CARTESIAN_POINT ( 'NONE',  ( 0.2648978790185584908, 10.67083876753500427, -6.008231198268870976 ) ) ;
#22172 = VECTOR ( 'NONE', #35203, 1000.000000000000000 ) ;
#22173 = EDGE_LOOP ( 'NONE', ( #11870, #27823, #18892, #26069 ) ) ;
#22174 = ORIENTED_EDGE ( 'NONE', *, *, #41402, .T. ) ;
#22175 = CARTESIAN_POINT ( 'NONE',  ( -27.08579483061202708, 0.2015567301747612228, 2.287150433979697528 ) ) ;
#22176 = STYLED_ITEM ( 'NONE', ( #49257 ), #30113 ) ;
#22177 = ORIENTED_EDGE ( 'NONE', *, *, #7110, .F. ) ;
#22178 = CARTESIAN_POINT ( 'NONE',  ( 0.3675815128205894289, 7.689697408877401941, -9.574637318041888889 ) ) ;
#22179 = CARTESIAN_POINT ( 'NONE',  ( 0.3665391374699464300, 11.62960183138732440, -3.952034409876179932 ) ) ;
#22180 = VECTOR ( 'NONE', #32534, 1000.000000000000000 ) ;
#22181 = CARTESIAN_POINT ( 'NONE',  ( 2.251139882113970980, 4.813633939919418125, 5.929826121559315766 ) ) ;
#22182 = DIRECTION ( 'NONE',  ( 1.000000000000000000, -0.000000000000000000, 0.000000000000000000 ) ) ;
#22183 = ORIENTED_EDGE ( 'NONE', *, *, #14390, .F. ) ;
#22184 = CARTESIAN_POINT ( 'NONE',  ( 2.835339799623972645, 2.367573116406979317, 7.466040501142034991 ) ) ;
#22185 = DIRECTION ( 'NONE',  ( 1.000000000000000000, 0.000000000000000000, 0.000000000000000000 ) ) ;
#22186 = CARTESIAN_POINT ( 'NONE',  ( -35.00000000000000000, 0.000000000000000000, 0.000000000000000000 ) ) ;
#22187 = DIRECTION ( 'NONE',  ( -0.000000000000000000, -1.000000000000000000, -0.000000000000000000 ) ) ;
#22188 = EDGE_CURVE ( 'NONE', #55976, #31867, #47212, .T. ) ;
#22189 = CARTESIAN_POINT ( 'NONE',  ( 0.000000000000000000, 6.883677378339475794, 0.8544109087186002593 ) ) ;
#22190 = ADVANCED_FACE ( 'NONE', ( #44444 ), #34482, .T. ) ;
#22191 = CARTESIAN_POINT ( 'NONE',  ( -35.00000000000000000, -0.2661492558804205988, 12.18359334611896472 ) ) ;
#22192 = ORIENTED_EDGE ( 'NONE', *, *, #29704, .F. ) ;
#22193 = CARTESIAN_POINT ( 'NONE',  ( -11.91618201078742523, -29.31229682091840871, -6.386286639733476100 ) ) ;
#22194 = ORIENTED_EDGE ( 'NONE', *, *, #63157, .T. ) ;
#22195 = CARTESIAN_POINT ( 'NONE',  ( -35.04643116707788408, -0.01156612771643569793, -0.003844232202723438241 ) ) ;
#22196 = CARTESIAN_POINT ( 'NONE',  ( 2.665405856346786173, 9.304623509366205525, 2.226920474533411021 ) ) ;
#22197 = DIRECTION ( 'NONE',  ( -1.000000000000000000, 0.000000000000000000, 0.000000000000000000 ) ) ;
#22198 = EDGE_CURVE ( 'NONE', #33015, #19363, #3696, .T. ) ;
#22199 = DIRECTION ( 'NONE',  ( 1.000000000000000000, 0.000000000000000000, -0.000000000000000000 ) ) ;
#22200 = DIRECTION ( 'NONE',  ( 0.000000000000000000, 0.1764146379942750364, 0.9843159429275484262 ) ) ;
#22201 = AXIS2_PLACEMENT_3D ( 'NONE', #20216, #19893, #49831 ) ;
#22202 = ORIENTED_EDGE ( 'NONE', *, *, #4217, .T. ) ;
#22203 = ORIENTED_EDGE ( 'NONE', *, *, #21347, .T. ) ;
#22204 = ORIENTED_EDGE ( 'NONE', *, *, #53553, .T. ) ;
#22205 = CARTESIAN_POINT ( 'NONE',  ( 35.00000000000000000, 1.262958560998929558, 12.12087942037208066 ) ) ;
#22206 = CARTESIAN_POINT ( 'NONE',  ( -22.27834755396594346, 3.434702243602638205, 1.338300169228680003 ) ) ;
#22207 = CARTESIAN_POINT ( 'NONE',  ( -35.00000000000000000, -4.983891302653499444, -11.73555825188281609 ) ) ;
#22208 = DIRECTION ( 'NONE',  ( -1.000000000000000000, 0.000000000000000000, 0.000000000000000000 ) ) ;
#22210 = DIRECTION ( 'NONE',  ( -1.000000000000000000, 0.000000000000000000, 0.000000000000000000 ) ) ;
#22209 = AXIS2_PLACEMENT_3D ( 'NONE', #37878, #42861, #54158 ) ;
#22211 = CARTESIAN_POINT ( 'NONE',  ( 2.276905613633649406, 7.555317002492091483, 1.175741125184106339 ) ) ;
#22212 = CARTESIAN_POINT ( 'NONE',  ( -17.08916676964391357, 2.790706569880187615, -13.20909463602864697 ) ) ;
#22213 = ORIENTED_EDGE ( 'NONE', *, *, #20340, .F. ) ;
#22214 = EDGE_CURVE ( 'NONE', #52362, #53221, #52532, .T. ) ;
#22215 = EDGE_CURVE ( 'NONE', #3010, #60035, #18548, .T. ) ;
#22216 = ORIENTED_EDGE ( 'NONE', *, *, #13488, .T. ) ;
#22217 = CARTESIAN_POINT ( 'NONE',  ( 1.014383007554952254, -5.859361736620408045, 11.03701226956414239 ) ) ;
#22218 = ORIENTED_EDGE ( 'NONE', *, *, #62412, .T. ) ;
#22219 =( LENGTH_UNIT ( ) NAMED_UNIT ( * ) SI_UNIT ( .MILLI., .METRE. ) );
#22220 = EDGE_CURVE ( 'NONE', #45080, #22263, #51490, .T. ) ;
#22221 = CARTESIAN_POINT ( 'NONE',  ( 22.80864547236593154, -11.57366291690524029, -6.957251879747434309 ) ) ;
#22222 = VECTOR ( 'NONE', #59753, 1000.000000000000000 ) ;
#22223 = DIRECTION ( 'NONE',  ( 0.000000000000000000, 0.01356324068818000848, -0.9999080150203990547 ) ) ;
#22224 = CARTESIAN_POINT ( 'NONE',  ( 35.00000000000000000, -6.303578524887018197, -10.42955799785318050 ) ) ;
#22226 = VERTEX_POINT ( 'NONE', #24503 ) ;
#22225 = CIRCLE ( 'NONE', #10536, 2.899999999999996803 ) ;
#22227 = CYLINDRICAL_SURFACE ( 'NONE', #5747, 12.74999999999999822 ) ;
#22228 = CARTESIAN_POINT ( 'NONE',  ( -17.34314652423486081, -29.56569286319712475, -9.163921882788894635 ) ) ;
#22229 = CARTESIAN_POINT ( 'NONE',  ( 0.000000000000000000, 0.08317740279931498670, 7.499538753794337431 ) ) ;
#22230 = VERTEX_POINT ( 'NONE', #65061 ) ;
#22231 = VERTEX_POINT ( 'NONE', #44778 ) ;
#22232 = DIRECTION ( 'NONE',  ( 0.000000000000000000, -0.8696919319575129315, -0.4935949184179356242 ) ) ;
#22233 = VERTEX_POINT ( 'NONE', #19536 ) ;
#22234 = EDGE_LOOP ( 'NONE', ( #48998, #4158, #7796, #46896, #42266, #3532, #62419, #60872, #8308, #41330, #23198, #16091, #13478, #63003, #56055, #9018, #57189, #20834, #13446, #54650, #32030, #59606, #65526, #27816, #14108, #13671, #45142, #53374, #40057, #45363, #16993, #36125, #55153, #45366, #60924, #2226, #51592, #28340, #14821, #28565, #46595, #22059, #27874, #34223, #41008, #14061, #52135, #17158, #20888, #43231, #17144, #16529, #59209, #57243, #14465, #56479, #14317, #40834, #60989, #2358, #20913, #14478, #39348, #22203, #21249, #39234, #45015, #63845, #20181, #28827, #19131, #33835, #46792, #18014, #13064, #44013, #49887, #33977, #41359, #17779, #36718, #56453, #16421, #42167, #50137, #37921, #43053, #40605, #29819, #24945, #47945, #28476, #1676, #58144, #17852, #2619, #42979, #52219, #50250, #55135, #24862, #57472, #50195, #7947, #65616, #15730, #52335, #35292, #25648, #65270, #61019, #7503, #55525, #2131, #62274, #847, #28419, #63288, #61476, #20639, #18665, #48481, #17311, #34800, #23993, #3062, #63679, #13452, #35162, #12559, #52784, #5659, #55332, #58432, #49429, #26622, #44206, #55917, #5287, #56775, #43104, #28705, #55985, #48643, #55884, #63126, #15425, #51239, #29327, #3737, #8453, #26790, #64561, #44886, #27079, #35226, #14722, #38543, #31497, #52331, #42141, #15450, #37340, #29401, #37905, #61813, #39406, #11843, #14456, #26560, #59442, #29321, #56860, #18579, #1180, #7258, #33531, #12642, #52215, #36499, #18333, #11120, #58600, #42521, #49869, #15287, #59514, #5219, #59933, #22039, #36713, #31832, #65301, #55872, #1195, #41869, #23976, #52320, #7671, #12175, #2737, #14385, #52884, #47558, #22721, #65803, #49582, #13276, #57821, #23880, #4512, #12189, #62858, #53243, #38892, #49900, #54922, #5984, #39327, #20259, #3759, #4834, #27601, #41200, #39757, #24484, #15562, #54440, #27959, #10381, #49320, #29187, #16525, #40459, #31298, #63608, #4937 ) ) ;
#22235 = DIRECTION ( 'NONE',  ( 1.000000000000000000, 0.000000000000000000, -0.000000000000000000 ) ) ;
#22236 = ORIENTED_EDGE ( 'NONE', *, *, #21015, .T. ) ;
#22237 = VECTOR ( 'NONE', #13320, 1000.000000000000000 ) ;
#22238 = ORIENTED_EDGE ( 'NONE', *, *, #31967, .T. ) ;
#22239 = CARTESIAN_POINT ( 'NONE',  ( 0.3164563675027637912, 4.419430877662341217, 11.43920928915625623 ) ) ;
#22240 = ADVANCED_FACE ( 'NONE', ( #50119 ), #4575, .T. ) ;
#22241 = DIRECTION ( 'NONE',  ( -1.000000000000000000, -0.000000000000000000, -0.000000000000000000 ) ) ;
#22242 = FACE_OUTER_BOUND ( 'NONE', #44761, .T. ) ;
#22243 = CARTESIAN_POINT ( 'NONE',  ( -27.32343372485685862, 1.625341394141133655, -2.534722478175129190 ) ) ;
#22244 = CARTESIAN_POINT ( 'NONE',  ( 5.536195898058073439, 0.005266167600747600520, 0.006672323185952732348 ) ) ;
#22245 = EDGE_CURVE ( 'NONE', #38335, #26398, #54671, .T. ) ;
#22246 = DIRECTION ( 'NONE',  ( -1.000000000000000000, 0.000000000000000000, 0.000000000000000000 ) ) ;
#22247 = VERTEX_POINT ( 'NONE', #45435 ) ;
#22248 = LINE ( 'NONE', #62475, #12584 ) ;
#22249 = CARTESIAN_POINT ( 'NONE',  ( 2.440552418640466126, 4.797131306497566250, 6.024135401262375566 ) ) ;
#22250 = CARTESIAN_POINT ( 'NONE',  ( 37.00000000000000711, 1.771820996347156507, -11.61175578952786935 ) ) ;
#22251 = DIRECTION ( 'NONE',  ( 1.000000000000000000, 0.000000000000000000, 0.000000000000000000 ) ) ;
#22252 = DIRECTION ( 'NONE',  ( 0.000000000000000000, -0.01356324068817998940, 0.9999080150203990547 ) ) ;
#22253 = LINE ( 'NONE', #22933, #61026 ) ;
#22254 = CIRCLE ( 'NONE', #1045, 12.74999999999999822 ) ;
#22255 = ORIENTED_EDGE ( 'NONE', *, *, #40737, .T. ) ;
#22256 = CARTESIAN_POINT ( 'NONE',  ( 1.719304012338199517, 0.000000000000000000, 0.000000000000000000 ) ) ;
#22257 = VERTEX_POINT ( 'NONE', #568 ) ;
#22258 = CYLINDRICAL_SURFACE ( 'NONE', #8358, 5.000000000000000888 ) ;
#22259 = CARTESIAN_POINT ( 'NONE',  ( 0.2759803524722198587, -0.1894460813476845917, 12.24828167798667877 ) ) ;
#22260 = CARTESIAN_POINT ( 'NONE',  ( 17.75832895199378214, -29.67262258703657096, 8.626345146652846907 ) ) ;
#22261 = CARTESIAN_POINT ( 'NONE',  ( -27.08429572838383947, -0.5764601019425836803, -2.217805374070540125 ) ) ;
#22262 = CARTESIAN_POINT ( 'NONE',  ( 2.268878695253353950, -6.692359410363624583, 3.692782103667259452 ) ) ;
#22263 = VERTEX_POINT ( 'NONE', #65700 ) ;
#22264 = LINE ( 'NONE', #17631, #54739 ) ;
#22265 = CARTESIAN_POINT ( 'NONE',  ( 0.3675815128205894289, 11.44679196252409348, 4.447030445008218535 ) ) ;
#22266 = DIRECTION ( 'NONE',  ( 1.000000000000000000, 0.000000000000000000, 0.000000000000000000 ) ) ;
#22267 = CARTESIAN_POINT ( 'NONE',  ( 26.17129964821461385, 11.44745868472665684, 3.602463285258926895 ) ) ;
#22268 = CIRCLE ( 'NONE', #12710, 5.000000000000000888 ) ;
#22269 = CIRCLE ( 'NONE', #27585, 5.000000000000000888 ) ;
#22270 = EDGE_CURVE ( 'NONE', #4031, #44052, #20830, .T. ) ;
#22271 = FACE_OUTER_BOUND ( 'NONE', #64211, .T. ) ;
#22272 = ORIENTED_EDGE ( 'NONE', *, *, #33076, .T. ) ;
#22273 = CARTESIAN_POINT ( 'NONE',  ( 0.2655924914740778742, -9.352877839710654229, 7.905499957109207720 ) ) ;
#22274 = PRODUCT_DEFINITION_SHAPE ( 'NONE', 'NONE',  #57568 ) ;
#22275 = CARTESIAN_POINT ( 'NONE',  ( 5.530133899448235191, 0.004396748047611225528, 0.01536822665454896930 ) ) ;
#22276 = ADVANCED_FACE ( 'NONE', ( #30471 ), #5896, .T. ) ;
#22277 = ORIENTED_EDGE ( 'NONE', *, *, #33206, .T. ) ;
#22278 = ORIENTED_EDGE ( 'NONE', *, *, #41891, .F. ) ;
#22279 = CARTESIAN_POINT ( 'NONE',  ( 2.844750968616207576, -6.613363922490621327, 4.202329849280634910 ) ) ;
#22280 = DIRECTION ( 'NONE',  ( 1.000000000000000000, -0.000000000000000000, -0.000000000000000000 ) ) ;
#22281 = CARTESIAN_POINT ( 'NONE',  ( 0.9232167919969205272, -7.691547553333184517, 9.809608956680843761 ) ) ;
#22282 = DIRECTION ( 'NONE',  ( 0.000000000000000000, -0.01356324068817992175, 0.9999080150203990547 ) ) ;
#22283 = ORIENTED_EDGE ( 'NONE', *, *, #58315, .F. ) ;
#22284 = VERTEX_POINT ( 'NONE', #21494 ) ;
#22285 = ORIENTED_EDGE ( 'NONE', *, *, #42860, .F. ) ;
#22286 = CARTESIAN_POINT ( 'NONE',  ( 2.931247277082683844, 7.855653518374123401, 0.3703309885897093090 ) ) ;
#22287 = B_SPLINE_CURVE_WITH_KNOTS ( 'NONE', 3,
 ( #1209, #52414, #12151, #17146, #33084, #37755, #28114, #21488, #37418, #32424, #42721, #63020, #57730, #41757, #47735, #2182, #22461, #17481, #12463 ),
 .UNSPECIFIED., .F., .F.,
 ( 4, 3, 3, 3, 3, 3, 4 ),
 ( 1.038473834433558171E-17, 4.457896483015033660E-05, 6.639290541542310726E-05, 8.820687556479056698E-05, 0.0001100173248778915164, 0.0001545671401658174149, 0.0001830328308068568150 ),
 .UNSPECIFIED. ) ;
#22288 = CIRCLE ( 'NONE', #52033, 20.19615242270663558 ) ;
#22289 = VECTOR ( 'NONE', #61748, 1000.000000000000000 ) ;
#22290 = ORIENTED_EDGE ( 'NONE', *, *, #15569, .F. ) ;
#22291 = CARTESIAN_POINT ( 'NONE',  ( -27.27855387000350262, -12.26939275170277632, 5.631341004100471892 ) ) ;
#22292 = CARTESIAN_POINT ( 'NONE',  ( 2.665405856346785729, -8.559192023451554832, 4.274976649834437481 ) ) ;
#22293 = EDGE_LOOP ( 'NONE', ( #26456, #25156, #39888, #60091 ) ) ;
#22294 = CARTESIAN_POINT ( 'NONE',  ( 35.00000000000000000, 11.81949347079746637, -2.968224442958448783 ) ) ;
#22295 = CARTESIAN_POINT ( 'NONE',  ( 2.242418902651938772, -2.704708480794760117, -7.139616612143416141 ) ) ;
#22296 = CARTESIAN_POINT ( 'NONE',  ( 24.67819621425959298, 0.8561783389638295549, 11.97593107962119419 ) ) ;
#22297 = ORIENTED_EDGE ( 'NONE', *, *, #38518, .F. ) ;
#22298 = ORIENTED_EDGE ( 'NONE', *, *, #5249, .F. ) ;
#22299 = LINE ( 'NONE', #7334, #64980 ) ;
#22300 = ORIENTED_EDGE ( 'NONE', *, *, #37222, .F. ) ;
#22301 = CARTESIAN_POINT ( 'NONE',  ( 11.39183535642925804, 0.2409185311480156466, -13.49808056869716033 ) ) ;
#22302 = CARTESIAN_POINT ( 'NONE',  ( -17.66721521611205503, -6.974610761929137759, 11.56240511626955758 ) ) ;
#22303 = CARTESIAN_POINT ( 'NONE',  ( 3.152665057734079568, -2.258875078502220024, -7.609997527621126245 ) ) ;
#22304 = ADVANCED_FACE ( 'NONE', ( #55426 ), #60403, .T. ) ;
#22305 = DIRECTION ( 'NONE',  ( 0.000000000000000000, -0.6745969609292555846, -0.7381862504172049810 ) ) ;
#22306 = DIRECTION ( 'NONE',  ( -1.000000000000000000, 0.000000000000000000, 0.000000000000000000 ) ) ;
#22307 = CARTESIAN_POINT ( 'NONE',  ( 2.990245332647881948, -7.779904630197274074, -3.377079998295690277 ) ) ;
#22308 = CARTESIAN_POINT ( 'NONE',  ( 0.5572780756290600657, 6.434474476008377408, -10.53376864352708431 ) ) ;
#22309 = CARTESIAN_POINT ( 'NONE',  ( 5.587718367926578722, -9.343663864590265433, -7.538223026388563675 ) ) ;
#22310 = ORIENTED_EDGE ( 'NONE', *, *, #17491, .T. ) ;
#22311 = AXIS2_PLACEMENT_3D ( 'NONE', #42814, #12884, #62431 ) ;
#22312 = DIRECTION ( 'NONE',  ( 0.000000000000000000, 0.8696919319575167062, 0.4935949184179292404 ) ) ;
#22313 =( BOUNDED_SURFACE ( )  B_SPLINE_SURFACE ( 3, 1, ( 
 ( #42000, #15735 ),
 ( #37342, #26076 ),
 ( #57652, #794 ),
 ( #61623, #36365 ) ),
 .UNSPECIFIED., .F., .F., .F. ) 
 B_SPLINE_SURFACE_WITH_KNOTS ( ( 4, 4 ),
 ( 2, 2 ),
 ( 0.000000000000000000, 1.000000000000000000 ),
 ( 0.000000000000000000, 1.000000000000000000 ),
 .UNSPECIFIED. ) 
 GEOMETRIC_REPRESENTATION_ITEM ( )  RATIONAL_B_SPLINE_SURFACE ( (
 ( 1.000000000000000000, 1.000000000000000000),
 ( 0.9942764183789327692, 0.8450855930916585379),
 ( 0.9942764183789327692, 0.8450855930916585379),
 ( 1.000000000000000000, 1.000000000000000000) ) ) 
 REPRESENTATION_ITEM ( '' )  SURFACE ( )  );
#22314 = ORIENTED_EDGE ( 'NONE', *, *, #17354, .T. ) ;
#22315 = DIRECTION ( 'NONE',  ( 0.000000000000000000, 0.000000000000000000, 1.000000000000000000 ) ) ;
#22316 = CARTESIAN_POINT ( 'NONE',  ( 2.260457164925429918, 6.685239696061921144, 3.699855525214781338 ) ) ;
#22317 = ORIENTED_EDGE ( 'NONE', *, *, #54999, .T. ) ;
#22318 = CYLINDRICAL_SURFACE ( 'NONE', #21163, 2.899999999999994582 ) ;
#22319 = CARTESIAN_POINT ( 'NONE',  ( 0.2958664285830439056, 12.02992237133200071, -2.345117904768493577 ) ) ;
#22320 = LINE ( 'NONE', #46313, #52494 ) ;
#22322 = ADVANCED_FACE ( 'NONE', ( #30154 ), #16167, .T. ) ;
#22321 = EDGE_LOOP ( 'NONE', ( #15698, #52921, #41806, #55269 ) ) ;
#22323 = ORIENTED_EDGE ( 'NONE', *, *, #8149, .F. ) ;
#22324 = CARTESIAN_POINT ( 'NONE',  ( 2.844750968616333697, -6.946006365804024973, -3.626176236708053224 ) ) ;
#22325 = AXIS2_PLACEMENT_3D ( 'NONE', #38009, #43325, #18075 ) ;
#22326 = ORIENTED_EDGE ( 'NONE', *, *, #8923, .F. ) ;
#22327 = DIRECTION ( 'NONE',  ( 0.000000000000000000, -0.9847383929261634972, 0.1740410799127515284 ) ) ;
#22328 = CARTESIAN_POINT ( 'NONE',  ( -27.08421860617808008, 2.116856729767824685, 0.8768262158915500759 ) ) ;
#22330 = CIRCLE ( 'NONE', #40408, 2.899999999999996358 ) ;
#22329 = DIRECTION ( 'NONE',  ( 0.000000000000000000, -0.01356324068817991828, 0.9999080150203990547 ) ) ;
#22331 = CARTESIAN_POINT ( 'NONE',  ( -19.69476066079020171, -4.201994156881551312, 11.24025111398909615 ) ) ;
#22332 = ORIENTED_EDGE ( 'NONE', *, *, #25201, .F. ) ;
#22333 = DIRECTION ( 'NONE',  ( 1.000000000000000000, 0.000000000000000000, -0.000000000000000000 ) ) ;
#22334 = B_SPLINE_CURVE_WITH_KNOTS ( 'NONE', 3,
 ( #45418, #54446, #19522, #44123, #34769, #50105, #40426, #10176 ),
 .UNSPECIFIED., .F., .F.,
 ( 4, 2, 2, 4 ),
 ( 0.000000000000000000, 0.0003639104015149874404, 0.0007278208030299748808, 0.001455641606059947593 ),
 .UNSPECIFIED. ) ;
#22335 = VECTOR ( 'NONE', #50183, 1000.000000000000000 ) ;
#22336 = EDGE_CURVE ( 'NONE', #24509, #55514, #27022, .T. ) ;
#22337 = STYLED_ITEM ( 'NONE', ( #43769 ), #6945 ) ;
#22338 = AXIS2_PLACEMENT_3D ( 'NONE', #30276, #38946, #13656 ) ;
#22339 = AXIS2_PLACEMENT_3D ( 'NONE', #45506, #50844, #9947 ) ;
#22340 = EDGE_CURVE ( 'NONE', #17445, #38122, #49774, .T. ) ;
#22341 = CARTESIAN_POINT ( 'NONE',  ( 18.04777717444645191, -29.74456712077427056, -8.215504029118783080 ) ) ;
#22342 = CARTESIAN_POINT ( 'NONE',  ( 35.00000000000000000, -4.339012074899872395, 10.91536515067652324 ) ) ;
#22343 = DIRECTION ( 'NONE',  ( 0.000000000000000000, -0.01356324068817991828, 0.9999080150203990547 ) ) ;
#22344 = CARTESIAN_POINT ( 'NONE',  ( 2.000000000000001776, 1.754183803416655474, -6.711026108862266248 ) ) ;
#22345 = EDGE_CURVE ( 'NONE', #45562, #63445, #14081, .T. ) ;
#22346 = CARTESIAN_POINT ( 'NONE',  ( -8.891032880924177206, -11.36194426013948444, -3.860857758255646921 ) ) ;
#22347 = CARTESIAN_POINT ( 'NONE',  ( -35.00000000000000000, -10.07641281632181673, 6.036400161834530209 ) ) ;
#22348 = CARTESIAN_POINT ( 'NONE',  ( 2.507146904658102304, 5.128007631637142794, -5.774795220010139118 ) ) ;
#22349 = AXIS2_PLACEMENT_3D ( 'NONE', #40040, #50037, #19456 ) ;
#22350 = EDGE_CURVE ( 'NONE', #59860, #39182, #64182, .T. ) ;
#22351 = VERTEX_POINT ( 'NONE', #6204 ) ;
#22352 = DIRECTION ( 'NONE',  ( -1.000000000000000000, -0.000000000000000000, 0.000000000000000000 ) ) ;
#22353 = DIRECTION ( 'NONE',  ( -1.000000000000000000, 0.000000000000000000, 0.000000000000000000 ) ) ;
#22354 = VECTOR ( 'NONE', #2583, 1000.000000000000000 ) ;
#22355 = CONICAL_SURFACE ( 'NONE', #42519, 7.938172270156617749, 1.280189991382167047 ) ;
#22356 = EDGE_LOOP ( 'NONE', ( #33151, #45127, #46021, #19688 ) ) ;
#22357 = CARTESIAN_POINT ( 'NONE',  ( -22.28350523959500862, 3.687952016964566759, -0.3047406164877188850 ) ) ;
#22358 = EDGE_CURVE ( 'NONE', #36702, #57461, #33422, .T. ) ;
#22359 = CARTESIAN_POINT ( 'NONE',  ( 2.177405672430581252, -6.173731551725364142, -9.343720763427118214 ) ) ;
#22360 = EDGE_LOOP ( 'NONE', ( #29297, #40058, #45678, #17475 ) ) ;
#22361 = AXIS2_PLACEMENT_3D ( 'NONE', #60441, #64760, #8934 ) ;
#22362 = CARTESIAN_POINT ( 'NONE',  ( 2.241509619876138615, 4.936617871859581008, -5.823675573301023256 ) ) ;
#22363 = VERTEX_POINT ( 'NONE', #25828 ) ;
#22364 = DIRECTION ( 'NONE',  ( 0.9759340573753173542, 0.2180658516479614117, 0.000000000000000000 ) ) ;
#22365 = VERTEX_POINT ( 'NONE', #31462 ) ;
#22366 = VERTEX_POINT ( 'NONE', #5217 ) ;
#22367 = B_SPLINE_CURVE_WITH_KNOTS ( 'NONE', 3,
 ( #45734, #10813, #30438, #5526, #31101, #46395, #15141, #20138, #844, #61673, #35424, #36416, #6172, #26434, #1177, #55729, #10159, #22100, #21799, #62644 ),
 .UNSPECIFIED., .F., .F.,
 ( 4, 2, 2, 2, 2, 2, 2, 2, 2, 4 ),
 ( 0.000000000000000000, 0.001078581342907173040, 0.002157162685814346080, 0.003235744028721518686, 0.004314325371628692160, 0.005392906714535864766, 0.005932197385989450636, 0.006471488057443037373, 0.007550069400350215183, 0.008628650743257391259 ),
 .UNSPECIFIED. ) ;
#22368 = CARTESIAN_POINT ( 'NONE',  ( -27.08416813689867908, -1.759517419957075113, 1.467601568343269491 ) ) ;
#22369 = VERTEX_POINT ( 'NONE', #51762 ) ;
#22370 = ADVANCED_FACE ( 'NONE', ( #25484 ), #45773, .T. ) ;
#22371 = CARTESIAN_POINT ( 'NONE',  ( 35.00000000000000000, 7.146664589317909488, -9.321877890560465119 ) ) ;
#22372 = CARTESIAN_POINT ( 'NONE',  ( 2.835339799623984192, -2.985412098050548746, 7.241165502254432340 ) ) ;
#22373 = FACE_OUTER_BOUND ( 'NONE', #776, .T. ) ;
#22374 = CIRCLE ( 'NONE', #40404, 12.73084802173761787 ) ;
#22375 = CARTESIAN_POINT ( 'NONE',  ( 20.00005080000000035, 0.000000000000000000, 0.000000000000000000 ) ) ;
#22376 = ORIENTED_EDGE ( 'NONE', *, *, #46484, .T. ) ;
#22377 = CARTESIAN_POINT ( 'NONE',  ( 37.00000000000000711, 9.677500615117898164, -6.657191900728355094 ) ) ;
#22378 = CARTESIAN_POINT ( 'NONE',  ( -0.8584944786142326700, -27.82166925786467004, 12.56635396443958719 ) ) ;
#22379 = CARTESIAN_POINT ( 'NONE',  ( -27.05874794189610455, 1.734723475976807094E-15, -8.673617379884035472E-15 ) ) ;
#22381 = ORIENTED_EDGE ( 'NONE', *, *, #60536, .T. ) ;
#22380 = DIRECTION ( 'NONE',  ( 0.000000000000000000, 0.01356324068817998940, -0.9999080150203990547 ) ) ;
#22383 = AXIS2_PLACEMENT_3D ( 'NONE', #39799, #55086, #9515 ) ;
#22382 = CARTESIAN_POINT ( 'NONE',  ( 5.530133899448235191, -0.006510401266731714702, -0.01459891979722877098 ) ) ;
#22384 = ORIENTED_EDGE ( 'NONE', *, *, #55425, .T. ) ;
#22385 = DIRECTION ( 'NONE',  ( 0.000000000000000000, -0.9970832820307047317, -0.07632122047555413291 ) ) ;
#22386 = EDGE_LOOP ( 'NONE', ( #60483, #7037, #30620, #28796 ) ) ;
#22387 = CARTESIAN_POINT ( 'NONE',  ( -35.00000000000000000, 0.000000000000000000, 0.000000000000000000 ) ) ;
#22388 = CARTESIAN_POINT ( 'NONE',  ( 35.00000000000000000, 9.512294188640899151, -6.891188680298859559 ) ) ;
#22389 = CARTESIAN_POINT ( 'NONE',  ( 1.375507693217711713, -4.865932489130966765, 11.64019206974660214 ) ) ;
#22390 = AXIS2_PLACEMENT_3D ( 'NONE', #33722, #8458, #43363 ) ;
#22391 = VERTEX_POINT ( 'NONE', #52739 ) ;
#22392 = AXIS2_PLACEMENT_3D ( 'NONE', #14553, #23925, #39186 ) ;
#22394 = AXIS2_PLACEMENT_3D ( 'NONE', #27437, #15815, #46748 ) ;
#22393 = CARTESIAN_POINT ( 'NONE',  ( 1.000000000000000888, 3.073484823194335025, 6.841322316745041654 ) ) ;
#22395 = DIRECTION ( 'NONE',  ( -0.3865475372811021937, 0.9220659470476461061, -0.01937500237528741107 ) ) ;
#22396 = CARTESIAN_POINT ( 'NONE',  ( 12.10998784662220551, 10.46621227226785322, -8.526922110106907482 ) ) ;
#22397 = ORIENTED_EDGE ( 'NONE', *, *, #61209, .T. ) ;
#22398 = ORIENTED_EDGE ( 'NONE', *, *, #46405, .F. ) ;
#22399 = AXIS2_PLACEMENT_3D ( 'NONE', #55368, #35403, #9806 ) ;
#22400 = DIRECTION ( 'NONE',  ( 0.000000000000000000, 0.9999080150203990547, 0.01356324068817645230 ) ) ;
#22401 = ORIENTED_EDGE ( 'NONE', *, *, #13158, .T. ) ;
#22402 = VERTEX_POINT ( 'NONE', #62684 ) ;
#22403 = CARTESIAN_POINT ( 'NONE',  ( 0.3675815128205894289, 1.872154644482245889, -12.13672785388548547 ) ) ;
#22404 = CYLINDRICAL_SURFACE ( 'NONE', #60206, 12.18649999999999878 ) ;
#22405 = LINE ( 'NONE', #57025, #27714 ) ;
#22406 = CARTESIAN_POINT ( 'NONE',  ( -22.29770266787582500, 1.047554374660461418, 3.593535545924332109 ) ) ;
#22408 = AXIS2_PLACEMENT_3D ( 'NONE', #55612, #21238, #6948 ) ;
#22407 = DIRECTION ( 'NONE',  ( -1.000000000000000000, 0.000000000000000000, 0.000000000000000000 ) ) ;
#22409 = EDGE_CURVE ( 'NONE', #52056, #42316, #62058, .T. ) ;
#22410 = AXIS2_PLACEMENT_3D ( 'NONE', #54242, #49903, #3389 ) ;
#22411 = CARTESIAN_POINT ( 'NONE',  ( 35.00000000000000000, -11.37311665002365579, -2.936739658819832677 ) ) ;
#22412 = DIRECTION ( 'NONE',  ( -1.000000000000000000, 0.000000000000000000, 0.000000000000000000 ) ) ;
#22413 = VECTOR ( 'NONE', #40245, 1000.000000000000000 ) ;
#22414 = ORIENTED_EDGE ( 'NONE', *, *, #16980, .T. ) ;
#22415 = VECTOR ( 'NONE', #24934, 1000.000000000000000 ) ;
#22416 = DIRECTION ( 'NONE',  ( -1.000000000000000000, 0.000000000000000000, 0.000000000000000000 ) ) ;
#22417 = CARTESIAN_POINT ( 'NONE',  ( -37.00000000000000711, -12.38385022362079724, -3.033604067594711129 ) ) ;
#22418 = CIRCLE ( 'NONE', #13913, 4.999999999999999112 ) ;
#22419 = B_SPLINE_CURVE_WITH_KNOTS ( 'NONE', 3,
 ( #64243, #18718, #8389, #38973, #32336, #52649, #7074, #27347, #29008, #40, #64551, #49315, #30311, #59268, #8724, #39952, #13690, #54285, #9043, #65531, #44944, #59926 ),
 .UNSPECIFIED., .F., .F.,
 ( 4, 3, 3, 3, 3, 3, 3, 4 ),
 ( 6.732537572691704696E-18, 6.990956068646403821E-05, 0.0001398191187764042775, 0.0002097286751720212191, 0.0002796382307041356675, 0.0003495477861619808576, 0.0004194573423310286289, 0.0005586102576333144961 ),
 .UNSPECIFIED. ) ;
#22420 = CARTESIAN_POINT ( 'NONE',  ( -35.04643116707788408, 0.003844232202716499347, -0.01156612771644957571 ) ) ;
#22421 = CARTESIAN_POINT ( 'NONE',  ( -37.00000000000000711, -12.08216339958899788, -1.591260454995368390 ) ) ;
#22422 = EDGE_CURVE ( 'NONE', #4031, #42345, #62912, .T. ) ;
#22423 = CARTESIAN_POINT ( 'NONE',  ( 0.000000000000000000, 0.000000000000000000, 0.000000000000000000 ) ) ;
#22424 = CIRCLE ( 'NONE', #57475, 7.499999999999988454 ) ;
#22425 = DIRECTION ( 'NONE',  ( 1.000000000000000000, 0.000000000000000000, -0.000000000000000000 ) ) ;
#22426 = EDGE_CURVE ( 'NONE', #38782, #49313, #58946, .T. ) ;
#22427 = DIRECTION ( 'NONE',  ( 1.000000000000000000, 0.000000000000000000, 0.000000000000000000 ) ) ;
#22428 = AXIS2_PLACEMENT_3D ( 'NONE', #15419, #24407, #60003 ) ;
#22429 = EDGE_CURVE ( 'NONE', #54444, #13128, #4787, .T. ) ;
#22430 = VERTEX_POINT ( 'NONE', #7844 ) ;
#22431 = CARTESIAN_POINT ( 'NONE',  ( 2.000000000000001776, 2.469490258309515518, -6.482025155313297482 ) ) ;
#22432 = DIRECTION ( 'NONE',  ( -1.000000000000000000, 0.000000000000000000, 0.000000000000000000 ) ) ;
#22433 = CARTESIAN_POINT ( 'NONE',  ( 1.937114397841935398, -8.920887662793408168, -9.228205347192542263 ) ) ;
#22434 = CARTESIAN_POINT ( 'NONE',  ( 2.430348790457659724, -1.528169972228470508, -7.544199152379142070 ) ) ;
#22435 = AXIS2_PLACEMENT_3D ( 'NONE', #16716, #27035, #51983 ) ;
#22436 = CIRCLE ( 'NONE', #53264, 5.000000000000000888 ) ;
#22437 = VECTOR ( 'NONE', #37655, 1000.000000000000000 ) ;
#22438 = EDGE_CURVE ( 'NONE', #46997, #15192, #41910, .T. ) ;
#22439 = DIRECTION ( 'NONE',  ( 0.000000000000000000, 0.9868265225415265851, -0.1617819965527618475 ) ) ;
#22440 = CARTESIAN_POINT ( 'NONE',  ( 0.3665391374699465965, -6.368473106897055480, -10.50279796150443268 ) ) ;
#22441 = ORIENTED_EDGE ( 'NONE', *, *, #40336, .F. ) ;
#22442 = CARTESIAN_POINT ( 'NONE',  ( 19.28625800530496903, -1.699513388191772778, 11.87904264843580471 ) ) ;
#22443 = CARTESIAN_POINT ( 'NONE',  ( -17.97167269346459051, 4.327294505063981944, 12.78955090225081648 ) ) ;
#22444 = EDGE_CURVE ( 'NONE', #22231, #53630, #8544, .T. ) ;
#22445 = CARTESIAN_POINT ( 'NONE',  ( 2.247206125382657405, -4.819320926502908442, -5.923516414428318555 ) ) ;
#22446 = CARTESIAN_POINT ( 'NONE',  ( -35.04834644901396956, 0.01383120537647295270, -0.0002835132723611888264 ) ) ;
#22447 = ORIENTED_EDGE ( 'NONE', *, *, #49457, .F. ) ;
#22448 = CARTESIAN_POINT ( 'NONE',  ( 1.000000000000000888, 5.097042323172538580, -5.501832381651401427 ) ) ;
#22449 = DIRECTION ( 'NONE',  ( 0.000000000000000000, -0.01356324068817998940, 0.9999080150203990547 ) ) ;
#22450 = ORIENTED_EDGE ( 'NONE', *, *, #10956, .T. ) ;
#22451 = VERTEX_POINT ( 'NONE', #12468 ) ;
#22452 = CARTESIAN_POINT ( 'NONE',  ( -37.00000000000000711, -8.699265615722922007, -8.534258022646191932 ) ) ;
#22453 = EDGE_CURVE ( 'NONE', #64447, #44513, #42959, .T. ) ;
#22454 = VECTOR ( 'NONE', #33446, 1000.000000000000000 ) ;
#22455 = VECTOR ( 'NONE', #55970, 1000.000000000000000 ) ;
#22456 = B_SPLINE_CURVE_WITH_KNOTS ( 'NONE', 3,
 ( #31135, #61070, #565, #55757, #10189, #61373, #5215, #50451, #50116, #25160, #20828, #29806 ),
 .UNSPECIFIED., .F., .F.,
 ( 4, 2, 2, 2, 2, 4 ),
 ( 0.006656218235223304580, 0.007268574118352267091, 0.007880930001481229602, 0.009105641767739156359, 0.01033035353399708312, 0.01155506530025500814 ),
 .UNSPECIFIED. ) ;
#22457 = LINE ( 'NONE', #7156, #63696 ) ;
#22458 = EDGE_LOOP ( 'NONE', ( #51553, #24774, #64388, #25873 ) ) ;
#22460 = ADVANCED_FACE ( 'NONE', ( #32741 ), #57392, .T. ) ;
#22459 = AXIS2_PLACEMENT_3D ( 'NONE', #45827, #45169, #14555 ) ;
#22461 = CARTESIAN_POINT ( 'NONE',  ( 0.2657645697724674849, -9.477802844074094679, 7.755260067564130111 ) ) ;
#22462 = CARTESIAN_POINT ( 'NONE',  ( 5.515539859299206427, 0.005991790098943838676, -0.0008592514567755067450 ) ) ;
#22463 = CARTESIAN_POINT ( 'NONE',  ( 0.000000000000000000, 3.152010634611773110, -6.039758645301250617 ) ) ;
#22464 = DIRECTION ( 'NONE',  ( -1.000000000000000000, 0.000000000000000000, 0.000000000000000000 ) ) ;
#22465 = CARTESIAN_POINT ( 'NONE',  ( -8.813892140501407013, 7.428019780266606809, -9.432948737998053446 ) ) ;
#22466 = AXIS2_PLACEMENT_3D ( 'NONE', #58729, #3528, #14438 ) ;
#22467 = EDGE_CURVE ( 'NONE', #53449, #41765, #14284, .T. ) ;
#22468 = CARTESIAN_POINT ( 'NONE',  ( -10.64311535907469874, -9.781890035361623603, 9.304428041637393676 ) ) ;
#22470 = VERTEX_POINT ( 'NONE', #32102 ) ;
#22469 = DIRECTION ( 'NONE',  ( -1.000000000000000000, 0.000000000000000000, 0.000000000000000000 ) ) ;
#22471 = CARTESIAN_POINT ( 'NONE',  ( 0.9296196016850740707, 4.652334946095896484, -11.56707937094533634 ) ) ;
#22472 = ORIENTED_EDGE ( 'NONE', *, *, #97, .F. ) ;
#22473 = DIRECTION ( 'NONE',  ( 0.000000000000000000, -0.9467777615094604693, -0.3218879778915876844 ) ) ;
#22474 = AXIS2_PLACEMENT_3D ( 'NONE', #40065, #19141, #34091 ) ;
#22475 = ORIENTED_EDGE ( 'NONE', *, *, #24038, .T. ) ;
#22476 = VERTEX_POINT ( 'NONE', #43064 ) ;
#22477 = APPLICATION_PROTOCOL_DEFINITION ( 'draft international standard', 'automotive_design', 1998, #27271 ) ;
#22478 = DIRECTION ( 'NONE',  ( 0.000000000000000000, 0.000000000000000000, 1.000000000000000000 ) ) ;
#22479 = CARTESIAN_POINT ( 'NONE',  ( 2.827825597296809157, -5.372687261161216199, -7.250702617666037852 ) ) ;
#22480 = CARTESIAN_POINT ( 'NONE',  ( 35.00000000000000000, -8.839356091080105671, -8.389074212634254124 ) ) ;
#22481 = CARTESIAN_POINT ( 'NONE',  ( -25.79281180259794226, -3.718204414137740610, -24.00000000000000355 ) ) ;
#22482 = CARTESIAN_POINT ( 'NONE',  ( -27.08419797710328680, 0.8552720754637080924, -2.125717714519615331 ) ) ;
#22483 = ORIENTED_EDGE ( 'NONE', *, *, #8736, .T. ) ;
#22484 = AXIS2_PLACEMENT_3D ( 'NONE', #21852, #36800, #22156 ) ;
#22485 = CARTESIAN_POINT ( 'NONE',  ( 0.3040950598368152291, 1.881452845810536623, -12.11647736519418928 ) ) ;
#22486 = CARTESIAN_POINT ( 'NONE',  ( 0.5547464869798236498, -3.933612953276315771, 11.69908463509555396 ) ) ;
#22487 = EDGE_LOOP ( 'NONE', ( #1296, #60331, #30732, #21849 ) ) ;
#22488 = ORIENTED_EDGE ( 'NONE', *, *, #13841, .T. ) ;
#22489 = CYLINDRICAL_SURFACE ( 'NONE', #15197, 7.499999999999988454 ) ;
#22490 = VECTOR ( 'NONE', #7391, 1000.000000000000000 ) ;
#22491 = ORIENTED_EDGE ( 'NONE', *, *, #33036, .F. ) ;
#22492 = CYLINDRICAL_SURFACE ( 'NONE', #43365, 6.936499999999988120 ) ;
#22493 = CARTESIAN_POINT ( 'NONE',  ( 2.000000000000001776, -6.777474576704058506, 0.6925993764990423518 ) ) ;
#22494 = DIRECTION ( 'NONE',  ( -1.000000000000000000, 0.000000000000000000, 0.000000000000000000 ) ) ;
#22495 = CYLINDRICAL_SURFACE ( 'NONE', #50731, 12.75000000000000178 ) ;
#22496 = CIRCLE ( 'NONE', #2343, 12.75000000000000178 ) ;
#22497 = EDGE_CURVE ( 'NONE', #19326, #46419, #25993, .T. ) ;
#22498 = CIRCLE ( 'NONE', #32061, 5.000000000000000888 ) ;
#22499 = EDGE_CURVE ( 'NONE', #2584, #44869, #34711, .T. ) ;
#22500 = DIRECTION ( 'NONE',  ( -1.000000000000000000, 0.000000000000000000, -0.000000000000000000 ) ) ;
#22501 = FACE_BOUND ( 'NONE', #46772, .T. ) ;
#22502 = AXIS2_PLACEMENT_3D ( 'NONE', #17044, #47975, #63565 ) ;
#22503 = B_SPLINE_CURVE_WITH_KNOTS ( 'NONE', 3,
 ( #39245, #17678, #64510, #38255, #13003, #27627, #43574, #47930, #18341, #37939, #13645, #58232, #3048, #33287, #48926, #28957, #3381, #12652, #32935, #59223, #18677, #58920 ),
 .UNSPECIFIED., .F., .F.,
 ( 4, 3, 3, 3, 3, 3, 3, 4 ),
 ( 0.000000000000000000, 4.455945684386718414E-05, 6.636307477203950002E-05, 8.816671873158800788E-05, 0.0001099660380492623735, 0.0001317545563165321062, 0.0001762613022895059660, 0.0001867992666138413812 ),
 .UNSPECIFIED. ) ;
#22504 = CARTESIAN_POINT ( 'NONE',  ( 2.262775599886257094, 3.942403752832098540, -6.546038779272000951 ) ) ;
#22505 = ORIENTED_EDGE ( 'NONE', *, *, #44469, .F. ) ;
#22506 = CARTESIAN_POINT ( 'NONE',  ( 0.2648978790185584908, -11.46165506714225479, -4.312320170909353045 ) ) ;
#22507 = ORIENTED_EDGE ( 'NONE', *, *, #52818, .F. ) ;
#22508 = B_SPLINE_CURVE_WITH_KNOTS ( 'NONE', 3,
 ( #4736, #54498, #12592, #29221, #38194, #63461, #33221 ),
 .UNSPECIFIED., .F., .F.,
 ( 4, 3, 4 ),
 ( 5.216753085810794840E-15, 0.002398160485434687548, 0.005002426799382050059 ),
 .UNSPECIFIED. ) ;
#22509 = CARTESIAN_POINT ( 'NONE',  ( 0.2653141617321017609, -6.161204121352767515, 10.58343467791294046 ) ) ;
#22510 = CARTESIAN_POINT ( 'NONE',  ( -35.04834644901396956, 0.006670072992069154237, -0.01211993185718438990 ) ) ;
#22511 = CARTESIAN_POINT ( 'NONE',  ( 2.717984159219351437, -2.930214355830539574, -7.221467817271510548 ) ) ;
#22512 = EDGE_CURVE ( 'NONE', #30999, #9450, #37651, .T. ) ;
#22513 = LINE ( 'NONE', #23491, #27668 ) ;
#22514 = ORIENTED_EDGE ( 'NONE', *, *, #17675, .F. ) ;
#22515 = VECTOR ( 'NONE', #26870, 1000.000000000000000 ) ;
#22516 = ORIENTED_EDGE ( 'NONE', *, *, #25679, .T. ) ;
#22517 = EDGE_CURVE ( 'NONE', #61175, #56695, #48314, .T. ) ;
#22518 = FACE_OUTER_BOUND ( 'NONE', #17089, .T. ) ;
#22519 =( BOUNDED_SURFACE ( )  B_SPLINE_SURFACE ( 3, 1, ( 
 ( #22873, #27847 ),
 ( #8873, #53462 ),
 ( #38474, #13832 ),
 ( #23184, #33153 ) ),
 .UNSPECIFIED., .F., .F., .F. ) 
 B_SPLINE_SURFACE_WITH_KNOTS ( ( 4, 4 ),
 ( 2, 2 ),
 ( 0.000000000000000000, 1.000000000000000000 ),
 ( 0.000000000000000000, 1.000000000000000000 ),
 .UNSPECIFIED. ) 
 GEOMETRIC_REPRESENTATION_ITEM ( )  RATIONAL_B_SPLINE_SURFACE ( (
 ( 1.000000000000000000, 1.000000000000000000),
 ( 0.9856612449720755231, 0.9999558406602322425),
 ( 0.9856612449720755231, 0.9999558406602322425),
 ( 1.000000000000000000, 1.000000000000000000) ) ) 
 REPRESENTATION_ITEM ( '' )  SURFACE ( )  );
#22520 = ORIENTED_EDGE ( 'NONE', *, *, #20965, .F. ) ;
#22521 = DIRECTION ( 'NONE',  ( 0.000000000000000000, 0.000000000000000000, -1.000000000000000000 ) ) ;
#22522 = CYLINDRICAL_SURFACE ( 'NONE', #45069, 2.899999999999994582 ) ;
#22523 = VECTOR ( 'NONE', #36942, 1000.000000000000000 ) ;
#22524 = CARTESIAN_POINT ( 'NONE',  ( -35.00000000000000000, 11.24036214326520522, 6.018036132182202458 ) ) ;
#22525 = LINE ( 'NONE', #32475, #28618 ) ;
#22526 = ADVANCED_FACE ( 'NONE', ( #44061 ), #63662, .T. ) ;
#22527 = VERTEX_POINT ( 'NONE', #60017 ) ;
#22528 = DIRECTION ( 'NONE',  ( -1.000000000000000000, 0.000000000000000000, -0.000000000000000000 ) ) ;
#22530 = AXIS2_PLACEMENT_3D ( 'NONE', #30190, #4932, #20205 ) ;
#22529 = CARTESIAN_POINT ( 'NONE',  ( -22.30398854582848145, -2.594196582746997493, 2.724439933030915473 ) ) ;
#22531 = CARTESIAN_POINT ( 'NONE',  ( 0.2653519789438754106, -10.61653328464223023, -6.104019611498684661 ) ) ;
#22532 = CARTESIAN_POINT ( 'NONE',  ( -37.49868115534710711, -2.226531222652248232, 21.71250474234130579 ) ) ;
#22533 = CARTESIAN_POINT ( 'NONE',  ( 0.2706063244538022272, 6.275112929891760061, -10.51833723927416031 ) ) ;
#22534 = AXIS2_PLACEMENT_3D ( 'NONE', #44086, #49100, #54410 ) ;
#22535 = LINE ( 'NONE', #18203, #55291 ) ;
#22536 =( BOUNDED_SURFACE ( )  B_SPLINE_SURFACE ( 3, 1, ( 
 ( #12494, #46777 ),
 ( #1578, #32767 ),
 ( #51782, #6226 ),
 ( #42097, #42757 ) ),
 .UNSPECIFIED., .F., .F., .F. ) 
 B_SPLINE_SURFACE_WITH_KNOTS ( ( 4, 4 ),
 ( 2, 2 ),
 ( 0.000000000000000000, 1.000000000000000000 ),
 ( 0.000000000000000000, 1.000000000000000000 ),
 .UNSPECIFIED. ) 
 GEOMETRIC_REPRESENTATION_ITEM ( )  RATIONAL_B_SPLINE_SURFACE ( (
 ( 1.000000000000000000, 1.000000000000000000),
 ( 0.9942764183789327692, 0.8450855930916580938),
 ( 0.9942764183789327692, 0.8450855930916580938),
 ( 1.000000000000000000, 1.000000000000000000) ) ) 
 REPRESENTATION_ITEM ( '' )  SURFACE ( )  );
#22537 = ORIENTED_EDGE ( 'NONE', *, *, #55975, .F. ) ;
#22538 = CARTESIAN_POINT ( 'NONE',  ( -11.38801898431830040, -29.26006678106167769, -7.242958320505154646 ) ) ;
#22539 = ORIENTED_EDGE ( 'NONE', *, *, #63879, .F. ) ;
#22540 = LINE ( 'NONE', #63094, #28098 ) ;
#22541 = CARTESIAN_POINT ( 'NONE',  ( 1.375507693218733563, -8.553661013312394701, 9.273955665125873438 ) ) ;
#22542 = CYLINDRICAL_SURFACE ( 'NONE', #11773, 5.000000000000000888 ) ;
#22543 = DIRECTION ( 'NONE',  ( -1.000000000000000000, -0.000000000000000000, 0.000000000000000000 ) ) ;
#22544 = CARTESIAN_POINT ( 'NONE',  ( 0.2767916011545381583, -11.44495079483527711, 4.367596755337407544 ) ) ;
#22545 = EDGE_CURVE ( 'NONE', #17578, #9098, #16443, .T. ) ;
#22546 = CIRCLE ( 'NONE', #13002, 12.18650000000000055 ) ;
#22547 = VECTOR ( 'NONE', #19575, 1000.000000000000000 ) ;
#22548 = ORIENTED_EDGE ( 'NONE', *, *, #29771, .T. ) ;
#22549 = ORIENTED_EDGE ( 'NONE', *, *, #43628, .T. ) ;
#22550 = B_SPLINE_CURVE_WITH_KNOTS ( 'NONE', 3,
 ( #58190, #7644, #57211, #27264, #27929, #17949, #7990, #2688, #21640, #47556, #33237, #57542, #1691 ),
 .UNSPECIFIED., .F., .F.,
 ( 4, 3, 3, 3, 4 ),
 ( 2.168404344971008868E-18, 6.607593386745501222E-05, 0.0001321518677373524609, 0.0001982171734706209411, 0.0002642860854759490423 ),
 .UNSPECIFIED. ) ;
#22551 = FACE_OUTER_BOUND ( 'NONE', #27652, .T. ) ;
#22552 = EDGE_CURVE ( 'NONE', #16346, #2801, #53619, .T. ) ;
#22553 = ORIENTED_EDGE ( 'NONE', *, *, #10424, .T. ) ;
#22554 = CARTESIAN_POINT ( 'NONE',  ( -27.08426571771018487, -2.277536580310468128, 0.2528330215897273692 ) ) ;
#22555 = CARTESIAN_POINT ( 'NONE',  ( 3.152665057734130638, 7.609997527621177760, -2.258875078502145861 ) ) ;
#22556 = CARTESIAN_POINT ( 'NONE',  ( 35.00000000000000000, -12.12087942037208776, 1.262958560998883595 ) ) ;
#22557 = CARTESIAN_POINT ( 'NONE',  ( 2.241528039335007438, 0.01573255094252495184, -7.634443721858079179 ) ) ;
#22558 = CARTESIAN_POINT ( 'NONE',  ( 3.092491956583705015, 7.905533744257984274, -0.4473002062000842605 ) ) ;
#22559 = ADVANCED_FACE ( 'NONE', ( #59048 ), #10279, .F. ) ;
#22560 = CARTESIAN_POINT ( 'NONE',  ( 2.276198483118649030, 5.756970692721976590, 5.031786924856548104 ) ) ;
#22561 = FACE_OUTER_BOUND ( 'NONE', #35634, .T. ) ;
#22562 = ORIENTED_EDGE ( 'NONE', *, *, #44875, .T. ) ;
#22563 = ORIENTED_EDGE ( 'NONE', *, *, #40007, .T. ) ;
#22564 = CARTESIAN_POINT ( 'NONE',  ( 0.000000000000000000, 0.4804830611970945520, -6.919838746524566986 ) ) ;
#22565 = ORIENTED_EDGE ( 'NONE', *, *, #58482, .F. ) ;
#22566 = VECTOR ( 'NONE', #19197, 1000.000000000000000 ) ;
#22567 = CARTESIAN_POINT ( 'NONE',  ( 21.48552864291340825, -12.93924674466299507, -3.871244808164612916 ) ) ;
#22568 = CARTESIAN_POINT ( 'NONE',  ( -37.00000000000000711, 6.102719229070827645, -10.54834585426213422 ) ) ;
#22569 = CARTESIAN_POINT ( 'NONE',  ( -22.28482751661422867, -1.587261331312489032, 3.347211412506312822 ) ) ;
#22570 = VERTEX_POINT ( 'NONE', #33739 ) ;
#22571 = CARTESIAN_POINT ( 'NONE',  ( 1.452237505248555660, -0.5922625322516135160, -12.64182585313126772 ) ) ;
#22572 = CARTESIAN_POINT ( 'NONE',  ( -13.03183108261446144, -30.03462372422786331, -7.545134388565382544 ) ) ;
#22573 = LINE ( 'NONE', #52521, #65781 ) ;
#22574 = VERTEX_POINT ( 'NONE', #59352 ) ;
#22575 = CIRCLE ( 'NONE', #59731, 5.000000000000000888 ) ;
#22576 = ORIENTED_EDGE ( 'NONE', *, *, #40490, .F. ) ;
#22577 = DIRECTION ( 'NONE',  ( 0.000000000000000000, 0.2006870767258819854, -0.9796553971857756560 ) ) ;
#22578 = ORIENTED_EDGE ( 'NONE', *, *, #54484, .F. ) ;
#22579 = ORIENTED_EDGE ( 'NONE', *, *, #51482, .F. ) ;
#22580 = CARTESIAN_POINT ( 'NONE',  ( -37.00000000000000711, 0.000000000000000000, 0.000000000000000000 ) ) ;
#22581 = ORIENTED_EDGE ( 'NONE', *, *, #14063, .F. ) ;
#22582 = VERTEX_POINT ( 'NONE', #54039 ) ;
#22583 = DIRECTION ( 'NONE',  ( -1.000000000000000000, -1.836970198721029688E-16, 0.000000000000000000 ) ) ;
#22584 = DIRECTION ( 'NONE',  ( 1.000000000000000000, -0.000000000000000000, 0.000000000000000000 ) ) ;
#22585 = EDGE_CURVE ( 'NONE', #34249, #60329, #50428, .T. ) ;
#22586 = CARTESIAN_POINT ( 'NONE',  ( -19.29830389789112033, -11.99999999999998757, -0.6550734076493088809 ) ) ;
#22587 = CYLINDRICAL_SURFACE ( 'NONE', #45777, 12.75000000000000178 ) ;
#22588 = CARTESIAN_POINT ( 'NONE',  ( 37.00000000000000711, 4.705694406421931860E-17, -3.469127814946512892E-15 ) ) ;
#22589 = DIRECTION ( 'NONE',  ( -1.000000000000000000, 0.000000000000000000, 0.000000000000000000 ) ) ;
#22590 = EDGE_CURVE ( 'NONE', #22391, #63878, #39058, .T. ) ;
#22591 = ORIENTED_EDGE ( 'NONE', *, *, #31777, .T. ) ;
#22592 = LINE ( 'NONE', #27562, #32642 ) ;
#22593 = CARTESIAN_POINT ( 'NONE',  ( -22.27720412283625961, 2.752887114864236207, -2.444672752438185270 ) ) ;
#22594 = CARTESIAN_POINT ( 'NONE',  ( 5.514970785353741078, -0.002619824551223729620, -0.003929719953530097683 ) ) ;
#22596 = CARTESIAN_POINT ( 'NONE',  ( -37.00000000000000711, 0.000000000000000000, 0.000000000000000000 ) ) ;
#22595 = AXIS2_PLACEMENT_3D ( 'NONE', #3165, #33069, #43046 ) ;
#22597 = FACE_OUTER_BOUND ( 'NONE', #15760, .T. ) ;
#22598 = CARTESIAN_POINT ( 'NONE',  ( 0.2647959493198551173, -11.55693259385003735, -4.049980114636486661 ) ) ;
#22599 = ADVANCED_FACE ( 'NONE', ( #54383 ), #16696, .F. ) ;
#22600 = AXIS2_PLACEMENT_3D ( 'NONE', #1386, #27957, #63504 ) ;
#22601 = DIRECTION ( 'NONE',  ( -1.000000000000000000, -0.000000000000000000, -0.000000000000000000 ) ) ;
#22602 = CIRCLE ( 'NONE', #9854, 4.999999999999999112 ) ;
#22603 = VECTOR ( 'NONE', #25728, 1000.000000000000000 ) ;
#22604 = ORIENTED_EDGE ( 'NONE', *, *, #38585, .F. ) ;
#22605 = CARTESIAN_POINT ( 'NONE',  ( 37.00000000000000711, 2.080187960898562061, -12.57916205664482412 ) ) ;
#22606 = ORIENTED_EDGE ( 'NONE', *, *, #11523, .F. ) ;
#22607 = DIRECTION ( 'NONE',  ( -1.000000000000000000, 0.000000000000000000, 0.000000000000000000 ) ) ;
#22608 = CARTESIAN_POINT ( 'NONE',  ( 2.251139882113957658, 5.929826121559351293, -4.813633939919377269 ) ) ;
#22609 = CARTESIAN_POINT ( 'NONE',  ( 35.00000000000000000, -2.544412758415763864, 11.91791701451268715 ) ) ;
#22610 = DIRECTION ( 'NONE',  ( -1.000000000000000000, 0.000000000000000000, 0.000000000000000000 ) ) ;
#22611 = CARTESIAN_POINT ( 'NONE',  ( 2.507146904658097419, -4.796593924427943634, -6.052884339496478638 ) ) ;
#22612 = EDGE_CURVE ( 'NONE', #52172, #7317, #45905, .T. ) ;
#22613 = ORIENTED_EDGE ( 'NONE', *, *, #56617, .T. ) ;
#22614 = AXIS2_PLACEMENT_3D ( 'NONE', #17453, #31731, #57699 ) ;
#22615 = CARTESIAN_POINT ( 'NONE',  ( 1.372161826076961022, 10.61825687422752473, -6.811451307636878560 ) ) ;
#22616 = CARTESIAN_POINT ( 'NONE',  ( -37.00000000000000711, 11.05394794832836958, -5.130401251914614491 ) ) ;
#22617 = DIRECTION ( 'NONE',  ( -0.000000000000000000, -0.000000000000000000, 1.000000000000000000 ) ) ;
#22618 = CARTESIAN_POINT ( 'NONE',  ( 26.25871678826176847, 11.49115831596999371, 3.460539353551113972 ) ) ;
#22619 = EDGE_CURVE ( 'NONE', #20683, #23800, #15717, .T. ) ;
#22620 = DIRECTION ( 'NONE',  ( 0.000000000000000000, -0.9246979985058680906, -0.3807014730195321661 ) ) ;
#22621 = ORIENTED_EDGE ( 'NONE', *, *, #5431, .F. ) ;
#22622 = AXIS2_PLACEMENT_3D ( 'NONE', #36305, #56610, #11682 ) ;
#22623 = PRODUCT_DEFINITION_CONTEXT ( 'detailed design', #6035, 'design' ) ;
#22624 = CARTESIAN_POINT ( 'NONE',  ( 2.844750968615479714, -0.3326424433130156788, -7.828506085988468755 ) ) ;
#22625 = CYLINDRICAL_SURFACE ( 'NONE', #36317, 12.74999999999999822 ) ;
#22626 = EDGE_CURVE ( 'NONE', #27004, #7169, #51536, .T. ) ;
#22627 = VERTEX_POINT ( 'NONE', #31388 ) ;
#22628 = CARTESIAN_POINT ( 'NONE',  ( -9.345615655111398468, 10.52963412100725016, -8.456574980679686604 ) ) ;
#22629 = EDGE_CURVE ( 'NONE', #55862, #13910, #10663, .T. ) ;
#22630 = VERTEX_POINT ( 'NONE', #45044 ) ;
#22631 = CARTESIAN_POINT ( 'NONE',  ( 2.297017764050092836, -6.543724852214706900, 3.968300849026735300 ) ) ;
#22632 = CARTESIAN_POINT ( 'NONE',  ( 2.241352910868909643, -5.794346703933810794, -4.970878533273820565 ) ) ;
#22633 = DIRECTION ( 'NONE',  ( 0.000000000000000000, 0.01356324068817998940, -0.9999080150203990547 ) ) ;
#22634 = CARTESIAN_POINT ( 'NONE',  ( 1.633930747251776783, -7.601388527387466176, 10.17701904908730270 ) ) ;
#22635 = EDGE_CURVE ( 'NONE', #23433, #16276, #61048, .T. ) ;
#22636 = CARTESIAN_POINT ( 'NONE',  ( -22.31328051695926007, -2.109671368890623455, -3.148362328073181615 ) ) ;
#22637 = ORIENTED_EDGE ( 'NONE', *, *, #29417, .F. ) ;
#22638 = B_SPLINE_CURVE_WITH_KNOTS ( 'NONE', 3,
 ( #64949, #43696, #38042, #63982, #51334, #40677, #56290, #20396, #45662, #5784, #46332, #26052, #35348 ),
 .UNSPECIFIED., .F., .F.,
 ( 4, 3, 3, 3, 4 ),
 ( 3.469446951953614189E-18, 6.607593386745428039E-05, 0.0001321518677373504551, 0.0001982171734706186642, 0.0002642860854759481750 ),
 .UNSPECIFIED. ) ;
#22639 = VECTOR ( 'NONE', #62512, 1000.000000000000000 ) ;
#22640 = AXIS2_PLACEMENT_3D ( 'NONE', #38423, #48424, #53733 ) ;
#22641 = ORIENTED_EDGE ( 'NONE', *, *, #10552, .T. ) ;
#22642 = ORIENTED_EDGE ( 'NONE', *, *, #34224, .F. ) ;
#22643 = CARTESIAN_POINT ( 'NONE',  ( 2.255723233588951437, 7.222632368701306760, -2.488140745365793105 ) ) ;
#22644 = CIRCLE ( 'NONE', #21606, 14.99999999999998757 ) ;
#22646 = CIRCLE ( 'NONE', #14127, 12.18650000000000055 ) ;
#22645 = CARTESIAN_POINT ( 'NONE',  ( 3.152665057734040488, 0.000000000000000000, 0.000000000000000000 ) ) ;
#22647 = VERTEX_POINT ( 'NONE', #10768 ) ;
#22648 = CYLINDRICAL_SURFACE ( 'NONE', #57013, 5.000000000000000888 ) ;
#22649 = LINE ( 'NONE', #37924, #17253 ) ;
#22650 = ORIENTED_EDGE ( 'NONE', *, *, #58258, .T. ) ;
#22651 = DIRECTION ( 'NONE',  ( 0.000000000000000000, 0.01356324068817998940, -0.9999080150203990547 ) ) ;
#22652 = CARTESIAN_POINT ( 'NONE',  ( 2.000000000000001776, 0.000000000000000000, 0.000000000000000000 ) ) ;
#22653 = CARTESIAN_POINT ( 'NONE',  ( 2.290907136834312130, 7.132394668149571793, 2.768669624189211032 ) ) ;
#22654 = ORIENTED_EDGE ( 'NONE', *, *, #63233, .T. ) ;
#22655 = AXIS2_PLACEMENT_3D ( 'NONE', #60282, #45643, #9735 ) ;
#22656 = ORIENTED_EDGE ( 'NONE', *, *, #9920, .T. ) ;
#22657 = CARTESIAN_POINT ( 'NONE',  ( 0.2833330754217440739, 12.09951353627562298, -1.928200609300346091 ) ) ;
#22658 = ORIENTED_EDGE ( 'NONE', *, *, #28831, .T. ) ;
#22659 =( LENGTH_UNIT ( ) NAMED_UNIT ( * ) SI_UNIT ( .MILLI., .METRE. ) );
#22660 = ORIENTED_EDGE ( 'NONE', *, *, #53545, .T. ) ;
#22661 = CIRCLE ( 'NONE', #31143, 12.75000000000000178 ) ;
#22662 = CARTESIAN_POINT ( 'NONE',  ( 2.268878695253356170, 3.692782103667282101, 6.692359410363615702 ) ) ;
#22663 = DIRECTION ( 'NONE',  ( 1.000000000000000000, 0.000000000000000000, 0.000000000000000000 ) ) ;
#22664 = CIRCLE ( 'NONE', #5688, 12.74999999999999822 ) ;
#22665 = FACE_OUTER_BOUND ( 'NONE', #34212, .T. ) ;
#22666 = FACE_OUTER_BOUND ( 'NONE', #50007, .T. ) ;
#22667 = DIRECTION ( 'NONE',  ( 0.000000000000000000, -0.6876994588534296460, 0.7259954919231248471 ) ) ;
#22668 = DIRECTION ( 'NONE',  ( 0.000000000000000000, -0.01356324068817998593, 0.9999080150203990547 ) ) ;
#22669 = CARTESIAN_POINT ( 'NONE',  ( 3.720874945556317925, -10.52563386907497645, -5.765812798277466733 ) ) ;
#22670 = ORIENTED_EDGE ( 'NONE', *, *, #1312, .F. ) ;
#22671 = CARTESIAN_POINT ( 'NONE',  ( -35.00000000000000000, 9.896810808925495806, -7.110831038798170134 ) ) ;
#22672 = EDGE_CURVE ( 'NONE', #64505, #45493, #60661, .T. ) ;
#22673 = CIRCLE ( 'NONE', #52436, 12.18650000000000055 ) ;
#22674 = ORIENTED_EDGE ( 'NONE', *, *, #32858, .F. ) ;
#22675 = DIRECTION ( 'NONE',  ( -1.000000000000000000, 0.000000000000000000, -0.000000000000000000 ) ) ;
#22676 = AXIS2_PLACEMENT_3D ( 'NONE', #40904, #44902, #65807 ) ;
#22677 = DIRECTION ( 'NONE',  ( -1.000000000000000000, 0.000000000000000000, 0.000000000000000000 ) ) ;
#22678 = EDGE_LOOP ( 'NONE', ( #19791, #10787, #31536, #5723 ) ) ;
#22679 = CARTESIAN_POINT ( 'NONE',  ( 2.430348790457469210, 7.297553103283551224, 2.448665558939112863 ) ) ;
#22680 = CARTESIAN_POINT ( 'NONE',  ( 0.3006302518451994255, 6.323626002161084614, 10.50091819089218603 ) ) ;
#22681 = CARTESIAN_POINT ( 'NONE',  ( 0.2648978790185610999, -2.256510822326061483, -12.03635331166814382 ) ) ;
#22682 = ORIENTED_EDGE ( 'NONE', *, *, #54796, .F. ) ;
#22683 = EDGE_CURVE ( 'NONE', #39152, #41139, #11161, .T. ) ;
#22684 = VECTOR ( 'NONE', #14691, 1000.000000000000000 ) ;
#22685 = VERTEX_POINT ( 'NONE', #5481 ) ;
#22686 = DIRECTION ( 'NONE',  ( 0.000000000000000000, 0.5767582926624911233, 0.8169148498130316405 ) ) ;
#22687 = ORIENTED_EDGE ( 'NONE', *, *, #29117, .T. ) ;
#22688 = DIRECTION ( 'NONE',  ( 0.000000000000000000, -0.01356324068817991828, 0.9999080150203990547 ) ) ;
#22689 = DIRECTION ( 'NONE',  ( 1.000000000000000000, 0.000000000000000000, -0.000000000000000000 ) ) ;
#22690 = CARTESIAN_POINT ( 'NONE',  ( -3.551075549032100653, -11.20694143114970309, 7.536131228641787416 ) ) ;
#22691 = CYLINDRICAL_SURFACE ( 'NONE', #63973, 12.18650000000000055 ) ;
#22692 = EDGE_CURVE ( 'NONE', #42026, #56480, #50611, .T. ) ;
#22693 = ORIENTED_EDGE ( 'NONE', *, *, #62730, .F. ) ;
#22694 = AXIS2_PLACEMENT_3D ( 'NONE', #23090, #2834, #18103 ) ;
#22695 = CIRCLE ( 'NONE', #29052, 5.000000000000000888 ) ;
#22696 = DIRECTION ( 'NONE',  ( 1.000000000000000000, 0.000000000000000000, -0.000000000000000000 ) ) ;
#22697 = EDGE_CURVE ( 'NONE', #22365, #28181, #20712, .T. ) ;
#22698 = CARTESIAN_POINT ( 'NONE',  ( 9.372867312212058266, -27.54793913079791068, -14.59713702163757176 ) ) ;
#22699 = AXIS2_PLACEMENT_3D ( 'NONE', #1989, #63465, #43190 ) ;
#22700 = CARTESIAN_POINT ( 'NONE',  ( 22.11485272451896122, 12.73694106385319635, -4.489087575610414937 ) ) ;
#22701 = DIRECTION ( 'NONE',  ( 1.000000000000000000, 0.000000000000000000, -0.000000000000000000 ) ) ;
#22702 = DIRECTION ( 'NONE',  ( 0.000000000000000000, 0.6876994588534245390, -0.7259954919231297321 ) ) ;
#22703 = CARTESIAN_POINT ( 'NONE',  ( 2.259025283528082184, -5.764013728792217073, 5.014999102875841608 ) ) ;
#22704 = CARTESIAN_POINT ( 'NONE',  ( -22.28856623400852044, -2.668530796663827420, -2.585606290939622021 ) ) ;
#22705 = AXIS2_PLACEMENT_3D ( 'NONE', #43039, #17783, #38045 ) ;
#22706 = EDGE_CURVE ( 'NONE', #57602, #18732, #55736, .T. ) ;
#22707 = AXIS2_PLACEMENT_3D ( 'NONE', #56992, #1125, #31687 ) ;
#22708 = VERTEX_POINT ( 'NONE', #61309 ) ;
#22709 = CARTESIAN_POINT ( 'NONE',  ( -24.42101984568203932, 1.824625598916893798, 3.884389025764499515 ) ) ;
#22710 = CARTESIAN_POINT ( 'NONE',  ( 6.191737802758098930, -8.543386553998011834, 10.45875730708377560 ) ) ;
#22711 = VERTEX_POINT ( 'NONE', #15743 ) ;
#22712 = CARTESIAN_POINT ( 'NONE',  ( -16.80711177628372610, 7.518039125045333115, -9.354561933223482839 ) ) ;
#22713 = LINE ( 'NONE', #13050, #37429 ) ;
#22714 = CARTESIAN_POINT ( 'NONE',  ( -22.39032720737627713, 2.936932155721193816, 2.746561316202127401 ) ) ;
#22715 = AXIS2_PLACEMENT_3D ( 'NONE', #42419, #26495, #46783 ) ;
#22716 = VERTEX_POINT ( 'NONE', #36022 ) ;
#22717 = CARTESIAN_POINT ( 'NONE',  ( 2.298277635560813437, 6.543949079924037626, 3.968740875991768835 ) ) ;
#22718 = VERTEX_POINT ( 'NONE', #56320 ) ;
#22719 = DIRECTION ( 'NONE',  ( 0.000000000000000000, 0.000000000000000000, 1.000000000000000000 ) ) ;
#22720 = ORIENTED_EDGE ( 'NONE', *, *, #18926, .T. ) ;
#22721 = ORIENTED_EDGE ( 'NONE', *, *, #37533, .T. ) ;
#22722 = EDGE_CURVE ( 'NONE', #57595, #59842, #36341, .T. ) ;
#22723 = CARTESIAN_POINT ( 'NONE',  ( 0.3537226245948383863, -12.04110684114371388, -2.388187631842642045 ) ) ;
#22724 = ORIENTED_EDGE ( 'NONE', *, *, #16739, .F. ) ;
#22725 = CARTESIAN_POINT ( 'NONE',  ( -10.00000000000000178, 0.000000000000000000, 0.000000000000000000 ) ) ;
#22726 = CARTESIAN_POINT ( 'NONE',  ( 2.305787727787083519, -2.774453000917197265, 7.135468203929974607 ) ) ;
#22727 = DIRECTION ( 'NONE',  ( 0.000000000000000000, -1.000000000000000000, 0.000000000000000000 ) ) ;
#22728 = CYLINDRICAL_SURFACE ( 'NONE', #25843, 2.899999999999994582 ) ;
#22729 = VERTEX_POINT ( 'NONE', #22733 ) ;
#22730 =( BOUNDED_SURFACE ( )  B_SPLINE_SURFACE ( 3, 1, ( 
 ( #15572, #45504 ),
 ( #35838, #56833 ),
 ( #951, #41492 ),
 ( #61788, #52802 ) ),
 .UNSPECIFIED., .F., .F., .F. ) 
 B_SPLINE_SURFACE_WITH_KNOTS ( ( 4, 4 ),
 ( 2, 2 ),
 ( 0.000000000000000000, 1.000000000000000000 ),
 ( 0.000000000000000000, 1.000000000000000000 ),
 .UNSPECIFIED. ) 
 GEOMETRIC_REPRESENTATION_ITEM ( )  RATIONAL_B_SPLINE_SURFACE ( (
 ( 1.000000000000000000, 1.000000000000000000),
 ( 0.9856612449720755231, 0.9999558406602322425),
 ( 0.9856612449720755231, 0.9999558406602322425),
 ( 1.000000000000000000, 1.000000000000000000) ) ) 
 REPRESENTATION_ITEM ( '' )  SURFACE ( )  );
#22731 = CARTESIAN_POINT ( 'NONE',  ( 0.2767916011545359933, -7.727819755721539785, 9.504925141026333790 ) ) ;
#22732 = LINE ( 'NONE', #42995, #46879 ) ;
#22733 = CARTESIAN_POINT ( 'NONE',  ( -35.00000000000000000, 4.237620530777800987, 11.42599468261430928 ) ) ;
#22735 = EDGE_LOOP ( 'NONE', ( #44243, #52124, #55822, #62232 ) ) ;
#22734 = CARTESIAN_POINT ( 'NONE',  ( -24.45373054277663982, 7.205321492283886187, 9.606256275160440339 ) ) ;
#22736 = CARTESIAN_POINT ( 'NONE',  ( -37.00000000000000711, -11.98254675519230084, 2.220215194441857331 ) ) ;
#22737 = EDGE_LOOP ( 'NONE', ( #49460, #24426, #7704, #40194 ) ) ;
#22738 = VECTOR ( 'NONE', #20307, 1000.000000000000000 ) ;
#22739 = CARTESIAN_POINT ( 'NONE',  ( -18.45734883033349405, 13.50390945406918775, 0.07345776429000988594 ) ) ;
#22740 = VECTOR ( 'NONE', #50633, 1000.000000000000000 ) ;
#22741 = ORIENTED_EDGE ( 'NONE', *, *, #61191, .T. ) ;
#22742 = DIRECTION ( 'NONE',  ( 0.000000000000000000, 0.01356324068817998940, -0.9999080150203990547 ) ) ;
#22743 = DIRECTION ( 'NONE',  ( 0.000000000000000000, 0.000000000000000000, -1.000000000000000000 ) ) ;
#22744 = DIRECTION ( 'NONE',  ( -1.000000000000000000, 0.000000000000000000, 0.000000000000000000 ) ) ;
#22746 = CARTESIAN_POINT ( 'NONE',  ( 0.2671309869109478319, -4.036029264453062204, 11.56263543972757368 ) ) ;
#22745 = AXIS2_PLACEMENT_3D ( 'NONE', #8073, #38653, #28342 ) ;
#22747 = CARTESIAN_POINT ( 'NONE',  ( 1.104777566491145668, 8.411711248089098092, 9.281442536087510575 ) ) ;
#22748 = DIRECTION ( 'NONE',  ( 0.000000000000000000, 0.000000000000000000, 1.000000000000000000 ) ) ;
#22749 = CARTESIAN_POINT ( 'NONE',  ( -22.28856623400852044, -3.603818606161813598, -0.9049353338066584707 ) ) ;
#22750 = ORIENTED_EDGE ( 'NONE', *, *, #33177, .F. ) ;
#22751 = ADVANCED_FACE ( 'NONE', ( #42996 ), #17486, .F. ) ;
#22752 = CIRCLE ( 'NONE', #45002, 12.74999999999999822 ) ;
#22753 = VERTEX_POINT ( 'NONE', #47352 ) ;
#22754 = LINE ( 'NONE', #62306, #15711 ) ;
#22755 = ORIENTED_EDGE ( 'NONE', *, *, #37954, .T. ) ;
#22756 = EDGE_CURVE ( 'NONE', #59369, #50472, #18639, .T. ) ;
#22757 = ORIENTED_EDGE ( 'NONE', *, *, #10118, .T. ) ;
#22758 = AXIS2_PLACEMENT_3D ( 'NONE', #18095, #62982, #17444 ) ;
#22759 = CARTESIAN_POINT ( 'NONE',  ( -35.00000000000000000, 11.42599468261435192, -4.237620530777677530 ) ) ;
#22760 = CARTESIAN_POINT ( 'NONE',  ( -22.28629837673888048, 3.348758206500249468, 1.594277649056495827 ) ) ;
#22761 = CARTESIAN_POINT ( 'NONE',  ( -27.28573687977896967, 2.702109387930250239, -1.043905432732882277 ) ) ;
#22762 = CARTESIAN_POINT ( 'NONE',  ( -22.31213670151049300, 2.108126385153810567, 3.145266995071653859 ) ) ;
#22763 = DIRECTION ( 'NONE',  ( -1.000000000000000000, -0.000000000000000000, -0.000000000000000000 ) ) ;
#22764 = CIRCLE ( 'NONE', #20622, 12.73084802173761787 ) ;
#22765 = CARTESIAN_POINT ( 'NONE',  ( -37.00000000000000711, 1.262958560998759472, 12.12087942037210198 ) ) ;
#22766 = EDGE_CURVE ( 'NONE', #65266, #59, #55783, .T. ) ;
#22767 = DIRECTION ( 'NONE',  ( 0.000000000000000000, -1.000000000000000000, 0.000000000000000000 ) ) ;
#22768 = ORIENTED_EDGE ( 'NONE', *, *, #32919, .F. ) ;
#22769 = CIRCLE ( 'NONE', #27025, 7.499999999999988454 ) ;
#22770 = CARTESIAN_POINT ( 'NONE',  ( 35.00000000000000000, 7.561043153948098450, 9.557269938331469206 ) ) ;
#22771 = DIRECTION ( 'NONE',  ( -0.3865475372811021382, -0.1791957239473601637, -0.9046932595863066418 ) ) ;
#22772 = EDGE_CURVE ( 'NONE', #56983, #39884, #58303, .T. ) ;
#22773 = B_SPLINE_CURVE_WITH_KNOTS ( 'NONE', 3,
 ( #51581, #26944, #57541, #10644, #21288, #40928, #6339 ),
 .UNSPECIFIED., .F., .F.,
 ( 4, 3, 4 ),
 ( 4.934695962917737974E-15, 0.002398160485434642879, 0.005002426799381695308 ),
 .UNSPECIFIED. ) ;
#22774 = CARTESIAN_POINT ( 'NONE',  ( 2.269879328256737772, -4.798845682294072823, 5.949827370243852442 ) ) ;
#22775 = CARTESIAN_POINT ( 'NONE',  ( 37.00000000000000711, 4.705694406421931860E-17, -3.469127814946512892E-15 ) ) ;
#22776 = AXIS2_PLACEMENT_3D ( 'NONE', #45316, #29367, #19407 ) ;
#22777 = DIRECTION ( 'NONE',  ( 0.000000000000000000, -0.01356324068817999114, 0.9999080150203989437 ) ) ;
#22778 = DIRECTION ( 'NONE',  ( -1.000000000000000000, 0.000000000000000000, 0.000000000000000000 ) ) ;
#22779 = CARTESIAN_POINT ( 'NONE',  ( 11.55599502239090448, 0.7141290965170358218, -11.97894361706956978 ) ) ;
#22780 = ORIENTED_EDGE ( 'NONE', *, *, #18112, .F. ) ;
#22781 = CARTESIAN_POINT ( 'NONE',  ( -41.00000000000000711, -25.49198847189178707, 0.7539676769129274314 ) ) ;
#22782 = AXIS2_PLACEMENT_3D ( 'NONE', #22725, #7085, #42987 ) ;
#22783 = CYLINDRICAL_SURFACE ( 'NONE', #55871, 12.74999999999999822 ) ;
#22784 = CARTESIAN_POINT ( 'NONE',  ( -22.27834755396594346, -0.7418417409069250068, -3.610802913011852411 ) ) ;
#22785 = AXIS2_PLACEMENT_3D ( 'NONE', #17136, #56386, #10834 ) ;
#22786 = CARTESIAN_POINT ( 'NONE',  ( 0.000000000000000000, -6.997684042076912192, 2.698595569414189210 ) ) ;
#22787 = DIRECTION ( 'NONE',  ( 0.000000000000000000, -0.01356324068817998940, 0.9999080150203990547 ) ) ;
#22788 = DIRECTION ( 'NONE',  ( -1.000000000000000000, 0.000000000000000000, 0.000000000000000000 ) ) ;
#22789 = EDGE_LOOP ( 'NONE', ( #15570, #9869, #34281, #32508 ) ) ;
#22790 = CARTESIAN_POINT ( 'NONE',  ( 17.38692437177838102, -10.06616489666143011, 6.600398882461584016 ) ) ;
#22791 = CARTESIAN_POINT ( 'NONE',  ( 5.536195898058073439, 0.007230647766619690241, -0.004468797463753810574 ) ) ;
#22792 = DIRECTION ( 'NONE',  ( 0.000000000000000000, 0.000000000000000000, 1.000000000000000000 ) ) ;
#22793 = CARTESIAN_POINT ( 'NONE',  ( 2.000000000000001776, 0.000000000000000000, 0.000000000000000000 ) ) ;
#22794 = ORIENTED_EDGE ( 'NONE', *, *, #13501, .F. ) ;
#22795 = CYLINDRICAL_SURFACE ( 'NONE', #6414, 7.499999999999988454 ) ;
#22796 = DIRECTION ( 'NONE',  ( 0.000000000000000000, 0.4698238015817365332, 0.8827602140260315533 ) ) ;
#22797 = ORIENTED_EDGE ( 'NONE', *, *, #10342, .F. ) ;
#22798 = VERTEX_POINT ( 'NONE', #52004 ) ;
#22799 = DIRECTION ( 'NONE',  ( -1.000000000000000000, 0.000000000000000000, -0.000000000000000000 ) ) ;
#22800 = AXIS2_PLACEMENT_3D ( 'NONE', #2540, #22809, #42388 ) ;
#22801 = EDGE_CURVE ( 'NONE', #30460, #22630, #3750, .T. ) ;
#22802 = CARTESIAN_POINT ( 'NONE',  ( 2.000000000000001776, -1.865193240757140991, 6.552473556515165498 ) ) ;
#22803 = ORIENTED_EDGE ( 'NONE', *, *, #42029, .T. ) ;
#22804 = CARTESIAN_POINT ( 'NONE',  ( 35.00000000000000000, 11.72195762423409704, 0.7536123767498881243 ) ) ;
#22805 = CARTESIAN_POINT ( 'NONE',  ( 1.719304012341273724, 0.7661785589598685275, -12.70777170743938456 ) ) ;
#22806 = FACE_OUTER_BOUND ( 'NONE', #23075, .T. ) ;
#22807 = CARTESIAN_POINT ( 'NONE',  ( 2.259025283528085737, -7.546748801935443396, -1.191911401085089750 ) ) ;
#22808 = CARTESIAN_POINT ( 'NONE',  ( 2.430348790457457220, 3.678671624790124994, -6.761480562106341630 ) ) ;
#22809 = DIRECTION ( 'NONE',  ( -1.000000000000000000, 0.000000000000000000, 0.000000000000000000 ) ) ;
#22811 = EDGE_LOOP ( 'NONE', ( #13020, #16264, #23672, #30713 ) ) ;
#22810 = FACE_OUTER_BOUND ( 'NONE', #11340, .T. ) ;
#22812 = CARTESIAN_POINT ( 'NONE',  ( 8.937200413558842982, 4.476360154859214902, 12.73625532737129795 ) ) ;
#22813 = ORIENTED_EDGE ( 'NONE', *, *, #1355, .F. ) ;
#22814 = CARTESIAN_POINT ( 'NONE',  ( 24.52288356478241482, -2.685886811157186749, -11.70110727047867805 ) ) ;
#22815 = VERTEX_POINT ( 'NONE', #21756 ) ;
#22816 = VERTEX_POINT ( 'NONE', #17412 ) ;
#22817 = CONTEXT_DEPENDENT_SHAPE_REPRESENTATION ( #34056, #41907 ) ;
#22818 = CARTESIAN_POINT ( 'NONE',  ( -27.27855387000350262, 12.26939275170278343, 5.631341004100471892 ) ) ;
#22819 = CARTESIAN_POINT ( 'NONE',  ( 0.2648978790185593790, -4.063980959784970537, -11.55204314799267884 ) ) ;
#22820 = DIRECTION ( 'NONE',  ( -1.000000000000000000, 0.000000000000000000, 0.000000000000000000 ) ) ;
#22821 = EDGE_CURVE ( 'NONE', #4778, #11936, #62286, .T. ) ;
#22822 = CARTESIAN_POINT ( 'NONE',  ( -48.96282442591977713, -0.2094399512627133919, -1.553366803981108601 ) ) ;
#22823 = DIRECTION ( 'NONE',  ( -1.000000000000000000, -0.000000000000000000, -0.000000000000000000 ) ) ;
#22824 = VERTEX_POINT ( 'NONE', #1477 ) ;
#22825 = CARTESIAN_POINT ( 'NONE',  ( -22.27720387087365239, 0.5572161790460056219, 3.639274226782802657 ) ) ;
#22826 = EDGE_CURVE ( 'NONE', #9772, #27953, #33474, .T. ) ;
#22827 = CYLINDRICAL_SURFACE ( 'NONE', #19150, 5.000000000000000888 ) ;
#22829 = ORIENTED_EDGE ( 'NONE', *, *, #51808, .F. ) ;
#22828 = DIRECTION ( 'NONE',  ( 0.000000000000000000, -0.01356324068817998767, 0.9999080150203990547 ) ) ;
#22830 = ORIENTED_EDGE ( 'NONE', *, *, #14830, .T. ) ;
#22831 = CARTESIAN_POINT ( 'NONE',  ( 5.516018279890452902, -0.004180585980735018921, -0.005331956019561697423 ) ) ;
#22832 = EDGE_CURVE ( 'NONE', #13076, #51860, #20457, .T. ) ;
#22833 = ORIENTED_EDGE ( 'NONE', *, *, #54836, .T. ) ;
#22834 = DIRECTION ( 'NONE',  ( -1.000000000000000000, 0.000000000000000000, 0.000000000000000000 ) ) ;
#22835 = CARTESIAN_POINT ( 'NONE',  ( -37.00000000000000711, 0.000000000000000000, 0.000000000000000000 ) ) ;
#22836 = CARTESIAN_POINT ( 'NONE',  ( 8.937200413559450496, 4.243630616744383133, 12.81805183698073947 ) ) ;
#22837 = CARTESIAN_POINT ( 'NONE',  ( -22.27786964138239867, 3.004507515156379593, -2.131221155130656353 ) ) ;
#22838 = CARTESIAN_POINT ( 'NONE',  ( -35.00000000000000000, 0.000000000000000000, 0.000000000000000000 ) ) ;
#22839 = CARTESIAN_POINT ( 'NONE',  ( -29.14293782047111847, 1.979001771404295784, 13.38056321518360292 ) ) ;
#22840 = EDGE_CURVE ( 'NONE', #1587, #64727, #22852, .T. ) ;
#22841 = CARTESIAN_POINT ( 'NONE',  ( 2.258463476536644254, 3.937122681832576188, -6.547539277367990351 ) ) ;
#22842 = ORIENTED_EDGE ( 'NONE', *, *, #63502, .T. ) ;
#22843 = DIRECTION ( 'NONE',  ( 0.000000000000000000, -0.01356324068817998940, 0.9999080150203990547 ) ) ;
#22845 = ADVANCED_FACE ( 'NONE', ( #46676 ), #1131, .T. ) ;
#22844 = B_SPLINE_CURVE_WITH_KNOTS ( 'NONE', 3,
 ( #8103, #7774, #22746, #24050, #48012, #2468, #3465, #43008, #33019, #39000, #38339, #8757, #33686, #63603, #29038, #59294, #64275, #38010, #58314, #28373, #28060, #18076 ),
 .UNSPECIFIED., .F., .F.,
 ( 4, 3, 3, 3, 3, 3, 3, 4 ),
 ( 8.741117365843378158E-19, 4.449119708437015698E-05, 6.626296329540635663E-05, 8.803456484963026257E-05, 0.0001098060367612851225, 0.0001315774408628581462, 0.0001760698110411260207, 0.0001829697163287835105 ),
 .UNSPECIFIED. ) ;
#22846 = ORIENTED_EDGE ( 'NONE', *, *, #36174, .F. ) ;
#22847 = LINE ( 'NONE', #52770, #29970 ) ;
#22848 = CARTESIAN_POINT ( 'NONE',  ( 35.00000000000000000, 4.705694406421931860E-17, -3.469127814946512892E-15 ) ) ;
#22849 = CIRCLE ( 'NONE', #53616, 12.73084802173761787 ) ;
#22850 = CARTESIAN_POINT ( 'NONE',  ( 2.556980015513487192, -2.862731173723767508, -7.190718924764468056 ) ) ;
#22851 = FACE_OUTER_BOUND ( 'NONE', #34409, .T. ) ;
#22852 = CIRCLE ( 'NONE', #23903, 4.999999999999999112 ) ;
#22853 = ORIENTED_EDGE ( 'NONE', *, *, #47994, .F. ) ;
#22854 = ORIENTED_EDGE ( 'NONE', *, *, #40900, .T. ) ;
#22855 = CARTESIAN_POINT ( 'NONE',  ( -27.09861164373156583, 0.1603819633258403432, 2.328930759213672541 ) ) ;
#22856 = EDGE_CURVE ( 'NONE', #10868, #11758, #16433, .T. ) ;
#22857 = VERTEX_POINT ( 'NONE', #2797 ) ;
#22858 = DIRECTION ( 'NONE',  ( 0.000000000000000000, -0.4134677391718577510, -0.9105187689795923855 ) ) ;
#22859 = DIRECTION ( 'NONE',  ( 0.000000000000000000, 0.01356324068817998940, -0.9999080150203990547 ) ) ;
#22860 = EDGE_CURVE ( 'NONE', #27180, #32432, #5377, .T. ) ;
#22861 = CARTESIAN_POINT ( 'NONE',  ( -37.00000000000000711, 0.000000000000000000, 0.000000000000000000 ) ) ;
#22862 = CARTESIAN_POINT ( 'NONE',  ( 1.719304012340733934, -12.20344780066092305, -3.626341562669774365 ) ) ;
#22863 = ORIENTED_EDGE ( 'NONE', *, *, #10014, .T. ) ;
#22864 = CARTESIAN_POINT ( 'NONE',  ( 2.963017218115612028, 2.328652339224351664, 7.522800244854583873 ) ) ;
#22865 = CARTESIAN_POINT ( 'NONE',  ( 17.95036338764469619, 10.25346347048778739, 8.788876757364576520 ) ) ;
#22866 = CARTESIAN_POINT ( 'NONE',  ( -29.65781431629226361, -0.5515374799640114789, -13.49546472197990532 ) ) ;
#22867 = CARTESIAN_POINT ( 'NONE',  ( -31.45682506574155113, -3.065323467461852136, 24.16565572891780178 ) ) ;
#22868 = CIRCLE ( 'NONE', #21787, 5.000000000000000888 ) ;
#22869 = CARTESIAN_POINT ( 'NONE',  ( -27.08416974970326407, -0.4151546250413312156, -2.253221199357866134 ) ) ;
#22870 = CARTESIAN_POINT ( 'NONE',  ( -37.00000000000000711, 8.146229107149400406, 9.063649021438985542 ) ) ;
#22871 = ORIENTED_EDGE ( 'NONE', *, *, #36241, .T. ) ;
#22872 = DIRECTION ( 'NONE',  ( -1.000000000000000000, 0.000000000000000000, 0.000000000000000000 ) ) ;
#22873 = CARTESIAN_POINT ( 'NONE',  ( 5.514970785353741078, 0.001897634820904481583, -0.004324946436530190987 ) ) ;
#22874 = CARTESIAN_POINT ( 'NONE',  ( 35.00000000000000000, 4.705694406421931860E-17, -3.469127814946512892E-15 ) ) ;
#22875 = ORIENTED_EDGE ( 'NONE', *, *, #6546, .T. ) ;
#22876 = DIRECTION ( 'NONE',  ( 1.000000000000000000, 0.000000000000000000, 0.000000000000000000 ) ) ;
#22877 = CARTESIAN_POINT ( 'NONE',  ( 3.152665057734126197, 7.719888720907812640, 1.848755561852068130 ) ) ;
#22878 = CARTESIAN_POINT ( 'NONE',  ( -37.00000000000000711, 12.08216339958900676, 1.591260454995285789 ) ) ;
#22879 = CARTESIAN_POINT ( 'NONE',  ( 5.516018279890452902, -0.0002248006052447136570, 0.006771744149385739570 ) ) ;
#22880 = CARTESIAN_POINT ( 'NONE',  ( 0.2648321136542715060, -11.55519783395230604, 4.054947570138854651 ) ) ;
#22881 = ADVANCED_FACE ( 'NONE', ( #33992 ), #54306, .T. ) ;
#22882 = ORIENTED_EDGE ( 'NONE', *, *, #50969, .T. ) ;
#22883 = ORIENTED_EDGE ( 'NONE', *, *, #45577, .T. ) ;
#22884 = CARTESIAN_POINT ( 'NONE',  ( 0.2657645697724703160, 1.977350809428533029, 12.08564806881062026 ) ) ;
#22885 = ORIENTED_EDGE ( 'NONE', *, *, #64119, .T. ) ;
#22886 = FACE_OUTER_BOUND ( 'NONE', #12027, .T. ) ;
#22887 = DIRECTION ( 'NONE',  ( -1.000000000000000000, 0.000000000000000000, -0.000000000000000000 ) ) ;
#22888 = DIRECTION ( 'NONE',  ( -1.000000000000000000, 0.000000000000000000, 0.000000000000000000 ) ) ;
#22889 = DIRECTION ( 'NONE',  ( -0.000000000000000000, -0.000000000000000000, -1.000000000000000000 ) ) ;
#22890 = DIRECTION ( 'NONE',  ( -0.000000000000000000, -1.000000000000000000, -0.000000000000000000 ) ) ;
#22891 = CARTESIAN_POINT ( 'NONE',  ( 2.251152103363646351, 7.542379262759450143, 1.202724109297105937 ) ) ;
#22892 = DIRECTION ( 'NONE',  ( 0.000000000000000000, -0.8369827122275401710, -0.5472293298355185298 ) ) ;
#22893 = VERTEX_POINT ( 'NONE', #29027 ) ;
#22894 = VERTEX_POINT ( 'NONE', #44299 ) ;
#22895 = EDGE_CURVE ( 'NONE', #55534, #2111, #36652, .T. ) ;
#22896 = DIRECTION ( 'NONE',  ( 0.000000000000000000, 0.01356324068818000328, -0.9999080150203990547 ) ) ;
#22897 = ORIENTED_EDGE ( 'NONE', *, *, #6171, .T. ) ;
#22899 = CARTESIAN_POINT ( 'NONE',  ( -22.27719381268171617, 2.618044180756139205, -2.588413841766857182 ) ) ;
#22898 = AXIS2_PLACEMENT_3D ( 'NONE', #44379, #34724, #23465 ) ;
#22900 = CARTESIAN_POINT ( 'NONE',  ( 1.020182472824830988, 8.370187102470797669, -9.280950437305046208 ) ) ;
#22901 = EDGE_CURVE ( 'NONE', #53784, #62115, #7734, .T. ) ;
#22902 = CARTESIAN_POINT ( 'NONE',  ( 35.00000000000000000, 7.971186206369472060, -9.217970097227754067 ) ) ;
#22903 = ORIENTED_EDGE ( 'NONE', *, *, #31967, .F. ) ;
#22904 = CARTESIAN_POINT ( 'NONE',  ( 5.520433897694421610, -0.01491416502703812180, 0.002108682515300225845 ) ) ;
#22905 = CARTESIAN_POINT ( 'NONE',  ( 5.536195898058073439, -0.005656495196970933587, 0.006344799443923416181 ) ) ;
#22906 = DIRECTION ( 'NONE',  ( -0.2475719085175093481, -0.000000000000000000, -0.9688695217174488894 ) ) ;
#22907 = ORIENTED_EDGE ( 'NONE', *, *, #29784, .T. ) ;
#22908 = ORIENTED_EDGE ( 'NONE', *, *, #30287, .F. ) ;
#22909 = CARTESIAN_POINT ( 'NONE',  ( 2.000000000000001776, -7.387287142779332960, -1.295372019972250710 ) ) ;
#22910 = ADVANCED_FACE ( 'NONE', ( #43315 ), #53654, .T. ) ;
#22911 = EDGE_LOOP ( 'NONE', ( #12613, #20328, #49494, #49657 ) ) ;
#22912 = CARTESIAN_POINT ( 'NONE',  ( 2.288423627607478750, 3.963881558061958632, 6.543055113184225391 ) ) ;
#22913 = EDGE_LOOP ( 'NONE', ( #24258, #55285, #34126, #41826 ) ) ;
#22914 = VERTEX_POINT ( 'NONE', #43645 ) ;
#22915 = CARTESIAN_POINT ( 'NONE',  ( -22.27720387087365239, -2.873095842208885031, 2.302200479844923375 ) ) ;
#22916 = CARTESIAN_POINT ( 'NONE',  ( 2.251139882113697865, 5.003859976902833573, -5.770207524086111484 ) ) ;
#22917 = AXIS2_PLACEMENT_3D ( 'NONE', #41811, #47151, #62104 ) ;
#22918 = FACE_OUTER_BOUND ( 'NONE', #22356, .T. ) ;
#22919 = CARTESIAN_POINT ( 'NONE',  ( 0.2911222467163572247, 8.040284153519499100, -9.248441845564602914 ) ) ;
#22920 = DIRECTION ( 'NONE',  ( 0.000000000000000000, 0.8989688749565173387, 0.4380125133593943398 ) ) ;
#22921 = CARTESIAN_POINT ( 'NONE',  ( 0.3057689695767461524, 11.59726335252433316, 3.975296631252007717 ) ) ;
#22922 =( BOUNDED_CURVE ( )  B_SPLINE_CURVE ( 3, ( #54363, #28104, #18118, #48397 ),
 .UNSPECIFIED., .F., .F. ) 
 B_SPLINE_CURVE_WITH_KNOTS ( ( 4, 4 ),
 ( 6.141081411243264121, 6.425289203115908343 ),
 .UNSPECIFIED. ) 
 CURVE ( )  GEOMETRIC_REPRESENTATION_ITEM ( )  RATIONAL_B_SPLINE_CURVE ( ( 1.000000000000000000, 0.9932801471353227551, 0.9932801471353227551, 1.000000000000000000 ) ) 
 REPRESENTATION_ITEM ( '' )  );
#22923 = EDGE_LOOP ( 'NONE', ( #23286, #37709, #18529, #32208 ) ) ;
#22924 = DIRECTION ( 'NONE',  ( 0.000000000000000000, 0.1764146379942750642, 0.9843159429275485373 ) ) ;
#22925 = EDGE_CURVE ( 'NONE', #1336, #7715, #19225, .T. ) ;
#22926 = DIRECTION ( 'NONE',  ( -1.000000000000000000, 0.000000000000000000, 0.000000000000000000 ) ) ;
#22927 = CARTESIAN_POINT ( 'NONE',  ( 2.305787727787084407, 3.682701754025606178, -6.711944854845784292 ) ) ;
#22928 = ADVANCED_FACE ( 'NONE', ( #64263 ), #23055, .F. ) ;
#22929 = LINE ( 'NONE', #5765, #18931 ) ;
#22930 = CARTESIAN_POINT ( 'NONE',  ( 0.3675815128205894289, -8.093875121226016489, -9.235491948680088825 ) ) ;
#22931 = CARTESIAN_POINT ( 'NONE',  ( 1.719304012341273724, 0.7661785589598685275, -12.70777170743938456 ) ) ;
#22932 = CARTESIAN_POINT ( 'NONE',  ( -27.08423923533013422, 1.376387618994802997, 1.832018136655343188 ) ) ;
#22933 = CARTESIAN_POINT ( 'NONE',  ( -35.00000000000000000, -8.927548052240956267, 8.295159312811819063 ) ) ;
#22934 = CARTESIAN_POINT ( 'NONE',  ( 0.2648978790185584908, 7.972372351883154629, -9.295532325666371776 ) ) ;
#22935 = ADVANCED_FACE ( 'NONE', ( #3114 ), #23376, .T. ) ;
#22936 = VERTEX_POINT ( 'NONE', #18065 ) ;
#22937 = LINE ( 'NONE', #62483, #2539 ) ;
#22938 = EDGE_CURVE ( 'NONE', #44205, #62469, #9029, .T. ) ;
#22939 = AXIS2_PLACEMENT_3D ( 'NONE', #56118, #30208, #1271 ) ;
#22940 =( BOUNDED_CURVE ( )  B_SPLINE_CURVE ( 3, ( #61105, #51486, #5932, #4931 ),
 .UNSPECIFIED., .F., .F. ) 
 B_SPLINE_CURVE_WITH_KNOTS ( ( 4, 4 ),
 ( 0.5962944384795770825, 0.6311393659967107217 ),
 .UNSPECIFIED. ) 
 CURVE ( )  GEOMETRIC_REPRESENTATION_ITEM ( )  RATIONAL_B_SPLINE_CURVE ( ( 1.000000000000000000, 0.9998988218115538729, 0.9998988218115538729, 1.000000000000000000 ) ) 
 REPRESENTATION_ITEM ( '' )  );
#22941 = ORIENTED_EDGE ( 'NONE', *, *, #36143, .F. ) ;
#22942 = CARTESIAN_POINT ( 'NONE',  ( 0.000000000000000000, -6.253963800348222968, -4.139799123621093813 ) ) ;
#22943 = CARTESIAN_POINT ( 'NONE',  ( 41.00000000000000711, -1.694065894508793271E-18, 4.500000000000001776 ) ) ;
#22944 = CARTESIAN_POINT ( 'NONE',  ( 12.14692673679996737, -13.20602977273170175, -2.806489945550152854 ) ) ;
#22945 = EDGE_CURVE ( 'NONE', #64097, #7860, #34329, .T. ) ;
#22946 = DIRECTION ( 'NONE',  ( -1.000000000000000000, -0.000000000000000000, -0.000000000000000000 ) ) ;
#22947 = CARTESIAN_POINT ( 'NONE',  ( 2.241352910868908310, 2.689314586382351546, 7.145045428366586293 ) ) ;
#22948 = ORIENTED_EDGE ( 'NONE', *, *, #14154, .F. ) ;
#22949 = DIRECTION ( 'NONE',  ( 0.000000000000000000, -0.01356324068817991828, 0.9999080150203990547 ) ) ;
#22950 = DIRECTION ( 'NONE',  ( 0.000000000000000000, 0.8696919319575165952, 0.4935949184179292404 ) ) ;
#22951 = CARTESIAN_POINT ( 'NONE',  ( 2.080613030138687147, 9.283828902438220978E-16, 7.580821595991582562 ) ) ;
#22952 = DIRECTION ( 'NONE',  ( -1.000000000000000000, 0.000000000000000000, 0.000000000000000000 ) ) ;
#22953 = AXIS2_PLACEMENT_3D ( 'NONE', #59961, #59627, #14053 ) ;
#22954 = LINE ( 'NONE', #63811, #34995 ) ;
#22955 = ORIENTED_EDGE ( 'NONE', *, *, #21624, .T. ) ;
#22956 = DIRECTION ( 'NONE',  ( 1.000000000000000000, 0.000000000000000000, -0.000000000000000000 ) ) ;
#22957 = LINE ( 'NONE', #18296, #62385 ) ;
#22958 = CARTESIAN_POINT ( 'NONE',  ( 2.257661810676420799, -3.936095962955250993, -6.547845034191129621 ) ) ;
#22959 = EDGE_CURVE ( 'NONE', #61226, #57314, #728, .T. ) ;
#22960 = ORIENTED_EDGE ( 'NONE', *, *, #40864, .T. ) ;
#22961 = CARTESIAN_POINT ( 'NONE',  ( 2.354167843600960097, -6.278647867796540716, 25.00000000000000000 ) ) ;
#22962 = VERTEX_POINT ( 'NONE', #14368 ) ;
#22963 = DIRECTION ( 'NONE',  ( -1.000000000000000000, 0.000000000000000000, 0.000000000000000000 ) ) ;
#22964 = DIRECTION ( 'NONE',  ( 0.3865475372811021382, 0.1410344188397341658, 0.9114221272958283881 ) ) ;
#22965 = CARTESIAN_POINT ( 'NONE',  ( -25.00000000000000355, -9.999999999999998224, -24.00000000000000000 ) ) ;
#22966 = DIRECTION ( 'NONE',  ( 0.000000000000000000, 0.01356324068817998940, -0.9999080150203990547 ) ) ;
#22967 = CARTESIAN_POINT ( 'NONE',  ( -22.28776923226071105, -2.100802264239985284, -3.061913732988077452 ) ) ;
#22968 = VERTEX_POINT ( 'NONE', #20342 ) ;
#22969 = EDGE_CURVE ( 'NONE', #10113, #19062, #56847, .T. ) ;
#22970 = ORIENTED_EDGE ( 'NONE', *, *, #16779, .F. ) ;
#22971 = EDGE_LOOP ( 'NONE', ( #46178, #7056, #43470, #64652 ) ) ;
#22972 = CARTESIAN_POINT ( 'NONE',  ( 2.241311220309555097, 7.205198716057821251, -2.523702734785272739 ) ) ;
#22973 = CARTESIAN_POINT ( 'NONE',  ( 35.00000000000000000, 4.705694406421931860E-17, -3.469127814946512892E-15 ) ) ;
#22974 = ORIENTED_EDGE ( 'NONE', *, *, #12161, .T. ) ;
#22975 = CIRCLE ( 'NONE', #59060, 12.18649999999999878 ) ;
#22976 = CARTESIAN_POINT ( 'NONE',  ( 145.1370849898475797, 3.309064568108273190E-14, 0.000000000000000000 ) ) ;
#22977 = CARTESIAN_POINT ( 'NONE',  ( -22.28482751661422867, -0.2989970708918257558, -3.692400780723914089 ) ) ;
#22978 = ORIENTED_EDGE ( 'NONE', *, *, #61348, .F. ) ;
#22979 = VECTOR ( 'NONE', #37318, 1000.000000000000000 ) ;
#22980 = CARTESIAN_POINT ( 'NONE',  ( -27.08416974970326407, -0.3922151116844065921, -2.257332547928110777 ) ) ;
#22981 = FACE_OUTER_BOUND ( 'NONE', #37794, .T. ) ;
#22982 = DIRECTION ( 'NONE',  ( -1.000000000000000000, 0.000000000000000000, 0.000000000000000000 ) ) ;
#22983 = ORIENTED_EDGE ( 'NONE', *, *, #35744, .F. ) ;
#22984 = EDGE_LOOP ( 'NONE', ( #42421, #56525, #43818, #45795, #55295, #53351 ) ) ;
#22985 = ADVANCED_FACE ( 'NONE', ( #34640 ), #35298, .T. ) ;
#22986 = ORIENTED_EDGE ( 'NONE', *, *, #45621, .T. ) ;
#22987 = ORIENTED_EDGE ( 'NONE', *, *, #43142, .F. ) ;
#22988 = CARTESIAN_POINT ( 'NONE',  ( 5.516018279890452902, 0.005752102158674347356, 0.003580555109620895717 ) ) ;
#22989 = EDGE_CURVE ( 'NONE', #42463, #21230, #65310, .T. ) ;
#22990 = CARTESIAN_POINT ( 'NONE',  ( 16.10065672031734962, -35.00000000000000000, -4.574893970807972110 ) ) ;
#22991 = DIRECTION ( 'NONE',  ( 1.000000000000000000, 0.000000000000000000, 0.000000000000000000 ) ) ;
#22992 = DIRECTION ( 'NONE',  ( -1.000000000000000000, 0.000000000000000000, 0.000000000000000000 ) ) ;
#22993 = CARTESIAN_POINT ( 'NONE',  ( 35.00000000000000000, -8.830544224263011444, -9.196955404009264257 ) ) ;
#22994 = CYLINDRICAL_SURFACE ( 'NONE', #23896, 5.000000000000000888 ) ;
#22995 = CARTESIAN_POINT ( 'NONE',  ( -27.58700550753028224, -9.955571130810017877, -6.705838893603189632 ) ) ;
#22996 = ORIENTED_EDGE ( 'NONE', *, *, #56579, .T. ) ;
#22997 = CARTESIAN_POINT ( 'NONE',  ( 0.6473888112830233910, 10.87693551365371292, 5.898884566269048335 ) ) ;
#22998 = EDGE_LOOP ( 'NONE', ( #20275, #6455, #59146, #15241 ) ) ;
#22999 = CARTESIAN_POINT ( 'NONE',  ( 2.251139882113958990, -2.728563091335203250, 7.133642337268851108 ) ) ;
#23000 = CARTESIAN_POINT ( 'NONE',  ( 2.242418902651535095, 6.661183998166030129, 3.730710532465902229 ) ) ;
#23001 = ORIENTED_EDGE ( 'NONE', *, *, #59024, .F. ) ;
#23002 = FACE_OUTER_BOUND ( 'NONE', #19035, .T. ) ;
#23003 = CARTESIAN_POINT ( 'NONE',  ( 0.2958664285830381879, 6.318165763623623477, 10.50235171906342657 ) ) ;
#23004 = CARTESIAN_POINT ( 'NONE',  ( -22.27384469013076185, 2.581192766446265274, 2.625926801827853208 ) ) ;
#23005 = EDGE_CURVE ( 'NONE', #7169, #46362, #30328, .T. ) ;
#23006 = ORIENTED_EDGE ( 'NONE', *, *, #24960, .F. ) ;
#23007 = VERTEX_POINT ( 'NONE', #26003 ) ;
#23008 = CARTESIAN_POINT ( 'NONE',  ( 2.000000000000001776, -0.4804830611970390408, 6.919838746524553663 ) ) ;
#23009 = ADVANCED_FACE ( 'NONE', ( #40957 ), #25330, .T. ) ;
#23010 = B_SPLINE_CURVE_WITH_KNOTS ( 'NONE', 3,
 ( #61155, #50211, #35548, #30552, #14916, #54548, #40534, #8978, #59856, #9282, #55177, #49873, #50539, #4322, #24594, #20253 ),
 .UNSPECIFIED., .F., .F.,
 ( 4, 3, 3, 3, 3, 4 ),
 ( 1.084202172485504434E-19, 0.0003017745587525236749, 0.0006035491769808723310, 0.0009053241094668153808, 0.001207275924540830887, 0.001510325902534668824 ),
 .UNSPECIFIED. ) ;
#23011 = ORIENTED_EDGE ( 'NONE', *, *, #58192, .F. ) ;
#23012 = DIRECTION ( 'NONE',  ( 0.000000000000000000, 0.000000000000000000, -1.000000000000000000 ) ) ;
#23013 = DIRECTION ( 'NONE',  ( 0.000000000000000000, 0.3218879778915905154, -0.9467777615094595811 ) ) ;
#23014 = CARTESIAN_POINT ( 'NONE',  ( -27.08416813689867553, 2.150738950797704607, 0.7899859999124249077 ) ) ;
#23015 = ADVANCED_FACE ( 'NONE', ( #54936 ), #46287, .T. ) ;
#23016 = CARTESIAN_POINT ( 'NONE',  ( 0.3002738374340848670, -9.243462099800773046, -8.050654058169964600 ) ) ;
#23017 = CARTESIAN_POINT ( 'NONE',  ( -18.25006854224444908, -9.443202773001939221, 7.404452808139724063 ) ) ;
#23018 = ORIENTED_EDGE ( 'NONE', *, *, #52910, .F. ) ;
#23019 = CIRCLE ( 'NONE', #57006, 5.000000000000000888 ) ;
#23020 = CARTESIAN_POINT ( 'NONE',  ( 0.2657645697724709266, -12.03308811492267161, -2.275433120353216321 ) ) ;
#23021 = B_SPLINE_CURVE_WITH_KNOTS ( 'NONE', 3,
 ( #21057, #5475, #25741, #41338, #486, #20751, #61302 ),
 .UNSPECIFIED., .F., .F.,
 ( 4, 3, 4 ),
 ( 3.553148716079863012E-15, 0.002398160485434544433, 0.005002426799380215588 ),
 .UNSPECIFIED. ) ;
#23022 = EDGE_CURVE ( 'NONE', #11696, #28136, #8000, .T. ) ;
#23023 = CARTESIAN_POINT ( 'NONE',  ( 2.305787727787084851, -7.508843116234144688, -1.493241775258500770 ) ) ;
#23024 = CARTESIAN_POINT ( 'NONE',  ( 0.000000000000000000, -6.470132594555817462, 2.133363481234057168 ) ) ;
#23025 = CARTESIAN_POINT ( 'NONE',  ( 5.514970785353741078, 0.003262412238248228995, -0.003415090918276198536 ) ) ;
#23026 = DIRECTION ( 'NONE',  ( 1.000000000000000000, -0.000000000000000000, 0.000000000000000000 ) ) ;
#23027 = CARTESIAN_POINT ( 'NONE',  ( 6.507052240825795586, -8.968520638857693683, -7.975644518742436517 ) ) ;
#23028 = CARTESIAN_POINT ( 'NONE',  ( -22.28073302975500880, -2.626377654649347804, -2.595086548180010055 ) ) ;
#23029 = B_SPLINE_CURVE_WITH_KNOTS ( 'NONE', 3,
 ( #17629, #7983, #48233, #22611, #52862, #47240, #33231, #17291, #1995, #47876, #53541, #28249, #42876, #6987, #63164, #2682 ),
 .UNSPECIFIED., .F., .F.,
 ( 4, 3, 3, 3, 3, 4 ),
 ( 8.673617379884035472E-19, 0.0002176109881720253794, 0.0004352086762394625640, 0.0006528017811446917363, 0.0007615147961451743368, 0.0009453342004947433517 ),
 .UNSPECIFIED. ) ;
#23030 = PRODUCT_DEFINITION ( 'UNKNOWN', '', #61121, #57882 ) ;
#23031 = EDGE_LOOP ( 'NONE', ( #42337, #38622, #17403, #63380 ) ) ;
#23032 = CARTESIAN_POINT ( 'NONE',  ( -27.35552965826137140, 1.320216934008397569, 2.810569013793730697 ) ) ;
#23033 = EDGE_CURVE ( 'NONE', #12853, #53880, #43006, .T. ) ;
#23034 = VERTEX_POINT ( 'NONE', #4417 ) ;
#23035 = CARTESIAN_POINT ( 'NONE',  ( 0.2717059086739036511, 1.953280559502855951, -12.09156413799788155 ) ) ;
#23036 = DIRECTION ( 'NONE',  ( 1.000000000000000000, 0.000000000000000000, 0.000000000000000000 ) ) ;
#23037 = CYLINDRICAL_SURFACE ( 'NONE', #49143, 6.936499999999988120 ) ;
#23038 = VERTEX_POINT ( 'NONE', #29991 ) ;
#23039 = LINE ( 'NONE', #27350, #41559 ) ;
#23040 = VERTEX_POINT ( 'NONE', #45607 ) ;
#23041 = CARTESIAN_POINT ( 'NONE',  ( -36.00000000000000711, -0.9416912585473466990, -12.71517666308949046 ) ) ;
#23042 = EDGE_CURVE ( 'NONE', #54738, #22141, #53664, .T. ) ;
#23043 = ORIENTED_EDGE ( 'NONE', *, *, #60890, .F. ) ;
#23044 = ORIENTED_EDGE ( 'NONE', *, *, #11568, .T. ) ;
#23045 = DIRECTION ( 'NONE',  ( -1.000000000000000000, 0.000000000000000000, 0.000000000000000000 ) ) ;
#23046 = CARTESIAN_POINT ( 'NONE',  ( -22.27704833740210333, -3.351945466913909932, -1.521679877253181878 ) ) ;
#23047 = ORIENTED_EDGE ( 'NONE', *, *, #39112, .F. ) ;
#23048 = CARTESIAN_POINT ( 'NONE',  ( 2.305787727787085295, 5.756228004061457959, 5.047606869483074910 ) ) ;
#23049 = CARTESIAN_POINT ( 'NONE',  ( 2.639814597422737386, -2.896050884406582426, 7.207158938903940992 ) ) ;
#23050 = DIRECTION ( 'NONE',  ( -1.000000000000000000, 0.000000000000000000, 0.000000000000000000 ) ) ;
#23051 = FACE_OUTER_BOUND ( 'NONE', #41012, .T. ) ;
#23052 = ORIENTED_EDGE ( 'NONE', *, *, #26876, .T. ) ;
#23053 = CARTESIAN_POINT ( 'NONE',  ( 0.3006302518452007022, -7.704827863860860049, 9.533790235540713809 ) ) ;
#23054 = DIRECTION ( 'NONE',  ( 0.000000000000000000, 0.000000000000000000, -1.000000000000000000 ) ) ;
#23055 = CYLINDRICAL_SURFACE ( 'NONE', #64228, 14.19297241773857188 ) ;
#23057 = ORIENTED_EDGE ( 'NONE', *, *, #19890, .F. ) ;
#23056 = CARTESIAN_POINT ( 'NONE',  ( 0.2648978790185619880, -12.08224454301447182, -1.996248716311752824 ) ) ;
#23058 = CARTESIAN_POINT ( 'NONE',  ( 5.515539859299206427, 0.002856745161749541222, -0.005336559634876951626 ) ) ;
#23059 = ADVANCED_FACE ( 'NONE', ( #15663 ), #50303, .T. ) ;
#23060 = ADVANCED_FACE ( 'NONE', ( #45290 ), #30970, .T. ) ;
#23061 = EDGE_LOOP ( 'NONE', ( #9207, #22693, #53401, #43485 ) ) ;
#23062 = CARTESIAN_POINT ( 'NONE',  ( -18.00215407324301964, 13.42696834491351154, 1.444777302739133296 ) ) ;
#23063 = ORIENTED_EDGE ( 'NONE', *, *, #30117, .F. ) ;
#23064 = AXIS2_PLACEMENT_3D ( 'NONE', #54231, #14301, #28617 ) ;
#23065 = CARTESIAN_POINT ( 'NONE',  ( 2.241352910868908310, 6.652881166698511706, 3.744764251557016532 ) ) ;
#23066 = DIRECTION ( 'NONE',  ( 1.000000000000000000, 0.000000000000000000, 0.000000000000000000 ) ) ;
#23067 = EDGE_CURVE ( 'NONE', #60414, #7557, #50478, .T. ) ;
#23068 = DIRECTION ( 'NONE',  ( 0.000000000000000000, -0.01356324068817999114, 0.9999080150203989437 ) ) ;
#23069 = CARTESIAN_POINT ( 'NONE',  ( 37.00000000000000711, -7.474872387601069867, -9.060822531526026680 ) ) ;
#23070 = CARTESIAN_POINT ( 'NONE',  ( 0.3109076770649057964, 9.542672295796823079, 7.699281309344357282 ) ) ;
#23071 = LINE ( 'NONE', #57014, #29296 ) ;
#23072 = CARTESIAN_POINT ( 'NONE',  ( 2.241352910868908310, -5.901537464758487062, 4.843133558968109043 ) ) ;
#23073 = ORIENTED_EDGE ( 'NONE', *, *, #16660, .F. ) ;
#23074 = DIRECTION ( 'NONE',  ( 1.000000000000000000, 0.000000000000000000, 0.000000000000000000 ) ) ;
#23075 = EDGE_LOOP ( 'NONE', ( #7975, #37058, #27594, #55858 ) ) ;
#23076 = ORIENTED_EDGE ( 'NONE', *, *, #61195, .T. ) ;
#23077 = CARTESIAN_POINT ( 'NONE',  ( 2.000000000000001776, 5.396716205731493687, -4.158041573745044239 ) ) ;
#23078 = CARTESIAN_POINT ( 'NONE',  ( -22.29677679919927868, 3.364642266483124811, 1.633785040807670175 ) ) ;
#23079 = CARTESIAN_POINT ( 'NONE',  ( -10.00000000000000178, 0.000000000000000000, 0.000000000000000000 ) ) ;
#23080 = CARTESIAN_POINT ( 'NONE',  ( -22.28482751661422867, 2.105139449411431052, 3.048214341614463585 ) ) ;
#23081 = CARTESIAN_POINT ( 'NONE',  ( 2.000000000000001776, 4.570217215903371155, 5.218059682435623792 ) ) ;
#23082 = ADVANCED_FACE ( 'NONE', ( #60577 ), #65037, .F. ) ;
#23083 = CARTESIAN_POINT ( 'NONE',  ( 2.000000000000001776, 2.562706407243636075, 6.312399813420339179 ) ) ;
#23084 = CARTESIAN_POINT ( 'NONE',  ( 37.00000000000000711, -8.551552972817137999, -8.052525312709853722 ) ) ;
#23085 = VERTEX_POINT ( 'NONE', #36284 ) ;
#23086 = CARTESIAN_POINT ( 'NONE',  ( 37.00000000000000711, 7.215058775251253387, -9.821084925794595577 ) ) ;
#23087 = CARTESIAN_POINT ( 'NONE',  ( -27.08426571771018487, -1.357728109767519564, -1.845988025802334231 ) ) ;
#23088 = EDGE_CURVE ( 'NONE', #63048, #22962, #6914, .T. ) ;
#23089 = CARTESIAN_POINT ( 'NONE',  ( 2.260457164927193396, -4.804526096743045649, 5.941202713844093708 ) ) ;
#23090 = CARTESIAN_POINT ( 'NONE',  ( 0.000000000000000000, 0.000000000000000000, 0.000000000000000000 ) ) ;
#23091 = DIRECTION ( 'NONE',  ( 0.000000000000000000, -0.01356324068817998940, 0.9999080150203990547 ) ) ;
#23092 = CARTESIAN_POINT ( 'NONE',  ( 9.268253959421528521, 2.865053375548464398, -11.65528265421164811 ) ) ;
#23093 = ORIENTED_EDGE ( 'NONE', *, *, #47364, .T. ) ;
#23094 = DIRECTION ( 'NONE',  ( 1.000000000000000000, -0.000000000000000000, -0.000000000000000000 ) ) ;
#23095 = CARTESIAN_POINT ( 'NONE',  ( -35.00000000000000000, 10.64792938439755332, 5.927257550915355999 ) ) ;
#23096 = CARTESIAN_POINT ( 'NONE',  ( -27.04788180060268843, -1.373100113388784349, -2.923150379392654319 ) ) ;
#23097 = VECTOR ( 'NONE', #53080, 1000.000000000000000 ) ;
#23098 = CIRCLE ( 'NONE', #5035, 12.74999999999999822 ) ;
#23099 = CARTESIAN_POINT ( 'NONE',  ( 37.00000000000000711, 9.700295462048767803, 7.376655759824772396 ) ) ;
#23100 = DIRECTION ( 'NONE',  ( -1.000000000000000000, 0.000000000000000000, 0.000000000000000000 ) ) ;
#23101 = ADVANCED_FACE ( 'NONE', ( #16990 ), #57242, .T. ) ;
#23102 =( BOUNDED_SURFACE ( )  B_SPLINE_SURFACE ( 3, 1, ( 
 ( #55577, #64232 ),
 ( #29963, #50268 ),
 ( #28992, #34614 ),
 ( #10017, #60544 ) ),
 .UNSPECIFIED., .F., .F., .F. ) 
 B_SPLINE_SURFACE_WITH_KNOTS ( ( 4, 4 ),
 ( 2, 2 ),
 ( 0.000000000000000000, 1.000000000000000000 ),
 ( 0.000000000000000000, 1.000000000000000000 ),
 .UNSPECIFIED. ) 
 GEOMETRIC_REPRESENTATION_ITEM ( )  RATIONAL_B_SPLINE_SURFACE ( (
 ( 1.000000000000000000, 1.000000000000000000),
 ( 0.9932032654565553509, 0.8386279382598740284),
 ( 0.9932032654565553509, 0.8386279382598740284),
 ( 1.000000000000000000, 1.000000000000000000) ) ) 
 REPRESENTATION_ITEM ( '' )  SURFACE ( )  );
#23103 = ORIENTED_EDGE ( 'NONE', *, *, #53839, .F. ) ;
#23104 = CARTESIAN_POINT ( 'NONE',  ( 1.937114397841932290, -1.334979369128338922, -12.76557247858999844 ) ) ;
#23105 = CARTESIAN_POINT ( 'NONE',  ( -35.00000000000000000, 4.725891942574755866, 10.75351884295729477 ) ) ;
#23106 = LINE ( 'NONE', #13761, #30750 ) ;
#23107 = ORIENTED_EDGE ( 'NONE', *, *, #38757, .T. ) ;
#23108 = CARTESIAN_POINT ( 'NONE',  ( 0.2958664285830421292, 2.345117904768619699, 12.02992237133198472 ) ) ;
#23109 = DIRECTION ( 'NONE',  ( 0.000000000000000000, 0.01356324068817991828, -0.9999080150203990547 ) ) ;
#23110 = ORIENTED_EDGE ( 'NONE', *, *, #48806, .T. ) ;
#23111 = ORIENTED_EDGE ( 'NONE', *, *, #65051, .F. ) ;
#23112 = CARTESIAN_POINT ( 'NONE',  ( 2.889800649504073782, 3.002151847318991429, -5.334644486274164876 ) ) ;
#23113 = ADVANCED_FACE ( 'NONE', ( #57579 ), #6706, .T. ) ;
#23114 = EDGE_LOOP ( 'NONE', ( #9316, #46498, #37679, #40366 ) ) ;
#23115 = CARTESIAN_POINT ( 'NONE',  ( -35.00000000000000000, 7.745827850123011338, 10.12742074351899291 ) ) ;
#23116 = CARTESIAN_POINT ( 'NONE',  ( 0.2650492594609225039, 6.218173512054911534, -10.54996119777439034 ) ) ;
#23117 = CARTESIAN_POINT ( 'NONE',  ( -10.00000000000000178, 0.000000000000000000, 0.000000000000000000 ) ) ;
#23118 = CARTESIAN_POINT ( 'NONE',  ( 35.00000000000000000, 11.71932350927024657, -3.511386971104992760 ) ) ;
#23119 = DIRECTION ( 'NONE',  ( 0.000000000000000000, -0.01356324068817999114, 0.9999080150203989437 ) ) ;
#23120 = CARTESIAN_POINT ( 'NONE',  ( 1.452237505248552996, -7.672309600508628868, -10.06489946308209760 ) ) ;
#23122 = ORIENTED_EDGE ( 'NONE', *, *, #41970, .F. ) ;
#23121 = DIRECTION ( 'NONE',  ( 1.000000000000000000, -0.000000000000000000, -0.000000000000000000 ) ) ;
#23123 = DIRECTION ( 'NONE',  ( -1.000000000000000000, 0.000000000000000000, 0.000000000000000000 ) ) ;
#23124 = EDGE_CURVE ( 'NONE', #20489, #65370, #11210, .T. ) ;
#23125 = EDGE_LOOP ( 'NONE', ( #8097, #1654 ) ) ;
#23126 = LINE ( 'NONE', #33436, #63554 ) ;
#23127 = ORIENTED_EDGE ( 'NONE', *, *, #44434, .T. ) ;
#23128 = ORIENTED_EDGE ( 'NONE', *, *, #59532, .T. ) ;
#23129 = SHAPE_DEFINITION_REPRESENTATION ( #64646, #25052 ) ;
#23130 = CARTESIAN_POINT ( 'NONE',  ( -16.31771647384731949, 8.296044977521708219, 10.65025654402225364 ) ) ;
#23131 = CARTESIAN_POINT ( 'NONE',  ( -7.278994278378053018, -27.16225867570152275, 15.27062364585564858 ) ) ;
#23132 = VECTOR ( 'NONE', #20922, 1000.000000000000000 ) ;
#23133 = CARTESIAN_POINT ( 'NONE',  ( -25.06408389988974150, 11.89233385548744693, 6.391198624005284934 ) ) ;
#23134 = CARTESIAN_POINT ( 'NONE',  ( 22.57855258442565116, 3.026812727784649493, 11.61199400236328749 ) ) ;
#23135 = CARTESIAN_POINT ( 'NONE',  ( -45.36026561873624274, -0.9018867892165756128, 12.73108497882287971 ) ) ;
#23136 = LINE ( 'NONE', #53414, #14985 ) ;
#23137 = ORIENTED_EDGE ( 'NONE', *, *, #33420, .F. ) ;
#23138 = AXIS2_PLACEMENT_3D ( 'NONE', #7878, #27817, #53435 ) ;
#23139 = CARTESIAN_POINT ( 'NONE',  ( -22.27722015946438816, 0.6262261846986705294, 3.628085906632207092 ) ) ;
#23140 = CARTESIAN_POINT ( 'NONE',  ( -22.65999102136915866, -4.450325798697170043, 1.886119913916104229 ) ) ;
#23141 = DIRECTION ( 'NONE',  ( 0.000000000000000000, -0.01356324068817998940, 0.9999080150203990547 ) ) ;
#23142 = VERTEX_POINT ( 'NONE', #26983 ) ;
#23143 = CARTESIAN_POINT ( 'NONE',  ( 2.000000000000001776, 1.754183803416544452, 6.711026108862249373 ) ) ;
#23144 = VECTOR ( 'NONE', #509, 1000.000000000000000 ) ;
#23145 = VERTEX_POINT ( 'NONE', #42236 ) ;
#23146 = DIRECTION ( 'NONE',  ( 1.000000000000000000, 0.000000000000000000, 0.000000000000000000 ) ) ;
#23147 = VECTOR ( 'NONE', #7436, 1000.000000000000000 ) ;
#23148 = CARTESIAN_POINT ( 'NONE',  ( 0.2833330754217426306, 0.2021515668287386658, -12.25052326018166227 ) ) ;
#23149 = LINE ( 'NONE', #59073, #10801 ) ;
#23150 = CARTESIAN_POINT ( 'NONE',  ( 0.000000000000000000, 5.450255447309745982, 4.087611905901426645 ) ) ;
#23151 = DIRECTION ( 'NONE',  ( -1.000000000000000000, 0.000000000000000000, 0.000000000000000000 ) ) ;
#23152 = CARTESIAN_POINT ( 'NONE',  ( -27.10128162969864007, -1.945744751331068167, 1.304299867635182242 ) ) ;
#23153 = VECTOR ( 'NONE', #61083, 1000.000000000000000 ) ;
#23154 = DIRECTION ( 'NONE',  ( -1.000000000000000000, 0.000000000000000000, 0.000000000000000000 ) ) ;
#23155 = ORIENTED_EDGE ( 'NONE', *, *, #8866, .F. ) ;
#23156 = CARTESIAN_POINT ( 'NONE',  ( -35.00000000000000000, -12.18632975068352842, -0.06441628369849203284 ) ) ;
#23157 = EDGE_LOOP ( 'NONE', ( #20802, #7332, #327, #25116 ) ) ;
#23158 = DIRECTION ( 'NONE',  ( 0.000000000000000000, 0.1081190184239352453, 0.9941379571543603744 ) ) ;
#23159 = EDGE_CURVE ( 'NONE', #27199, #56769, #55300, .T. ) ;
#23160 = FILL_AREA_STYLE ('',( #9163 ) ) ;
#23161 = CARTESIAN_POINT ( 'NONE',  ( 35.00000000000000000, -0.06441628369827803735, 12.18632975068352309 ) ) ;
#23162 = ADVANCED_FACE ( 'NONE', ( #41931 ), #62216, .T. ) ;
#23163 = CARTESIAN_POINT ( 'NONE',  ( 2.665405856346782620, -1.089747929268628068, -9.505137710817304963 ) ) ;
#23164 = CARTESIAN_POINT ( 'NONE',  ( 47.00000000000000711, 4.705694406421931860E-17, -3.469127814946512892E-15 ) ) ;
#23165 = ORIENTED_EDGE ( 'NONE', *, *, #33733, .F. ) ;
#23166 = CARTESIAN_POINT ( 'NONE',  ( 2.000000000000001776, 6.812627895098307462, -0.04423456934727655609 ) ) ;
#23167 = CARTESIAN_POINT ( 'NONE',  ( 0.2638984909335716500, 11.57533005135184645, -4.001111175853627522 ) ) ;
#23168 = CARTESIAN_POINT ( 'NONE',  ( 2.259025283528085737, 1.461109758650560142, 7.499281868334248813 ) ) ;
#23169 = CARTESIAN_POINT ( 'NONE',  ( 35.00000000000000000, -8.854740511458901508, -7.717887834988215623 ) ) ;
#23170 = VERTEX_POINT ( 'NONE', #47278 ) ;
#23171 = CARTESIAN_POINT ( 'NONE',  ( 0.2767916011545390464, 12.09541651105896598, 1.940025653808885364 ) ) ;
#23172 = CARTESIAN_POINT ( 'NONE',  ( -22.29570301036918423, -2.586939527522297055, 2.696988360630612203 ) ) ;
#23173 = FACE_OUTER_BOUND ( 'NONE', #44092, .T. ) ;
#23175 = CARTESIAN_POINT ( 'NONE',  ( 37.00000000000000711, 11.73555825188276280, -4.983891302653623789 ) ) ;
#23174 = B_SPLINE_CURVE_WITH_KNOTS ( 'NONE', 3,
 ( #64360, #18823, #12835, #2568, #43412, #14139 ),
 .UNSPECIFIED., .F., .F.,
 ( 4, 2, 4 ),
 ( 0.000000000000000000, 0.0004528561986909391515, 0.0009057123973818783031 ),
 .UNSPECIFIED. ) ;
#23176 = CIRCLE ( 'NONE', #61417, 12.75000000000000178 ) ;
#23177 = ADVANCED_FACE ( 'NONE', ( #33607 ), #59528, .T. ) ;
#23178 = CARTESIAN_POINT ( 'NONE',  ( 2.269879328256734219, -0.1483462450596719218, -7.642470739868882035 ) ) ;
#23179 = CARTESIAN_POINT ( 'NONE',  ( -37.00000000000000711, 10.92721691015462149, -4.309077947445535628 ) ) ;
#23180 = AXIS2_PLACEMENT_3D ( 'NONE', #62833, #22952, #11638 ) ;
#23181 = VECTOR ( 'NONE', #60667, 1000.000000000000000 ) ;
#23182 = EDGE_CURVE ( 'NONE', #14607, #35879, #59212, .T. ) ;
#23183 = ORIENTED_EDGE ( 'NONE', *, *, #10293, .F. ) ;
#23184 = CARTESIAN_POINT ( 'NONE',  ( 5.514970785353741078, -0.003262412238248734667, -0.003415090918276127846 ) ) ;
#23185 = CARTESIAN_POINT ( 'NONE',  ( -12.85491158824215141, -29.00000000000000711, -3.284771503683518556 ) ) ;
#23186 = ORIENTED_EDGE ( 'NONE', *, *, #45109, .T. ) ;
#23187 = VECTOR ( 'NONE', #26414, 1000.000000000000000 ) ;
#23188 = EDGE_CURVE ( 'NONE', #12876, #10229, #42920, .T. ) ;
#23189 = LINE ( 'NONE', #48800, #6836 ) ;
#23190 = DIRECTION ( 'NONE',  ( 0.000000000000000000, 0.01356324068817992522, -0.9999080150203990547 ) ) ;
#23191 = DIRECTION ( 'NONE',  ( -0.000000000000000000, -0.000000000000000000, -1.000000000000000000 ) ) ;
#23192 = VECTOR ( 'NONE', #27479, 1000.000000000000000 ) ;
#23193 = CARTESIAN_POINT ( 'NONE',  ( 35.00000000000000000, 4.705694406421931860E-17, -3.469127814946512892E-15 ) ) ;
#23194 = CARTESIAN_POINT ( 'NONE',  ( 0.2911222467163567251, -11.58731125337563128, 3.989243506922300231 ) ) ;
#23196 = ORIENTED_EDGE ( 'NONE', *, *, #52870, .T. ) ;
#23195 = EDGE_CURVE ( 'NONE', #21663, #25020, #63199, .T. ) ;
#23197 = DIRECTION ( 'NONE',  ( 1.000000000000000000, -0.000000000000000000, 0.000000000000000000 ) ) ;
#23198 = ORIENTED_EDGE ( 'NONE', *, *, #43658, .T. ) ;
#23199 = CARTESIAN_POINT ( 'NONE',  ( 16.78263030916553333, -10.48479066935623827, 5.836879698929882565 ) ) ;
#23200 = CARTESIAN_POINT ( 'NONE',  ( 2.963017218115626239, 7.522800244854608742, -2.328652339224271728 ) ) ;
#23201 = DIRECTION ( 'NONE',  ( 0.000000000000000000, 0.000000000000000000, 1.000000000000000000 ) ) ;
#23202 = CARTESIAN_POINT ( 'NONE',  ( 0.5547464869798263143, 3.933612953276393931, -11.69908463509552199 ) ) ;
#23203 = DIRECTION ( 'NONE',  ( -0.3865475372811021937, 0.3335716741247191641, 0.8598319252293130655 ) ) ;
#23204 = EDGE_CURVE ( 'NONE', #57229, #62196, #12641, .T. ) ;
#23205 = B_SPLINE_CURVE_WITH_KNOTS ( 'NONE', 3,
 ( #59999, #14420, #34694, #54993, #4478, #45344, #40342, #40688, #1111, #56978, #15415, #15080, #5796, #10103, #21388, #55665, #26371, #56658, #41010, #26063, #31675, #16412 ),
 .UNSPECIFIED., .F., .F.,
 ( 4, 3, 3, 3, 3, 3, 3, 4 ),
 ( 1.167721476617577340E-18, 6.990956068646398400E-05, 0.0001398191187764044130, 0.0002097286751720215715, 0.0002796382307041361554, 0.0003495477861619811829, 0.0004194573423310285747, 0.0005586102576333138456 ),
 .UNSPECIFIED. ) ;
#23206 = CARTESIAN_POINT ( 'NONE',  ( 2.276905613633648073, -1.175741125184132319, 7.555317002492079936 ) ) ;
#23207 = CARTESIAN_POINT ( 'NONE',  ( 2.000000000000001776, -5.450255447309769963, 4.087611905901399112 ) ) ;
#23208 = EDGE_LOOP ( 'NONE', ( #41157, #39555, #35719, #23730 ) ) ;
#23209 = ORIENTED_EDGE ( 'NONE', *, *, #53098, .T. ) ;
#23210 = ORIENTED_EDGE ( 'NONE', *, *, #42387, .T. ) ;
#23211 = CARTESIAN_POINT ( 'NONE',  ( -22.28284753389937123, 2.590196335759734847, -2.640101649307530884 ) ) ;
#23212 = LINE ( 'NONE', #8247, #30033 ) ;
#23213 = VECTOR ( 'NONE', #16631, 1000.000000000000000 ) ;
#23214 = EDGE_CURVE ( 'NONE', #65319, #12565, #19723, .T. ) ;
#23215 = LINE ( 'NONE', #58824, #52140 ) ;
#23216 = VERTEX_POINT ( 'NONE', #23635 ) ;
#23217 = CARTESIAN_POINT ( 'NONE',  ( 0.3109076770649042976, 5.925244271826596076, -10.73466383006815406 ) ) ;
#23218 = CARTESIAN_POINT ( 'NONE',  ( 1.719304012340549859, -10.62216384465898500, -7.017415949616274240 ) ) ;
#23219 = AXIS2_PLACEMENT_3D ( 'NONE', #47764, #37112, #11844 ) ;
#23220 = DIRECTION ( 'NONE',  ( 0.000000000000000000, 0.8169148498130297531, -0.5767582926624941209 ) ) ;
#23221 = ORIENTED_EDGE ( 'NONE', *, *, #36269, .T. ) ;
#23222 = ORIENTED_EDGE ( 'NONE', *, *, #11874, .T. ) ;
#23223 = DIRECTION ( 'NONE',  ( -1.000000000000000000, -0.000000000000000000, -0.000000000000000000 ) ) ;
#23224 = ORIENTED_EDGE ( 'NONE', *, *, #45884, .T. ) ;
#23225 = CARTESIAN_POINT ( 'NONE',  ( -35.00000000000000000, 10.14433819232434253, 6.753013023069750709 ) ) ;
#23226 = ORIENTED_EDGE ( 'NONE', *, *, #47591, .F. ) ;
#23227 = ORIENTED_EDGE ( 'NONE', *, *, #65406, .F. ) ;
#23228 = CARTESIAN_POINT ( 'NONE',  ( 0.2655924914740778742, -6.161287456391609574, -10.58356227062115806 ) ) ;
#23230 = AXIS2_PLACEMENT_3D ( 'NONE', #53432, #32771, #23482 ) ;
#23229 = CARTESIAN_POINT ( 'NONE',  ( -27.08588607604449194, -1.616144682268085608, 1.631236259433588742 ) ) ;
#23231 = CARTESIAN_POINT ( 'NONE',  ( 0.2801149460245135336, 10.51028947658253010, -6.294737133725693212 ) ) ;
#23232 = CARTESIAN_POINT ( 'NONE',  ( 0.2833330754217422420, 8.029341648258490949, -9.254504746325713072 ) ) ;
#23233 = DIRECTION ( 'NONE',  ( -1.000000000000000000, 0.000000000000000000, 0.000000000000000000 ) ) ;
#23234 = CIRCLE ( 'NONE', #12621, 4.999999999999999112 ) ;
#23235 = AXIS2_PLACEMENT_3D ( 'NONE', #53242, #17339, #33612 ) ;
#23236 = ORIENTED_EDGE ( 'NONE', *, *, #27535, .F. ) ;
#23237 = CARTESIAN_POINT ( 'NONE',  ( 2.245754705088395031, -1.435454129948258606, 7.499730934370272273 ) ) ;
#23238 = CARTESIAN_POINT ( 'NONE',  ( -22.27721056931765631, 2.768264578996979974, -2.427163553894355452 ) ) ;
#23239 = CARTESIAN_POINT ( 'NONE',  ( 2.256373768223936871, 3.703993494727017666, -6.681391662622068850 ) ) ;
#23240 = CYLINDRICAL_SURFACE ( 'NONE', #58275, 4.999999999999999112 ) ;
#23241 = CARTESIAN_POINT ( 'NONE',  ( 27.85039655636127875, 11.11615754980423176, 4.533728555765254242 ) ) ;
#23242 = CARTESIAN_POINT ( 'NONE',  ( 1.462291587751302524, 0.6330131614661951289, -12.62932306616629141 ) ) ;
#23243 = CARTESIAN_POINT ( 'NONE',  ( 2.969415267404644343, -4.269695207293366046, -6.619534278261627769 ) ) ;
#23244 = CARTESIAN_POINT ( 'NONE',  ( 0.2915757698887299632, -11.58754481235184386, -3.989025639548751112 ) ) ;
#23245 = FACE_OUTER_BOUND ( 'NONE', #56508, .T. ) ;
#23246 = EDGE_CURVE ( 'NONE', #13659, #32821, #43562, .T. ) ;
#23247 = ORIENTED_EDGE ( 'NONE', *, *, #64470, .T. ) ;
#23248 = DIRECTION ( 'NONE',  ( 0.000000000000000000, 0.000000000000000000, 1.000000000000000000 ) ) ;
#23249 = ORIENTED_EDGE ( 'NONE', *, *, #56323, .T. ) ;
#23250 = CARTESIAN_POINT ( 'NONE',  ( 37.00000000000000711, -7.971186206369407223, 9.217970097227803805 ) ) ;
#23251 = CARTESIAN_POINT ( 'NONE',  ( 0.3278977287071231372, -0.2481246099268901439, 12.26453627383315670 ) ) ;
#23252 = CARTESIAN_POINT ( 'NONE',  ( 11.02943363989745684, -13.39302490721040151, -1.700353917502927859 ) ) ;
#23253 = CARTESIAN_POINT ( 'NONE',  ( -27.10719052120871098, -1.044362304621479165, 2.116547233941197703 ) ) ;
#23254 = CARTESIAN_POINT ( 'NONE',  ( 2.844750968615155085, 7.767336242080566500, 1.031816958530825001 ) ) ;
#23255 = ORIENTED_EDGE ( 'NONE', *, *, #54154, .T. ) ;
#23256 = CARTESIAN_POINT ( 'NONE',  ( 1.283627346226907218, 10.61381050043341112, -6.763590725840940010 ) ) ;
#23257 = CARTESIAN_POINT ( 'NONE',  ( -35.04582288351658548, -0.01270482153516100908, 0.0001464581944993508693 ) ) ;
#23258 = DIRECTION ( 'NONE',  ( 0.000000000000000000, -0.6745969609292717939, -0.7381862504171901040 ) ) ;
#23259 = CARTESIAN_POINT ( 'NONE',  ( -35.00000000000000000, 1.771820996347319710, -11.61175578952784448 ) ) ;
#23260 = B_SPLINE_CURVE_WITH_KNOTS ( 'NONE', 3,
 ( #17392, #48975, #37979, #58282, #7742, #57964, #37667, #22357, #42974, #3432, #27672, #43624, #12701, #33657, #53634, #32984, #52955, #12374, #38306, #47979, #32644, #53295 ),
 .UNSPECIFIED., .F., .F.,
 ( 4, 3, 3, 3, 3, 3, 3, 4 ),
 ( 0.000000000000000000, 4.447697177976369992E-05, 6.624143997791436314E-05, 8.800576886944573996E-05, 0.0001097699864780930454, 0.0001315341395364416101, 0.0001760120188223352595, 0.0001867971373174796466 ),
 .UNSPECIFIED. ) ;
#23261 = CIRCLE ( 'NONE', #33883, 12.75000000000000178 ) ;
#23262 = EDGE_CURVE ( 'NONE', #48402, #51469, #37735, .T. ) ;
#23263 = CARTESIAN_POINT ( 'NONE',  ( -4.989057617119008192, -0.9162120371760335003, -13.46887357958837406 ) ) ;
#23264 = ORIENTED_EDGE ( 'NONE', *, *, #29345, .T. ) ;
#23265 = CIRCLE ( 'NONE', #3112, 5.000000000000000888 ) ;
#23266 = EDGE_CURVE ( 'NONE', #65690, #54019, #3792, .T. ) ;
#23267 = CARTESIAN_POINT ( 'NONE',  ( 2.430348790456971386, -0.1949172018038362320, -7.694949746373680455 ) ) ;
#23268 = EDGE_CURVE ( 'NONE', #55634, #47275, #18664, .T. ) ;
#23269 = CARTESIAN_POINT ( 'NONE',  ( -35.04643116707788408, 0.009112266603805360687, -0.008094444324502694799 ) ) ;
#23270 = CARTESIAN_POINT ( 'NONE',  ( 2.256373768223415510, -3.934258165100021909, -6.548448293197169257 ) ) ;
#23271 = EDGE_LOOP ( 'NONE', ( #22948, #30966, #16916, #10558 ) ) ;
#23272 = VERTEX_POINT ( 'NONE', #18969 ) ;
#23273 = LINE ( 'NONE', #53209, #63641 ) ;
#23274 = CIRCLE ( 'NONE', #33898, 5.000000000000001776 ) ;
#23275 = ORIENTED_EDGE ( 'NONE', *, *, #19749, .F. ) ;
#23276 = CYLINDRICAL_SURFACE ( 'NONE', #4326, 12.18649999999999878 ) ;
#23277 = CARTESIAN_POINT ( 'NONE',  ( 2.305787727787085295, 7.508843116234176662, -1.493241775258346227 ) ) ;
#23278 = CARTESIAN_POINT ( 'NONE',  ( -27.08430792439081003, -1.614882584889912431, -1.625846845508604144 ) ) ;
#23279 = DIRECTION ( 'NONE',  ( 1.000000000000000000, 0.000000000000000000, -0.000000000000000000 ) ) ;
#23280 = EDGE_CURVE ( 'NONE', #32989, #35536, #65351, .T. ) ;
#23281 = DIRECTION ( 'NONE',  ( 1.000000000000000000, 0.000000000000000000, 0.000000000000000000 ) ) ;
#23282 = VERTEX_POINT ( 'NONE', #28604 ) ;
#23283 = EDGE_CURVE ( 'NONE', #27444, #59695, #63225, .T. ) ;
#23284 = VERTEX_POINT ( 'NONE', #32923 ) ;
#23285 = AXIS2_PLACEMENT_3D ( 'NONE', #59720, #14148, #34440 ) ;
#23286 = ORIENTED_EDGE ( 'NONE', *, *, #1493, .F. ) ;
#23287 = DIRECTION ( 'NONE',  ( 1.000000000000000000, 0.000000000000000000, 0.000000000000000000 ) ) ;
#23288 = EDGE_CURVE ( 'NONE', #54975, #40566, #55829, .T. ) ;
#23289 = B_SPLINE_CURVE_WITH_KNOTS ( 'NONE', 3,
 ( #16813, #58051, #51759, #37090, #32427, #1212, #6202, #12466, #26464, #46750, #57390, #11817, #52417, #27130, #47427, #47739 ),
 .UNSPECIFIED., .F., .F.,
 ( 4, 2, 2, 2, 2, 2, 2, 4 ),
 ( 0.000000000000000000, 0.001204540821560086709, 0.002409081643120173418, 0.003613622464680259910, 0.004818163286240346836, 0.007227244929360519821, 0.008431785750920607614, 0.009636326572480693672 ),
 .UNSPECIFIED. ) ;
#23290 = DIRECTION ( 'NONE',  ( -1.000000000000000000, 0.000000000000000000, 0.000000000000000000 ) ) ;
#23291 = ORIENTED_EDGE ( 'NONE', *, *, #57289, .T. ) ;
#23292 = DIRECTION ( 'NONE',  ( -1.000000000000000000, 0.000000000000000000, 0.000000000000000000 ) ) ;
#23293 = EDGE_CURVE ( 'NONE', #54167, #64126, #27966, .T. ) ;
#23294 = CARTESIAN_POINT ( 'NONE',  ( -22.27706485742869091, -0.3729136217355977778, -3.662257305743823022 ) ) ;
#23295 = ORIENTED_EDGE ( 'NONE', *, *, #53276, .T. ) ;
#23296 =( BOUNDED_CURVE ( )  B_SPLINE_CURVE ( 3, ( #65510, #54600, #9024, #23680 ),
 .UNSPECIFIED., .F., .F. ) 
 B_SPLINE_CURVE_WITH_KNOTS ( ( 4, 4 ),
 ( 1.254278954140350288, 1.289274629942205985 ),
 .UNSPECIFIED. ) 
 CURVE ( )  GEOMETRIC_REPRESENTATION_ITEM ( )  RATIONAL_B_SPLINE_CURVE ( ( 1.000000000000000000, 0.9998979444935354177, 0.9998979444935354177, 1.000000000000000000 ) ) 
 REPRESENTATION_ITEM ( '' )  );
#23297 = CARTESIAN_POINT ( 'NONE',  ( 2.705197763288547552, 7.218866228162286625, 2.925192046931933465 ) ) ;
#23298 = FACE_OUTER_BOUND ( 'NONE', #34258, .T. ) ;
#23299 = CARTESIAN_POINT ( 'NONE',  ( -37.00000000000000711, 0.000000000000000000, 0.000000000000000000 ) ) ;
#23300 = VERTEX_POINT ( 'NONE', #43235 ) ;
#23302 = EDGE_CURVE ( 'NONE', #21425, #8645, #63513, .T. ) ;
#23301 = ORIENTED_EDGE ( 'NONE', *, *, #44113, .T. ) ;
#23303 = DIRECTION ( 'NONE',  ( 0.000000000000000000, -0.8009703041134103030, -0.5987040770935764256 ) ) ;
#23304 = ORIENTED_EDGE ( 'NONE', *, *, #44799, .F. ) ;
#23305 = CARTESIAN_POINT ( 'NONE',  ( -47.00000000000000711, 0.000000000000000000, 0.000000000000000000 ) ) ;
#23306 = ORIENTED_EDGE ( 'NONE', *, *, #42555, .F. ) ;
#23307 = CARTESIAN_POINT ( 'NONE',  ( 2.034671305879536263, 9.380408876024983300, -6.953089744305774644 ) ) ;
#23308 = DIRECTION ( 'NONE',  ( -1.000000000000000000, 0.000000000000000000, 0.000000000000000000 ) ) ;
#23309 = CARTESIAN_POINT ( 'NONE',  ( -2.311295102025900494, -30.63172828985306140, -15.19685615870497131 ) ) ;
#23311 = DIRECTION ( 'NONE',  ( -1.000000000000000000, 0.000000000000000000, -0.000000000000000000 ) ) ;
#23310 = AXIS2_PLACEMENT_3D ( 'NONE', #39770, #3888, #63712 ) ;
#23312 = CARTESIAN_POINT ( 'NONE',  ( 0.9232167919969107572, 11.56588005394304020, -4.649596781010288282 ) ) ;
#23313 = FACE_OUTER_BOUND ( 'NONE', #44160, .T. ) ;
#23314 = ORIENTED_EDGE ( 'NONE', *, *, #11714, .F. ) ;
#23315 = CARTESIAN_POINT ( 'NONE',  ( -37.00000000000000711, 10.28547182238008162, 5.672855678558722303 ) ) ;
#23316 = VERTEX_POINT ( 'NONE', #3035 ) ;
#23317 = AXIS2_PLACEMENT_3D ( 'NONE', #13016, #9011, #43259 ) ;
#23318 = LINE ( 'NONE', #33936, #32744 ) ;
#23319 = DIRECTION ( 'NONE',  ( -1.000000000000000000, 0.000000000000000000, 0.000000000000000000 ) ) ;
#23320 = ORIENTED_EDGE ( 'NONE', *, *, #61590, .F. ) ;
#23321 = CARTESIAN_POINT ( 'NONE',  ( 24.90079489126682688, 10.54408982692485530, -8.432554294912229409 ) ) ;
#23322 = CARTESIAN_POINT ( 'NONE',  ( 0.3654063281920707507, 12.04448018134539744, -2.391195511198528134 ) ) ;
#23323 = CARTESIAN_POINT ( 'NONE',  ( 0.3057689695767561444, -2.355923806019124100, -12.03117299329037415 ) ) ;
#23324 = VECTOR ( 'NONE', #34558, 1000.000000000000000 ) ;
#23325 = VERTEX_POINT ( 'NONE', #34248 ) ;
#23326 = EDGE_CURVE ( 'NONE', #35454, #61571, #46258, .T. ) ;
#23327 = ORIENTED_EDGE ( 'NONE', *, *, #42456, .F. ) ;
#23328 = CARTESIAN_POINT ( 'NONE',  ( 35.00000000000000000, 4.705694406421931860E-17, -3.469127814946512892E-15 ) ) ;
#23329 = CIRCLE ( 'NONE', #54131, 12.74999999999999822 ) ;
#23330 = ORIENTED_EDGE ( 'NONE', *, *, #20063, .T. ) ;
#23331 = CARTESIAN_POINT ( 'NONE',  ( -26.43107551473783090, -12.39219842031925012, 5.356174113667619530 ) ) ;
#23332 = DIRECTION ( 'NONE',  ( 0.000000000000000000, 0.8827602140260297769, -0.4698238015817396418 ) ) ;
#23333 = CARTESIAN_POINT ( 'NONE',  ( 35.00000000000000000, 4.705694406421931860E-17, -3.469127814946512892E-15 ) ) ;
#23334 = CARTESIAN_POINT ( 'NONE',  ( -3.456237872026009850, 8.328074767851541438, 8.678162217191049521 ) ) ;
#23335 = CARTESIAN_POINT ( 'NONE',  ( 37.00000000000000711, 11.53507381115583108, 2.216820770815121744 ) ) ;
#23336 = ORIENTED_EDGE ( 'NONE', *, *, #18100, .T. ) ;
#23337 = EDGE_CURVE ( 'NONE', #2788, #31673, #2750, .T. ) ;
#23338 = CIRCLE ( 'NONE', #52010, 5.000000000000000000 ) ;
#23339 = CARTESIAN_POINT ( 'NONE',  ( 0.2676618633000474867, -12.03196378632209118, -2.284744117040205413 ) ) ;
#23340 = EDGE_CURVE ( 'NONE', #57752, #52961, #64309, .T. ) ;
#23341 = CARTESIAN_POINT ( 'NONE',  ( 3.047904605210315587, -7.698174516567070746, -1.788881754552557046 ) ) ;
#23342 = CARTESIAN_POINT ( 'NONE',  ( 0.9232058338315048962, 4.617996777200729319, -11.58467545991549130 ) ) ;
#23343 = CARTESIAN_POINT ( 'NONE',  ( 5.515539859299206427, 0.005336559634876441617, -0.002856745161749584157 ) ) ;
#23344 = EDGE_CURVE ( 'NONE', #46695, #40629, #24322, .T. ) ;
#23345 = CARTESIAN_POINT ( 'NONE',  ( -19.69476066079020171, -4.201994156881551312, 25.00000000000000000 ) ) ;
#23346 = DIRECTION ( 'NONE',  ( 0.000000000000000000, 0.000000000000000000, 1.000000000000000000 ) ) ;
#23347 = DIRECTION ( 'NONE',  ( -1.000000000000000000, 0.000000000000000000, 0.000000000000000000 ) ) ;
#23348 = AXIS2_PLACEMENT_3D ( 'NONE', #64463, #64158, #49534 ) ;
#23349 = VERTEX_POINT ( 'NONE', #14600 ) ;
#23350 = CARTESIAN_POINT ( 'NONE',  ( 2.298277635560272536, -0.1650558796844638076, 7.651596582281741554 ) ) ;
#23351 = ORIENTED_EDGE ( 'NONE', *, *, #41718, .F. ) ;
#23352 = CYLINDRICAL_SURFACE ( 'NONE', #42701, 12.18649999999999878 ) ;
#23353 = CIRCLE ( 'NONE', #60518, 5.000000000000000888 ) ;
#23354 = CYLINDRICAL_SURFACE ( 'NONE', #22745, 12.18649999999999878 ) ;
#23355 = FACE_OUTER_BOUND ( 'NONE', #33478, .T. ) ;
#23356 = EDGE_LOOP ( 'NONE', ( #33241, #57932, #47937, #32363 ) ) ;
#23357 = DIRECTION ( 'NONE',  ( 1.000000000000000000, 0.000000000000000000, -0.000000000000000000 ) ) ;
#23358 = CARTESIAN_POINT ( 'NONE',  ( 35.00000000000000000, 12.16632754454236398, -0.7008968033239244555 ) ) ;
#23359 = ORIENTED_EDGE ( 'NONE', *, *, #30278, .T. ) ;
#23360 = ORIENTED_EDGE ( 'NONE', *, *, #55111, .F. ) ;
#23361 = ORIENTED_EDGE ( 'NONE', *, *, #30900, .T. ) ;
#23362 = CARTESIAN_POINT ( 'NONE',  ( 29.28325686113022641, -11.61404609382441855, 6.885459852046807327 ) ) ;
#23363 = EDGE_CURVE ( 'NONE', #33997, #32649, #48966, .T. ) ;
#23364 = AXIS2_PLACEMENT_3D ( 'NONE', #4901, #28845, #40445 ) ;
#23365 = CARTESIAN_POINT ( 'NONE',  ( -22.27706485742869091, -3.358064672837095976, -1.508175983031630585 ) ) ;
#23366 = ORIENTED_EDGE ( 'NONE', *, *, #48885, .T. ) ;
#23367 = EDGE_CURVE ( 'NONE', #25087, #15837, #26685, .T. ) ;
#23368 = CARTESIAN_POINT ( 'NONE',  ( -22.27721056931765631, -2.427163553894363890, -2.768264578996979974 ) ) ;
#23369 = CARTESIAN_POINT ( 'NONE',  ( 2.711717199018286450, 2.143848034498841315, 13.33439168509460337 ) ) ;
#23370 = AXIS2_PLACEMENT_3D ( 'NONE', #22802, #11488, #1856 ) ;
#23371 = CARTESIAN_POINT ( 'NONE',  ( 35.00000000000000000, -3.287724142101329683, 11.73463472867578972 ) ) ;
#23372 = DIRECTION ( 'NONE',  ( -0.000000000000000000, -0.000000000000000000, -1.000000000000000000 ) ) ;
#23373 = ORIENTED_EDGE ( 'NONE', *, *, #9452, .F. ) ;
#23374 = DIRECTION ( 'NONE',  ( 1.000000000000000000, 0.000000000000000000, 0.000000000000000000 ) ) ;
#23375 = DIRECTION ( 'NONE',  ( -1.000000000000000000, 0.000000000000000000, 0.000000000000000000 ) ) ;
#23376 = CYLINDRICAL_SURFACE ( 'NONE', #17533, 6.183183579532408380 ) ;
#23378 = VERTEX_POINT ( 'NONE', #65477 ) ;
#23377 = CYLINDRICAL_SURFACE ( 'NONE', #49999, 12.75000000000000178 ) ;
#23379 = EDGE_CURVE ( 'NONE', #57516, #13558, #60839, .T. ) ;
#23380 = CARTESIAN_POINT ( 'NONE',  ( 5.515188684475870851, 0.003154373509839861981, -0.004322737127823984143 ) ) ;
#23381 = ORIENTED_EDGE ( 'NONE', *, *, #9673, .T. ) ;
#23382 = CARTESIAN_POINT ( 'NONE',  ( 0.2648978790185610999, 9.295532325666560070, -7.972372351882934360 ) ) ;
#23383 = AXIS2_PLACEMENT_3D ( 'NONE', #42166, #56163, #61166 ) ;
#23384 = ORIENTED_EDGE ( 'NONE', *, *, #7908, .F. ) ;
#23385 = CARTESIAN_POINT ( 'NONE',  ( 21.47577844137839520, -11.77878740299461313, -2.329267728435745255 ) ) ;
#23386 = FACE_OUTER_BOUND ( 'NONE', #37016, .T. ) ;
#23387 = FACE_OUTER_BOUND ( 'NONE', #49942, .T. ) ;
#23388 = DIRECTION ( 'NONE',  ( 1.000000000000000000, 0.000000000000000000, 0.000000000000000000 ) ) ;
#23389 = B_SPLINE_CURVE_WITH_KNOTS ( 'NONE', 3,
 ( #51978, #40679, #51662, #15408, #26363, #55972, #10406, #25718, #46008, #466, #41004, #56292, #10739, #31028, #2770, #7379 ),
 .UNSPECIFIED., .F., .F.,
 ( 4, 3, 3, 3, 3, 4 ),
 ( 0.000000000000000000, 0.0002999043160757392380, 0.0005998071753051102163, 0.0008997092107374701732, 0.001204458948196132986, 0.001510329163477478658 ),
 .UNSPECIFIED. ) ;
#23390 = DIRECTION ( 'NONE',  ( 1.000000000000000000, 0.000000000000000000, 0.000000000000000000 ) ) ;
#23391 = CARTESIAN_POINT ( 'NONE',  ( -10.87317010465706346, -6.818838523886362246, -11.65834341784620065 ) ) ;
#23392 = DIRECTION ( 'NONE',  ( 0.000000000000000000, -0.2006870767258961963, 0.9796553971857727694 ) ) ;
#23393 = ORIENTED_EDGE ( 'NONE', *, *, #1736, .F. ) ;
#23394 = DIRECTION ( 'NONE',  ( -1.000000000000000000, 0.000000000000000000, 0.000000000000000000 ) ) ;
#23395 = ORIENTED_EDGE ( 'NONE', *, *, #10956, .F. ) ;
#23396 = ORIENTED_EDGE ( 'NONE', *, *, #21808, .F. ) ;
#23397 = CARTESIAN_POINT ( 'NONE',  ( 24.82652845881425208, 8.390869743685042792, -8.578654028722157321 ) ) ;
#23398 = CARTESIAN_POINT ( 'NONE',  ( 5.516018279890452902, -0.002527316374434348482, -0.006286471671801920590 ) ) ;
#23399 = CARTESIAN_POINT ( 'NONE',  ( 35.00000000000000000, -8.551552972817137999, -8.052525312709853722 ) ) ;
#23400 = CARTESIAN_POINT ( 'NONE',  ( 0.3109076770649005228, -10.49874397806409831, 6.333869442011739181 ) ) ;
#23401 = DIRECTION ( 'NONE',  ( 0.000000000000000000, 0.01356324068817991828, -0.9999080150203990547 ) ) ;
#23402 = DIRECTION ( 'NONE',  ( 0.000000000000000000, -0.9246979985058680906, -0.3807014730195321661 ) ) ;
#23403 = CIRCLE ( 'NONE', #56332, 2.899999999999994582 ) ;
#23404 = EDGE_CURVE ( 'NONE', #22451, #34672, #25585, .T. ) ;
#23405 =( GEOMETRIC_REPRESENTATION_CONTEXT ( 3 ) GLOBAL_UNCERTAINTY_ASSIGNED_CONTEXT ( ( #62931 ) ) GLOBAL_UNIT_ASSIGNED_CONTEXT ( ( #53612, #46711, #21449 ) ) REPRESENTATION_CONTEXT ( 'NONE', 'WORKASPACE' ) );
#23406 = CIRCLE ( 'NONE', #49989, 6.000000000000000888 ) ;
#23407 = CARTESIAN_POINT ( 'NONE',  ( 1.014383007554949145, -11.03701226956412107, -5.859361736620448013 ) ) ;
#23408 = EDGE_CURVE ( 'NONE', #41367, #8147, #556, .T. ) ;
#23409 = VERTEX_POINT ( 'NONE', #58067 ) ;
#23410 = CARTESIAN_POINT ( 'NONE',  ( -37.00000000000000711, 0.000000000000000000, 0.000000000000000000 ) ) ;
#23411 = CARTESIAN_POINT ( 'NONE',  ( -27.08423923533013422, -1.376387618994799000, -1.832018136655361396 ) ) ;
#23412 = DIRECTION ( 'NONE',  ( -1.000000000000000000, 0.000000000000000000, -0.000000000000000000 ) ) ;
#23413 = EDGE_CURVE ( 'NONE', #33694, #37925, #35638, .T. ) ;
#23414 = DIRECTION ( 'NONE',  ( -1.000000000000000000, -0.000000000000000000, -0.000000000000000000 ) ) ;
#23415 = CARTESIAN_POINT ( 'NONE',  ( 1.719304012341629884, 8.755325027796281745, -9.242227816402079910 ) ) ;
#23416 = AXIS2_PLACEMENT_3D ( 'NONE', #10394, #6097, #26354 ) ;
#23417 = CARTESIAN_POINT ( 'NONE',  ( 33.02316666837520387, -2.861627175174544568, -23.69173491641420171 ) ) ;
#23418 = CARTESIAN_POINT ( 'NONE',  ( -10.74967964958609201, -6.109637884495152882, 12.04509226909001640 ) ) ;
#23420 = ORIENTED_EDGE ( 'NONE', *, *, #52586, .F. ) ;
#23419 = EDGE_CURVE ( 'NONE', #60081, #10789, #64273, .T. ) ;
#23421 = CARTESIAN_POINT ( 'NONE',  ( 0.2648978790185602672, -11.55204314799261311, -4.063980959785162383 ) ) ;
#23422 = DIRECTION ( 'NONE',  ( -1.000000000000000000, 0.000000000000000000, 0.000000000000000000 ) ) ;
#23423 = FACE_OUTER_BOUND ( 'NONE', #49061, .T. ) ;
#23424 = AXIS2_PLACEMENT_3D ( 'NONE', #62539, #37279, #47599 ) ;
#23425 = EDGE_CURVE ( 'NONE', #65358, #61028, #54747, .T. ) ;
#23426 = CARTESIAN_POINT ( 'NONE',  ( -27.20164183316781248, 0.1019800881472613385, 2.642567708136680960 ) ) ;
#23427 = DIRECTION ( 'NONE',  ( 0.000000000000000000, 0.000000000000000000, 1.000000000000000000 ) ) ;
#23428 = CIRCLE ( 'NONE', #25560, 5.000000000000000000 ) ;
#23429 = EDGE_LOOP ( 'NONE', ( #46509, #50555, #51267, #4094 ) ) ;
#23430 = CARTESIAN_POINT ( 'NONE',  ( 0.000000000000000000, 0.000000000000000000, 0.000000000000000000 ) ) ;
#23431 = CARTESIAN_POINT ( 'NONE',  ( 0.2956976708475470561, 9.245952174682551927, 8.045468685196958347 ) ) ;
#23432 = CARTESIAN_POINT ( 'NONE',  ( -22.27834755396593991, -2.756126180273653414, 2.447855249718975390 ) ) ;
#23433 = VERTEX_POINT ( 'NONE', #64658 ) ;
#23434 = CARTESIAN_POINT ( 'NONE',  ( 37.00000000000000711, 11.73463472867580393, 3.287724142101285274 ) ) ;
#23435 = VECTOR ( 'NONE', #52737, 1000.000000000000000 ) ;
#23436 = CARTESIAN_POINT ( 'NONE',  ( 0.2648978790185593790, -4.312320170909161199, -11.46165506714232762 ) ) ;
#23437 = ORIENTED_EDGE ( 'NONE', *, *, #44167, .F. ) ;
#23438 = ORIENTED_EDGE ( 'NONE', *, *, #33397, .T. ) ;
#23439 = EDGE_CURVE ( 'NONE', #55813, #50026, #26071, .T. ) ;
#23440 = CIRCLE ( 'NONE', #38340, 12.75000000000000178 ) ;
#23441 = AXIS2_PLACEMENT_3D ( 'NONE', #11956, #8289, #18281 ) ;
#23442 = VECTOR ( 'NONE', #15574, 1000.000000000000000 ) ;
#23443 = VERTEX_POINT ( 'NONE', #28443 ) ;
#23444 = EDGE_CURVE ( 'NONE', #8833, #15077, #38837, .T. ) ;
#23445 = CARTESIAN_POINT ( 'NONE',  ( 35.00000000000000000, 4.705694406421931860E-17, -3.469127814946512892E-15 ) ) ;
#23446 = DIRECTION ( 'NONE',  ( -1.000000000000000000, 0.000000000000000000, -0.000000000000000000 ) ) ;
#23447 = DIRECTION ( 'NONE',  ( 0.000000000000000000, 0.3807014730195220631, -0.9246979985058721985 ) ) ;
#23448 = CARTESIAN_POINT ( 'NONE',  ( 2.276905613633650738, -7.555317002492078160, -1.175741125184157410 ) ) ;
#23449 = CIRCLE ( 'NONE', #98, 12.75000000000000178 ) ;
#23450 = CARTESIAN_POINT ( 'NONE',  ( 1.459561108992493361, 12.08294179906902954, 3.725588117663684695 ) ) ;
#23452 = ORIENTED_EDGE ( 'NONE', *, *, #17613, .F. ) ;
#23451 = CARTESIAN_POINT ( 'NONE',  ( -37.00000000000000711, 0.000000000000000000, 0.000000000000000000 ) ) ;
#23453 = CARTESIAN_POINT ( 'NONE',  ( -22.27719412087655471, 2.283949229175435303, 2.887588494201198230 ) ) ;
#23454 = ORIENTED_EDGE ( 'NONE', *, *, #55642, .F. ) ;
#23455 = CARTESIAN_POINT ( 'NONE',  ( -22.66110217412718342, -4.900671186447923766, -0.6585288088160191622 ) ) ;
#23456 = EDGE_LOOP ( 'NONE', ( #48338, #38565, #13301, #5166 ) ) ;
#23457 = ORIENTED_EDGE ( 'NONE', *, *, #23124, .T. ) ;
#23458 = CARTESIAN_POINT ( 'NONE',  ( -25.37500095553464163, 11.65763308310754809, 6.809669256228112033 ) ) ;
#23459 = VECTOR ( 'NONE', #17901, 1000.000000000000000 ) ;
#23460 = CARTESIAN_POINT ( 'NONE',  ( -8.761386526127953545, -27.42676914488322026, 14.81571904625999103 ) ) ;
#23461 = CARTESIAN_POINT ( 'NONE',  ( -26.42332584564274711, 12.40027562897680369, 5.341196054782874292 ) ) ;
#23462 = AXIS2_PLACEMENT_3D ( 'NONE', #19318, #19654, #50242 ) ;
#23463 = CYLINDRICAL_SURFACE ( 'NONE', #45557, 2.899999999999994582 ) ;
#23464 = ADVANCED_FACE ( 'NONE', ( #59701 ), #19633, .F. ) ;
#23465 = DIRECTION ( 'NONE',  ( 0.000000000000000000, -0.8989688749565110104, -0.4380125133594070519 ) ) ;
#23466 = CARTESIAN_POINT ( 'NONE',  ( -27.08417568107323703, 0.8117865859100341641, -2.142502990753190506 ) ) ;
#23467 = EDGE_LOOP ( 'NONE', ( #31856, #24239, #6184, #8680 ) ) ;
#23468 = VECTOR ( 'NONE', #22197, 1000.000000000000000 ) ;
#23469 = DIRECTION ( 'NONE',  ( 0.000000000000000000, -1.000000000000000000, 0.000000000000000000 ) ) ;
#23470 = DIRECTION ( 'NONE',  ( 0.000000000000000000, 0.01356324068817992695, -0.9999080150203990547 ) ) ;
#23471 = DIRECTION ( 'NONE',  ( 0.000000000000000000, 0.000000000000000000, 1.000000000000000000 ) ) ;
#23472 = ORIENTED_EDGE ( 'NONE', *, *, #39535, .F. ) ;
#23473 = CIRCLE ( 'NONE', #31946, 12.00000000000000000 ) ;
#23474 = CARTESIAN_POINT ( 'NONE',  ( 0.000000000000000000, 6.796153407501448029, 1.388283512725836388 ) ) ;
#23475 = VERTEX_POINT ( 'NONE', #4170 ) ;
#23476 = CIRCLE ( 'NONE', #28785, 15.00000000000000000 ) ;
#23477 = CARTESIAN_POINT ( 'NONE',  ( 35.00000000000000000, -2.216820770815006725, 11.53507381115585417 ) ) ;
#23478 = CARTESIAN_POINT ( 'NONE',  ( 0.3002738374340842564, 0.2255758963753189406, -12.25576345519757027 ) ) ;
#23479 = DIRECTION ( 'NONE',  ( -1.000000000000000000, 0.000000000000000000, 0.000000000000000000 ) ) ;
#23480 = CARTESIAN_POINT ( 'NONE',  ( -22.28121537037577227, 3.028566507474732550, -2.114437713163330290 ) ) ;
#23481 = DIRECTION ( 'NONE',  ( -1.000000000000000000, 0.000000000000000000, -0.000000000000000000 ) ) ;
#23482 = DIRECTION ( 'NONE',  ( 0.000000000000000000, -0.8009703041134232926, -0.5987040770935588840 ) ) ;
#23483 = DIRECTION ( 'NONE',  ( 1.000000000000000000, 0.000000000000000000, 0.000000000000000000 ) ) ;
#23484 = CIRCLE ( 'NONE', #60635, 12.74999999999999822 ) ;
#23485 = EDGE_CURVE ( 'NONE', #21858, #34626, #60053, .T. ) ;
#23486 = VERTEX_POINT ( 'NONE', #3541 ) ;
#23487 = DIRECTION ( 'NONE',  ( 0.000000000000000000, 0.9346839223284527653, -0.3554799084909002205 ) ) ;
#23488 = ORIENTED_EDGE ( 'NONE', *, *, #8067, .T. ) ;
#23489 = CARTESIAN_POINT ( 'NONE',  ( 2.305787727787084407, -7.508843116234166004, 1.493241775258399073 ) ) ;
#23490 = SURFACE_STYLE_USAGE ( .BOTH. , #4188 ) ;
#23491 = CARTESIAN_POINT ( 'NONE',  ( 2.000000000000001776, -6.250523986464001425, 3.007653927006548766 ) ) ;
#23492 = AXIS2_PLACEMENT_3D ( 'NONE', #42810, #48804, #22200 ) ;
#23493 = AXIS2_PLACEMENT_3D ( 'NONE', #35986, #16043, #1764 ) ;
#23494 = DIRECTION ( 'NONE',  ( -1.000000000000000000, 0.000000000000000000, 0.000000000000000000 ) ) ;
#23495 = ADVANCED_FACE ( 'NONE', ( #4510 ), #43741, .T. ) ;
#23496 = VECTOR ( 'NONE', #27658, 1000.000000000000000 ) ;
#23497 = FACE_OUTER_BOUND ( 'NONE', #2355, .T. ) ;
#23498 =( BOUNDED_SURFACE ( )  B_SPLINE_SURFACE ( 3, 1, ( 
 ( #61523, #57216 ),
 ( #22275, #25979 ),
 ( #46262, #61864 ),
 ( #37583, #51257 ) ),
 .UNSPECIFIED., .F., .F., .F. ) 
 B_SPLINE_SURFACE_WITH_KNOTS ( ( 4, 4 ),
 ( 2, 2 ),
 ( 0.000000000000000000, 1.000000000000000000 ),
 ( 0.000000000000000000, 1.000000000000000000 ),
 .UNSPECIFIED. ) 
 GEOMETRIC_REPRESENTATION_ITEM ( )  RATIONAL_B_SPLINE_SURFACE ( (
 ( 1.000000000000000000, 1.000000000000000000),
 ( 0.6933888150995267674, 0.9895912004443193632),
 ( 0.6933888150995267674, 0.9895912004443193632),
 ( 1.000000000000000000, 1.000000000000000000) ) ) 
 REPRESENTATION_ITEM ( '' )  SURFACE ( )  );
#23499 = VERTEX_POINT ( 'NONE', #59367 ) ;
#23500 = CARTESIAN_POINT ( 'NONE',  ( 37.00000000000000711, -7.608228585767796481, -10.23119532541070420 ) ) ;
#23501 = DIRECTION ( 'NONE',  ( 0.000000000000000000, 0.000000000000000000, 1.000000000000000000 ) ) ;
#23502 = CARTESIAN_POINT ( 'NONE',  ( -27.09364415740217424, -2.088137158972232843, -1.009938549039995692 ) ) ;
#23503 = CARTESIAN_POINT ( 'NONE',  ( 2.430348790457581565, -5.095533593439965259, -5.769383131055120906 ) ) ;
#23504 = EDGE_CURVE ( 'NONE', #12570, #37018, #45188, .T. ) ;
#23505 = ORIENTED_EDGE ( 'NONE', *, *, #61763, .T. ) ;
#23506 = DIRECTION ( 'NONE',  ( -1.000000000000000000, 0.000000000000000000, 0.000000000000000000 ) ) ;
#23507 = DIRECTION ( 'NONE',  ( -1.000000000000000000, 0.000000000000000000, 0.000000000000000000 ) ) ;
#23508 = DIRECTION ( 'NONE',  ( -1.000000000000000000, 0.000000000000000000, 0.000000000000000000 ) ) ;
#23509 = CARTESIAN_POINT ( 'NONE',  ( -22.23402523511428086, -0.6266381416564568152, -3.496364702451518092 ) ) ;
#23510 = VECTOR ( 'NONE', #13164, 1000.000000000000000 ) ;
#23511 = ADVANCED_FACE ( 'NONE', ( #8171 ), #65331, .T. ) ;
#23512 = VECTOR ( 'NONE', #36337, 1000.000000000000227 ) ;
#23513 = AXIS2_PLACEMENT_3D ( 'NONE', #14249, #29530, #4283 ) ;
#23514 = CARTESIAN_POINT ( 'NONE',  ( 2.276905613633652958, -0.1540880535620453018, -7.644700064315453680 ) ) ;
#23515 = CARTESIAN_POINT ( 'NONE',  ( -28.19906601428456838, -11.19867358001292068, -4.323235035335756038 ) ) ;
#23516 = ORIENTED_EDGE ( 'NONE', *, *, #10306, .F. ) ;
#23517 = CARTESIAN_POINT ( 'NONE',  ( 2.241526690369557429, 7.634439869182790162, -0.01730530154279370444 ) ) ;
#23518 = CARTESIAN_POINT ( 'NONE',  ( 5.520433897694421610, -0.01491416502703864569, -0.002108682515300430542 ) ) ;
#23519 = CIRCLE ( 'NONE', #19298, 5.000000000000000000 ) ;
#23520 = CARTESIAN_POINT ( 'NONE',  ( -3.456075311296388453, -27.96820792850356341, -12.23233986317338129 ) ) ;
#23521 = ORIENTED_EDGE ( 'NONE', *, *, #7413, .T. ) ;
#23522 = CARTESIAN_POINT ( 'NONE',  ( 5.514624014163232779, -0.004137701579365772077, 0.0001700579043839103323 ) ) ;
#23523 = CYLINDRICAL_SURFACE ( 'NONE', #48013, 17.25474371510545879 ) ;
#23524 = CARTESIAN_POINT ( 'NONE',  ( -36.00000000000000711, -1.738225594539906771, -12.63095688309031139 ) ) ;
#23525 = AXIS2_PLACEMENT_3D ( 'NONE', #37118, #61403, #15843 ) ;
#23526 = B_SPLINE_CURVE_WITH_KNOTS ( 'NONE', 3,
 ( #6806, #47041, #41706, #1499, #37033, #27715, #62621, #27077, #27387, #47371, #12097, #22074, #47682, #21777, #2128, #32376 ),
 .UNSPECIFIED., .F., .F.,
 ( 4, 3, 3, 3, 3, 4 ),
 ( 0.000000000000000000, 0.0002176109881720229670, 0.0004352086762394590945, 0.0006528017811446854479, 0.0007615147961451684822, 0.0009453342004947398822 ),
 .UNSPECIFIED. ) ;
#23527 = CARTESIAN_POINT ( 'NONE',  ( 36.00000000000000711, -9.913596905230170009, -8.017674001891752056 ) ) ;
#23528 = CARTESIAN_POINT ( 'NONE',  ( 0.2706063244538047807, -11.56807224179756233, 4.023948952279222446 ) ) ;
#23529 = EDGE_CURVE ( 'NONE', #4710, #31308, #62189, .T. ) ;
#23530 = DIRECTION ( 'NONE',  ( -1.000000000000000000, 0.000000000000000000, 0.000000000000000000 ) ) ;
#23531 = ORIENTED_EDGE ( 'NONE', *, *, #473, .T. ) ;
#23532 = DIRECTION ( 'NONE',  ( 0.000000000000000000, 0.000000000000000000, 1.000000000000000000 ) ) ;
#23533 = CIRCLE ( 'NONE', #3386, 7.499999999999988454 ) ;
#23534 = CARTESIAN_POINT ( 'NONE',  ( 5.530133899448235191, -0.01589823604557753789, -0.001661287012794294493 ) ) ;
#23535 = CARTESIAN_POINT ( 'NONE',  ( 0.2915757698887291860, -9.524403232224818439, -7.711631695122943775 ) ) ;
#23536 = DIRECTION ( 'NONE',  ( -1.000000000000000000, -0.000000000000000000, -0.000000000000000000 ) ) ;
#23537 = DIRECTION ( 'NONE',  ( 0.000000000000000000, -0.9246979985058763063, -0.3807014730195120711 ) ) ;
#23538 = FACE_OUTER_BOUND ( 'NONE', #27045, .T. ) ;
#23539 = DIRECTION ( 'NONE',  ( -1.000000000000000000, -0.000000000000000000, 0.000000000000000000 ) ) ;
#23540 = CARTESIAN_POINT ( 'NONE',  ( 35.00000000000000000, 4.705694406421931860E-17, -3.469127814946512892E-15 ) ) ;
#23541 = AXIS2_PLACEMENT_3D ( 'NONE', #30580, #46878, #15617 ) ;
#23542 = ORIENTED_EDGE ( 'NONE', *, *, #18776, .F. ) ;
#23543 = VECTOR ( 'NONE', #56839, 1000.000000000000000 ) ;
#23544 = ORIENTED_EDGE ( 'NONE', *, *, #47699, .F. ) ;
#23545 = VERTEX_POINT ( 'NONE', #55024 ) ;
#23546 = DIRECTION ( 'NONE',  ( 1.000000000000000000, -0.000000000000000000, 0.000000000000000000 ) ) ;
#23547 = EDGE_CURVE ( 'NONE', #58033, #14694, #15423, .T. ) ;
#23549 = CARTESIAN_POINT ( 'NONE',  ( 3.459614771489464946, -11.09853614738469396, -7.685863346768205595 ) ) ;
#23548 = AXIS2_PLACEMENT_3D ( 'NONE', #20891, #26873, #21570 ) ;
#23550 = AXIS2_PLACEMENT_3D ( 'NONE', #17002, #37281, #12014 ) ;
#23551 = VECTOR ( 'NONE', #39362, 1000.000000000000114 ) ;
#23552 = LINE ( 'NONE', #7250, #40432 ) ;
#23553 = ORIENTED_EDGE ( 'NONE', *, *, #19244, .T. ) ;
#23554 = DIRECTION ( 'NONE',  ( 0.000000000000000000, -0.04924826701373154203, -0.9987865678893285137 ) ) ;
#23555 = CARTESIAN_POINT ( 'NONE',  ( 2.260457164927182738, 6.546788723198603499, -3.939659644572469865 ) ) ;
#23556 = CARTESIAN_POINT ( 'NONE',  ( 2.305787727787084851, -1.493241775258474124, 7.508843116234150905 ) ) ;
#23557 = VERTEX_POINT ( 'NONE', #18508 ) ;
#23558 = ORIENTED_EDGE ( 'NONE', *, *, #26804, .T. ) ;
#23559 = CARTESIAN_POINT ( 'NONE',  ( -37.00000000000000711, 0.000000000000000000, 0.000000000000000000 ) ) ;
#23560 = LINE ( 'NONE', #23225, #19556 ) ;
#23561 = VERTEX_POINT ( 'NONE', #59061 ) ;
#23562 = ORIENTED_EDGE ( 'NONE', *, *, #43943, .T. ) ;
#23563 = VECTOR ( 'NONE', #44202, 1000.000000000000114 ) ;
#23564 = DIRECTION ( 'NONE',  ( 0.000000000000000000, -0.6051742151937717917, 0.7960930657056387583 ) ) ;
#23565 = CARTESIAN_POINT ( 'NONE',  ( -35.00000000000000000, 10.59380114696480391, -7.094637218249239652 ) ) ;
#23566 = AXIS2_PLACEMENT_3D ( 'NONE', #36166, #46493, #56473 ) ;
#23567 = CARTESIAN_POINT ( 'NONE',  ( -27.10422407540562517, -2.346206748218703009, 0.1544383239736372149 ) ) ;
#23568 = CARTESIAN_POINT ( 'NONE',  ( 35.00000000000000000, 10.28547182238015978, 5.672855678558568648 ) ) ;
#23569 = DIRECTION ( 'NONE',  ( -1.000000000000000000, 0.000000000000000000, 0.000000000000000000 ) ) ;
#23570 = CARTESIAN_POINT ( 'NONE',  ( 1.719304012338199517, 0.000000000000000000, 0.000000000000000000 ) ) ;
#23571 = EDGE_CURVE ( 'NONE', #4661, #14900, #9456, .T. ) ;
#23572 = VERTEX_POINT ( 'NONE', #19797 ) ;
#23573 = LINE ( 'NONE', #8589, #50726 ) ;
#23574 = DIRECTION ( 'NONE',  ( 0.000000000000000000, 0.8515178078024886466, -0.5243256840888532722 ) ) ;
#23575 = AXIS2_PLACEMENT_3D ( 'NONE', #59872, #60179, #25588 ) ;
#23576 = EDGE_CURVE ( 'NONE', #2181, #58998, #13344, .T. ) ;
#23577 = CARTESIAN_POINT ( 'NONE',  ( 0.2651627923886310523, -0.08809136839524371598, 12.24583724871548540 ) ) ;
#23578 = CARTESIAN_POINT ( 'NONE',  ( 35.00000000000000000, -11.74614673114903596, -0.01609748574441245694 ) ) ;
#23579 = CIRCLE ( 'NONE', #57347, 12.75000000000000178 ) ;
#23580 = CARTESIAN_POINT ( 'NONE',  ( 28.16476997869163412, 10.96217668651337007, 4.899552670153406453 ) ) ;
#23581 = CARTESIAN_POINT ( 'NONE',  ( -35.00000000000000000, 11.60979404548639948, -3.704519465651187282 ) ) ;
#23582 = AXIS2_PLACEMENT_3D ( 'NONE', #53348, #17101, #7121 ) ;
#23583 = DIRECTION ( 'NONE',  ( 0.000000000000000000, 0.9651210252299785575, 0.2618041379715665973 ) ) ;
#23584 = CARTESIAN_POINT ( 'NONE',  ( 35.00000000000000000, 4.732539170486261604, -11.23004253107766282 ) ) ;
#23585 = CYLINDRICAL_SURFACE ( 'NONE', #28908, 4.999999999999999112 ) ;
#23586 = ORIENTED_EDGE ( 'NONE', *, *, #23280, .F. ) ;
#23587 = EDGE_CURVE ( 'NONE', #10033, #35942, #39612, .T. ) ;
#23588 = CARTESIAN_POINT ( 'NONE',  ( 0.3164563675027619039, 0.2404665832031381567, 12.26087493884171664 ) ) ;
#23589 = VECTOR ( 'NONE', #3809, 1000.000000000000114 ) ;
#23590 = ORIENTED_EDGE ( 'NONE', *, *, #37390, .T. ) ;
#23591 = DIRECTION ( 'NONE',  ( 0.000000000000000000, -0.9467777615094604693, -0.3218879778915875178 ) ) ;
#23592 = LINE ( 'NONE', #37569, #1146 ) ;
#23593 = DIRECTION ( 'NONE',  ( 0.000000000000000000, 0.9246979985058709772, 0.3807014730195252827 ) ) ;
#23594 = CARTESIAN_POINT ( 'NONE',  ( -10.61476244842199002, -9.390648123693877025, 9.710410838802262745 ) ) ;
#23595 = CARTESIAN_POINT ( 'NONE',  ( -35.00000000000000000, 11.66664283989679696, 5.143145423404321903 ) ) ;
#23596 = EDGE_CURVE ( 'NONE', #10568, #12727, #57936, .T. ) ;
#23597 = EDGE_LOOP ( 'NONE', ( #21218, #47341, #41597, #36958 ) ) ;
#23598 = CARTESIAN_POINT ( 'NONE',  ( -27.45775109278351067, 8.499184579339635448, -8.471355351200609007 ) ) ;
#23599 = CARTESIAN_POINT ( 'NONE',  ( 2.269879328256729334, -3.692763753156697248, 6.692746930935561167 ) ) ;
#23600 = VECTOR ( 'NONE', #22133, 1000.000000000000000 ) ;
#23601 = CARTESIAN_POINT ( 'NONE',  ( -35.00000000000000000, 0.000000000000000000, 0.000000000000000000 ) ) ;
#23602 = DIRECTION ( 'NONE',  ( -1.000000000000000000, 0.000000000000000000, 0.000000000000000000 ) ) ;
#23603 = AXIS2_PLACEMENT_3D ( 'NONE', #1546, #22799, #21821 ) ;
#23604 = VECTOR ( 'NONE', #53845, 1000.000000000000000 ) ;
#23605 = ADVANCED_FACE ( 'NONE', ( #54397 ), #813, .F. ) ;
#23606 = DIRECTION ( 'NONE',  ( 0.000000000000000000, 0.04924826701374583615, 0.9987865678893277366 ) ) ;
#23607 = EDGE_LOOP ( 'NONE', ( #17435, #24856, #38991, #15564 ) ) ;
#23608 = DIRECTION ( 'NONE',  ( -1.000000000000000000, 0.000000000000000000, 0.000000000000000000 ) ) ;
#23609 = CARTESIAN_POINT ( 'NONE',  ( 0.5547464869798240938, -8.164898018378748290, -9.256151063740635010 ) ) ;
#23610 = CARTESIAN_POINT ( 'NONE',  ( 47.00000000000000711, 4.705694406421931860E-17, -3.469127814946512892E-15 ) ) ;
#23611 = CIRCLE ( 'NONE', #32073, 12.74999999999999822 ) ;
#23612 = ORIENTED_EDGE ( 'NONE', *, *, #57402, .F. ) ;
#23613 = VERTEX_POINT ( 'NONE', #56010 ) ;
#23614 = CARTESIAN_POINT ( 'NONE',  ( -9.765880726038068005, 12.49572852913685139, -5.113274341876826057 ) ) ;
#23615 = ORIENTED_EDGE ( 'NONE', *, *, #28956, .T. ) ;
#23616 = CARTESIAN_POINT ( 'NONE',  ( 2.269879328256532158, 5.026125315665035842, 5.759117113708084545 ) ) ;
#23617 = CARTESIAN_POINT ( 'NONE',  ( 2.241526690369557429, -5.859443871527007630, -4.894066724724313033 ) ) ;
#23618 = DIRECTION ( 'NONE',  ( 1.000000000000000000, 0.000000000000000000, 0.000000000000000000 ) ) ;
#23619 = CARTESIAN_POINT ( 'NONE',  ( 5.530133899448235191, 0.004396748047611614973, -0.01536822665454942727 ) ) ;
#23620 = AXIS2_PLACEMENT_3D ( 'NONE', #2300, #23223, #23894 ) ;
#23621 = CARTESIAN_POINT ( 'NONE',  ( 0.3665391374699465965, -9.576575648338966573, -7.691255657244391308 ) ) ;
#23622 = ORIENTED_EDGE ( 'NONE', *, *, #43573, .T. ) ;
#23623 = ORIENTED_EDGE ( 'NONE', *, *, #57949, .F. ) ;
#23624 = ORIENTED_EDGE ( 'NONE', *, *, #38187, .T. ) ;
#23625 = CARTESIAN_POINT ( 'NONE',  ( -35.00000000000000000, -6.415447294506628317, -11.01837265713079894 ) ) ;
#23626 = ADVANCED_FACE ( 'NONE', ( #60677 ), #51704, .T. ) ;
#23627 = CARTESIAN_POINT ( 'NONE',  ( -35.00000000000000000, -12.16893194857547478, -3.805206332242601963 ) ) ;
#23628 = ORIENTED_EDGE ( 'NONE', *, *, #65601, .F. ) ;
#23629 = CARTESIAN_POINT ( 'NONE',  ( 35.00000000000000000, -0.8294751490778421443, 12.15823808070322976 ) ) ;
#23630 = CIRCLE ( 'NONE', #12986, 12.18649999999999878 ) ;
#23631 = CARTESIAN_POINT ( 'NONE',  ( -22.30986928587821794, -0.2539257557460598003, -3.771068405887407771 ) ) ;
#23632 = ORIENTED_EDGE ( 'NONE', *, *, #26352, .T. ) ;
#23633 = CARTESIAN_POINT ( 'NONE',  ( 35.00000000000000000, 4.705694406421931860E-17, -3.469127814946512892E-15 ) ) ;
#23634 = DIRECTION ( 'NONE',  ( 0.000000000000000000, 0.000000000000000000, -1.000000000000000000 ) ) ;
#23635 = CARTESIAN_POINT ( 'NONE',  ( -35.00000000000000000, 12.54989509947650994, 2.250029553613800637 ) ) ;
#23636 = ORIENTED_EDGE ( 'NONE', *, *, #379, .F. ) ;
#23637 = VERTEX_POINT ( 'NONE', #11128 ) ;
#23638 = CARTESIAN_POINT ( 'NONE',  ( -17.96927786591848886, -9.630624776632364714, 7.160636282608096259 ) ) ;
#23639 = UNCERTAINTY_MEASURE_WITH_UNIT (LENGTH_MEASURE( 1.000000000000000082E-05 ), #53809, 'distance_accuracy_value', 'NONE');
#23640 = ORIENTED_EDGE ( 'NONE', *, *, #8257, .F. ) ;
#23641 = DIRECTION ( 'NONE',  ( 1.000000000000000000, 0.000000000000000000, -0.000000000000000000 ) ) ;
#23642 = ORIENTED_EDGE ( 'NONE', *, *, #43914, .F. ) ;
#23643 = CIRCLE ( 'NONE', #22600, 5.000000000000001776 ) ;
#23644 = VERTEX_POINT ( 'NONE', #163 ) ;
#23645 = CARTESIAN_POINT ( 'NONE',  ( 0.2648978790185602672, -4.063980959785125080, 11.55204314799262555 ) ) ;
#23646 = CARTESIAN_POINT ( 'NONE',  ( 0.2651627923886321070, 11.47719387551886427, 4.271101819784393072 ) ) ;
#23647 = LINE ( 'NONE', #49579, #35790 ) ;
#23648 = CIRCLE ( 'NONE', #25719, 7.499999999999988454 ) ;
#23650 = CIRCLE ( 'NONE', #51276, 7.499999999999988454 ) ;
#23649 = DIRECTION ( 'NONE',  ( -1.000000000000000000, 0.000000000000000000, 0.000000000000000000 ) ) ;
#23651 = ADVANCED_FACE ( 'NONE', ( #25762 ), #15111, .T. ) ;
#23652 = CARTESIAN_POINT ( 'NONE',  ( 1.372161826077490154, 11.63973780005268388, -4.864129100817252471 ) ) ;
#23653 = CARTESIAN_POINT ( 'NONE',  ( 37.00000000000000711, 5.015831474386306610, -10.62137734850269943 ) ) ;
#23654 = ORIENTED_EDGE ( 'NONE', *, *, #21555, .T. ) ;
#23655 = DIRECTION ( 'NONE',  ( 1.000000000000000000, 0.000000000000000000, 0.000000000000000000 ) ) ;
#23656 = ORIENTED_EDGE ( 'NONE', *, *, #36566, .T. ) ;
#23657 = CARTESIAN_POINT ( 'NONE',  ( 2.305787727787083519, -2.774453000917197265, 7.135468203929974607 ) ) ;
#23658 = EDGE_CURVE ( 'NONE', #11179, #13729, #18807, .T. ) ;
#23659 = LINE ( 'NONE', #18685, #64873 ) ;
#23660 = EDGE_CURVE ( 'NONE', #3297, #21470, #13380, .T. ) ;
#23661 = ORIENTED_EDGE ( 'NONE', *, *, #45275, .T. ) ;
#23662 = CARTESIAN_POINT ( 'NONE',  ( 0.000000000000000000, 0.000000000000000000, 0.000000000000000000 ) ) ;
#23663 = CARTESIAN_POINT ( 'NONE',  ( 0.2676618633000464320, 4.037335446657237092, 11.56235835488941355 ) ) ;
#23664 = CARTESIAN_POINT ( 'NONE',  ( 0.3654063281920748585, -2.391195511198570323, -12.04448018134538678 ) ) ;
#23665 = B_SPLINE_CURVE_WITH_KNOTS ( 'NONE', 3,
 ( #40056, #5163, #35718, #15451, #56343, #21088, #61653, #20114, #35396, #25113 ),
 .UNSPECIFIED., .F., .F.,
 ( 4, 3, 3, 4 ),
 ( 5.401523115762575937E-05, 0.0008136511341527827203, 0.004068255670953102761, 0.005063778443040927411 ),
 .UNSPECIFIED. ) ;
#23666 = ORIENTED_EDGE ( 'NONE', *, *, #9633, .T. ) ;
#23667 = CIRCLE ( 'NONE', #59773, 2.899999999999995026 ) ;
#23668 = ORIENTED_EDGE ( 'NONE', *, *, #42291, .T. ) ;
#23669 = ADVANCED_FACE ( 'NONE', ( #41701 ), #505, .T. ) ;
#23670 = CARTESIAN_POINT ( 'NONE',  ( 2.781367136452675304, -6.916275212954791307, -3.637318098960500290 ) ) ;
#23671 = CIRCLE ( 'NONE', #50200, 12.74999999999999822 ) ;
#23672 = ORIENTED_EDGE ( 'NONE', *, *, #51033, .T. ) ;
#23674 = ADVANCED_FACE ( 'NONE', ( #10785 ), #8082, .T. ) ;
#23673 = B_SPLINE_CURVE_WITH_KNOTS ( 'NONE', 3,
 ( #47752, #36787, #47113, #1565, #21839, #42086, #7173 ),
 .UNSPECIFIED., .F., .F.,
 ( 4, 3, 4 ),
 ( 0.000000000000000000, 0.001700533616330558370, 0.005002426799373359094 ),
 .UNSPECIFIED. ) ;
#23675 = CARTESIAN_POINT ( 'NONE',  ( -28.71060117729524919, 3.670315194194619490, 12.99175741217617563 ) ) ;
#23676 = CARTESIAN_POINT ( 'NONE',  ( 35.00000000000000000, -4.946702696913249042, -11.13736569743272753 ) ) ;
#23677 = VECTOR ( 'NONE', #28862, 1000.000000000000000 ) ;
#23678 = CARTESIAN_POINT ( 'NONE',  ( 35.00000000000000000, 4.705694406421931860E-17, -3.469127814946512892E-15 ) ) ;
#23679 = CARTESIAN_POINT ( 'NONE',  ( 12.52750123246316072, 0.4973700281276248192, 25.00000000000000000 ) ) ;
#23680 = CARTESIAN_POINT ( 'NONE',  ( -19.47984447937493613, -3.750539801530005768, -12.96855624952674724 ) ) ;
#23681 = VERTEX_POINT ( 'NONE', #31071 ) ;
#23682 = CARTESIAN_POINT ( 'NONE',  ( -30.18541646480305829, -1.811670027856088439, 13.38380110246788490 ) ) ;
#23683 = EDGE_CURVE ( 'NONE', #14200, #2755, #3756, .T. ) ;
#23684 = EDGE_CURVE ( 'NONE', #40131, #52526, #21775, .T. ) ;
#23685 = EDGE_CURVE ( 'NONE', #22527, #45722, #15446, .T. ) ;
#23686 = CARTESIAN_POINT ( 'NONE',  ( 2.655192694323995628, -2.733486750964454703, 9.204230091442163086 ) ) ;
#23687 = DIRECTION ( 'NONE',  ( 0.000000000000000000, -0.1118654143051685257, -0.9937233664769752339 ) ) ;
#23688 = CARTESIAN_POINT ( 'NONE',  ( 0.3665391374699467075, 9.576575648339128222, -7.691255657244196797 ) ) ;
#23689 = CARTESIAN_POINT ( 'NONE',  ( 2.000000000000001776, -6.883677378339447372, -0.8544109087186817497 ) ) ;
#23690 = CARTESIAN_POINT ( 'NONE',  ( -10.00000000000000178, 0.000000000000000000, 0.000000000000000000 ) ) ;
#23691 = AXIS2_PLACEMENT_3D ( 'NONE', #31532, #56840, #31220 ) ;
#23692 = CIRCLE ( 'NONE', #15164, 4.999999999999999112 ) ;
#23693 = AXIS2_PLACEMENT_3D ( 'NONE', #42442, #32153, #15869 ) ;
#23694 = CIRCLE ( 'NONE', #23751, 15.00000000000000000 ) ;
#23695 = ORIENTED_EDGE ( 'NONE', *, *, #34452, .T. ) ;
#23696 = LINE ( 'NONE', #2433, #44788 ) ;
#23697 =( BOUNDED_SURFACE ( )  B_SPLINE_SURFACE ( 3, 1, ( 
 ( #60878, #1017 ),
 ( #25966, #15951 ),
 ( #21282, #20950 ),
 ( #41560, #61851 ) ),
 .UNSPECIFIED., .F., .F., .F. ) 
 B_SPLINE_SURFACE_WITH_KNOTS ( ( 4, 4 ),
 ( 2, 2 ),
 ( 0.000000000000000000, 1.000000000000000000 ),
 ( 0.000000000000000000, 1.000000000000000000 ),
 .UNSPECIFIED. ) 
 GEOMETRIC_REPRESENTATION_ITEM ( )  RATIONAL_B_SPLINE_SURFACE ( (
 ( 1.000000000000000000, 1.000000000000000000),
 ( 0.8716676215708681896, 0.8964445200148164483),
 ( 0.8716676215708681896, 0.8964445200148164483),
 ( 1.000000000000000000, 1.000000000000000000) ) ) 
 REPRESENTATION_ITEM ( '' )  SURFACE ( )  );
#23698 = EDGE_LOOP ( 'NONE', ( #19118, #42731, #42184, #34642 ) ) ;
#23699 = CARTESIAN_POINT ( 'NONE',  ( 0.2648978790185602672, 1.996248716311790128, -12.08224454301446826 ) ) ;
#23700 = CARTESIAN_POINT ( 'NONE',  ( 0.000000000000000000, 0.000000000000000000, 0.000000000000000000 ) ) ;
#23701 = CARTESIAN_POINT ( 'NONE',  ( 0.2648978790185602672, 6.237101853238547378, 10.53870023327865901 ) ) ;
#23702 = CARTESIAN_POINT ( 'NONE',  ( -27.45775109278351067, 11.83395752356219077, -1.989333891161980894 ) ) ;
#23703 = ORIENTED_EDGE ( 'NONE', *, *, #39331, .F. ) ;
#23704 = AXIS2_PLACEMENT_3D ( 'NONE', #46563, #16959, #45919 ) ;
#23705 = ORIENTED_EDGE ( 'NONE', *, *, #2124, .T. ) ;
#23706 = ORIENTED_EDGE ( 'NONE', *, *, #40490, .T. ) ;
#23707 = CARTESIAN_POINT ( 'NONE',  ( 29.34908395106651469, -11.50269583891679659, 7.070024793111046257 ) ) ;
#23708 = CIRCLE ( 'NONE', #62987, 2.899999999999994582 ) ;
#23710 = ADVANCED_FACE ( 'NONE', ( #25107 ), #64641, .F. ) ;
#23709 = DIRECTION ( 'NONE',  ( -1.000000000000000000, 0.000000000000000000, -0.000000000000000000 ) ) ;
#23711 = EDGE_CURVE ( 'NONE', #52094, #44262, #44147, .T. ) ;
#23712 = ORIENTED_EDGE ( 'NONE', *, *, #45998, .T. ) ;
#23713 = CARTESIAN_POINT ( 'NONE',  ( -22.27711351828769892, -2.547249869018253676, -2.657880562424696613 ) ) ;
#23714 = B_SPLINE_CURVE_WITH_KNOTS ( 'NONE', 3,
 ( #37532, #16923, #26566, #52188, #52829, #32202, #36203, #51855, #52525, #46857, #1651, #26250, #10955, #1322, #46220, #62150, #57173, #661 ),
 .UNSPECIFIED., .F., .F.,
 ( 4, 2, 2, 2, 2, 2, 2, 2, 4 ),
 ( 7.770031522344853663E-18, 0.002493514729510051386, 0.003116893411887563473, 0.003740272094265075127, 0.004987029459020096700, 0.006233786823775119140, 0.007480544188530139846, 0.008727301553285160551, 0.009974058918040182992 ),
 .UNSPECIFIED. ) ;
#23715 = DIRECTION ( 'NONE',  ( -1.000000000000000000, 0.000000000000000000, 0.000000000000000000 ) ) ;
#23716 = CARTESIAN_POINT ( 'NONE',  ( 0.2869720083484361695, 10.50600528807146894, 6.306330337780551076 ) ) ;
#23717 = CARTESIAN_POINT ( 'NONE',  ( 17.54591139300511671, 9.528221380451970646, 7.352565480027280387 ) ) ;
#23718 = ORIENTED_EDGE ( 'NONE', *, *, #27254, .F. ) ;
#23719 = DIRECTION ( 'NONE',  ( 1.000000000000000000, 0.000000000000000000, -0.000000000000000000 ) ) ;
#23720 =( BOUNDED_SURFACE ( )  B_SPLINE_SURFACE ( 3, 1, ( 
 ( #47726, #42374 ),
 ( #22118, #52063 ),
 ( #57057, #6512 ),
 ( #41749, #11481 ) ),
 .UNSPECIFIED., .F., .F., .T. ) 
 B_SPLINE_SURFACE_WITH_KNOTS ( ( 4, 4 ),
 ( 2, 2 ),
 ( 0.000000000000000000, 1.000000000000000000 ),
 ( 0.000000000000000000, 1.000000000000000000 ),
 .UNSPECIFIED. ) 
 GEOMETRIC_REPRESENTATION_ITEM ( )  RATIONAL_B_SPLINE_SURFACE ( (
 ( 1.000000000000000000, 1.000000000000000000),
 ( 0.9856612449720755231, 0.9999558406602322425),
 ( 0.9856612449720755231, 0.9999558406602322425),
 ( 1.000000000000000000, 1.000000000000000000) ) ) 
 REPRESENTATION_ITEM ( '' )  SURFACE ( )  );
#23721 = CIRCLE ( 'NONE', #56615, 5.000000000000000000 ) ;
#23722 = CARTESIAN_POINT ( 'NONE',  ( 37.25000000000000711, -27.21021009056489603, 4.499999999999997335 ) ) ;
#23723 = CARTESIAN_POINT ( 'NONE',  ( -29.43980975494970309, -3.641506875706030488, -11.43413432115371364 ) ) ;
#23725 = ORIENTED_EDGE ( 'NONE', *, *, #30086, .T. ) ;
#23724 = FACE_OUTER_BOUND ( 'NONE', #17199, .T. ) ;
#23726 = CARTESIAN_POINT ( 'NONE',  ( -35.04683013664716640, 0.006266879427285388868, 0.01065093278704546884 ) ) ;
#23727 = ORIENTED_EDGE ( 'NONE', *, *, #41903, .T. ) ;
#23728 = DIRECTION ( 'NONE',  ( -1.000000000000000000, 0.000000000000000000, 0.000000000000000000 ) ) ;
#23729 = EDGE_CURVE ( 'NONE', #23832, #47920, #23071, .T. ) ;
#23730 = ORIENTED_EDGE ( 'NONE', *, *, #37449, .T. ) ;
#23731 = CARTESIAN_POINT ( 'NONE',  ( 21.74356534222384596, -11.95363809093303686, -1.123395297719272712 ) ) ;
#23732 = CARTESIAN_POINT ( 'NONE',  ( 0.2648978790185584908, -4.312320170909314854, 11.46165506714226900 ) ) ;
#23733 = DIRECTION ( 'NONE',  ( 0.000000000000000000, 0.3554799084908970563, 0.9346839223284539866 ) ) ;
#23734 = AXIS2_PLACEMENT_3D ( 'NONE', #10062, #5389, #30631 ) ;
#23735 = DIRECTION ( 'NONE',  ( 1.000000000000000000, 0.000000000000000000, 0.000000000000000000 ) ) ;
#23736 = EDGE_CURVE ( 'NONE', #47135, #58095, #42659, .T. ) ;
#23737 = DIRECTION ( 'NONE',  ( -1.000000000000000000, 0.000000000000000000, 0.000000000000000000 ) ) ;
#23738 = FACE_OUTER_BOUND ( 'NONE', #340, .T. ) ;
#23739 = EDGE_LOOP ( 'NONE', ( #56201, #53289, #41511, #59052 ) ) ;
#23740 = CARTESIAN_POINT ( 'NONE',  ( 5.520433897694421610, -0.0005131706886599361186, -0.01505375422439122687 ) ) ;
#23741 = ORIENTED_EDGE ( 'NONE', *, *, #19527, .T. ) ;
#23742 = EDGE_CURVE ( 'NONE', #30009, #50989, #50578, .T. ) ;
#23743 = CIRCLE ( 'NONE', #51373, 4.999999999999999112 ) ;
#23744 = ORIENTED_EDGE ( 'NONE', *, *, #53288, .F. ) ;
#23745 = FACE_OUTER_BOUND ( 'NONE', #19703, .T. ) ;
#23746 = CARTESIAN_POINT ( 'NONE',  ( 0.2638984909335720941, 12.09426044257624078, 1.930290337334096717 ) ) ;
#23747 = CARTESIAN_POINT ( 'NONE',  ( -27.20102706715913854, 2.512061365242613142, -0.8206313329275921609 ) ) ;
#23748 = CARTESIAN_POINT ( 'NONE',  ( -22.28350523959500862, 2.107889123925603680, 3.041489826385490591 ) ) ;
#23749 = CARTESIAN_POINT ( 'NONE',  ( -35.00000000000000000, -12.74921544981111055, 0.1414404973751688388 ) ) ;
#23750 = CARTESIAN_POINT ( 'NONE',  ( -7.181456785175555524, -8.540743096806455270, -10.45493698471458188 ) ) ;
#23751 = AXIS2_PLACEMENT_3D ( 'NONE', #2015, #17315, #57560 ) ;
#23752 = LINE ( 'NONE', #27728, #35498 ) ;
#23753 = ORIENTED_EDGE ( 'NONE', *, *, #25978, .F. ) ;
#23754 = EDGE_CURVE ( 'NONE', #15421, #43985, #11255, .T. ) ;
#23755 = CARTESIAN_POINT ( 'NONE',  ( 22.57855258442565116, 3.026812727784649493, 25.00000000000000000 ) ) ;
#23756 = CIRCLE ( 'NONE', #60902, 12.18650000000000055 ) ;
#23757 = CARTESIAN_POINT ( 'NONE',  ( 2.247206125382828823, -5.774712443419418584, -4.996658593545119764 ) ) ;
#23758 = DIRECTION ( 'NONE',  ( -1.000000000000000000, 0.000000000000000000, 0.000000000000000000 ) ) ;
#23759 = EDGE_CURVE ( 'NONE', #16732, #27686, #632, .T. ) ;
#23760 = AXIS2_PLACEMENT_3D ( 'NONE', #54834, #30210, #54517 ) ;
#23761 = ADVANCED_FACE ( 'NONE', ( #31707 ), #53622, .F. ) ;
#23762 = AXIS2_PLACEMENT_3D ( 'NONE', #21407, #25405, #25743 ) ;
#23763 = CARTESIAN_POINT ( 'NONE',  ( 2.305787727787084407, -1.164987321564783684, 7.566723232958066703 ) ) ;
#23764 = EDGE_CURVE ( 'NONE', #55569, #36553, #21894, .T. ) ;
#23765 = CARTESIAN_POINT ( 'NONE',  ( -10.33756816907811782, -3.910582247997075989, 12.92259563996709026 ) ) ;
#23766 = AXIS2_PLACEMENT_3D ( 'NONE', #50883, #51227, #35882 ) ;
#23767 = EDGE_CURVE ( 'NONE', #62086, #48650, #33574, .T. ) ;
#23768 = CARTESIAN_POINT ( 'NONE',  ( -9.037010005417281278, -3.102636015309993223, 13.14221497168421848 ) ) ;
#23769 = ORIENTED_EDGE ( 'NONE', *, *, #13216, .F. ) ;
#23770 = CARTESIAN_POINT ( 'NONE',  ( 1.000000000000000888, 2.473437528934141483, 7.080403010454977775 ) ) ;
#23771 = DIRECTION ( 'NONE',  ( -0.3939253465568944290, 0.4679616473074844074, 0.7910971609033218277 ) ) ;
#23772 = DIRECTION ( 'NONE',  ( 0.000000000000000000, 0.01356324068817998940, -0.9999080150203990547 ) ) ;
#23773 = AXIS2_PLACEMENT_3D ( 'NONE', #61809, #37183, #11918 ) ;
#23774 = CARTESIAN_POINT ( 'NONE',  ( -24.97643703457612929, 7.232049057323012065, 9.582644723418388466 ) ) ;
#23775 = CARTESIAN_POINT ( 'NONE',  ( 2.990245332647875287, -0.5125330575220037321, 8.465748356453847379 ) ) ;
#23776 = ORIENTED_EDGE ( 'NONE', *, *, #32758, .T. ) ;
#23777 = CYLINDRICAL_SURFACE ( 'NONE', #22595, 2.899999999999994582 ) ;
#23778 = DIRECTION ( 'NONE',  ( 0.000000000000000000, 0.01356324068817991481, -0.9999080150203990547 ) ) ;
#23779 = CARTESIAN_POINT ( 'NONE',  ( -22.27706485742869091, 2.154081322712221969, 2.985151051101477382 ) ) ;
#23780 = VERTEX_POINT ( 'NONE', #47035 ) ;
#23781 = CARTESIAN_POINT ( 'NONE',  ( 145.1370849898475797, 3.309064568108273190E-14, 0.000000000000000000 ) ) ;
#23782 = CARTESIAN_POINT ( 'NONE',  ( 2.000000000000001776, 0.000000000000000000, 0.000000000000000000 ) ) ;
#23783 = ORIENTED_EDGE ( 'NONE', *, *, #62463, .F. ) ;
#23784 = VECTOR ( 'NONE', #7158, 1000.000000000000000 ) ;
#23785 = AXIS2_PLACEMENT_3D ( 'NONE', #4960, #4644, #9260 ) ;
#23786 = ORIENTED_EDGE ( 'NONE', *, *, #20024, .F. ) ;
#23787 = DIRECTION ( 'NONE',  ( 0.000000000000000000, -0.01356324068818000328, 0.9999080150203990547 ) ) ;
#23788 = ADVANCED_FACE ( 'NONE', ( #21771 ), #7777, .T. ) ;
#23789 = ORIENTED_EDGE ( 'NONE', *, *, #31498, .T. ) ;
#23790 = CARTESIAN_POINT ( 'NONE',  ( 0.3675815128205912052, -12.04510820461657516, -2.391755495700727874 ) ) ;
#23791 = EDGE_CURVE ( 'NONE', #14430, #42534, #30377, .T. ) ;
#23792 = CARTESIAN_POINT ( 'NONE',  ( -35.00000000000000000, 12.31350058095527977, -3.307597835713114609 ) ) ;
#23793 = CARTESIAN_POINT ( 'NONE',  ( 0.3537226245948340009, -6.362463382302340875, 10.49813096858607686 ) ) ;
#23794 = LINE ( 'NONE', #44364, #59512 ) ;
#23795 = CIRCLE ( 'NONE', #19512, 5.000000000000000888 ) ;
#23796 = B_SPLINE_CURVE_WITH_KNOTS ( 'NONE', 3,
 ( #9960, #45869, #45520, #30553, #30879, #45209, #50857, #56155, #15272, #51198, #40538, #55846, #50212, #36190, #10274, #5305, #25574, #5983, #24935 ),
 .UNSPECIFIED., .F., .F.,
 ( 4, 3, 3, 3, 3, 3, 4 ),
 ( 0.000000000000000000, 2.836829843012877734E-05, 4.224792512550914851E-05, 5.612066614913206291E-05, 6.998859278354786935E-05, 9.832141288087123897E-05, 0.0001178161482478541221 ),
 .UNSPECIFIED. ) ;
#23797 = AXIS2_PLACEMENT_3D ( 'NONE', #28469, #48776, #59727 ) ;
#23798 = DIRECTION ( 'NONE',  ( -1.000000000000000000, 0.000000000000000000, 0.000000000000000000 ) ) ;
#23800 = VERTEX_POINT ( 'NONE', #28063 ) ;
#23799 = DIRECTION ( 'NONE',  ( -1.000000000000000000, 0.000000000000000000, 0.000000000000000000 ) ) ;
#23801 = PRODUCT_DEFINITION_SHAPE ( 'NONE', 'NONE',  #64445 ) ;
#23802 = CARTESIAN_POINT ( 'NONE',  ( 35.00000000000000000, 4.705694406421931860E-17, -3.469127814946512892E-15 ) ) ;
#23803 = EDGE_LOOP ( 'NONE', ( #42168, #27464, #64969, #29049 ) ) ;
#23804 = CARTESIAN_POINT ( 'NONE',  ( -41.00000000000000711, -1.853910857666116187E-16, -1.500000000000000222 ) ) ;
#23805 = CIRCLE ( 'NONE', #29111, 5.000000000000000000 ) ;
#23806 = ORIENTED_EDGE ( 'NONE', *, *, #45390, .F. ) ;
#23807 = EDGE_CURVE ( 'NONE', #40945, #41782, #53750, .T. ) ;
#23808 = ORIENTED_EDGE ( 'NONE', *, *, #12796, .F. ) ;
#23809 = CARTESIAN_POINT ( 'NONE',  ( -17.98414573016741613, 7.072294406407991119, 11.50157350705893755 ) ) ;
#23810 = CARTESIAN_POINT ( 'NONE',  ( -8.639472567037733697, -29.08579227083833629, 11.67554154369881836 ) ) ;
#23811 = CIRCLE ( 'NONE', #14238, 3.000000000000000444 ) ;
#23812 = CARTESIAN_POINT ( 'NONE',  ( 2.000000000000001776, 0.000000000000000000, 0.000000000000000000 ) ) ;
#23813 = CARTESIAN_POINT ( 'NONE',  ( 0.000000000000000000, -2.480520636974139936, -6.345145617221269241 ) ) ;
#23814 = CARTESIAN_POINT ( 'NONE',  ( 35.00000000000000000, 4.705694406421931860E-17, -3.469127814946512892E-15 ) ) ;
#23815 = CARTESIAN_POINT ( 'NONE',  ( -35.00000000000000000, 11.66953048682404415, -3.511814412391998541 ) ) ;
#23816 = VERTEX_POINT ( 'NONE', #62617 ) ;
#23817 = DIRECTION ( 'NONE',  ( 1.000000000000000000, 0.000000000000000000, 0.000000000000000000 ) ) ;
#23818 = ORIENTED_EDGE ( 'NONE', *, *, #14342, .T. ) ;
#23819 = DIRECTION ( 'NONE',  ( 1.000000000000000000, 0.000000000000000000, 0.000000000000000000 ) ) ;
#23820 = DIRECTION ( 'NONE',  ( -1.000000000000000000, 0.000000000000000000, 0.000000000000000000 ) ) ;
#23821 = EDGE_CURVE ( 'NONE', #37036, #35685, #25115, .T. ) ;
#23822 = VERTEX_POINT ( 'NONE', #27382 ) ;
#23823 = CARTESIAN_POINT ( 'NONE',  ( 2.269879328256732443, -7.500604381673471543, 1.473193649116112391 ) ) ;
#23824 = FACE_OUTER_BOUND ( 'NONE', #49964, .T. ) ;
#23825 = CARTESIAN_POINT ( 'NONE',  ( 35.00000000000000000, 8.146229107149526527, 9.063649021438864750 ) ) ;
#23826 = EDGE_CURVE ( 'NONE', #4279, #33015, #18747, .T. ) ;
#23827 = CARTESIAN_POINT ( 'NONE',  ( -22.31213670151049300, 3.145266995071685834, -2.108126385153777704 ) ) ;
#23828 = DIRECTION ( 'NONE',  ( 0.000000000000000000, -0.01356324068817991828, 0.9999080150203990547 ) ) ;
#23829 = VECTOR ( 'NONE', #27314, 1000.000000000000000 ) ;
#23830 = CARTESIAN_POINT ( 'NONE',  ( -37.00000000000000711, 0.000000000000000000, 0.000000000000000000 ) ) ;
#23831 = VERTEX_POINT ( 'NONE', #48673 ) ;
#23832 = VERTEX_POINT ( 'NONE', #29664 ) ;
#23833 = CARTESIAN_POINT ( 'NONE',  ( -37.00000000000000711, 10.43555801961483098, -5.391785509270847321 ) ) ;
#23834 = AXIS2_PLACEMENT_3D ( 'NONE', #38742, #18794, #14431 ) ;
#23835 = CARTESIAN_POINT ( 'NONE',  ( 2.491965175174512659, 4.796682362486732742, -6.046355957631024403 ) ) ;
#23836 = AXIS2_PLACEMENT_3D ( 'NONE', #23862, #44122, #64389 ) ;
#23837 = DIRECTION ( 'NONE',  ( 0.000000000000000000, -0.01356324068817991828, 0.9999080150203990547 ) ) ;
#23838 = EDGE_CURVE ( 'NONE', #39026, #24684, #31423, .T. ) ;
#23839 = DIRECTION ( 'NONE',  ( -0.000000000000000000, -0.000000000000000000, -1.000000000000000000 ) ) ;
#23840 = CYLINDRICAL_SURFACE ( 'NONE', #43867, 6.936499999999988120 ) ;
#23841 = ADVANCED_FACE ( 'NONE', ( #13405 ), #43661, .T. ) ;
#23842 = VECTOR ( 'NONE', #64681, 1000.000000000000000 ) ;
#23843 = CARTESIAN_POINT ( 'NONE',  ( -9.860341104261298284, -4.079292048029911300, -11.29117792640004936 ) ) ;
#23844 = CARTESIAN_POINT ( 'NONE',  ( 2.241526690369557873, 5.837196604699912861, -4.920579984890902203 ) ) ;
#23845 = EDGE_CURVE ( 'NONE', #38680, #25311, #29126, .T. ) ;
#23846 = DIRECTION ( 'NONE',  ( -1.000000000000000000, -0.000000000000000000, 0.000000000000000000 ) ) ;
#23847 = DIRECTION ( 'NONE',  ( -1.000000000000000000, 0.000000000000000000, 0.000000000000000000 ) ) ;
#23848 = ORIENTED_EDGE ( 'NONE', *, *, #33750, .T. ) ;
#23849 = VECTOR ( 'NONE', #40659, 1000.000000000000000 ) ;
#23850 = CARTESIAN_POINT ( 'NONE',  ( 3.459614771489464946, -11.09853614738469396, 25.00000000000000000 ) ) ;
#23851 = DIRECTION ( 'NONE',  ( -1.000000000000000000, 0.000000000000000000, 0.000000000000000000 ) ) ;
#23852 = CARTESIAN_POINT ( 'NONE',  ( 3.152665057734128862, 5.761241965769081652, 5.461013642405580626 ) ) ;
#23853 = AXIS2_PLACEMENT_3D ( 'NONE', #54785, #64095, #9202 ) ;
#23854 = CARTESIAN_POINT ( 'NONE',  ( -27.08429572838383947, 1.338867938658203860, 1.859677275556406384 ) ) ;
#23855 = CARTESIAN_POINT ( 'NONE',  ( 1.633930747253003135, -5.012862767614699067, -11.67150509329692376 ) ) ;
#23856 = ORIENTED_EDGE ( 'NONE', *, *, #56796, .T. ) ;
#23857 = CARTESIAN_POINT ( 'NONE',  ( 0.2646305136544072623, -7.972778379581612285, 9.296005949277201807 ) ) ;
#23859 = AXIS2_PLACEMENT_3D ( 'NONE', #40721, #55357, #50709 ) ;
#23858 = CARTESIAN_POINT ( 'NONE',  ( 29.60251855095053486, 10.89349753539994836, 7.986429861213258263 ) ) ;
#23860 = CARTESIAN_POINT ( 'NONE',  ( -8.269707202464745777, -26.46746146559253532, -14.47885724100708416 ) ) ;
#23861 = ORIENTED_EDGE ( 'NONE', *, *, #58536, .F. ) ;
#23862 = CARTESIAN_POINT ( 'NONE',  ( -10.00000000000000178, 0.000000000000000000, 0.000000000000000000 ) ) ;
#23863 = DIRECTION ( 'NONE',  ( 0.000000000000000000, 0.01356324068817998940, -0.9999080150203990547 ) ) ;
#23864 = CARTESIAN_POINT ( 'NONE',  ( 18.84867683979356201, -5.944105725974474730, 12.12095735156416509 ) ) ;
#23866 = CARTESIAN_POINT ( 'NONE',  ( 0.3537226245948352776, -8.088784578751358367, 9.233810598191753982 ) ) ;
#23865 = B_SPLINE_CURVE_WITH_KNOTS ( 'NONE', 3,
 ( #42784, #37141, #37479, #33141, #53448, #6585, #48136, #17541, #43111, #1269, #42439, #36826, #7893, #26851, #57123, #58431, #21547, #16558, #47791 ),
 .UNSPECIFIED., .F., .F.,
 ( 4, 3, 3, 3, 3, 3, 4 ),
 ( 0.000000000000000000, 2.831840207499449323E-05, 4.217266859840357231E-05, 5.602024318395839903E-05, 6.290810167969001913E-05, 9.120440630944526609E-05, 0.0001153103026479762659 ),
 .UNSPECIFIED. ) ;
#23867 = CARTESIAN_POINT ( 'NONE',  ( 0.3654063281920737483, -11.44627072062582052, 4.446369912832466298 ) ) ;
#23868 = VECTOR ( 'NONE', #63787, 1000.000000000000000 ) ;
#23869 = DIRECTION ( 'NONE',  ( 0.000000000000000000, -0.9796553971857722143, -0.2006870767258996102 ) ) ;
#23870 = EDGE_LOOP ( 'NONE', ( #12111, #30742, #14681, #59341 ) ) ;
#23871 = CARTESIAN_POINT ( 'NONE',  ( 41.00000000000000711, -1.694065894508600678E-18, 0.000000000000000000 ) ) ;
#23872 = EDGE_CURVE ( 'NONE', #60517, #56420, #51620, .T. ) ;
#23873 = CARTESIAN_POINT ( 'NONE',  ( 17.27839441901508621, -10.52068335315807524, 5.771933972472480967 ) ) ;
#23874 = CARTESIAN_POINT ( 'NONE',  ( 2.373367633546872302, 7.275198254387443164, -2.455525055524816480 ) ) ;
#23875 = CARTESIAN_POINT ( 'NONE',  ( 2.907497136251146141, -4.769582063554104856, 6.243048412629086386 ) ) ;
#23876 = CARTESIAN_POINT ( 'NONE',  ( 37.00000000000000711, -8.573591947375261313, 8.029056188533775895 ) ) ;
#23877 = DIRECTION ( 'NONE',  ( 1.000000000000000000, -0.000000000000000000, 0.000000000000000000 ) ) ;
#23878 = CARTESIAN_POINT ( 'NONE',  ( -29.95631573795198577, 0.8334892910201414651, -11.97922705870643334 ) ) ;
#23879 = CARTESIAN_POINT ( 'NONE',  ( 9.575800908719084958, 13.45729701195361372, -1.072919909436246266 ) ) ;
#23880 = ORIENTED_EDGE ( 'NONE', *, *, #61619, .T. ) ;
#23881 = VECTOR ( 'NONE', #16593, 1000.000000000000000 ) ;
#23882 = ORIENTED_EDGE ( 'NONE', *, *, #30315, .T. ) ;
#23883 = ORIENTED_EDGE ( 'NONE', *, *, #2071, .T. ) ;
#23884 = CARTESIAN_POINT ( 'NONE',  ( -22.29570301036918778, 2.586939527522315707, -2.696988360630598880 ) ) ;
#23885 = CARTESIAN_POINT ( 'NONE',  ( -36.00000000000000711, -12.66641127287624968, -1.457575200925676828 ) ) ;
#23886 = CARTESIAN_POINT ( 'NONE',  ( -22.29479313954897890, -1.627767898183747119, 3.360948587163227863 ) ) ;
#23887 = VERTEX_POINT ( 'NONE', #64277 ) ;
#23888 = CARTESIAN_POINT ( 'NONE',  ( 0.2648978790185619880, 6.008231198269132989, -10.67083876753485328 ) ) ;
#23889 = VECTOR ( 'NONE', #527, 1000.000000000000000 ) ;
#23890 = CARTESIAN_POINT ( 'NONE',  ( 2.251152103363642354, 6.550893877460208792, -3.926807817126119371 ) ) ;
#23891 = CARTESIAN_POINT ( 'NONE',  ( -35.00000000000000000, 0.000000000000000000, 0.000000000000000000 ) ) ;
#23892 = VERTEX_POINT ( 'NONE', #34343 ) ;
#23893 = ORIENTED_EDGE ( 'NONE', *, *, #22107, .T. ) ;
#23894 = DIRECTION ( 'NONE',  ( 0.000000000000000000, 0.000000000000000000, 1.000000000000000000 ) ) ;
#23895 = EDGE_CURVE ( 'NONE', #11924, #20989, #25070, .T. ) ;
#23896 = AXIS2_PLACEMENT_3D ( 'NONE', #28302, #63859, #53907 ) ;
#23897 = DIRECTION ( 'NONE',  ( 1.000000000000000000, 0.000000000000000000, 0.000000000000000000 ) ) ;
#23898 = EDGE_LOOP ( 'NONE', ( #8005, #47522, #51701, #47340 ) ) ;
#23899 = VERTEX_POINT ( 'NONE', #13722 ) ;
#23900 = B_SPLINE_CURVE_WITH_KNOTS ( 'NONE', 3,
 ( #63107, #23874, #12889, #2275, #2624, #18570, #17568, #13225, #48485, #2934, #58807, #23200, #27865, #42817, #64399, #22555 ),
 .UNSPECIFIED., .F., .F.,
 ( 4, 3, 3, 3, 3, 4 ),
 ( 4.336808689942017255E-19, 0.0002176109881720234007, 0.0004352086762394597992, 0.0006528017811446890258, 0.0007615147961451721684, 0.0009453342004947402075 ),
 .UNSPECIFIED. ) ;
#23901 = CARTESIAN_POINT ( 'NONE',  ( 12.47628546223243617, 0.000000000000000000, 13.50000000000000178 ) ) ;
#23902 = ADVANCED_FACE ( 'NONE', ( #34007 ), #44312, .T. ) ;
#23903 = AXIS2_PLACEMENT_3D ( 'NONE', #27696, #6131, #26392 ) ;
#23904 = DIRECTION ( 'NONE',  ( 0.000000000000000000, -0.2355298848897378339, -0.9718671068226493182 ) ) ;
#23905 = CARTESIAN_POINT ( 'NONE',  ( 0.2647959493198558389, 10.53111783886899744, -6.249846955854157393 ) ) ;
#23906 = CARTESIAN_POINT ( 'NONE',  ( 0.3160775863651102413, 8.065044686487434333, -9.237902461149165134 ) ) ;
#23907 = CARTESIAN_POINT ( 'NONE',  ( -37.00000000000000711, 0.000000000000000000, 0.000000000000000000 ) ) ;
#23908 = CARTESIAN_POINT ( 'NONE',  ( -35.00000000000000000, 11.50504120060943158, 4.018060380616439886 ) ) ;
#23909 = EDGE_LOOP ( 'NONE', ( #56380, #29280, #46861, #14455 ) ) ;
#23910 =( BOUNDED_SURFACE ( )  B_SPLINE_SURFACE ( 3, 1, ( 
 ( #30712, #5482 ),
 ( #6132, #26393 ),
 ( #51021, #36023 ),
 ( #36374, #25410 ) ),
 .UNSPECIFIED., .F., .F., .F. ) 
 B_SPLINE_SURFACE_WITH_KNOTS ( ( 4, 4 ),
 ( 2, 2 ),
 ( 0.000000000000000000, 1.000000000000000000 ),
 ( 0.000000000000000000, 1.000000000000000000 ),
 .UNSPECIFIED. ) 
 GEOMETRIC_REPRESENTATION_ITEM ( )  RATIONAL_B_SPLINE_SURFACE ( (
 ( 1.000000000000000000, 1.000000000000000000),
 ( 0.9942764183789327692, 0.8450855930916585379),
 ( 0.9942764183789327692, 0.8450855930916585379),
 ( 1.000000000000000000, 1.000000000000000000) ) ) 
 REPRESENTATION_ITEM ( '' )  SURFACE ( )  );
#23911 = LINE ( 'NONE', #53173, #41153 ) ;
#23912 = CARTESIAN_POINT ( 'NONE',  ( -14.51274404441612376, 7.865079314623513618, 9.063796499285235342 ) ) ;
#23913 = CARTESIAN_POINT ( 'NONE',  ( 0.2648978790185619880, -9.295532325666501450, 7.972372351882998309 ) ) ;
#23914 = DIRECTION ( 'NONE',  ( 1.000000000000000000, 0.000000000000000000, 0.000000000000000000 ) ) ;
#23915 = DIRECTION ( 'NONE',  ( 0.000000000000000000, 0.000000000000000000, 1.000000000000000000 ) ) ;
#23916 = CARTESIAN_POINT ( 'NONE',  ( -22.71097035706202405, -4.510116093748277599, 2.118550233809401107 ) ) ;
#23917 = CARTESIAN_POINT ( 'NONE',  ( 3.092491956585653679, -4.340140213817308634, -6.622742949902657550 ) ) ;
#23918 = CARTESIAN_POINT ( 'NONE',  ( -29.43980975494970309, -3.641506875706030488, 25.00000000000000000 ) ) ;
#23919 = CARTESIAN_POINT ( 'NONE',  ( 1.109979610369147274, 5.843815872356888264, 11.08130463534426902 ) ) ;
#23920 = EDGE_CURVE ( 'NONE', #52172, #55547, #24052, .T. ) ;
#23921 = ORIENTED_EDGE ( 'NONE', *, *, #55545, .T. ) ;
#23922 = CARTESIAN_POINT ( 'NONE',  ( -17.67947061630126271, 7.441336280027901040, -9.417258690134145738 ) ) ;
#23923 = ORIENTED_EDGE ( 'NONE', *, *, #42113, .F. ) ;
#23924 = DIRECTION ( 'NONE',  ( 0.000000000000000000, 0.4380125133593912312, -0.8989688749565187820 ) ) ;
#23925 = DIRECTION ( 'NONE',  ( 1.000000000000000000, 0.000000000000000000, 0.000000000000000000 ) ) ;
#23926 = CARTESIAN_POINT ( 'NONE',  ( 2.305787727787084407, 6.711944854845823372, 3.682701754025536012 ) ) ;
#23927 = CARTESIAN_POINT ( 'NONE',  ( -35.00000000000000000, -11.81949347079749124, 2.968224442958359965 ) ) ;
#23928 = CARTESIAN_POINT ( 'NONE',  ( 0.2638984909335720941, -4.375449752477059029, -11.43908195192333821 ) ) ;
#23929 = ORIENTED_EDGE ( 'NONE', *, *, #18318, .F. ) ;
#23930 = CARTESIAN_POINT ( 'NONE',  ( 35.00000000000000000, -1.262958560998847624, -12.12087942037209665 ) ) ;
#23931 = CARTESIAN_POINT ( 'NONE',  ( -22.27834755396594346, 3.610802913011834203, -0.7418417409069075763 ) ) ;
#23932 = DIRECTION ( 'NONE',  ( 0.000000000000000000, 0.000000000000000000, -1.000000000000000000 ) ) ;
#23933 = CARTESIAN_POINT ( 'NONE',  ( -22.28694879868232803, 2.661377239830763131, 2.586016167700781576 ) ) ;
#23934 = EDGE_CURVE ( 'NONE', #36243, #23284, #26115, .T. ) ;
#23935 = CARTESIAN_POINT ( 'NONE',  ( 2.080613030138687591, 5.400000000000000355, 0.000000000000000000 ) ) ;
#23936 = AXIS2_PLACEMENT_3D ( 'NONE', #15954, #51248, #46561 ) ;
#23937 = ORIENTED_EDGE ( 'NONE', *, *, #29146, .F. ) ;
#23938 = CARTESIAN_POINT ( 'NONE',  ( -19.02967556479663713, 11.99999999999999645, 1.585036030062028271E-15 ) ) ;
#23939 = ORIENTED_EDGE ( 'NONE', *, *, #43030, .F. ) ;
#23940 = CARTESIAN_POINT ( 'NONE',  ( 3.152665057736253829, 5.761241965767907480, -5.461013642407265500 ) ) ;
#23941 = DIRECTION ( 'NONE',  ( 0.000000000000000000, -0.5767582926625031137, -0.8169148498130233138 ) ) ;
#23942 = CYLINDRICAL_SURFACE ( 'NONE', #37355, 12.74999999999999822 ) ;
#23943 = DIRECTION ( 'NONE',  ( 1.000000000000000000, 0.000000000000000000, 0.000000000000000000 ) ) ;
#23944 = VECTOR ( 'NONE', #2722, 1000.000000000000000 ) ;
#23945 = EDGE_LOOP ( 'NONE', ( #60937, #63206, #62749, #57928 ) ) ;
#23946 = ORIENTED_EDGE ( 'NONE', *, *, #43009, .F. ) ;
#23947 = CARTESIAN_POINT ( 'NONE',  ( -27.10719052120871098, 2.261993590776037788, -0.6736837626858775963 ) ) ;
#23948 = EDGE_CURVE ( 'NONE', #21913, #6336, #47386, .T. ) ;
#23949 = CARTESIAN_POINT ( 'NONE',  ( -37.00000000000000711, 0.000000000000000000, 0.000000000000000000 ) ) ;
#23950 = LINE ( 'NONE', #3687, #13021 ) ;
#23951 = FACE_OUTER_BOUND ( 'NONE', #65387, .T. ) ;
#23952 = CARTESIAN_POINT ( 'NONE',  ( 3.092491956585968982, 6.622742949902548304, -4.340140213817556436 ) ) ;
#23953 = CARTESIAN_POINT ( 'NONE',  ( -35.00000000000000000, -6.564808257521844048, 10.93004082984016279 ) ) ;
#23954 = EDGE_CURVE ( 'NONE', #19473, #19363, #63260, .T. ) ;
#23955 = ORIENTED_EDGE ( 'NONE', *, *, #24021, .T. ) ;
#23956 = ORIENTED_EDGE ( 'NONE', *, *, #35626, .T. ) ;
#23957 = ORIENTED_EDGE ( 'NONE', *, *, #53041, .F. ) ;
#23958 = CARTESIAN_POINT ( 'NONE',  ( 2.245754705088395031, 7.212684575686813204, -2.506725724682591583 ) ) ;
#23959 = CARTESIAN_POINT ( 'NONE',  ( -35.00000000000000000, 0.000000000000000000, 0.000000000000000000 ) ) ;
#23960 = EDGE_CURVE ( 'NONE', #44463, #52168, #60095, .T. ) ;
#23961 = ORIENTED_EDGE ( 'NONE', *, *, #10244, .T. ) ;
#23962 = FACE_OUTER_BOUND ( 'NONE', #13903, .T. ) ;
#23963 = DIRECTION ( 'NONE',  ( 1.000000000000000000, -0.000000000000000000, 0.000000000000000000 ) ) ;
#23964 = VERTEX_POINT ( 'NONE', #34972 ) ;
#23965 = CARTESIAN_POINT ( 'NONE',  ( 2.889800649504073782, -3.002151847318879518, -5.334644486274226161 ) ) ;
#23966 = CARTESIAN_POINT ( 'NONE',  ( 37.00000000000000711, -12.73293890771483561, -0.6593684648220077271 ) ) ;
#23967 = DIRECTION ( 'NONE',  ( 1.000000000000000000, 0.000000000000000000, 0.000000000000000000 ) ) ;
#23968 = ORIENTED_EDGE ( 'NONE', *, *, #1859, .T. ) ;
#23969 = ORIENTED_EDGE ( 'NONE', *, *, #20310, .F. ) ;
#23970 = CARTESIAN_POINT ( 'NONE',  ( 2.255723233588950993, 2.488140745365865047, 7.222632368701277450 ) ) ;
#23971 = EDGE_LOOP ( 'NONE', ( #13566, #48740, #16926, #35295 ) ) ;
#23972 = EDGE_CURVE ( 'NONE', #15089, #61328, #6072, .T. ) ;
#23973 = AXIS2_PLACEMENT_3D ( 'NONE', #25835, #31468, #21501 ) ;
#23974 = SURFACE_SIDE_STYLE ('',( #28948 ) ) ;
#23975 = VERTEX_POINT ( 'NONE', #30006 ) ;
#23976 = ORIENTED_EDGE ( 'NONE', *, *, #61719, .T. ) ;
#23977 = ORIENTED_EDGE ( 'NONE', *, *, #24878, .T. ) ;
#23978 = DIRECTION ( 'NONE',  ( 0.000000000000000000, 0.000000000000000000, 1.000000000000000000 ) ) ;
#23979 = CARTESIAN_POINT ( 'NONE',  ( -11.19906371801375577, -32.63487729457269637, -12.17775756912196172 ) ) ;
#23980 = CARTESIAN_POINT ( 'NONE',  ( -21.17861794710831091, 13.00977982294135593, -3.604945070120774808 ) ) ;
#23981 = CARTESIAN_POINT ( 'NONE',  ( 0.3675815128205912052, 11.44679196252415210, -4.447030445008065769 ) ) ;
#23982 = CARTESIAN_POINT ( 'NONE',  ( 0.8375941296801872049, -0.3844307390187073903, 12.43103843094035454 ) ) ;
#23983 = VERTEX_POINT ( 'NONE', #56605 ) ;
#23984 = DIRECTION ( 'NONE',  ( 0.000000000000000000, 0.000000000000000000, 1.000000000000000000 ) ) ;
#23985 = VERTEX_POINT ( 'NONE', #50318 ) ;
#23986 = DIRECTION ( 'NONE',  ( 0.9261641133930337277, 0.000000000000000000, -0.3771207168306929813 ) ) ;
#23987 = CARTESIAN_POINT ( 'NONE',  ( -18.74580655112670868, -4.843304743421753322, -12.60275085743400680 ) ) ;
#23988 = ORIENTED_EDGE ( 'NONE', *, *, #47884, .T. ) ;
#23989 = DIRECTION ( 'NONE',  ( 1.000000000000000000, 0.000000000000000000, -0.000000000000000000 ) ) ;
#23990 = CARTESIAN_POINT ( 'NONE',  ( 28.25627792643572889, 10.45952599874087063, 5.894934686502148580 ) ) ;
#23991 = CARTESIAN_POINT ( 'NONE',  ( -35.04643116707788408, -0.002453861112623398344, -0.01193867652721398998 ) ) ;
#23992 = VECTOR ( 'NONE', #55939, 1000.000000000000000 ) ;
#23993 = ORIENTED_EDGE ( 'NONE', *, *, #32550, .T. ) ;
#23994 = EDGE_LOOP ( 'NONE', ( #16254, #28259, #22537, #38419 ) ) ;
#23995 = CARTESIAN_POINT ( 'NONE',  ( 2.269879328256732887, -7.642470739868881147, 0.1483462450596979287 ) ) ;
#23996 = ORIENTED_EDGE ( 'NONE', *, *, #51164, .F. ) ;
#23997 = CARTESIAN_POINT ( 'NONE',  ( 35.00000000000000000, -8.496612874013090178, 9.506317355798454827 ) ) ;
#23998 = CARTESIAN_POINT ( 'NONE',  ( 37.00000000000000711, 4.705694406421931860E-17, -3.469127814946512892E-15 ) ) ;
#23999 = CARTESIAN_POINT ( 'NONE',  ( -30.03609618253042868, 0.3802027729374650722, 13.49649232113790909 ) ) ;
#24000 = CARTESIAN_POINT ( 'NONE',  ( 3.031336079629076696, 4.304138522350157814, 6.621879275826709765 ) ) ;
#24001 = CARTESIAN_POINT ( 'NONE',  ( 13.19552928342135090, 11.39730694699084523, -3.781285820845986301 ) ) ;
#24002 = ORIENTED_EDGE ( 'NONE', *, *, #42252, .F. ) ;
#24003 = CARTESIAN_POINT ( 'NONE',  ( 0.6511581176960867801, 1.822219471614292763, 12.23990098761610490 ) ) ;
#24004 = EDGE_CURVE ( 'NONE', #19340, #36463, #10776, .T. ) ;
#24005 = B_SPLINE_CURVE_WITH_KNOTS ( 'NONE', 3,
 ( #44607, #53, #15008, #55605, #60915, #15354, #6055 ),
 .UNSPECIFIED., .F., .F.,
 ( 4, 3, 4 ),
 ( 0.000000000000000000, 0.001700533616330540372, 0.005002426799371281763 ),
 .UNSPECIFIED. ) ;
#24006 = CARTESIAN_POINT ( 'NONE',  ( 0.2834382757448029588, -12.09963924911733457, -1.927645269571007125 ) ) ;
#24007 = DIRECTION ( 'NONE',  ( 1.000000000000000000, 0.000000000000000000, 0.000000000000000000 ) ) ;
#24008 = B_SPLINE_CURVE_WITH_KNOTS ( 'NONE', 3,
 ( #32760, #23140, #48433, #8176, #17167, #37107 ),
 .UNSPECIFIED., .F., .F.,
 ( 4, 2, 4 ),
 ( 0.0002637379172149909154, 0.0009975831966603271490, 0.001731428476105663708 ),
 .UNSPECIFIED. ) ;
#24009 = CARTESIAN_POINT ( 'NONE',  ( -35.00000000000000000, -5.921969905510425569, 10.14408668126211488 ) ) ;
#24010 = CARTESIAN_POINT ( 'NONE',  ( 0.2648978790185602672, 7.972372351883029395, 9.295532325666474804 ) ) ;
#24011 = CARTESIAN_POINT ( 'NONE',  ( 7.195572628608377208, -7.349260008028998037, -9.497068771844457302 ) ) ;
#24012 = DIRECTION ( 'NONE',  ( -1.000000000000000000, 0.000000000000000000, 0.000000000000000000 ) ) ;
#24013 = EDGE_CURVE ( 'NONE', #23085, #3506, #27198, .T. ) ;
#24014 = AXIS2_PLACEMENT_3D ( 'NONE', #12011, #21335, #62879 ) ;
#24015 = EDGE_LOOP ( 'NONE', ( #65092, #29023, #49642, #11256 ) ) ;
#24016 = CARTESIAN_POINT ( 'NONE',  ( -27.08429572838383947, -1.338867938658200307, -1.859677275556420151 ) ) ;
#24017 = AXIS2_PLACEMENT_3D ( 'NONE', #117, #45338, #14724 ) ;
#24019 = ORIENTED_EDGE ( 'NONE', *, *, #37458, .F. ) ;
#24018 = EDGE_CURVE ( 'NONE', #39168, #59008, #39918, .T. ) ;
#24020 = CARTESIAN_POINT ( 'NONE',  ( 2.000000000000001776, 4.915517050588478654, -4.717154614762057108 ) ) ;
#24021 = EDGE_CURVE ( 'NONE', #20717, #17286, #36301, .T. ) ;
#24022 = LINE ( 'NONE', #19026, #14079 ) ;
#24023 = CARTESIAN_POINT ( 'NONE',  ( 2.440552418640497212, -7.301551120181781762, 2.447453236303800406 ) ) ;
#24024 = CARTESIAN_POINT ( 'NONE',  ( 41.00000000000000711, -25.03188948156373428, -4.500000000000011546 ) ) ;
#24025 = EDGE_CURVE ( 'NONE', #65378, #64221, #61140, .T. ) ;
#24026 = VERTEX_POINT ( 'NONE', #60268 ) ;
#24027 = ORIENTED_EDGE ( 'NONE', *, *, #44272, .T. ) ;
#24028 = ORIENTED_EDGE ( 'NONE', *, *, #63637, .T. ) ;
#24029 = CARTESIAN_POINT ( 'NONE',  ( 0.3160775863651094642, -7.697077652699381822, -9.546663463486119383 ) ) ;
#24030 = EDGE_CURVE ( 'NONE', #41230, #17964, #31325, .T. ) ;
#24031 = ORIENTED_EDGE ( 'NONE', *, *, #6802, .F. ) ;
#24032 = CARTESIAN_POINT ( 'NONE',  ( -22.27721038036499834, -2.320305412324239036, -2.858424446490937854 ) ) ;
#24033 = CARTESIAN_POINT ( 'NONE',  ( -35.00000000000000000, -7.251710744571512102, -9.240395740215712195 ) ) ;
#24034 = CARTESIAN_POINT ( 'NONE',  ( 0.3610902822527213840, -9.234828023175149170, 8.091349661862597742 ) ) ;
#24035 = DIRECTION ( 'NONE',  ( 1.000000000000000000, -0.000000000000000000, 0.000000000000000000 ) ) ;
#24036 = ORIENTED_EDGE ( 'NONE', *, *, #9649, .T. ) ;
#24037 = CARTESIAN_POINT ( 'NONE',  ( 35.00000000000000000, 4.705694406421931860E-17, -3.469127814946512892E-15 ) ) ;
#24038 = EDGE_CURVE ( 'NONE', #4569, #33520, #25680, .T. ) ;
#24039 = CARTESIAN_POINT ( 'NONE',  ( 0.000000000000000000, -6.662861565602071323, 1.421313227905616650 ) ) ;
#24040 = CARTESIAN_POINT ( 'NONE',  ( 2.247112776671470247, -1.440655381229420939, -7.499199956302001091 ) ) ;
#24042 = ORIENTED_EDGE ( 'NONE', *, *, #27432, .T. ) ;
#24041 = DIRECTION ( 'NONE',  ( 0.000000000000000000, -0.01356324068817998940, 0.9999080150203990547 ) ) ;
#24043 = DIRECTION ( 'NONE',  ( -1.000000000000000000, 0.000000000000000000, 0.000000000000000000 ) ) ;
#24044 = ORIENTED_EDGE ( 'NONE', *, *, #21332, .F. ) ;
#24045 = CARTESIAN_POINT ( 'NONE',  ( -37.00000000000000711, -10.49591321039677005, -5.273331777780449592 ) ) ;
#24046 = ORIENTED_EDGE ( 'NONE', *, *, #27243, .T. ) ;
#24047 = CARTESIAN_POINT ( 'NONE',  ( 2.990245332647881060, 2.413832934171125100, 8.130497889782944299 ) ) ;
#24048 = CARTESIAN_POINT ( 'NONE',  ( -35.00000000000000000, 0.000000000000000000, 0.000000000000000000 ) ) ;
#24049 = CARTESIAN_POINT ( 'NONE',  ( 3.152665057735509979, 7.102135024646700323, 3.546019893115181620 ) ) ;
#24050 = CARTESIAN_POINT ( 'NONE',  ( 0.2717059086739018192, -4.023283916512504277, 11.56868249951480365 ) ) ;
#24051 = CARTESIAN_POINT ( 'NONE',  ( 37.00000000000000711, 4.705694406421931860E-17, -3.469127814946512892E-15 ) ) ;
#24052 = LINE ( 'NONE', #39322, #47391 ) ;
#24053 = DIRECTION ( 'NONE',  ( 1.000000000000000000, -0.000000000000000000, 0.000000000000000000 ) ) ;
#24055 = VERTEX_POINT ( 'NONE', #61249 ) ;
#24054 = CARTESIAN_POINT ( 'NONE',  ( -27.15511094194037156, -2.092607239484530091, 1.375165223101502576 ) ) ;
#24056 = EDGE_CURVE ( 'NONE', #28113, #5802, #35954, .T. ) ;
#24057 = ORIENTED_EDGE ( 'NONE', *, *, #32225, .T. ) ;
#24058 = CARTESIAN_POINT ( 'NONE',  ( 35.00000000000000000, 4.705694406421931860E-17, -3.469127814946512892E-15 ) ) ;
#24059 = VERTEX_POINT ( 'NONE', #46301 ) ;
#24060 = ORIENTED_EDGE ( 'NONE', *, *, #34870, .F. ) ;
#24061 = DIRECTION ( 'NONE',  ( 0.000000000000000000, 0.000000000000000000, 1.000000000000000000 ) ) ;
#24062 = CARTESIAN_POINT ( 'NONE',  ( -37.00000000000000711, 0.000000000000000000, 0.000000000000000000 ) ) ;
#24063 = DIRECTION ( 'NONE',  ( 0.000000000000000000, 0.01356324068817992175, -0.9999080150203990547 ) ) ;
#24064 = CARTESIAN_POINT ( 'NONE',  ( 47.00000000000000711, 4.705694406421931860E-17, -3.469127814946512892E-15 ) ) ;
#24065 = CARTESIAN_POINT ( 'NONE',  ( 0.2676618633000462100, 10.68562420805850621, -5.983781707237496583 ) ) ;
#24066 = CIRCLE ( 'NONE', #47420, 4.999999999999999112 ) ;
#24067 = CARTESIAN_POINT ( 'NONE',  ( 25.05309951391468459, 25.00000000000000000, -8.132934882857099979 ) ) ;
#24068 = CIRCLE ( 'NONE', #4940, 4.999999999999999112 ) ;
#24069 = ORIENTED_EDGE ( 'NONE', *, *, #39904, .T. ) ;
#24070 = DIRECTION ( 'NONE',  ( 0.000000000000000000, -0.01356324068818000848, 0.9999080150203990547 ) ) ;
#24071 = CARTESIAN_POINT ( 'NONE',  ( -27.08421723179412410, -1.556274442127719704, -1.681635392574643673 ) ) ;
#24072 = DIRECTION ( 'NONE',  ( -0.000000000000000000, -1.000000000000000000, -0.000000000000000000 ) ) ;
#24073 = ORIENTED_EDGE ( 'NONE', *, *, #49049, .F. ) ;
#24074 = EDGE_CURVE ( 'NONE', #46959, #5369, #52080, .T. ) ;
#24075 =( BOUNDED_CURVE ( )  B_SPLINE_CURVE ( 3, ( #19883, #61746, #51484, #40142 ),
 .UNSPECIFIED., .F., .F. ) 
 B_SPLINE_CURVE_WITH_KNOTS ( ( 4, 4 ),
 ( 5.102875344919000966, 5.142681165258892406 ),
 .UNSPECIFIED. ) 
 CURVE ( )  GEOMETRIC_REPRESENTATION_ITEM ( )  RATIONAL_B_SPLINE_CURVE ( ( 1.000000000000000000, 0.9998679624143003153, 0.9998679624143003153, 1.000000000000000000 ) ) 
 REPRESENTATION_ITEM ( '' )  );
#24076 = CARTESIAN_POINT ( 'NONE',  ( -6.736209972540539326, -1.198479029871813095, 13.44688918519066334 ) ) ;
#24077 = CARTESIAN_POINT ( 'NONE',  ( -35.00000000000000000, 11.70009620280411688, 1.039216533672945753 ) ) ;
#24078 = ORIENTED_EDGE ( 'NONE', *, *, #15747, .T. ) ;
#24079 = CARTESIAN_POINT ( 'NONE',  ( 1.452237505248552996, -3.767214359061047180, -12.08199618361516592 ) ) ;
#24080 = CARTESIAN_POINT ( 'NONE',  ( -35.00000000000000000, 11.30684963584389280, 4.545979934229452901 ) ) ;
#24081 = CARTESIAN_POINT ( 'NONE',  ( 3.624631522511398529, 4.203481679627634193, 11.24801011402735362 ) ) ;
#24082 = EDGE_CURVE ( 'NONE', #58016, #28622, #19587, .T. ) ;
#24083 = EDGE_CURVE ( 'NONE', #61832, #39576, #42043, .T. ) ;
#24084 = CARTESIAN_POINT ( 'NONE',  ( -35.00000000000000000, -4.018060380616481631, 11.50504120060941915 ) ) ;
#24085 = DIRECTION ( 'NONE',  ( 1.000000000000000000, 0.000000000000000000, 0.000000000000000000 ) ) ;
#24086 = VERTEX_POINT ( 'NONE', #41943 ) ;
#24087 = ADVANCED_FACE ( 'NONE', ( #62230 ), #28163, .F. ) ;
#24088 = CARTESIAN_POINT ( 'NONE',  ( 2.280717697723837922, 0.1564731737570113912, 7.645922213779906329 ) ) ;
#24089 = CARTESIAN_POINT ( 'NONE',  ( -37.00000000000000711, -10.63508530065525370, 4.986700593229667078 ) ) ;
#24090 = CARTESIAN_POINT ( 'NONE',  ( 3.152665057734040488, 0.000000000000000000, 0.000000000000000000 ) ) ;
#24091 = ORIENTED_EDGE ( 'NONE', *, *, #65095, .T. ) ;
#24092 = DIRECTION ( 'NONE',  ( 1.000000000000000000, 0.000000000000000000, 0.000000000000000000 ) ) ;
#24093 = CARTESIAN_POINT ( 'NONE',  ( 2.241528039335009215, 6.603755931420482561, 3.830846649711536323 ) ) ;
#24094 = EDGE_CURVE ( 'NONE', #59597, #60093, #27064, .T. ) ;
#24095 = ORIENTED_EDGE ( 'NONE', *, *, #58730, .T. ) ;
#24096 = ORIENTED_EDGE ( 'NONE', *, *, #9009, .F. ) ;
#24097 = AXIS2_PLACEMENT_3D ( 'NONE', #42747, #21510, #46440 ) ;
#24098 = DIRECTION ( 'NONE',  ( 1.000000000000000000, 0.000000000000000000, 0.000000000000000000 ) ) ;
#24099 = AXIS2_PLACEMENT_3D ( 'NONE', #8019, #17660, #53229 ) ;
#24100 = VERTEX_POINT ( 'NONE', #56941 ) ;
#24101 = FACE_OUTER_BOUND ( 'NONE', #1945, .T. ) ;
#24102 = CARTESIAN_POINT ( 'NONE',  ( 5.515539859299206427, -0.0001942659352250951453, -0.006049968793488818240 ) ) ;
#24103 = CARTESIAN_POINT ( 'NONE',  ( 0.2706063244538029489, -6.275112929891680125, 10.51833723927420472 ) ) ;
#24104 = CARTESIAN_POINT ( 'NONE',  ( 2.241352910868909643, -7.532448145350499225, -1.243507963608171174 ) ) ;
#24105 = ADVANCED_FACE ( 'NONE', ( #1730 ), #6721, .T. ) ;
#24106 = CARTESIAN_POINT ( 'NONE',  ( 1.283627346226324351, 12.00363697230078408, 3.783098238613546993 ) ) ;
#24108 = ORIENTED_EDGE ( 'NONE', *, *, #36212, .F. ) ;
#24107 = CARTESIAN_POINT ( 'NONE',  ( 0.000000000000000000, 0.000000000000000000, 0.000000000000000000 ) ) ;
#24109 = CARTESIAN_POINT ( 'NONE',  ( 0.3665391374699464300, 9.237363111276767569, 8.095513416941260587 ) ) ;
#24110 = EDGE_CURVE ( 'NONE', #25348, #33198, #61907, .T. ) ;
#24111 = ORIENTED_EDGE ( 'NONE', *, *, #29300, .F. ) ;
#24112 = CARTESIAN_POINT ( 'NONE',  ( -35.05012975565874456, -0.005092487515925959649, 0.01296790604420273996 ) ) ;
#24113 = ORIENTED_EDGE ( 'NONE', *, *, #63099, .T. ) ;
#24114 = ORIENTED_EDGE ( 'NONE', *, *, #52243, .T. ) ;
#24115 = DIRECTION ( 'NONE',  ( -1.000000000000000000, 0.000000000000000000, 0.000000000000000000 ) ) ;
#24116 = EDGE_CURVE ( 'NONE', #47989, #48505, #63968, .T. ) ;
#24117 = CARTESIAN_POINT ( 'NONE',  ( -14.21898193534997290, -33.70038524408893466, 9.575031237889474411 ) ) ;
#24118 = CARTESIAN_POINT ( 'NONE',  ( -24.80857425325906718, 8.631266723926000139, 10.38663870023611757 ) ) ;
#24119 = CARTESIAN_POINT ( 'NONE',  ( 23.74857913196462178, -3.119318027837767460, 11.59209599145404646 ) ) ;
#24120 = CARTESIAN_POINT ( 'NONE',  ( -35.00000000000000000, 11.38112321385055026, -2.905556151562505462 ) ) ;
#24121 = ADVANCED_FACE ( 'NONE', ( #11678 ), #31634, .T. ) ;
#24122 = CARTESIAN_POINT ( 'NONE',  ( 34.00000000000000000, 11.99999999999999822, 1.469576158976822172E-15 ) ) ;
#24124 = VERTEX_POINT ( 'NONE', #37941 ) ;
#24123 = ADVANCED_FACE ( 'NONE', ( #57593 ), #17680, .T. ) ;
#24125 = ORIENTED_EDGE ( 'NONE', *, *, #42763, .T. ) ;
#24126 = CARTESIAN_POINT ( 'NONE',  ( 2.000000000000001776, 6.250523986463984549, 3.007653927006597172 ) ) ;
#24127 = ADVANCED_FACE ( 'NONE', ( #58234 ), #51944, .T. ) ;
#24128 = B_SPLINE_CURVE_WITH_KNOTS ( 'NONE', 3,
 ( #64940, #56278, #35666, #25056, #65587, #29687, #30029, #45327, #49671, #103, #9402, #4115, #61274 ),
 .UNSPECIFIED., .F., .F.,
 ( 4, 3, 3, 3, 4 ),
 ( 3.127317220692750759E-18, 6.607593386745476828E-05, 0.0001321518677373526235, 0.0001982171734706228384, 0.0002642860854759475787 ),
 .UNSPECIFIED. ) ;
#24129 = ORIENTED_EDGE ( 'NONE', *, *, #40467, .F. ) ;
#24130 = LINE ( 'NONE', #38436, #8314 ) ;
#24131 = DIRECTION ( 'NONE',  ( 0.000000000000000000, 0.000000000000000000, 1.000000000000000000 ) ) ;
#24132 = CARTESIAN_POINT ( 'NONE',  ( 0.000000000000000000, 4.962980376314141573, -4.846014654777754060 ) ) ;
#24133 = CARTESIAN_POINT ( 'NONE',  ( -35.00000000000000000, -10.91072401419407001, -5.428340790341820821 ) ) ;
#24134 = LINE ( 'NONE', #8844, #56462 ) ;
#24135 = DIRECTION ( 'NONE',  ( 0.000000000000000000, 0.01356324068817998940, -0.9999080150203990547 ) ) ;
#24136 = EDGE_LOOP ( 'NONE', ( #2337, #1711, #22050, #59136 ) ) ;
#24137 = AXIS2_PLACEMENT_3D ( 'NONE', #24062, #65272, #9390 ) ;
#24138 = ORIENTED_EDGE ( 'NONE', *, *, #25371, .F. ) ;
#24139 = DIRECTION ( 'NONE',  ( 0.000000000000000000, -0.04924826701373159060, -0.9987865678893284027 ) ) ;
#24140 = DIRECTION ( 'NONE',  ( -1.000000000000000000, 0.000000000000000000, 0.000000000000000000 ) ) ;
#24141 = AXIS2_PLACEMENT_3D ( 'NONE', #17267, #63137, #37867 ) ;
#24142 = ADVANCED_FACE ( 'NONE', ( #18984 ), #13333, .T. ) ;
#24143 = ORIENTED_EDGE ( 'NONE', *, *, #58947, .F. ) ;
#24144 = CARTESIAN_POINT ( 'NONE',  ( -35.00000000000000000, -2.696588552978969933, -12.46157735505192221 ) ) ;
#24145 = AXIS2_PLACEMENT_3D ( 'NONE', #42085, #16175, #31775 ) ;
#24146 = CARTESIAN_POINT ( 'NONE',  ( -5.806076944307488219, -1.481863301461679772, -11.90854409942760661 ) ) ;
#24147 = DIRECTION ( 'NONE',  ( 0.000000000000000000, -0.01356324068817991828, 0.9999080150203990547 ) ) ;
#24148 = CARTESIAN_POINT ( 'NONE',  ( 5.536195898058073439, -0.004468797463753836595, 0.007230647766619077016 ) ) ;
#24149 = CARTESIAN_POINT ( 'NONE',  ( 47.00000000000000711, 4.705694406421931860E-17, -3.469127814946512892E-15 ) ) ;
#24150 = ORIENTED_EDGE ( 'NONE', *, *, #27678, .T. ) ;
#24151 = FACE_OUTER_BOUND ( 'NONE', #13487, .T. ) ;
#24152 = LINE ( 'NONE', #61046, #294 ) ;
#24153 = ADVANCED_FACE ( 'NONE', ( #27981 ), #18594, .T. ) ;
#24154 = CARTESIAN_POINT ( 'NONE',  ( 37.00000000000000711, -7.561043153948031836, -9.557269938331533154 ) ) ;
#24155 = CARTESIAN_POINT ( 'NONE',  ( 37.00000000000000711, 5.556331110570566167, 11.47561260193570654 ) ) ;
#24156 = ORIENTED_EDGE ( 'NONE', *, *, #47884, .F. ) ;
#24157 = CARTESIAN_POINT ( 'NONE',  ( 2.241352910868908310, -2.532612177304491397, 7.202080440908734005 ) ) ;
#24158 = FACE_OUTER_BOUND ( 'NONE', #48711, .T. ) ;
#24159 = CARTESIAN_POINT ( 'NONE',  ( 6.734959099364806079, -31.93290117444115594, -13.38585010773448580 ) ) ;
#24160 = ORIENTED_EDGE ( 'NONE', *, *, #10804, .T. ) ;
#24161 = CARTESIAN_POINT ( 'NONE',  ( 1.719304012338836563, -7.017415949612288095, 10.62216384465580710 ) ) ;
#24162 = DIRECTION ( 'NONE',  ( 0.000000000000000000, 0.9289767198167898643, 0.3701381553399183955 ) ) ;
#24163 = CARTESIAN_POINT ( 'NONE',  ( 2.798553295784531159, 25.00000000000000000, 7.462808788758677814 ) ) ;
#24164 = EDGE_CURVE ( 'NONE', #49356, #13076, #8497, .T. ) ;
#24165 = CARTESIAN_POINT ( 'NONE',  ( 0.2706063244538020052, -8.006269958070651782, 9.268878137104373138 ) ) ;
#24166 = CARTESIAN_POINT ( 'NONE',  ( -9.733281154747491115, -12.57221497072713490, -4.922044890244330340 ) ) ;
#24167 = AXIS2_PLACEMENT_3D ( 'NONE', #58308, #3788, #38682 ) ;
#24168 = CARTESIAN_POINT ( 'NONE',  ( 0.7400311444011700157, 12.14938086789865856, -2.502569705372845288 ) ) ;
#24169 = ORIENTED_EDGE ( 'NONE', *, *, #58012, .T. ) ;
#24170 = DIRECTION ( 'NONE',  ( -0.000000000000000000, -1.000000000000000000, -0.000000000000000000 ) ) ;
#24171 = CARTESIAN_POINT ( 'NONE',  ( -7.181456785175555524, 8.540743096806467705, -10.45493698471458188 ) ) ;
#24172 = CIRCLE ( 'NONE', #61477, 4.999999999999999112 ) ;
#24173 = DIRECTION ( 'NONE',  ( -1.000000000000000000, 0.000000000000000000, 0.000000000000000000 ) ) ;
#24174 = CARTESIAN_POINT ( 'NONE',  ( 0.000000000000000000, 0.000000000000000000, 0.000000000000000000 ) ) ;
#24175 = DIRECTION ( 'NONE',  ( -1.000000000000000000, -0.000000000000000000, -0.000000000000000000 ) ) ;
#24176 = CARTESIAN_POINT ( 'NONE',  ( 35.00000000000000000, 4.705694406421931860E-17, -3.469127814946512892E-15 ) ) ;
#24177 = CYLINDRICAL_SURFACE ( 'NONE', #17477, 12.18650000000000055 ) ;
#24178 = CARTESIAN_POINT ( 'NONE',  ( 2.000000000000001776, -2.664846396702436948, -6.404188155573047325 ) ) ;
#24179 = ORIENTED_EDGE ( 'NONE', *, *, #28234, .T. ) ;
#24180 = EDGE_LOOP ( 'NONE', ( #38207, #38278, #58455, #60550 ) ) ;
#24181 = LINE ( 'NONE', #60744, #50191 ) ;
#24182 = ORIENTED_EDGE ( 'NONE', *, *, #30960, .T. ) ;
#24183 = AXIS2_PLACEMENT_3D ( 'NONE', #16116, #31416, #6156 ) ;
#24184 = SURFACE_STYLE_USAGE ( .BOTH. , #19855 ) ;
#24185 = EDGE_CURVE ( 'NONE', #32335, #21666, #13974, .T. ) ;
#24186 = DIRECTION ( 'NONE',  ( 0.000000000000000000, -0.9105187689795911643, 0.4134677391718608597 ) ) ;
#24187 = AXIS2_PLACEMENT_3D ( 'NONE', #44153, #18890, #24192 ) ;
#24188 = EDGE_CURVE ( 'NONE', #11102, #49132, #25951, .T. ) ;
#24189 = DIRECTION ( 'NONE',  ( 1.000000000000000000, -0.000000000000000000, 0.000000000000000000 ) ) ;
#24190 = ORIENTED_EDGE ( 'NONE', *, *, #23419, .T. ) ;
#24191 = CARTESIAN_POINT ( 'NONE',  ( -22.27218376572352554, -0.9173404081777536412, 3.566922835983782569 ) ) ;
#24192 = DIRECTION ( 'NONE',  ( 0.000000000000000000, 0.01356324068817998940, -0.9999080150203990547 ) ) ;
#24193 = LINE ( 'NONE', #54798, #35020 ) ;
#24194 = EDGE_LOOP ( 'NONE', ( #56195, #41028, #9433, #25331 ) ) ;
#24195 = VERTEX_POINT ( 'NONE', #3383 ) ;
#24196 = ADVANCED_FACE ( 'NONE', ( #23313 ), #22994, .T. ) ;
#24197 = CARTESIAN_POINT ( 'NONE',  ( 37.00000000000000711, -10.64792938439759595, -5.927257550915285833 ) ) ;
#24198 = DIRECTION ( 'NONE',  ( 0.000000000000000000, 0.01356324068817998940, -0.9999080150203989437 ) ) ;
#24199 = ORIENTED_EDGE ( 'NONE', *, *, #15516, .T. ) ;
#24200 = CARTESIAN_POINT ( 'NONE',  ( -27.71554010819489378, -10.41834511119169626, -5.961899762888907439 ) ) ;
#24201 = ORIENTED_EDGE ( 'NONE', *, *, #29794, .F. ) ;
#24202 = DIRECTION ( 'NONE',  ( -0.2475719085175094869, 0.000000000000000000, -0.9688695217174488894 ) ) ;
#24203 = CYLINDRICAL_SURFACE ( 'NONE', #30490, 5.000000000000000888 ) ;
#24204 = CARTESIAN_POINT ( 'NONE',  ( 2.000000000000001776, 6.812627895098307462, 2.855765430652722259 ) ) ;
#24205 = CARTESIAN_POINT ( 'NONE',  ( 5.530133899448235191, 0.01324661008606530140, 0.008946569461392205394 ) ) ;
#24206 = B_SPLINE_CURVE_WITH_KNOTS ( 'NONE', 3,
 ( #26738, #62958, #42015, #47672, #57009, #51699, #27069, #12087, #57992, #36383 ),
 .UNSPECIFIED., .F., .F.,
 ( 4, 3, 3, 4 ),
 ( 2.453269466693398698E-18, 6.607638129004608145E-05, 9.911389841680660494E-05, 0.0001667630577588617149 ),
 .UNSPECIFIED. ) ;
#24207 = CARTESIAN_POINT ( 'NONE',  ( 1.719304012338199517, 0.000000000000000000, 0.000000000000000000 ) ) ;
#24208 = ORIENTED_EDGE ( 'NONE', *, *, #48826, .F. ) ;
#24209 = DIRECTION ( 'NONE',  ( -1.000000000000000000, 0.000000000000000000, 0.000000000000000000 ) ) ;
#24210 = CARTESIAN_POINT ( 'NONE',  ( -17.88840112149050654, 6.209967363062701473, 10.27068265694474292 ) ) ;
#24211 = CARTESIAN_POINT ( 'NONE',  ( 0.2652384770603652409, -0.06606665821606472200, 12.24598129987882444 ) ) ;
#24212 = CARTESIAN_POINT ( 'NONE',  ( 2.305787727787084407, 7.654065630109506913, -0.1666591538752953128 ) ) ;
#24213 = DIRECTION ( 'NONE',  ( -1.000000000000000000, -1.685093406416449860E-16, 1.011030131491573426E-17 ) ) ;
#24214 = CARTESIAN_POINT ( 'NONE',  ( -27.10307689719147817, 1.615391801699798791, -1.703783570823888871 ) ) ;
#24215 = CARTESIAN_POINT ( 'NONE',  ( -27.15525204139121840, 2.440367606305298587, 0.5628609503965231742 ) ) ;
#24216 = CARTESIAN_POINT ( 'NONE',  ( 1.719304012341202004, 11.67935079956989775, -5.066286238790292273 ) ) ;
#24217 = CARTESIAN_POINT ( 'NONE',  ( -8.891032880924177206, 11.36194426013951997, -3.860857758255646921 ) ) ;
#24218 = AXIS2_PLACEMENT_3D ( 'NONE', #49729, #59706, #58747 ) ;
#24219 = EDGE_CURVE ( 'NONE', #54308, #34453, #32361, .T. ) ;
#24220 = ORIENTED_EDGE ( 'NONE', *, *, #10142, .F. ) ;
#24221 = CARTESIAN_POINT ( 'NONE',  ( 0.2767916011545367705, 0.1897947303542835418, 12.24854187541375161 ) ) ;
#24222 = EDGE_CURVE ( 'NONE', #21760, #25143, #40876, .T. ) ;
#24223 = ORIENTED_EDGE ( 'NONE', *, *, #54746, .T. ) ;
#24224 = CARTESIAN_POINT ( 'NONE',  ( 2.350038591458163406, 8.861946706685587927, 5.855794476068265197 ) ) ;
#24225 = CARTESIAN_POINT ( 'NONE',  ( 2.253265082352432724, -7.498995607278126307, -1.452519439326532824 ) ) ;
#24226 = CARTESIAN_POINT ( 'NONE',  ( 2.241451721903216399, -4.953785420083449687, 5.809054012306841486 ) ) ;
#24227 = DIRECTION ( 'NONE',  ( 0.000000000000000000, 0.8169148498130295311, -0.5767582926624942319 ) ) ;
#24228 = LINE ( 'NONE', #30836, #39244 ) ;
#24229 = ORIENTED_EDGE ( 'NONE', *, *, #4406, .F. ) ;
#24230 = CARTESIAN_POINT ( 'NONE',  ( -35.00000000000000000, 5.927257550915472351, -10.64792938439748937 ) ) ;
#24231 = DIRECTION ( 'NONE',  ( -1.000000000000000000, 0.000000000000000000, -0.000000000000000000 ) ) ;
#24232 = EDGE_CURVE ( 'NONE', #36610, #29381, #44189, .T. ) ;
#24233 = CARTESIAN_POINT ( 'NONE',  ( -35.00000000000000000, 5.927257550915472351, -10.64792938439748937 ) ) ;
#24234 = CARTESIAN_POINT ( 'NONE',  ( 17.05023968204110574, -34.50000000000000000, -4.356789313881336057 ) ) ;
#24235 = LINE ( 'NONE', #23935, #46741 ) ;
#24236 = ORIENTED_EDGE ( 'NONE', *, *, #4032, .F. ) ;
#24237 = CARTESIAN_POINT ( 'NONE',  ( 5.514970785353741078, -0.0003039746380528621597, -0.004713149585127533910 ) ) ;
#24238 = B_SPLINE_CURVE_WITH_KNOTS ( 'NONE', 3,
 ( #18862, #8881, #29173, #14497, #9853, #18564, #64711 ),
 .UNSPECIFIED., .F., .F.,
 ( 4, 3, 4 ),
 ( 3.571408088770477977E-15, 0.002398160485435184546, 0.005002426799386577687 ),
 .UNSPECIFIED. ) ;
#24239 = ORIENTED_EDGE ( 'NONE', *, *, #41382, .T. ) ;
#24240 = CARTESIAN_POINT ( 'NONE',  ( -35.04582288351658548, 0.002280196168869179450, -0.01249938581188446245 ) ) ;
#24242 = EDGE_CURVE ( 'NONE', #23409, #61480, #20705, .T. ) ;
#24241 = CARTESIAN_POINT ( 'NONE',  ( -11.92921645562187294, -32.88698380610403404, 11.67323352594769936 ) ) ;
#24243 = ADVANCED_FACE ( 'NONE', ( #19312 ), #39583, .T. ) ;
#24244 = CARTESIAN_POINT ( 'NONE',  ( 2.665405856346788838, 6.580881457836806447, -6.944580094494265943 ) ) ;
#24245 = EDGE_CURVE ( 'NONE', #14872, #42626, #10071, .T. ) ;
#24246 = PLANE ( 'NONE',  #54319 ) ;
#24247 = EDGE_LOOP ( 'NONE', ( #42409, #58592, #14622, #3219 ) ) ;
#24248 = ORIENTED_EDGE ( 'NONE', *, *, #8057, .T. ) ;
#24249 = CARTESIAN_POINT ( 'NONE',  ( 0.000000000000000000, -33.00000000000000000, 0.000000000000000000 ) ) ;
#24250 = FACE_OUTER_BOUND ( 'NONE', #28921, .T. ) ;
#24251 = DIRECTION ( 'NONE',  ( -1.000000000000000000, -0.000000000000000000, 0.000000000000000000 ) ) ;
#24252 = CARTESIAN_POINT ( 'NONE',  ( 0.2706063244538038925, 12.24670371972918481, 0.1752385892652434385 ) ) ;
#24253 = CARTESIAN_POINT ( 'NONE',  ( 0.9232058338315048962, -11.58467545991550907, -4.617996777200689351 ) ) ;
#24254 = DIRECTION ( 'NONE',  ( 0.000000000000000000, 0.000000000000000000, 1.000000000000000000 ) ) ;
#24255 = CARTESIAN_POINT ( 'NONE',  ( 2.241352910868909643, -7.503490710578223144, -1.407733736974942973 ) ) ;
#24256 = ORIENTED_EDGE ( 'NONE', *, *, #40771, .T. ) ;
#24257 = VERTEX_POINT ( 'NONE', #9304 ) ;
#24258 = ORIENTED_EDGE ( 'NONE', *, *, #37587, .F. ) ;
#24259 = CARTESIAN_POINT ( 'NONE',  ( -22.30625920655495165, 3.635849356906417640, -1.076742202099146839 ) ) ;
#24260 = EDGE_CURVE ( 'NONE', #37036, #44332, #22849, .T. ) ;
#24261 = AXIS2_PLACEMENT_3D ( 'NONE', #3294, #23569, #17920 ) ;
#24262 = DIRECTION ( 'NONE',  ( 0.000000000000000000, 1.000000000000000000, 0.000000000000000000 ) ) ;
#24263 = VERTEX_POINT ( 'NONE', #15931 ) ;
#24264 = DIRECTION ( 'NONE',  ( 0.000000000000000000, -0.1081190184239489566, 0.9941379571543588201 ) ) ;
#24265 = EDGE_CURVE ( 'NONE', #58366, #26477, #24930, .T. ) ;
#24266 = CARTESIAN_POINT ( 'NONE',  ( -22.51237073810381517, 0.2145858836692361438, 4.418556976583610130 ) ) ;
#24268 = VERTEX_POINT ( 'NONE', #46230 ) ;
#24267 = AXIS2_PLACEMENT_3D ( 'NONE', #54264, #14640, #4726 ) ;
#24269 = CIRCLE ( 'NONE', #38070, 5.000000000000000888 ) ;
#24270 = CARTESIAN_POINT ( 'NONE',  ( 2.507146904658097419, 7.180414359940957780, 2.843654641958914375 ) ) ;
#24271 =( BOUNDED_SURFACE ( )  B_SPLINE_SURFACE ( 3, 1, ( 
 ( #22244, #17270 ),
 ( #24205, #33847 ),
 ( #38180, #18604 ),
 ( #49505, #44471 ) ),
 .UNSPECIFIED., .F., .F., .F. ) 
 B_SPLINE_SURFACE_WITH_KNOTS ( ( 4, 4 ),
 ( 2, 2 ),
 ( 0.000000000000000000, 1.000000000000000000 ),
 ( 0.000000000000000000, 1.000000000000000000 ),
 .UNSPECIFIED. ) 
 GEOMETRIC_REPRESENTATION_ITEM ( )  RATIONAL_B_SPLINE_SURFACE ( (
 ( 1.000000000000000000, 1.000000000000000000),
 ( 0.6933888150995267674, 0.9895912004443193632),
 ( 0.6933888150995267674, 0.9895912004443193632),
 ( 1.000000000000000000, 1.000000000000000000) ) ) 
 REPRESENTATION_ITEM ( '' )  SURFACE ( )  );
#24272 = CARTESIAN_POINT ( 'NONE',  ( 35.00000000000000000, 9.506317355798490354, 8.496612874013052874 ) ) ;
#24273 = CARTESIAN_POINT ( 'NONE',  ( -27.09229696323320979, -2.247106967994379811, -0.5586335684093849396 ) ) ;
#24274 = ORIENTED_EDGE ( 'NONE', *, *, #14469, .F. ) ;
#24275 = ORIENTED_EDGE ( 'NONE', *, *, #61695, .F. ) ;
#24276 = CIRCLE ( 'NONE', #8333, 1.500000000000000444 ) ;
#24277 = CARTESIAN_POINT ( 'NONE',  ( 2.242819959140646802, 2.514828506625070403, 7.208832857235885072 ) ) ;
#24278 = ORIENTED_EDGE ( 'NONE', *, *, #3945, .F. ) ;
#24279 = DIRECTION ( 'NONE',  ( -1.000000000000000000, 0.000000000000000000, 0.000000000000000000 ) ) ;
#24280 = VERTEX_POINT ( 'NONE', #61491 ) ;
#24281 = ORIENTED_EDGE ( 'NONE', *, *, #4672, .F. ) ;
#24282 = AXIS2_PLACEMENT_3D ( 'NONE', #38785, #44097, #54742 ) ;
#24283 = ORIENTED_EDGE ( 'NONE', *, *, #5963, .T. ) ;
#24284 = CARTESIAN_POINT ( 'NONE',  ( -37.00000000000000711, -8.573591947375380329, 8.029056188533655103 ) ) ;
#24285 = CARTESIAN_POINT ( 'NONE',  ( -6.328161288312280419, -31.25458527549038124, -14.40172722985745324 ) ) ;
#24286 = DIRECTION ( 'NONE',  ( 0.000000000000000000, 0.01356324068817992175, -0.9999080150203990547 ) ) ;
#24287 = CARTESIAN_POINT ( 'NONE',  ( -22.46225619532221529, -0.1595555201818088242, -4.233934615764606946 ) ) ;
#24288 = ORIENTED_EDGE ( 'NONE', *, *, #9458, .T. ) ;
#24289 = EDGE_CURVE ( 'NONE', #27612, #53714, #29199, .T. ) ;
#24290 = DIRECTION ( 'NONE',  ( 0.000000000000000000, -0.6745969609292717939, -0.7381862504171902151 ) ) ;
#24291 = VERTEX_POINT ( 'NONE', #50237 ) ;
#24292 = DIRECTION ( 'NONE',  ( 0.000000000000000000, 0.000000000000000000, 1.000000000000000000 ) ) ;
#24293 = CARTESIAN_POINT ( 'NONE',  ( -17.66784097051423075, -6.970076762182745078, -11.56512672300377886 ) ) ;
#24294 = ORIENTED_EDGE ( 'NONE', *, *, #58173, .T. ) ;
#24295 = CARTESIAN_POINT ( 'NONE',  ( -35.00000000000000000, 2.772148766916116891, 11.86701198550357361 ) ) ;
#24296 = CARTESIAN_POINT ( 'NONE',  ( 3.152665057734086229, 4.725420687650732532, 6.378477742800449768 ) ) ;
#24297 = CARTESIAN_POINT ( 'NONE',  ( -35.00000000000000000, 11.73555825188283386, -4.983891302653459476 ) ) ;
#24298 = ORIENTED_EDGE ( 'NONE', *, *, #18030, .T. ) ;
#24299 = ORIENTED_EDGE ( 'NONE', *, *, #9834, .T. ) ;
#24300 = LINE ( 'NONE', #14628, #44946 ) ;
#24301 = EDGE_CURVE ( 'NONE', #60499, #16108, #21761, .T. ) ;
#24302 = AXIS2_PLACEMENT_3D ( 'NONE', #61331, #40384, #16112 ) ;
#24303 = EDGE_LOOP ( 'NONE', ( #18691, #59593, #52812, #25655 ) ) ;
#24304 = CARTESIAN_POINT ( 'NONE',  ( 9.687175622948609899, 25.00000000000000000, -0.5854820436212360146 ) ) ;
#24305 = CARTESIAN_POINT ( 'NONE',  ( 0.000000000000000000, -6.935703035393425253, 0.1051458740707039013 ) ) ;
#24306 = CARTESIAN_POINT ( 'NONE',  ( 3.100650473569754872, 7.074394303868267286, -3.562766772868470877 ) ) ;
#24307 = CARTESIAN_POINT ( 'NONE',  ( -3.472933359965475475, 10.12749893407059254, 6.449612554627071503 ) ) ;
#24308 = CARTESIAN_POINT ( 'NONE',  ( 13.36879067795435283, 11.08032463289294256, -4.612831250830367935 ) ) ;
#24309 = ORIENTED_EDGE ( 'NONE', *, *, #16259, .F. ) ;
#24310 = DIRECTION ( 'NONE',  ( 0.000000000000000000, 0.7617968321374856133, 0.6478160128811973895 ) ) ;
#24311 = DIRECTION ( 'NONE',  ( -1.000000000000000000, -0.000000000000000000, 0.000000000000000000 ) ) ;
#24312 = CIRCLE ( 'NONE', #9394, 5.000000000000000888 ) ;
#24313 = ADVANCED_FACE ( 'NONE', ( #30575 ), #4348, .T. ) ;
#24314 = VECTOR ( 'NONE', #10736, 1000.000000000000114 ) ;
#24315 = CARTESIAN_POINT ( 'NONE',  ( 0.2648978790185619880, -12.08224454301447182, -1.996248716311752824 ) ) ;
#24317 = CIRCLE ( 'NONE', #52997, 12.74999999999999822 ) ;
#24316 = CARTESIAN_POINT ( 'NONE',  ( 2.770579946183330922, -5.249166435139399844, 5.784075095088772045 ) ) ;
#24318 = CARTESIAN_POINT ( 'NONE',  ( 37.00000000000000711, -6.547236723513950807, 9.752226076388957665 ) ) ;
#24319 = CARTESIAN_POINT ( 'NONE',  ( 41.00000000000000711, -1.694065894508600678E-18, 0.000000000000000000 ) ) ;
#24320 = CARTESIAN_POINT ( 'NONE',  ( -37.00000000000000711, 0.000000000000000000, 0.000000000000000000 ) ) ;
#24321 = AXIS2_PLACEMENT_3D ( 'NONE', #28720, #44028, #49373 ) ;
#24322 = B_SPLINE_CURVE_WITH_KNOTS ( 'NONE', 3,
 ( #8330, #45217, #15280, #4334, #44538, #40888, #34570, #20610, #59867, #49883, #331, #24273, #61167, #55186, #14929, #60176, #55524, #10283, #30889 ),
 .UNSPECIFIED., .F., .F.,
 ( 4, 3, 3, 3, 3, 3, 4 ),
 ( 0.000000000000000000, 2.832085443540737559E-05, 4.217789847394784225E-05, 5.603488375046119081E-05, 6.989180858579295227E-05, 9.821094829918946873E-05, 0.0001178165571465047653 ),
 .UNSPECIFIED. ) ;
#24323 = ORIENTED_EDGE ( 'NONE', *, *, #34026, .T. ) ;
#24324 = CARTESIAN_POINT ( 'NONE',  ( 11.07172588725403273, -11.87906629146547210, -1.711250688108173712 ) ) ;
#24325 = ORIENTED_EDGE ( 'NONE', *, *, #26344, .T. ) ;
#24326 = CARTESIAN_POINT ( 'NONE',  ( 0.3109076770649007448, 1.896437056876628446, -12.11383728282218897 ) ) ;
#24327 = CARTESIAN_POINT ( 'NONE',  ( 2.000000000000001776, 0.000000000000000000, 0.000000000000000000 ) ) ;
#24328 = CARTESIAN_POINT ( 'NONE',  ( 0.000000000000000000, 1.754183803416544452, 6.711026108862249373 ) ) ;
#24329 = CARTESIAN_POINT ( 'NONE',  ( 2.245754705088790271, -1.216173395687026426, -7.538396044170202259 ) ) ;
#24330 = EDGE_LOOP ( 'NONE', ( #53421, #38017, #20318, #16500 ) ) ;
#24331 = ORIENTED_EDGE ( 'NONE', *, *, #30160, .F. ) ;
#24332 = VERTEX_POINT ( 'NONE', #35878 ) ;
#24333 = CARTESIAN_POINT ( 'NONE',  ( -27.20164183316780182, 2.642567708136682736, -0.1019800881472440052 ) ) ;
#24334 = ADVANCED_FACE ( 'NONE', ( #65180 ), #60514, .T. ) ;
#24336 = CARTESIAN_POINT ( 'NONE',  ( -35.00000000000000000, 9.512294188641000403, -6.891188680298720115 ) ) ;
#24335 = AXIS2_PLACEMENT_3D ( 'NONE', #18621, #44184, #35507 ) ;
#24337 = ORIENTED_EDGE ( 'NONE', *, *, #1365, .F. ) ;
#24338 = CARTESIAN_POINT ( 'NONE',  ( 2.835339799623976198, 5.783398714696559750, 5.281994181469010563 ) ) ;
#24339 = DIRECTION ( 'NONE',  ( -1.000000000000000000, -1.836970198721029688E-16, 0.000000000000000000 ) ) ;
#24340 = CARTESIAN_POINT ( 'NONE',  ( 0.3053067050349165812, 10.49978800868460915, 6.328522421120307939 ) ) ;
#24341 = CARTESIAN_POINT ( 'NONE',  ( -35.00000000000000000, -7.718225330433740261, -9.430788938294131896 ) ) ;
#24342 = VERTEX_POINT ( 'NONE', #60857 ) ;
#24343 = DIRECTION ( 'NONE',  ( 0.000000000000000000, 0.01356324068818000328, -0.9999080150203990547 ) ) ;
#24344 = CIRCLE ( 'NONE', #19042, 2.899999999999995470 ) ;
#24345 = CARTESIAN_POINT ( 'NONE',  ( -11.13812830829075473, -32.61426855637730426, -12.21782902109653612 ) ) ;
#24346 = CARTESIAN_POINT ( 'NONE',  ( -32.16141091265169649, 25.00000000000000000, 5.384978440493686236 ) ) ;
#24348 = EDGE_LOOP ( 'NONE', ( #4420, #63566, #5314, #56087 ) ) ;
#24347 = CARTESIAN_POINT ( 'NONE',  ( -35.00000000000000000, -12.49688848680886188, 2.527899948230592830 ) ) ;
#24349 = CARTESIAN_POINT ( 'NONE',  ( 3.152665057734040488, 0.000000000000000000, 0.000000000000000000 ) ) ;
#24350 = EDGE_LOOP ( 'NONE', ( #5221, #59453, #46739, #17273 ) ) ;
#24351 = CARTESIAN_POINT ( 'NONE',  ( 0.3610902822527257694, -6.364812822043094620, -10.49957835860569766 ) ) ;
#24352 = ORIENTED_EDGE ( 'NONE', *, *, #3815, .T. ) ;
#24353 = FACE_OUTER_BOUND ( 'NONE', #13464, .T. ) ;
#24354 = CARTESIAN_POINT ( 'NONE',  ( 13.24596223717851373, -11.31509987884708046, -4.002165216063023223 ) ) ;
#24355 = CIRCLE ( 'NONE', #29615, 5.000000000000000000 ) ;
#24356 = LINE ( 'NONE', #55272, #28738 ) ;
#24357 = CARTESIAN_POINT ( 'NONE',  ( 0.5547464869798260922, -6.433541106625019879, -10.53334899235177247 ) ) ;
#24358 = EDGE_CURVE ( 'NONE', #64321, #10113, #26025, .T. ) ;
#24359 = CARTESIAN_POINT ( 'NONE',  ( 0.2671309869109471657, 9.484919892054820778, 7.747281147400578938 ) ) ;
#24360 = CARTESIAN_POINT ( 'NONE',  ( -7.721880503586887379, -2.140633088631647585, -13.33031841795283512 ) ) ;
#24361 = CARTESIAN_POINT ( 'NONE',  ( 3.152665057733834431, -3.161213418913157991, 7.281573230474281289 ) ) ;
#24363 = ORIENTED_EDGE ( 'NONE', *, *, #52989, .T. ) ;
#24362 = DIRECTION ( 'NONE',  ( -1.000000000000000000, 0.000000000000000000, 0.000000000000000000 ) ) ;
#24364 = CIRCLE ( 'NONE', #8426, 12.18650000000000233 ) ;
#24365 = ORIENTED_EDGE ( 'NONE', *, *, #48152, .F. ) ;
#24366 = CYLINDRICAL_SURFACE ( 'NONE', #17875, 4.725920239717170901 ) ;
#24367 = ORIENTED_EDGE ( 'NONE', *, *, #296, .F. ) ;
#24368 = ORIENTED_EDGE ( 'NONE', *, *, #17934, .F. ) ;
#24369 = CARTESIAN_POINT ( 'NONE',  ( 0.2646305136544072623, 6.237419468587225069, -10.53923716745240391 ) ) ;
#24370 = CARTESIAN_POINT ( 'NONE',  ( -25.00000000000000355, -30.00000000000000000, -25.00000000000000000 ) ) ;
#24371 = AXIS2_PLACEMENT_3D ( 'NONE', #25925, #51206, #10950 ) ;
#24372 = CARTESIAN_POINT ( 'NONE',  ( -27.08429572838383947, -2.217805374070538349, 0.5764601019425888984 ) ) ;
#24373 = DIRECTION ( 'NONE',  ( 0.000000000000000000, 0.01356324068817991828, -0.9999080150203990547 ) ) ;
#24374 = CARTESIAN_POINT ( 'NONE',  ( -22.29290468048228036, 1.621390503294497742, -3.357740900108092674 ) ) ;
#24375 = DIRECTION ( 'NONE',  ( 0.000000000000000000, -0.01356324068817999114, 0.9999080150203989437 ) ) ;
#24376 = DIRECTION ( 'NONE',  ( 0.000000000000000000, 0.01356324068817991828, -0.9999080150203990547 ) ) ;
#24377 = EDGE_CURVE ( 'NONE', #416, #24479, #30903, .T. ) ;
#24378 = EDGE_CURVE ( 'NONE', #29292, #5936, #48918, .T. ) ;
#24379 = EDGE_LOOP ( 'NONE', ( #56344, #4084, #63610, #3458 ) ) ;
#24380 = CARTESIAN_POINT ( 'NONE',  ( -35.00000000000000000, 11.01837265713082203, -6.415447294506590126 ) ) ;
#24381 = CYLINDRICAL_SURFACE ( 'NONE', #15399, 7.499999999999988454 ) ;
#24382 = ADVANCED_FACE ( 'NONE', ( #9631 ), #51082, .F. ) ;
#24383 = CARTESIAN_POINT ( 'NONE',  ( -18.06762394718330711, -4.853757295686705220, 12.59799896500893190 ) ) ;
#24384 = ORIENTED_EDGE ( 'NONE', *, *, #36263, .T. ) ;
#24385 = CIRCLE ( 'NONE', #29689, 12.18650000000000411 ) ;
#24386 = CIRCLE ( 'NONE', #55342, 12.18650000000000055 ) ;
#24387 = EDGE_CURVE ( 'NONE', #46364, #46522, #5899, .T. ) ;
#24388 = AXIS2_PLACEMENT_3D ( 'NONE', #49669, #43681, #29063 ) ;
#24389 = CARTESIAN_POINT ( 'NONE',  ( 39.53125591517012083, -1.906753238347150381, -20.35939770057403564 ) ) ;
#24390 = FACE_OUTER_BOUND ( 'NONE', #36518, .T. ) ;
#24391 = VERTEX_POINT ( 'NONE', #10298 ) ;
#24393 = EDGE_CURVE ( 'NONE', #20149, #34412, #348, .T. ) ;
#24392 = CARTESIAN_POINT ( 'NONE',  ( 2.305787727787084407, 3.682701754025606178, -6.711944854845784292 ) ) ;
#24394 = CARTESIAN_POINT ( 'NONE',  ( 2.000000000000001776, -3.979254915827401540, 5.681598592373737766 ) ) ;
#24395 = DIRECTION ( 'NONE',  ( 0.9703875065674330003, 0.000000000000000000, 0.2415534870330798278 ) ) ;
#24396 = AXIS2_PLACEMENT_3D ( 'NONE', #28273, #48569, #3019 ) ;
#24397 = ADVANCED_FACE ( 'NONE', ( #42180 ), #57852, .T. ) ;
#24398 = DIRECTION ( 'NONE',  ( 1.000000000000000000, 0.000000000000000000, -0.000000000000000000 ) ) ;
#24399 = CARTESIAN_POINT ( 'NONE',  ( 6.361445718264521432, -4.355102044641763648, 25.00000000000000000 ) ) ;
#24400 = AXIS2_PLACEMENT_3D ( 'NONE', #15081, #20742, #35361 ) ;
#24401 = EDGE_LOOP ( 'NONE', ( #57891, #24944, #55469, #23006 ) ) ;
#24402 = CARTESIAN_POINT ( 'NONE',  ( -37.00000000000000711, 2.143131898507868297E-16, 1.750000000000000000 ) ) ;
#24403 = CARTESIAN_POINT ( 'NONE',  ( 0.3675815128205894289, -12.13672785388551389, 1.872154644482044938 ) ) ;
#24404 = LINE ( 'NONE', #54023, #8459 ) ;
#24405 = VERTEX_POINT ( 'NONE', #21261 ) ;
#24406 = CARTESIAN_POINT ( 'NONE',  ( 8.437200413559441614, 4.215340780676140930, 12.82799475126035560 ) ) ;
#24407 = DIRECTION ( 'NONE',  ( 0.5417962735734949131, 0.000000000000000000, -0.8405098440481674205 ) ) ;
#24408 = ORIENTED_EDGE ( 'NONE', *, *, #34224, .T. ) ;
#24409 = CIRCLE ( 'NONE', #3222, 5.000000000000000888 ) ;
#24410 = ORIENTED_EDGE ( 'NONE', *, *, #28061, .F. ) ;
#24411 = ORIENTED_EDGE ( 'NONE', *, *, #63802, .F. ) ;
#24412 = CARTESIAN_POINT ( 'NONE',  ( 0.3675815128205894289, 5.910255304480596550, -10.76447900494934196 ) ) ;
#24413 = VERTEX_POINT ( 'NONE', #7272 ) ;
#24414 = LINE ( 'NONE', #4149, #18578 ) ;
#24415 = DIRECTION ( 'NONE',  ( 1.000000000000000000, -0.000000000000000000, -0.000000000000000000 ) ) ;
#24416 = CYLINDRICAL_SURFACE ( 'NONE', #11021, 5.000000000000000888 ) ;
#24417 = CARTESIAN_POINT ( 'NONE',  ( -22.46225619532223305, -2.255146441673796964, -3.586917175123550017 ) ) ;
#24418 = CARTESIAN_POINT ( 'NONE',  ( -10.50558643126015923, -29.12101583629321055, 8.365681325885642394 ) ) ;
#24419 = CARTESIAN_POINT ( 'NONE',  ( 2.000000000000001776, -6.812627895098285258, 0.04423456934719675882 ) ) ;
#24421 = ORIENTED_EDGE ( 'NONE', *, *, #33784, .T. ) ;
#24420 = CARTESIAN_POINT ( 'NONE',  ( 2.241509619876137283, -7.634391113243452764, -0.03828218718778049479 ) ) ;
#24422 = CARTESIAN_POINT ( 'NONE',  ( -22.27711653538342773, 2.191780254295688568, 2.958138731383619380 ) ) ;
#24423 = ORIENTED_EDGE ( 'NONE', *, *, #47234, .F. ) ;
#24424 = CARTESIAN_POINT ( 'NONE',  ( 2.305787727787084407, -5.756228004061490822, 5.047606869483037606 ) ) ;
#24425 = ORIENTED_EDGE ( 'NONE', *, *, #15098, .F. ) ;
#24426 = ORIENTED_EDGE ( 'NONE', *, *, #15449, .F. ) ;
#24427 = DIRECTION ( 'NONE',  ( 0.000000000000000000, 1.000000000000000000, 0.000000000000000000 ) ) ;
#24428 = CARTESIAN_POINT ( 'NONE',  ( -16.02805653289875920, -29.20913999211457224, 10.57890313540342220 ) ) ;
#24429 = DIRECTION ( 'NONE',  ( 0.000000000000000000, 0.000000000000000000, 1.000000000000000000 ) ) ;
#24430 = EDGE_CURVE ( 'NONE', #5232, #27547, #27557, .T. ) ;
#24431 = CIRCLE ( 'NONE', #45653, 5.000000000000000888 ) ;
#24432 = AXIS2_PLACEMENT_3D ( 'NONE', #39420, #29760, #59721 ) ;
#24433 = CARTESIAN_POINT ( 'NONE',  ( 23.55819837055134158, -3.414313941384615081, 11.50760599575436949 ) ) ;
#24434 = CARTESIAN_POINT ( 'NONE',  ( 5.520433897694421610, 0.004666464468078328209, -0.01432141647227113193 ) ) ;
#24435 = DIRECTION ( 'NONE',  ( -1.000000000000000000, 0.000000000000000000, -0.000000000000000000 ) ) ;
#24436 = ORIENTED_EDGE ( 'NONE', *, *, #39937, .T. ) ;
#24437 = ORIENTED_EDGE ( 'NONE', *, *, #12276, .T. ) ;
#24438 = CARTESIAN_POINT ( 'NONE',  ( 2.000000000000001776, -4.444115772890149252, 5.163689623839303522 ) ) ;
#24439 = VERTEX_POINT ( 'NONE', #31564 ) ;
#24440 = ORIENTED_EDGE ( 'NONE', *, *, #7151, .T. ) ;
#24441 = B_SPLINE_CURVE_WITH_KNOTS ( 'NONE', 3,
 ( #57054, #21814, #32723, #42711, #22115, #57716, #53033, #62038, #58360, #12780, #62343, #33071, #42371, #17134, #46733, #37408 ),
 .UNSPECIFIED., .F., .F.,
 ( 4, 3, 3, 3, 3, 4 ),
 ( 8.415671965864807093E-19, 0.0003017745587525263312, 0.0006035491769808766678, 0.0009053241094668192839, 0.001207275924540517119, 0.001510325902534023941 ),
 .UNSPECIFIED. ) ;
#24442 = CARTESIAN_POINT ( 'NONE',  ( 2.241509619876138615, -1.363398699156099125, 7.511759925807393934 ) ) ;
#24443 = CARTESIAN_POINT ( 'NONE',  ( 0.2759803524722239110, 0.1894460813477723549, -12.24828167798666456 ) ) ;
#24444 = DIRECTION ( 'NONE',  ( -0.000000000000000000, -0.000000000000000000, -1.000000000000000000 ) ) ;
#24446 = CIRCLE ( 'NONE', #15942, 5.000000000000000888 ) ;
#24445 = CARTESIAN_POINT ( 'NONE',  ( 2.249013661412229581, 7.636012530783587771, 0.1200550008339432706 ) ) ;
#24447 = DIRECTION ( 'NONE',  ( 0.6147887355352468219, -0.7886918350401329603, 0.000000000000000000 ) ) ;
#24448 = ADVANCED_FACE ( 'NONE', ( #47855 ), #51867, .T. ) ;
#24449 = CARTESIAN_POINT ( 'NONE',  ( 26.34661844826604593, -13.08594712317289321, 3.317828791472332117 ) ) ;
#24450 = VECTOR ( 'NONE', #64713, 1000.000000000000000 ) ;
#24451 = VERTEX_POINT ( 'NONE', #16934 ) ;
#24452 =( BOUNDED_SURFACE ( )  B_SPLINE_SURFACE ( 3, 1, ( 
 ( #33286, #53589 ),
 ( #18981, #3047 ),
 ( #39243, #49263 ),
 ( #44548, #64830 ) ),
 .UNSPECIFIED., .F., .F., .F. ) 
 B_SPLINE_SURFACE_WITH_KNOTS ( ( 4, 4 ),
 ( 2, 2 ),
 ( 0.000000000000000000, 1.000000000000000000 ),
 ( 0.000000000000000000, 1.000000000000000000 ),
 .UNSPECIFIED. ) 
 GEOMETRIC_REPRESENTATION_ITEM ( )  RATIONAL_B_SPLINE_SURFACE ( (
 ( 1.000000000000000000, 1.000000000000000000),
 ( 0.9932032654565553509, 0.8386279382598740284),
 ( 0.9932032654565553509, 0.8386279382598740284),
 ( 1.000000000000000000, 1.000000000000000000) ) ) 
 REPRESENTATION_ITEM ( '' )  SURFACE ( )  );
#24453 = EDGE_CURVE ( 'NONE', #57089, #19006, #25306, .T. ) ;
#24454 = ORIENTED_EDGE ( 'NONE', *, *, #61949, .T. ) ;
#24455 = EDGE_CURVE ( 'NONE', #38649, #62456, #16285, .T. ) ;
#24456 = CARTESIAN_POINT ( 'NONE',  ( 35.00000000000000000, -10.91072401419414462, -5.428340790341669830 ) ) ;
#24457 = DIRECTION ( 'NONE',  ( 1.000000000000000000, -0.000000000000000000, -0.000000000000000000 ) ) ;
#24458 = DIRECTION ( 'NONE',  ( 0.000000000000000000, -0.01356324068817992001, 0.9999080150203990547 ) ) ;
#24459 = CARTESIAN_POINT ( 'NONE',  ( 2.000000000000001776, 6.883677378339481123, -0.8544109087185395301 ) ) ;
#24460 = CARTESIAN_POINT ( 'NONE',  ( -35.00000000000000000, 3.307597835713244283, 12.31350058095524247 ) ) ;
#24461 = ADVANCED_FACE ( 'NONE', ( #1332 ), #11295, .T. ) ;
#24462 = CARTESIAN_POINT ( 'NONE',  ( 6.918530584243898218, -8.212880376810627325, -10.72188286460056439 ) ) ;
#24463 = EDGE_CURVE ( 'NONE', #8336, #52191, #50804, .T. ) ;
#24464 = CARTESIAN_POINT ( 'NONE',  ( 2.241449424704146320, 5.808712090826680274, -4.954182807723280568 ) ) ;
#24465 = CARTESIAN_POINT ( 'NONE',  ( 35.00000000000000000, 10.63508530065521640, -4.986700593229742573 ) ) ;
#24466 = CARTESIAN_POINT ( 'NONE',  ( 9.575800908719084958, -11.95193887484098028, -1.072919909436247154 ) ) ;
#24467 = AXIS2_PLACEMENT_3D ( 'NONE', #26154, #21492, #6860 ) ;
#24468 = ORIENTED_EDGE ( 'NONE', *, *, #50266, .T. ) ;
#24469 = LINE ( 'NONE', #64060, #46284 ) ;
#24470 = CARTESIAN_POINT ( 'NONE',  ( 5.516018279890452902, 0.004525000489649935558, -0.005042957932159086720 ) ) ;
#24471 = DIRECTION ( 'NONE',  ( 0.000000000000000000, -0.01356324068817998593, 0.9999080150203990547 ) ) ;
#24472 = ADVANCED_FACE ( 'NONE', ( #6005 ), #62163, .T. ) ;
#24473 = AXIS2_PLACEMENT_3D ( 'NONE', #1920, #58440, #33150 ) ;
#24474 = CIRCLE ( 'NONE', #56334, 12.74999999999999822 ) ;
#24475 = AXIS2_PLACEMENT_3D ( 'NONE', #38056, #33415, #43050 ) ;
#24476 = ADVANCED_FACE ( 'NONE', ( #12267 ), #41535, .T. ) ;
#24477 = CARTESIAN_POINT ( 'NONE',  ( -14.34460386949599631, -34.50739325218108888, -8.058841881767305537 ) ) ;
#24478 = CARTESIAN_POINT ( 'NONE',  ( 2.241311220309555097, -5.907514893712957793, 4.835827934491001123 ) ) ;
#24479 = VERTEX_POINT ( 'NONE', #1974 ) ;
#24480 = CARTESIAN_POINT ( 'NONE',  ( 5.514970785353741078, 0.004532877335078317783, -0.001326349372336594603 ) ) ;
#24481 = CARTESIAN_POINT ( 'NONE',  ( 2.931247277082558611, 6.618030015945723044, 4.248542803114288446 ) ) ;
#24483 = EDGE_CURVE ( 'NONE', #41989, #26974, #57180, .T. ) ;
#24482 = CARTESIAN_POINT ( 'NONE',  ( 1.749504362522309897, -27.84680466544767796, -12.51149646090675915 ) ) ;
#24484 = ORIENTED_EDGE ( 'NONE', *, *, #53760, .T. ) ;
#24485 = CARTESIAN_POINT ( 'NONE',  ( 2.305787727787084407, 7.249469779319909435, 2.461236246751095536 ) ) ;
#24486 = CARTESIAN_POINT ( 'NONE',  ( 2.000000000000001776, 0.000000000000000000, 0.000000000000000000 ) ) ;
#24487 = CARTESIAN_POINT ( 'NONE',  ( -22.29195009621226475, -1.030739959031446107, -3.580440466953083156 ) ) ;
#24488 = DIRECTION ( 'NONE',  ( 1.000000000000000000, 0.000000000000000000, -0.000000000000000000 ) ) ;
#24489 = CARTESIAN_POINT ( 'NONE',  ( -27.08485414902839494, 2.215517476308469291, 0.5917839443972277014 ) ) ;
#24490 = VECTOR ( 'NONE', #56681, 1000.000000000000114 ) ;
#24491 = CIRCLE ( 'NONE', #25598, 7.499999999999988454 ) ;
#24492 = DIRECTION ( 'NONE',  ( 1.000000000000000000, 0.000000000000000000, 0.000000000000000000 ) ) ;
#24493 = ORIENTED_EDGE ( 'NONE', *, *, #53609, .T. ) ;
#24494 = VECTOR ( 'NONE', #50732, 1000.000000000000114 ) ;
#24495 = CARTESIAN_POINT ( 'NONE',  ( 2.268878695253352618, -7.231932316093180546, 2.474564429974472901 ) ) ;
#24496 = CIRCLE ( 'NONE', #36159, 6.936499999999989008 ) ;
#24497 = CARTESIAN_POINT ( 'NONE',  ( 35.00000000000000000, -7.718225330433870823, -9.430788938294027091 ) ) ;
#24498 = CARTESIAN_POINT ( 'NONE',  ( 37.00000000000000711, -8.017674001891711200, 9.913596905230193101 ) ) ;
#24499 = LINE ( 'NONE', #29479, #56471 ) ;
#24500 = DIRECTION ( 'NONE',  ( 0.000000000000000000, 0.01356324068817998940, -0.9999080150203990547 ) ) ;
#24501 = CARTESIAN_POINT ( 'NONE',  ( -35.00000000000000000, -11.91791701451264629, -2.544412758415973030 ) ) ;
#24502 = AXIS2_PLACEMENT_3D ( 'NONE', #5424, #91, #25361 ) ;
#24503 = CARTESIAN_POINT ( 'NONE',  ( -25.00000000000000355, -9.999999999999998224, 25.00000000000000000 ) ) ;
#24504 = CARTESIAN_POINT ( 'NONE',  ( 2.288423627606496424, 1.169285315516220169, -7.560204962262810469 ) ) ;
#24505 = VERTEX_POINT ( 'NONE', #61828 ) ;
#24506 = EDGE_LOOP ( 'NONE', ( #19274, #5018, #55955, #64851 ) ) ;
#24507 = CARTESIAN_POINT ( 'NONE',  ( -18.24855926006501505, -5.449082428673613698, -10.69225419630004481 ) ) ;
#24508 = VECTOR ( 'NONE', #49896, 1000.000000000000000 ) ;
#24509 = VERTEX_POINT ( 'NONE', #56872 ) ;
#24510 = CARTESIAN_POINT ( 'NONE',  ( 3.423896178748679020, -10.94279856996580413, -7.910751437345123982 ) ) ;
#24511 = EDGE_CURVE ( 'NONE', #62855, #22570, #33791, .T. ) ;
#24512 = EDGE_CURVE ( 'NONE', #15438, #11272, #56105, .T. ) ;
#24513 = CARTESIAN_POINT ( 'NONE',  ( -17.83419946441818027, -9.720786832536937538, 9.367833439828872955 ) ) ;
#24514 = ORIENTED_EDGE ( 'NONE', *, *, #19629, .F. ) ;
#24515 = DIRECTION ( 'NONE',  ( -1.000000000000000000, -0.000000000000000000, 0.000000000000000000 ) ) ;
#24516 = CARTESIAN_POINT ( 'NONE',  ( 12.64346310766591586, 9.915289356383874875, -6.770812359651990242 ) ) ;
#24517 = DIRECTION ( 'NONE',  ( -1.000000000000000000, -1.836970198721029688E-16, -0.000000000000000000 ) ) ;
#24518 = ORIENTED_EDGE ( 'NONE', *, *, #57008, .T. ) ;
#24519 = VERTEX_POINT ( 'NONE', #46871 ) ;
#24520 = DIRECTION ( 'NONE',  ( -1.000000000000000000, 0.000000000000000000, 0.000000000000000000 ) ) ;
#24521 = DIRECTION ( 'NONE',  ( 1.000000000000000000, -0.000000000000000000, 0.000000000000000000 ) ) ;
#24522 = EDGE_CURVE ( 'NONE', #30009, #37953, #55021, .T. ) ;
#24523 = ORIENTED_EDGE ( 'NONE', *, *, #9414, .T. ) ;
#24524 = FACE_OUTER_BOUND ( 'NONE', #39841, .T. ) ;
#24525 = EDGE_LOOP ( 'NONE', ( #4967, #62507, #28292, #40915 ) ) ;
#24526 = CARTESIAN_POINT ( 'NONE',  ( 0.2646305136544072623, -6.237419468587005689, -10.53923716745253358 ) ) ;
#24527 = DIRECTION ( 'NONE',  ( -1.000000000000000000, 0.000000000000000000, 0.000000000000000000 ) ) ;
#24528 = CIRCLE ( 'NONE', #7533, 6.936499999999991672 ) ;
#24529 = VECTOR ( 'NONE', #41810, 1000.000000000000000 ) ;
#24530 = CARTESIAN_POINT ( 'NONE',  ( 1.000000000000000888, -6.586971819220345026, 3.586335490831356054 ) ) ;
#24531 = CARTESIAN_POINT ( 'NONE',  ( 0.2651627923886329397, -10.64925183219497740, 6.046629261473301042 ) ) ;
#24532 = AXIS2_PLACEMENT_3D ( 'NONE', #1297, #36848, #26542 ) ;
#24533 = EDGE_CURVE ( 'NONE', #26974, #40555, #31881, .T. ) ;
#24534 = CARTESIAN_POINT ( 'NONE',  ( -14.11589373245165469, 8.250315036047107142, -10.68561190601526256 ) ) ;
#24535 = EDGE_LOOP ( 'NONE', ( #33110, #43, #32992, #64185 ) ) ;
#24536 = CARTESIAN_POINT ( 'NONE',  ( 2.305787727787084851, -1.493241775258474124, 7.508843116234150905 ) ) ;
#24537 = CIRCLE ( 'NONE', #7382, 4.999999999999999112 ) ;
#24538 = CARTESIAN_POINT ( 'NONE',  ( 0.2651627682582904932, 7.803986935114140877, -9.437482589529897936 ) ) ;
#24539 = DIRECTION ( 'NONE',  ( 1.000000000000000000, 0.000000000000000000, -0.000000000000000000 ) ) ;
#24540 = ADVANCED_FACE ( 'NONE', ( #47217 ), #24271, .F. ) ;
#24541 = CYLINDRICAL_SURFACE ( 'NONE', #16823, 4.999999999999999112 ) ;
#24542 = CARTESIAN_POINT ( 'NONE',  ( -20.74400292461320916, 13.15690609773952602, -3.073985401093241254 ) ) ;
#24543 = CARTESIAN_POINT ( 'NONE',  ( 24.18616158388540782, -2.148571468477003865, 13.33263367692836177 ) ) ;
#24544 = DIRECTION ( 'NONE',  ( -1.000000000000000000, 0.000000000000000000, 0.000000000000000000 ) ) ;
#24545 = CARTESIAN_POINT ( 'NONE',  ( -35.00000000000000000, -8.766823244862047559, 7.817610399097479679 ) ) ;
#24546 = CARTESIAN_POINT ( 'NONE',  ( 0.3401186441510242187, 9.233880480307307792, 8.081824149807733448 ) ) ;
#24547 = CIRCLE ( 'NONE', #44752, 5.000000000000000888 ) ;
#24548 = ORIENTED_EDGE ( 'NONE', *, *, #62647, .T. ) ;
#24549 = CIRCLE ( 'NONE', #61703, 12.18650000000000055 ) ;
#24550 = AXIS2_PLACEMENT_3D ( 'NONE', #58311, #38008, #22743 ) ;
#24551 = VERTEX_POINT ( 'NONE', #3943 ) ;
#24552 = CARTESIAN_POINT ( 'NONE',  ( 0.2646305136544072623, -12.03696649559616283, 2.256625640822276235 ) ) ;
#24553 = CARTESIAN_POINT ( 'NONE',  ( 2.276198483117255478, -7.501576331167725264, -1.479169956994139890 ) ) ;
#24554 = ADVANCED_FACE ( 'NONE', ( #13262 ), #37870, .T. ) ;
#24555 = CARTESIAN_POINT ( 'NONE',  ( 35.00000000000000000, 4.705694406421931860E-17, -3.469127814946512892E-15 ) ) ;
#24556 = FACE_OUTER_BOUND ( 'NONE', #24330, .T. ) ;
#24557 = CARTESIAN_POINT ( 'NONE',  ( 37.00000000000000711, -11.59095880812006385, 1.903127969211307224 ) ) ;
#24558 = ORIENTED_EDGE ( 'NONE', *, *, #51591, .T. ) ;
#24559 = CARTESIAN_POINT ( 'NONE',  ( 145.1370849898475797, 3.309064568108273190E-14, 0.000000000000000000 ) ) ;
#24561 = AXIS2_PLACEMENT_3D ( 'NONE', #39826, #13880, #29509 ) ;
#24560 = CARTESIAN_POINT ( 'NONE',  ( -29.92777678363736626, -3.750539801530011985, -11.39883551934752681 ) ) ;
#24562 = DIRECTION ( 'NONE',  ( 1.000000000000000000, 0.000000000000000000, 0.000000000000000000 ) ) ;
#24563 = CARTESIAN_POINT ( 'NONE',  ( 1.283627346226435373, 2.725559306498919643, 12.28700367512541014 ) ) ;
#24564 = EDGE_CURVE ( 'NONE', #34567, #8663, #63503, .T. ) ;
#24565 = ADVANCED_FACE ( 'NONE', ( #54148 ), #48565, .F. ) ;
#24566 = AXIS2_PLACEMENT_3D ( 'NONE', #33537, #28867, #29506 ) ;
#24567 = CYLINDRICAL_SURFACE ( 'NONE', #48901, 6.936499999999988120 ) ;
#24568 = ORIENTED_EDGE ( 'NONE', *, *, #23439, .F. ) ;
#24570 = EDGE_CURVE ( 'NONE', #16604, #31040, #38859, .T. ) ;
#24569 = CARTESIAN_POINT ( 'NONE',  ( -35.00000000000000000, 0.000000000000000000, 0.000000000000000000 ) ) ;
#24571 = EDGE_LOOP ( 'NONE', ( #59119, #51281, #2574, #12081 ) ) ;
#24572 = CIRCLE ( 'NONE', #43694, 12.18650000000000233 ) ;
#24573 = DIRECTION ( 'NONE',  ( 0.000000000000000000, 1.000000000000000000, 0.000000000000000000 ) ) ;
#24574 = CARTESIAN_POINT ( 'NONE',  ( -36.00000000000000711, 5.556331110570408960, 11.47561260193578825 ) ) ;
#24575 = CARTESIAN_POINT ( 'NONE',  ( -2.816255946208519934, -7.711081843936708147, 11.08213906273405769 ) ) ;
#24576 = LINE ( 'NONE', #28918, #59624 ) ;
#24577 = CIRCLE ( 'NONE', #11791, 12.75000000000000178 ) ;
#24578 = CIRCLE ( 'NONE', #138, 2.899999999999995914 ) ;
#24579 = VECTOR ( 'NONE', #63088, 1000.000000000000000 ) ;
#24580 = ORIENTED_EDGE ( 'NONE', *, *, #25110, .T. ) ;
#24581 = ORIENTED_EDGE ( 'NONE', *, *, #30455, .F. ) ;
#24582 = CARTESIAN_POINT ( 'NONE',  ( 2.000000000000001776, 5.396716205731493687, -4.158041573745044239 ) ) ;
#24583 = ORIENTED_EDGE ( 'NONE', *, *, #11458, .T. ) ;
#24584 = CARTESIAN_POINT ( 'NONE',  ( 1.948354844646968731, 6.595573209513781343, 9.982942661979748777 ) ) ;
#24585 = DIRECTION ( 'NONE',  ( 1.000000000000000000, 0.000000000000000000, 0.000000000000000000 ) ) ;
#24586 = CARTESIAN_POINT ( 'NONE',  ( -35.00000000000000000, 11.44858830469740241, -2.627174906296955381 ) ) ;
#24587 = LINE ( 'NONE', #59508, #19460 ) ;
#24588 = DIRECTION ( 'NONE',  ( 1.000000000000000000, 0.000000000000000000, 0.000000000000000000 ) ) ;
#24589 = LINE ( 'NONE', #44867, #8371 ) ;
#24590 = CARTESIAN_POINT ( 'NONE',  ( -18.77940254910617668, -11.98723174400094393, 0.6435659898533969692 ) ) ;
#24591 = ORIENTED_EDGE ( 'NONE', *, *, #42228, .F. ) ;
#24592 = VERTEX_POINT ( 'NONE', #48207 ) ;
#24593 = VERTEX_POINT ( 'NONE', #33205 ) ;
#24594 = CARTESIAN_POINT ( 'NONE',  ( 1.633930747253001581, -2.909970528251876853, -12.36466318969099198 ) ) ;
#24595 = VECTOR ( 'NONE', #9798, 1000.000000000000000 ) ;
#24596 = CIRCLE ( 'NONE', #58555, 5.000000000000000888 ) ;
#24597 = DIRECTION ( 'NONE',  ( -1.000000000000000000, 0.000000000000000000, 0.000000000000000000 ) ) ;
#24598 = EDGE_CURVE ( 'NONE', #18920, #48103, #7268, .T. ) ;
#24599 = ORIENTED_EDGE ( 'NONE', *, *, #39092, .T. ) ;
#24600 = AXIS2_PLACEMENT_3D ( 'NONE', #19158, #50086, #4545 ) ;
#24601 = FACE_BOUND ( 'NONE', #4336, .T. ) ;
#24602 = ADVANCED_FACE ( 'NONE', ( #63450 ), #28873, .F. ) ;
#24603 = ORIENTED_EDGE ( 'NONE', *, *, #7803, .F. ) ;
#24604 = CARTESIAN_POINT ( 'NONE',  ( 2.241537034860906275, 6.614004440763098458, -3.813147095850915491 ) ) ;
#24605 = FACE_OUTER_BOUND ( 'NONE', #16495, .T. ) ;
#24606 = CARTESIAN_POINT ( 'NONE',  ( 2.844750968615830100, 7.242618984642876789, -2.990088422897238196 ) ) ;
#24607 = ORIENTED_EDGE ( 'NONE', *, *, #37642, .F. ) ;
#24608 = AXIS2_PLACEMENT_3D ( 'NONE', #44614, #24043, #33359 ) ;
#24609 = EDGE_LOOP ( 'NONE', ( #44121, #30260, #37335, #52992 ) ) ;
#24610 = CARTESIAN_POINT ( 'NONE',  ( 2.899286259009682620, -6.972741252562078884, 3.614094927251911837 ) ) ;
#24611 = EDGE_LOOP ( 'NONE', ( #58543, #20237, #64500, #53806 ) ) ;
#24612 = ORIENTED_EDGE ( 'NONE', *, *, #27123, .F. ) ;
#24613 = EDGE_CURVE ( 'NONE', #63532, #58825, #23176, .T. ) ;
#24614 = ORIENTED_EDGE ( 'NONE', *, *, #64139, .F. ) ;
#24615 = B_SPLINE_CURVE_WITH_KNOTS ( 'NONE', 3,
 ( #25435, #39749, #45384, #514, #45071, #41052, #19805, #14775, #55712, #61333, #25775, #20121, #15122, #19480, #36048, #50405, #65007, #55037, #14459, #56348, #34734, #10146 ),
 .UNSPECIFIED., .F., .F.,
 ( 4, 3, 3, 3, 3, 3, 3, 4 ),
 ( 0.000000000000000000, 4.455945684386757038E-05, 6.636307477204008278E-05, 8.816671873158727604E-05, 0.0001099660380492610995, 0.0001317545563165303715, 0.0001762613022895040686, 0.0001867992666138395923 ),
 .UNSPECIFIED. ) ;
#24616 = ORIENTED_EDGE ( 'NONE', *, *, #63921, .T. ) ;
#24617 = CARTESIAN_POINT ( 'NONE',  ( 35.00000000000000000, 3.640372113593551173, -12.21925492305363470 ) ) ;
#24618 = CARTESIAN_POINT ( 'NONE',  ( -7.613843340947280325, -31.56230424472762053, -13.96789312046469789 ) ) ;
#24619 = DIRECTION ( 'NONE',  ( -0.000000000000000000, -1.000000000000000000, -0.000000000000000000 ) ) ;
#24620 = CARTESIAN_POINT ( 'NONE',  ( -35.00000000000000000, 9.677500615117999416, -6.657191900728212985 ) ) ;
#24621 = VERTEX_POINT ( 'NONE', #7960 ) ;
#24622 = CARTESIAN_POINT ( 'NONE',  ( 1.719304012338200849, 11.38834240361387096, 5.690355757826642602 ) ) ;
#24623 = AXIS2_PLACEMENT_3D ( 'NONE', #55038, #6814, #21098 ) ;
#24624 = ORIENTED_EDGE ( 'NONE', *, *, #37551, .T. ) ;
#24625 = DIRECTION ( 'NONE',  ( -1.000000000000000000, 0.000000000000000000, 0.000000000000000000 ) ) ;
#24626 = DIRECTION ( 'NONE',  ( 0.000000000000000000, -0.01356324068817991828, 0.9999080150203990547 ) ) ;
#24627 = CIRCLE ( 'NONE', #27805, 6.936499999999989896 ) ;
#24628 = EDGE_CURVE ( 'NONE', #10393, #6306, #59309, .T. ) ;
#24629 = ORIENTED_EDGE ( 'NONE', *, *, #63792, .F. ) ;
#24630 = CARTESIAN_POINT ( 'NONE',  ( 0.9296196016852207311, 9.812579935705901590, -7.691217109781619321 ) ) ;
#24631 = CARTESIAN_POINT ( 'NONE',  ( -37.00000000000000711, 2.216820770815248309, -11.53507381115581332 ) ) ;
#24632 = DIRECTION ( 'NONE',  ( -1.000000000000000000, 0.000000000000000000, 0.000000000000000000 ) ) ;
#24633 = ADVANCED_FACE ( 'NONE', ( #59458 ), #39164, .T. ) ;
#24634 = ORIENTED_EDGE ( 'NONE', *, *, #4285, .F. ) ;
#24635 = AXIS2_PLACEMENT_3D ( 'NONE', #4564, #24833, #29793 ) ;
#24636 = AXIS2_PLACEMENT_3D ( 'NONE', #58491, #47528, #17918 ) ;
#24637 = CIRCLE ( 'NONE', #61785, 5.000000000000000888 ) ;
#24638 = ORIENTED_EDGE ( 'NONE', *, *, #22444, .T. ) ;
#24639 = CARTESIAN_POINT ( 'NONE',  ( 2.259025283528086181, -7.639069972920485618, 0.1366755880739445317 ) ) ;
#24640 = ORIENTED_EDGE ( 'NONE', *, *, #28667, .F. ) ;
#24641 = DIRECTION ( 'NONE',  ( 1.000000000000000000, 0.000000000000000000, 0.000000000000000000 ) ) ;
#24642 = CARTESIAN_POINT ( 'NONE',  ( 1.633930747250580184, 10.17701904908664368, 7.601388527387680227 ) ) ;
#24643 = CARTESIAN_POINT ( 'NONE',  ( -2.534465382079141182, -26.62629929685679997, 16.11622222973024421 ) ) ;
#24644 = CARTESIAN_POINT ( 'NONE',  ( 2.844750968615600506, 4.202329849280348029, 6.613363922490565372 ) ) ;
#24645 = CARTESIAN_POINT ( 'NONE',  ( 12.60640452496583030, 11.71824542652569079, -2.591698231487439497 ) ) ;
#24646 = VERTEX_POINT ( 'NONE', #48845 ) ;
#24647 = CARTESIAN_POINT ( 'NONE',  ( -37.00000000000000711, -3.916263239775430005, 11.07407352312211302 ) ) ;
#24648 = FACE_OUTER_BOUND ( 'NONE', #58744, .T. ) ;
#24649 = FACE_OUTER_BOUND ( 'NONE', #7165, .T. ) ;
#24650 = VECTOR ( 'NONE', #28378, 1000.000000000000000 ) ;
#24651 = ADVANCED_FACE ( 'NONE', ( #2970 ), #21028, .T. ) ;
#24652 = AXIS2_PLACEMENT_3D ( 'NONE', #5110, #8787, #29383 ) ;
#24653 = EDGE_CURVE ( 'NONE', #18772, #52659, #53831, .T. ) ;
#24654 =( BOUNDED_SURFACE ( )  B_SPLINE_SURFACE ( 3, 1, ( 
 ( #13591, #63805 ),
 ( #13912, #3667 ),
 ( #23257, #23931 ),
 ( #34204, #53856 ) ),
 .UNSPECIFIED., .F., .F., .F. ) 
 B_SPLINE_SURFACE_WITH_KNOTS ( ( 4, 4 ),
 ( 2, 2 ),
 ( 0.000000000000000000, 1.000000000000000000 ),
 ( 0.000000000000000000, 1.000000000000000000 ),
 .UNSPECIFIED. ) 
 GEOMETRIC_REPRESENTATION_ITEM ( )  RATIONAL_B_SPLINE_SURFACE ( (
 ( 1.000000000000000000, 1.000000000000000000),
 ( 0.9257577194822556033, 0.9980522942447415113),
 ( 0.9257577194822556033, 0.9980522942447415113),
 ( 1.000000000000000000, 1.000000000000000000) ) ) 
 REPRESENTATION_ITEM ( '' )  SURFACE ( )  );
#24655 = CARTESIAN_POINT ( 'NONE',  ( 0.3006302518452063088, -12.10891847026070245, -1.905681544119362636 ) ) ;
#24656 = AXIS2_PLACEMENT_3D ( 'NONE', #28946, #49255, #39235 ) ;
#24658 = ADVANCED_FACE ( 'NONE', ( #59152 ), #13563, .T. ) ;
#24657 = CARTESIAN_POINT ( 'NONE',  ( 2.000000000000001776, -4.570217215903314312, -5.218059682435693958 ) ) ;
#24659 = CARTESIAN_POINT ( 'NONE',  ( 5.520433897694421610, 0.0005131706886599361186, -0.01505375422439068044 ) ) ;
#24660 = CARTESIAN_POINT ( 'NONE',  ( -27.45775109278351067, 25.00000000000000000, -8.471355351200609007 ) ) ;
#24661 = EDGE_CURVE ( 'NONE', #46638, #61418, #45471, .T. ) ;
#24662 = ORIENTED_EDGE ( 'NONE', *, *, #57584, .F. ) ;
#24663 = CARTESIAN_POINT ( 'NONE',  ( -37.00000000000000711, -6.036400161834495570, -10.07641281632183983 ) ) ;
#24664 = ORIENTED_EDGE ( 'NONE', *, *, #29765, .T. ) ;
#24666 =( BOUNDED_SURFACE ( )  B_SPLINE_SURFACE ( 3, 1, ( 
 ( #8696, #28976 ),
 ( #34280, #54592 ),
 ( #29299, #49593 ),
 ( #44566, #10312 ) ),
 .UNSPECIFIED., .F., .F., .F. ) 
 B_SPLINE_SURFACE_WITH_KNOTS ( ( 4, 4 ),
 ( 2, 2 ),
 ( 0.000000000000000000, 1.000000000000000000 ),
 ( 0.000000000000000000, 1.000000000000000000 ),
 .UNSPECIFIED. ) 
 GEOMETRIC_REPRESENTATION_ITEM ( )  RATIONAL_B_SPLINE_SURFACE ( (
 ( 1.000000000000000000, 1.000000000000000000),
 ( 0.9932032654565553509, 0.8386279382598736953),
 ( 0.9932032654565553509, 0.8386279382598736953),
 ( 1.000000000000000000, 1.000000000000000000) ) ) 
 REPRESENTATION_ITEM ( '' )  SURFACE ( )  );
#24665 = FACE_OUTER_BOUND ( 'NONE', #46579, .T. ) ;
#24667 = CARTESIAN_POINT ( 'NONE',  ( 16.78263030916553333, 25.00000000000000000, 5.836879698929882565 ) ) ;
#24668 = CARTESIAN_POINT ( 'NONE',  ( 0.2651627923886312188, 6.046629261473340122, 10.64925183219496319 ) ) ;
#24669 = CARTESIAN_POINT ( 'NONE',  ( 2.241352910868908754, 3.744764251556992996, 6.652881166698525028 ) ) ;
#24670 = ORIENTED_EDGE ( 'NONE', *, *, #33623, .F. ) ;
#24671 = CIRCLE ( 'NONE', #8868, 5.000000000000000888 ) ;
#24672 = ORIENTED_EDGE ( 'NONE', *, *, #39937, .F. ) ;
#24673 = ORIENTED_EDGE ( 'NONE', *, *, #47962, .T. ) ;
#24674 = B_SPLINE_CURVE_WITH_KNOTS ( 'NONE', 3,
 ( #5692, #25962, #56196, #30592, #20300, #46247 ),
 .UNSPECIFIED., .F., .F.,
 ( 4, 2, 4 ),
 ( 0.006113759649309998857, 0.008271820019583001060, 0.01042988038985600413 ),
 .UNSPECIFIED. ) ;
#24675 = DIRECTION ( 'NONE',  ( 0.000000000000000000, -0.01356324068817998940, 0.9999080150203990547 ) ) ;
#24677 = AXIS2_PLACEMENT_3D ( 'NONE', #58359, #12779, #28105 ) ;
#24676 = LINE ( 'NONE', #4407, #43800 ) ;
#24678 = ORIENTED_EDGE ( 'NONE', *, *, #36857, .F. ) ;
#24679 = CARTESIAN_POINT ( 'NONE',  ( 3.152665057734128862, 5.761241965769081652, 5.461013642405580626 ) ) ;
#24680 = FACE_OUTER_BOUND ( 'NONE', #36954, .T. ) ;
#24681 = DIRECTION ( 'NONE',  ( 0.000000000000000000, -0.5243256840888443904, -0.8515178078024941977 ) ) ;
#24682 = CARTESIAN_POINT ( 'NONE',  ( 37.00000000000000711, 4.705694406421931860E-17, -3.469127814946512892E-15 ) ) ;
#24683 = EDGE_CURVE ( 'NONE', #56961, #57088, #19564, .T. ) ;
#24684 = VERTEX_POINT ( 'NONE', #35795 ) ;
#24685 = CARTESIAN_POINT ( 'NONE',  ( 16.78263030916553333, 25.00000000000000000, 5.836879698929882565 ) ) ;
#24686 = CARTESIAN_POINT ( 'NONE',  ( -11.87635721007226053, -32.86858074101943572, -11.71246211286171857 ) ) ;
#24687 = DIRECTION ( 'NONE',  ( -1.000000000000000000, 0.000000000000000000, 0.000000000000000000 ) ) ;
#24689 = ORIENTED_EDGE ( 'NONE', *, *, #2489, .F. ) ;
#24688 = CARTESIAN_POINT ( 'NONE',  ( 5.530133899448235191, 0.01589823604557752748, 0.001661287012794398143 ) ) ;
#24690 = CARTESIAN_POINT ( 'NONE',  ( -37.00000000000000711, 6.950793414699792727, 10.68873102412845100 ) ) ;
#24691 = ORIENTED_EDGE ( 'NONE', *, *, #64261, .T. ) ;
#24692 = CARTESIAN_POINT ( 'NONE',  ( 0.6511581176964164053, -9.688955459274794180, 7.698038847496666115 ) ) ;
#24693 = ORIENTED_EDGE ( 'NONE', *, *, #50827, .T. ) ;
#24694 = DIRECTION ( 'NONE',  ( 0.000000000000000000, -0.6943713148249691658, 0.7196168960969744344 ) ) ;
#24695 = CIRCLE ( 'NONE', #21518, 5.000000000000000888 ) ;
#24696 = DIRECTION ( 'NONE',  ( 0.000000000000000000, -0.7381862504172023165, 0.6745969609292585822 ) ) ;
#24697 = CARTESIAN_POINT ( 'NONE',  ( 2.241352910868908310, -7.633946224498473043, -0.08337961031712197435 ) ) ;
#24698 = DIRECTION ( 'NONE',  ( 1.000000000000000000, 0.000000000000000000, -0.000000000000000000 ) ) ;
#24699 = AXIS2_PLACEMENT_3D ( 'NONE', #24020, #64880, #44280 ) ;
#24700 = CARTESIAN_POINT ( 'NONE',  ( 0.3057689695767477067, -12.25749431726082506, 0.2309407641932320343 ) ) ;
#24701 = CARTESIAN_POINT ( 'NONE',  ( 5.514624014163232779, 0.002216125254993666586, 0.003498325728817816473 ) ) ;
#24702 = CARTESIAN_POINT ( 'NONE',  ( -27.09252613521642772, -0.1722886739160256198, -2.309775830546441533 ) ) ;
#24703 = CARTESIAN_POINT ( 'NONE',  ( 36.00000000000000711, -12.42372387097884001, -2.865935305911582631 ) ) ;
#24705 = ORIENTED_EDGE ( 'NONE', *, *, #58640, .F. ) ;
#24704 = DIRECTION ( 'NONE',  ( 0.000000000000000000, -0.9937233664769749009, 0.1118654143051720229 ) ) ;
#24706 = AXIS2_PLACEMENT_3D ( 'NONE', #21672, #62525, #41926 ) ;
#24707 = VERTEX_POINT ( 'NONE', #60771 ) ;
#24708 = CARTESIAN_POINT ( 'NONE',  ( 11.31411741755062295, -13.43902530517520866, -1.288601721348704654 ) ) ;
#24709 = VERTEX_POINT ( 'NONE', #24872 ) ;
#24710 = VECTOR ( 'NONE', #17909, 1000.000000000000000 ) ;
#24711 = EDGE_CURVE ( 'NONE', #29943, #57229, #51495, .T. ) ;
#24712 = ORIENTED_EDGE ( 'NONE', *, *, #52579, .T. ) ;
#24713 = DIRECTION ( 'NONE',  ( 0.000000000000000000, -0.01356324068817992175, 0.9999080150203990547 ) ) ;
#24714 = DIRECTION ( 'NONE',  ( 0.000000000000000000, 0.01356324068817998940, -0.9999080150203990547 ) ) ;
#24715 = B_SPLINE_CURVE_WITH_KNOTS ( 'NONE', 3,
 ( #14611, #39579, #9301, #3718, #38604, #64508, #43923, #38935, #48925, #49893, #28954, #59222, #23979, #28299, #4345, #24618, #44239, #24285, #34893, #18339, #59540, #23309, #13971, #34261, #8998, #65178 ),
 .UNSPECIFIED., .F., .F.,
 ( 4, 2, 2, 2, 2, 2, 2, 2, 2, 2, 2, 2, 4 ),
 ( 0.000000000000000000, 0.002759437753103677511, 0.004139156629655517568, 0.005518875506207357624, 0.006898594382759197681, 0.008278313259311036870, 0.01103775101241471525, 0.01379718876551839189, 0.01517690764207022848, 0.01655662651862206680, 0.01931606427172574345, 0.02069578314827758003, 0.02207550202482942009 ),
 .UNSPECIFIED. ) ;
#24716 = LINE ( 'NONE', #40984, #16361 ) ;
#24717 = DIRECTION ( 'NONE',  ( 0.000000000000000000, 0.01356324068817998940, -0.9999080150203990547 ) ) ;
#24718 = CARTESIAN_POINT ( 'NONE',  ( 2.000000000000001776, -6.750946897830710114, 1.593658756657014397 ) ) ;
#24719 = EDGE_CURVE ( 'NONE', #8244, #11975, #14224, .T. ) ;
#24720 = CARTESIAN_POINT ( 'NONE',  ( 35.00000000000000000, -12.49688848680881748, 2.527899948230766913 ) ) ;
#24721 = FACE_OUTER_BOUND ( 'NONE', #13345, .T. ) ;
#24722 = CIRCLE ( 'NONE', #13035, 6.936499999999990784 ) ;
#24723 = VERTEX_POINT ( 'NONE', #25857 ) ;
#24724 = DIRECTION ( 'NONE',  ( -0.6147887355352408267, -0.7886918350401376232, 0.000000000000000000 ) ) ;
#24725 = LINE ( 'NONE', #15395, #44073 ) ;
#24726 = CARTESIAN_POINT ( 'NONE',  ( -18.17110097162331428, -4.731948580995131159, 12.64413186530607014 ) ) ;
#24727 = ORIENTED_EDGE ( 'NONE', *, *, #32131, .F. ) ;
#24728 = VECTOR ( 'NONE', #19437, 1000.000000000000000 ) ;
#24729 = EDGE_CURVE ( 'NONE', #62669, #43307, #29523, .T. ) ;
#24730 = VECTOR ( 'NONE', #12862, 1000.000000000000000 ) ;
#24731 = CIRCLE ( 'NONE', #33223, 7.938172270156617749 ) ;
#24732 = B_SPLINE_CURVE_WITH_KNOTS ( 'NONE', 3,
 ( #12273, #41545, #41884, #32537, #7282, #61836, #27565, #6323, #31262, #37556, #26588, #46882, #61500, #56879, #27247, #47538, #52544, #26270, #46547 ),
 .UNSPECIFIED., .F., .F.,
 ( 4, 3, 3, 3, 3, 3, 4 ),
 ( 9.619659766987995311E-18, 4.457896483015119041E-05, 6.639290541542508593E-05, 8.820687556479463274E-05, 0.0001100173248778967477, 0.0001545671401658198002, 0.0001830328308068606097 ),
 .UNSPECIFIED. ) ;
#24733 = CARTESIAN_POINT ( 'NONE',  ( -35.00000000000000000, 0.8294751490781091530, -12.15823808070321732 ) ) ;
#24734 = B_SPLINE_CURVE_WITH_KNOTS ( 'NONE', 3,
 ( #32645, #27673, #47980, #2437, #22714, #42975 ),
 .UNSPECIFIED., .F., .F.,
 ( 4, 2, 4 ),
 ( 0.0002637379172189280329, 0.0009975831966640225437, 0.001731428476109116892 ),
 .UNSPECIFIED. ) ;
#24735 = CARTESIAN_POINT ( 'NONE',  ( -10.89134765133834293, -7.913666455164804603, -10.93997517974822387 ) ) ;
#24736 = DIRECTION ( 'NONE',  ( 0.000000000000000000, -0.7381862504172023165, 0.6745969609292585822 ) ) ;
#24737 = EDGE_LOOP ( 'NONE', ( #335, #58887, #49282, #50174 ) ) ;
#24738 = LINE ( 'NONE', #10093, #20280 ) ;
#24739 = CARTESIAN_POINT ( 'NONE',  ( 14.80527133490690694, -33.90607016887848602, 8.874040421128851719 ) ) ;
#24740 = DIRECTION ( 'NONE',  ( 1.000000000000000000, 0.000000000000000000, 0.000000000000000000 ) ) ;
#24741 = VECTOR ( 'NONE', #40590, 1000.000000000000000 ) ;
#24742 = EDGE_CURVE ( 'NONE', #26468, #24709, #864, .T. ) ;
#24743 = CIRCLE ( 'NONE', #61901, 5.000000000000000888 ) ;
#24744 = LINE ( 'NONE', #45020, #23551 ) ;
#24745 = FACE_OUTER_BOUND ( 'NONE', #13664, .T. ) ;
#24746 = EDGE_LOOP ( 'NONE', ( #41017, #11064, #45378, #28636 ) ) ;
#24747 = CARTESIAN_POINT ( 'NONE',  ( 2.247112776671469359, 0.1165461824817750069, 7.635437439951568095 ) ) ;
#24748 = DIRECTION ( 'NONE',  ( 1.000000000000000000, -0.000000000000000000, -0.000000000000000000 ) ) ;
#24749 = AXIS2_PLACEMENT_3D ( 'NONE', #18516, #59069, #13477 ) ;
#24750 = DIRECTION ( 'NONE',  ( 0.000000000000000000, 0.4134677391718510897, 0.9105187689795954942 ) ) ;
#24751 = ORIENTED_EDGE ( 'NONE', *, *, #53839, .T. ) ;
#24752 = CARTESIAN_POINT ( 'NONE',  ( 8.936348816238876225, 2.397984168018178153, 13.28748829145446919 ) ) ;
#24753 = CARTESIAN_POINT ( 'NONE',  ( 1.000000000000000888, -3.795144977083577675, -6.468916029978841742 ) ) ;
#24754 = ORIENTED_EDGE ( 'NONE', *, *, #39399, .T. ) ;
#24755 = EDGE_LOOP ( 'NONE', ( #62322, #51675, #7678, #54075 ) ) ;
#24756 = ORIENTED_EDGE ( 'NONE', *, *, #64493, .F. ) ;
#24757 = VECTOR ( 'NONE', #65356, 1000.000000000000000 ) ;
#24758 = ORIENTED_EDGE ( 'NONE', *, *, #54972, .T. ) ;
#24759 = DIRECTION ( 'NONE',  ( 0.000000000000000000, 0.5472293298355273006, -0.8369827122275342868 ) ) ;
#24760 = DIRECTION ( 'NONE',  ( 0.000000000000000000, -0.9903235168508564001, -0.1387779952735713473 ) ) ;
#24761 = CARTESIAN_POINT ( 'NONE',  ( -35.00000000000000000, 0.000000000000000000, 0.000000000000000000 ) ) ;
#24762 = EDGE_CURVE ( 'NONE', #20510, #20746, #47266, .T. ) ;
#24763 = CARTESIAN_POINT ( 'NONE',  ( -15.04954985558960878, -34.74586518154888637, 6.983850705393018998 ) ) ;
#24764 = CARTESIAN_POINT ( 'NONE',  ( 22.88594695219327235, 3.421158645304719137, -13.05931366970166962 ) ) ;
#24766 = ORIENTED_EDGE ( 'NONE', *, *, #50382, .T. ) ;
#24765 = CARTESIAN_POINT ( 'NONE',  ( -27.08429572838383947, 1.608131779585724619, 1.632445743623414325 ) ) ;
#24767 = EDGE_CURVE ( 'NONE', #31684, #31935, #34824, .T. ) ;
#24768 = DIRECTION ( 'NONE',  ( 0.000000000000000000, -0.01356324068817998940, 0.9999080150203990547 ) ) ;
#24769 = ORIENTED_EDGE ( 'NONE', *, *, #38763, .F. ) ;
#24770 = AXIS2_PLACEMENT_3D ( 'NONE', #44865, #45197, #3349 ) ;
#24771 = CYLINDRICAL_SURFACE ( 'NONE', #29573, 4.999999999999999112 ) ;
#24772 = ORIENTED_EDGE ( 'NONE', *, *, #21642, .T. ) ;
#24773 = AXIS2_PLACEMENT_3D ( 'NONE', #58739, #33749, #39397 ) ;
#24774 = ORIENTED_EDGE ( 'NONE', *, *, #7957, .F. ) ;
#24775 = CARTESIAN_POINT ( 'NONE',  ( -27.15525204139121840, 1.831989866434750480, 1.707635684994303515 ) ) ;
#24776 = CARTESIAN_POINT ( 'NONE',  ( 13.56792483471932798, -30.10715271124615455, 6.611461891173466832 ) ) ;
#24778 = CARTESIAN_POINT ( 'NONE',  ( 2.406456491626625560, 8.382123850276952837, 6.212289237903838135 ) ) ;
#24777 = CIRCLE ( 'NONE', #33264, 12.74999999999999822 ) ;
#24779 = CIRCLE ( 'NONE', #59807, 4.999999999999999112 ) ;
#24780 = ADVANCED_FACE ( 'NONE', ( #10216 ), #4262, .T. ) ;
#24781 = CARTESIAN_POINT ( 'NONE',  ( -35.00000000000000000, -11.54110654723650420, 2.185196060783841432 ) ) ;
#24782 = DIRECTION ( 'NONE',  ( -1.000000000000000000, -0.000000000000000000, 0.000000000000000000 ) ) ;
#24783 = DIRECTION ( 'NONE',  ( 0.000000000000000000, 0.01356324068817992175, -0.9999080150203990547 ) ) ;
#24784 = ORIENTED_EDGE ( 'NONE', *, *, #47600, .F. ) ;
#24785 = VERTEX_POINT ( 'NONE', #60433 ) ;
#24786 = DIRECTION ( 'NONE',  ( -1.000000000000000000, 0.000000000000000000, 0.000000000000000000 ) ) ;
#24787 = ORIENTED_EDGE ( 'NONE', *, *, #58195, .F. ) ;
#24788 = CIRCLE ( 'NONE', #4630, 5.000000000000000888 ) ;
#24789 = ADVANCED_FACE ( 'NONE', ( #61096 ), #59791, .T. ) ;
#24790 = VERTEX_POINT ( 'NONE', #50792 ) ;
#24791 = CARTESIAN_POINT ( 'NONE',  ( 2.280717697723837922, -7.502592193582055202, 1.481796453660293222 ) ) ;
#24792 = CARTESIAN_POINT ( 'NONE',  ( 2.241449424704146320, 1.386092121067206140, 7.507583637787353048 ) ) ;
#24793 = CARTESIAN_POINT ( 'NONE',  ( 18.70366329277965178, -2.125550911571206569, 11.85937264694274518 ) ) ;
#24794 = CARTESIAN_POINT ( 'NONE',  ( -35.00000000000000000, 10.54834585426219995, 6.102719229070713070 ) ) ;
#24795 = CIRCLE ( 'NONE', #39636, 5.000000000000001776 ) ;
#24796 = CARTESIAN_POINT ( 'NONE',  ( -11.40165637463000259, -7.158503671335326501, -9.641458581199431777 ) ) ;
#24797 = DIRECTION ( 'NONE',  ( -1.000000000000000000, 0.000000000000000000, 0.000000000000000000 ) ) ;
#24798 = EDGE_LOOP ( 'NONE', ( #21265, #56917, #22136, #35413, #14297, #23264, #1496, #30316, #63325, #28593, #21340, #1041 ) ) ;
#24799 = CIRCLE ( 'NONE', #33293, 7.499999999999988454 ) ;
#24800 = ORIENTED_EDGE ( 'NONE', *, *, #2414, .F. ) ;
#24801 = CIRCLE ( 'NONE', #32238, 12.18650000000000411 ) ;
#24802 = CARTESIAN_POINT ( 'NONE',  ( 1.719304012338199517, 0.000000000000000000, 0.000000000000000000 ) ) ;
#24803 = CARTESIAN_POINT ( 'NONE',  ( 2.288423627607477417, 7.504187945869073673, -1.486973602181071552 ) ) ;
#24804 = FACE_OUTER_BOUND ( 'NONE', #42886, .T. ) ;
#24805 = CARTESIAN_POINT ( 'NONE',  ( 6.680451748998780026, -7.311972598139333535, 9.517076143087459528 ) ) ;
#24806 = VECTOR ( 'NONE', #41188, 1000.000000000000000 ) ;
#24807 = CARTESIAN_POINT ( 'NONE',  ( 1.452237505248552996, 11.67686475128079771, 4.880303821311048118 ) ) ;
#24808 = CARTESIAN_POINT ( 'NONE',  ( 7.182606707284545422, -7.361254329974325827, -11.31839762553341622 ) ) ;
#24809 = FACE_OUTER_BOUND ( 'NONE', #65249, .T. ) ;
#24810 = CARTESIAN_POINT ( 'NONE',  ( 2.430348790457011798, 6.019963855523680962, 4.796903114819394354 ) ) ;
#24811 = CARTESIAN_POINT ( 'NONE',  ( -22.31328051695926007, 2.748895659348141507, 2.608921479762082551 ) ) ;
#24812 = ORIENTED_EDGE ( 'NONE', *, *, #12305, .T. ) ;
#24813 = VECTOR ( 'NONE', #28506, 1000.000000000000000 ) ;
#24814 = CARTESIAN_POINT ( 'NONE',  ( -21.17861794710831091, 11.44571409049744304, -3.604945070120774808 ) ) ;
#24815 = CARTESIAN_POINT ( 'NONE',  ( -28.66013792860432119, 1.289369452666815796, 1.306994062650322919 ) ) ;
#24816 = AXIS2_PLACEMENT_3D ( 'NONE', #51031, #9793, #50047 ) ;
#24817 = CARTESIAN_POINT ( 'NONE',  ( 2.990245332647882837, 6.155689586375199696, 5.834301250882226952 ) ) ;
#24818 = CIRCLE ( 'NONE', #48203, 6.936499999999989896 ) ;
#24819 = ADVANCED_FACE ( 'NONE', ( #9228, #50148 ), #43341, .F. ) ;
#24820 = CARTESIAN_POINT ( 'NONE',  ( 2.963017218115626683, -6.619413971958186593, -4.265970453343994606 ) ) ;
#24821 = CARTESIAN_POINT ( 'NONE',  ( -28.06993472828175484, -9.866117616252182643, -6.837783180416262319 ) ) ;
#24822 = ORIENTED_EDGE ( 'NONE', *, *, #38913, .T. ) ;
#24823 = CARTESIAN_POINT ( 'NONE',  ( -37.00000000000000711, 4.018060380616562455, -11.50504120060938718 ) ) ;
#24824 = CARTESIAN_POINT ( 'NONE',  ( 2.770579946183238995, 6.607710183380625324, 4.165025702425821486 ) ) ;
#24825 = AXIS2_PLACEMENT_3D ( 'NONE', #64448, #18918, #39183 ) ;
#24826 = CARTESIAN_POINT ( 'NONE',  ( 9.075728589825974524, -28.84360970496360466, -9.643933591119377979 ) ) ;
#24827 = ORIENTED_EDGE ( 'NONE', *, *, #8513, .F. ) ;
#24828 = CARTESIAN_POINT ( 'NONE',  ( 0.6511581176957980110, -6.471755598256246245, 10.54760823437298001 ) ) ;
#24829 = CARTESIAN_POINT ( 'NONE',  ( 47.00000000000000711, 4.705694406421931860E-17, -3.469127814946512892E-15 ) ) ;
#24830 = CARTESIAN_POINT ( 'NONE',  ( 0.2646305136544072623, -12.24595685781654808, 0.1321451301297412451 ) ) ;
#24831 = AXIS2_PLACEMENT_3D ( 'NONE', #30758, #35742, #51074 ) ;
#24832 = CARTESIAN_POINT ( 'NONE',  ( 0.2869720083484367801, -8.034871682535149162, 9.251312689958732349 ) ) ;
#24833 = DIRECTION ( 'NONE',  ( -1.000000000000000000, 0.000000000000000000, 0.000000000000000000 ) ) ;
#24834 = VECTOR ( 'NONE', #8088, 1000.000000000000000 ) ;
#24835 = EDGE_CURVE ( 'NONE', #13080, #26919, #5242, .T. ) ;
#24836 = CARTESIAN_POINT ( 'NONE',  ( 1.014383007554945149, 12.22116704270661813, -2.605923236272006172 ) ) ;
#24837 = EDGE_LOOP ( 'NONE', ( #41638, #60898, #23996, #39890 ) ) ;
#24838 = CARTESIAN_POINT ( 'NONE',  ( -35.00000000000000000, 11.02904044024209185, -4.041347439435899247 ) ) ;
#24839 = CARTESIAN_POINT ( 'NONE',  ( 2.000000000000001776, -5.997115278587605403, -3.485633455389573587 ) ) ;
#24840 = CARTESIAN_POINT ( 'NONE',  ( 0.3341166715381310159, -9.559079491641819359, -7.691251065848441648 ) ) ;
#24841 = CARTESIAN_POINT ( 'NONE',  ( 0.9296196016848911059, -1.754499435239580851, -12.34355205587747228 ) ) ;
#24842 = CARTESIAN_POINT ( 'NONE',  ( 0.2851083653049530375, -0.4107471485392680810, -13.49374991542258151 ) ) ;
#24843 = ADVANCED_FACE ( 'NONE', ( #263 ), #40136, .T. ) ;
#24844 = AXIS2_PLACEMENT_3D ( 'NONE', #40137, #20198, #14534 ) ;
#24845 = CARTESIAN_POINT ( 'NONE',  ( 35.00000000000000000, 4.705694406421931860E-17, -3.469127814946512892E-15 ) ) ;
#24846 = CARTESIAN_POINT ( 'NONE',  ( 2.259025283526327588, 1.191911401087284217, -7.546748801934501927 ) ) ;
#24847 = ORIENTED_EDGE ( 'NONE', *, *, #34916, .T. ) ;
#24848 = EDGE_CURVE ( 'NONE', #21602, #25841, #48686, .T. ) ;
#24849 = EDGE_LOOP ( 'NONE', ( #64332, #54812, #17068, #42956 ) ) ;
#24850 = DIRECTION ( 'NONE',  ( -1.000000000000000000, 0.000000000000000000, 0.000000000000000000 ) ) ;
#24851 = VERTEX_POINT ( 'NONE', #57100 ) ;
#24852 = FACE_OUTER_BOUND ( 'NONE', #21497, .T. ) ;
#24853 = AXIS2_PLACEMENT_3D ( 'NONE', #28386, #3140, #39012 ) ;
#24854 = EDGE_CURVE ( 'NONE', #58967, #60906, #22123, .T. ) ;
#24855 = CARTESIAN_POINT ( 'NONE',  ( 5.530133899448235191, -0.01459891979722874843, 0.006510401266731764142 ) ) ;
#24856 = ORIENTED_EDGE ( 'NONE', *, *, #29067, .T. ) ;
#24857 = DIRECTION ( 'NONE',  ( 0.000000000000000000, 0.000000000000000000, 1.000000000000000000 ) ) ;
#24858 =( BOUNDED_CURVE ( )  B_SPLINE_CURVE ( 3, ( #49779, #29804, #20167, #4228 ),
 .UNSPECIFIED., .F., .F. ) 
 B_SPLINE_CURVE_WITH_KNOTS ( ( 4, 4 ),
 ( 0.3740640042953261024, 0.4316535298590248870 ),
 .UNSPECIFIED. ) 
 CURVE ( )  GEOMETRIC_REPRESENTATION_ITEM ( )  RATIONAL_B_SPLINE_CURVE ( ( 1.000000000000000000, 0.9997236396413186066, 0.9997236396413186066, 1.000000000000000000 ) ) 
 REPRESENTATION_ITEM ( '' )  );
#24859 = LINE ( 'NONE', #55772, #23153 ) ;
#24861 = EDGE_CURVE ( 'NONE', #12647, #36193, #1971, .T. ) ;
#24860 = CARTESIAN_POINT ( 'NONE',  ( 35.00000000000000000, -6.711949091238068377, 10.84030624090613060 ) ) ;
#24862 = ORIENTED_EDGE ( 'NONE', *, *, #52120, .T. ) ;
#24864 = ORIENTED_EDGE ( 'NONE', *, *, #6444, .F. ) ;
#24863 = B_SPLINE_CURVE_WITH_KNOTS ( 'NONE', 3,
 ( #48632, #18039, #58279, #59263, #12697, #53290, #38301, #33654, #13046, #53944, #33331, #53631, #28338, #48970, #3089, #38648, #63907, #8385, #3427, #9677, #39947, #29969, #24324, #39287, #44589, #34304 ),
 .UNSPECIFIED., .F., .F.,
 ( 4, 2, 2, 2, 2, 2, 2, 2, 2, 2, 2, 2, 4 ),
 ( 0.000000000000000000, 0.001208835475306771490, 0.001813253212960158969, 0.002417670950613546449, 0.003626506425920317939, 0.004230924163573704551, 0.004835341901227091163, 0.005439759638880478643, 0.006044177376533865255, 0.006648595114187251867, 0.007253012851840638479, 0.008461848327147414306, 0.009670683802454189265 ),
 .UNSPECIFIED. ) ;
#24865 = CARTESIAN_POINT ( 'NONE',  ( 2.000000000000001776, -6.201547234536999298, -2.820401998297984214 ) ) ;
#24866 = AXIS2_PLACEMENT_3D ( 'NONE', #29544, #56131, #45496 ) ;
#24867 = ORIENTED_EDGE ( 'NONE', *, *, #64686, .F. ) ;
#24868 = DIRECTION ( 'NONE',  ( 0.000000000000000000, -0.3807014730195285579, 0.9246979985058696450 ) ) ;
#24869 = ORIENTED_EDGE ( 'NONE', *, *, #2463, .T. ) ;
#24870 = CYLINDRICAL_SURFACE ( 'NONE', #57530, 12.75000000000000178 ) ;
#24871 = CARTESIAN_POINT ( 'NONE',  ( -27.09150307427401216, 1.001311209615680209, -2.085162835056712627 ) ) ;
#24872 = CARTESIAN_POINT ( 'NONE',  ( 37.00000000000000711, -0.6593684648219547695, 12.73293890771483561 ) ) ;
#24873 = EDGE_CURVE ( 'NONE', #18117, #11339, #42323, .T. ) ;
#24874 = CARTESIAN_POINT ( 'NONE',  ( -22.46509356695199600, -1.314379028669519833, -4.038408495643935225 ) ) ;
#24875 = ORIENTED_EDGE ( 'NONE', *, *, #15821, .F. ) ;
#24876 = CARTESIAN_POINT ( 'NONE',  ( 2.276905613633648962, 7.644700064315451016, -0.1540880535621231562 ) ) ;
#24877 = CARTESIAN_POINT ( 'NONE',  ( 0.2653519991613825235, 7.888569541500650040, -9.366979519113268537 ) ) ;
#24878 = EDGE_CURVE ( 'NONE', #57898, #2022, #50438, .T. ) ;
#24879 = DIRECTION ( 'NONE',  ( -1.000000000000000000, 0.000000000000000000, 0.000000000000000000 ) ) ;
#24880 = FACE_OUTER_BOUND ( 'NONE', #21778, .T. ) ;
#24881 = CARTESIAN_POINT ( 'NONE',  ( 10.33819151767390743, 13.43558936918568136, -1.319127422667911276 ) ) ;
#24882 = CARTESIAN_POINT ( 'NONE',  ( 24.36133864597850263, -0.004336254571473984777, 13.50457224143761259 ) ) ;
#24883 = FACE_OUTER_BOUND ( 'NONE', #19064, .T. ) ;
#24884 = CARTESIAN_POINT ( 'NONE',  ( -37.00000000000000711, 11.66664283989680051, 5.143145423404323680 ) ) ;
#24885 = CYLINDRICAL_SURFACE ( 'NONE', #6606, 8.049672981451799103 ) ;
#24886 = AXIS2_PLACEMENT_3D ( 'NONE', #11589, #6291, #26554 ) ;
#24887 = ORIENTED_EDGE ( 'NONE', *, *, #48375, .F. ) ;
#24888 = CARTESIAN_POINT ( 'NONE',  ( 0.2915757698887293525, 0.2147157799034817294, 12.25305747416127922 ) ) ;
#24889 = VERTEX_POINT ( 'NONE', #62384 ) ;
#24890 = FACE_OUTER_BOUND ( 'NONE', #59611, .T. ) ;
#24891 = CARTESIAN_POINT ( 'NONE',  ( 0.000000000000000000, -7.414200355365264450, 1.131208685655129775 ) ) ;
#24892 = CIRCLE ( 'NONE', #18556, 4.999999999999999112 ) ;
#24893 = CARTESIAN_POINT ( 'NONE',  ( -35.00000000000000000, 0.000000000000000000, 0.000000000000000000 ) ) ;
#24894 = FACE_OUTER_BOUND ( 'NONE', #62648, .T. ) ;
#24895 = CARTESIAN_POINT ( 'NONE',  ( 2.781367136452752575, 5.255136723410658739, 5.783466416658742837 ) ) ;
#24896 = VERTEX_POINT ( 'NONE', #36804 ) ;
#24897 = CARTESIAN_POINT ( 'NONE',  ( -37.00000000000000711, -10.01317267707891467, 6.946017217729903770 ) ) ;
#24898 = CARTESIAN_POINT ( 'NONE',  ( 3.092491956585225577, 2.283527081234640654, -7.581757403488093239 ) ) ;
#24899 = CARTESIAN_POINT ( 'NONE',  ( 9.040406806271612083, 3.542740750417936901, 11.46777809083421218 ) ) ;
#24900 = CARTESIAN_POINT ( 'NONE',  ( -27.10719052120871098, -0.5475695427849570640, 2.295785794152556125 ) ) ;
#24901 = EDGE_CURVE ( 'NONE', #5918, #36872, #62505, .T. ) ;
#24902 = VECTOR ( 'NONE', #25613, 1000.000000000000000 ) ;
#24903 = LINE ( 'NONE', #18632, #49987 ) ;
#24904 = ORIENTED_EDGE ( 'NONE', *, *, #19410, .F. ) ;
#24905 = CARTESIAN_POINT ( 'NONE',  ( -36.00000000000000711, 2.696588552979058750, 12.46157735505190267 ) ) ;
#24906 = ORIENTED_EDGE ( 'NONE', *, *, #11337, .F. ) ;
#24907 = CARTESIAN_POINT ( 'NONE',  ( 0.3057689695767489280, -0.2309407641931890687, -12.25749431726082506 ) ) ;
#24908 = DIRECTION ( 'NONE',  ( 0.000000000000000000, 0.01356324068817998940, -0.9999080150203990547 ) ) ;
#24909 = AXIS2_PLACEMENT_3D ( 'NONE', #35370, #15734, #60992 ) ;
#24910 = EDGE_CURVE ( 'NONE', #7095, #56961, #31075, .T. ) ;
#24911 = CARTESIAN_POINT ( 'NONE',  ( 35.00000000000000000, -7.379373053628789592, 10.39746860227898217 ) ) ;
#24912 = CARTESIAN_POINT ( 'NONE',  ( 0.000000000000000000, -3.073484823194281290, -6.841322316745092280 ) ) ;
#24913 = B_SPLINE_CURVE_WITH_KNOTS ( 'NONE', 3,
 ( #63245, #2078, #22028, #22348, #62918, #28020, #37972, #18377, #12693, #7731, #12369, #8066, #17041, #32636, #48319, #52949 ),
 .UNSPECIFIED., .F., .F.,
 ( 4, 3, 3, 3, 3, 4 ),
 ( 8.673617379884035472E-19, 0.0002176109881720281712, 0.0004352086762394674971, 0.0006528017811446998678, 0.0007615147961451848536, 0.0009453342004947393401 ),
 .UNSPECIFIED. ) ;
#24914 = EDGE_CURVE ( 'NONE', #11018, #14439, #47454, .T. ) ;
#24915 = ORIENTED_EDGE ( 'NONE', *, *, #15976, .T. ) ;
#24916 = EDGE_LOOP ( 'NONE', ( #16257, #58074, #24928, #28368 ) ) ;
#24917 = B_SPLINE_CURVE_WITH_KNOTS ( 'NONE', 3,
 ( #32687, #12417, #33377, #8114, #17765, #8432, #48025, #2482, #18436, #22760, #43019, #64287, #63293, #38019, #7787, #23078, #43337, #63613, #38354, #13412, #39011, #28385 ),
 .UNSPECIFIED., .F., .F.,
 ( 4, 3, 3, 3, 3, 3, 3, 4 ),
 ( 0.000000000000000000, 4.447697177976197875E-05, 6.624143997791211342E-05, 8.800576886944256867E-05, 0.0001097699864780881122, 0.0001315341395364362433, 0.0001760120188223267756, 0.0001867971373174692653 ),
 .UNSPECIFIED. ) ;
#24918 = DIRECTION ( 'NONE',  ( -1.000000000000000000, 0.000000000000000000, 0.000000000000000000 ) ) ;
#24919 = ORIENTED_EDGE ( 'NONE', *, *, #48571, .T. ) ;
#24920 = CARTESIAN_POINT ( 'NONE',  ( 2.298277635560274312, -6.543949079923912393, -3.968740875991624062 ) ) ;
#24922 = AXIS2_PLACEMENT_3D ( 'NONE', #24647, #58340, #13111 ) ;
#24921 = DIRECTION ( 'NONE',  ( -1.000000000000000000, 0.000000000000000000, 0.000000000000000000 ) ) ;
#24923 = CARTESIAN_POINT ( 'NONE',  ( 5.516018279890452902, -0.005976902763919015801, 0.003191189039764900665 ) ) ;
#24924 = DIRECTION ( 'NONE',  ( -1.000000000000000000, 0.000000000000000000, 0.000000000000000000 ) ) ;
#24925 = CARTESIAN_POINT ( 'NONE',  ( 2.665405856346790170, -5.274989403260943455, 7.981834391067692103 ) ) ;
#24926 = CARTESIAN_POINT ( 'NONE',  ( -37.00000000000000711, -6.415447294506628317, -11.01837265713080072 ) ) ;
#24927 = CARTESIAN_POINT ( 'NONE',  ( -27.08416974970326052, -0.4041872645907051420, -2.255186831366117417 ) ) ;
#24928 = ORIENTED_EDGE ( 'NONE', *, *, #43068, .F. ) ;
#24929 = EDGE_CURVE ( 'NONE', #32830, #65463, #2008, .T. ) ;
#24930 = CIRCLE ( 'NONE', #58943, 12.75000000000000178 ) ;
#24932 = VERTEX_POINT ( 'NONE', #61739 ) ;
#24931 = CARTESIAN_POINT ( 'NONE',  ( 1.020182472822703801, -11.03967505355367607, 5.858468047365960274 ) ) ;
#24933 = ORIENTED_EDGE ( 'NONE', *, *, #36645, .F. ) ;
#24934 = DIRECTION ( 'NONE',  ( 1.000000000000000000, 0.000000000000000000, -0.000000000000000000 ) ) ;
#24935 = CARTESIAN_POINT ( 'NONE',  ( -27.08429572838383947, 1.859677275556428810, -1.338867938658195200 ) ) ;
#24936 = ORIENTED_EDGE ( 'NONE', *, *, #32639, .T. ) ;
#24937 = CARTESIAN_POINT ( 'NONE',  ( -22.30625920655495165, 0.2529928606556913206, 3.783486345733959588 ) ) ;
#24938 = ORIENTED_EDGE ( 'NONE', *, *, #1517, .F. ) ;
#24939 = CARTESIAN_POINT ( 'NONE',  ( 37.00000000000000711, -7.817492529713787164, 9.348667969174485393 ) ) ;
#24940 = FACE_OUTER_BOUND ( 'NONE', #64467, .T. ) ;
#24942 = EDGE_CURVE ( 'NONE', #27683, #23780, #41121, .T. ) ;
#24941 = CARTESIAN_POINT ( 'NONE',  ( 0.000000000000000000, 0.000000000000000000, 0.000000000000000000 ) ) ;
#24943 = CARTESIAN_POINT ( 'NONE',  ( 2.430348790457227626, 7.164221884688219966, -2.814990071337918121 ) ) ;
#24944 = ORIENTED_EDGE ( 'NONE', *, *, #62315, .T. ) ;
#24945 = ORIENTED_EDGE ( 'NONE', *, *, #59532, .F. ) ;
#24946 = CARTESIAN_POINT ( 'NONE',  ( 2.373367633546870525, -6.738274194514239923, 3.681545031436630033 ) ) ;
#24948 = ORIENTED_EDGE ( 'NONE', *, *, #10396, .F. ) ;
#24947 = EDGE_CURVE ( 'NONE', #62360, #57516, #50856, .T. ) ;
#24949 = CARTESIAN_POINT ( 'NONE',  ( 0.3160775863651100748, 11.60348481172941426, -3.967735865794236538 ) ) ;
#24950 = VERTEX_POINT ( 'NONE', #57766 ) ;
#24951 = EDGE_LOOP ( 'NONE', ( #50885, #26335, #43049, #5753 ) ) ;
#24953 = EDGE_CURVE ( 'NONE', #17964, #21760, #48721, .T. ) ;
#24952 = ORIENTED_EDGE ( 'NONE', *, *, #61841, .F. ) ;
#24954 = CARTESIAN_POINT ( 'NONE',  ( 0.2650492594609225039, 11.46945808033133929, 4.291723947796354466 ) ) ;
#24955 = CARTESIAN_POINT ( 'NONE',  ( 12.41715713833625045, -27.32744910944862227, 12.80873342738428278 ) ) ;
#24956 = PLANE ( 'NONE',  #54249 ) ;
#24957 = CARTESIAN_POINT ( 'NONE',  ( -22.39032720737626647, -2.746561316202153602, 2.936932155721176496 ) ) ;
#24958 = ORIENTED_EDGE ( 'NONE', *, *, #38439, .T. ) ;
#24959 = EDGE_CURVE ( 'NONE', #6900, #43286, #31488, .T. ) ;
#24960 = EDGE_CURVE ( 'NONE', #4743, #45642, #26493, .T. ) ;
#24961 = CARTESIAN_POINT ( 'NONE',  ( -37.00000000000000711, 0.000000000000000000, 0.000000000000000000 ) ) ;
#24962 = ORIENTED_EDGE ( 'NONE', *, *, #50277, .F. ) ;
#24963 = CARTESIAN_POINT ( 'NONE',  ( -35.00000000000000000, -3.645068577060105230, 11.16627499335654150 ) ) ;
#24964 = FACE_OUTER_BOUND ( 'NONE', #24837, .T. ) ;
#24965 = EDGE_CURVE ( 'NONE', #39372, #37744, #29788, .T. ) ;
#24966 = AXIS2_PLACEMENT_3D ( 'NONE', #10040, #15352, #14667 ) ;
#24967 = ORIENTED_EDGE ( 'NONE', *, *, #65504, .F. ) ;
#24968 = CARTESIAN_POINT ( 'NONE',  ( 35.00000000000000000, -10.92721691015452912, 4.309077947445766554 ) ) ;
#24969 = DIRECTION ( 'NONE',  ( -1.000000000000000000, 0.000000000000000000, 0.000000000000000000 ) ) ;
#24970 = DIRECTION ( 'NONE',  ( -0.000000000000000000, -1.000000000000000000, -0.000000000000000000 ) ) ;
#24971 = B_SPLINE_CURVE_WITH_KNOTS ( 'NONE', 3,
 ( #31222, #51528, #5642, #959, #65777, #40528, #25910, #51839, #6286, #60824, #55840, #61456, #46199, #40872, #10266, #45861 ),
 .UNSPECIFIED., .F., .F.,
 ( 4, 3, 3, 3, 3, 4 ),
 ( 0.000000000000000000, 0.0002999043160757438459, 0.0005998071753051191068, 0.0008997092107374842678, 0.001204458948196640827, 0.001510329163478487616 ),
 .UNSPECIFIED. ) ;
#24972 = ORIENTED_EDGE ( 'NONE', *, *, #45655, .F. ) ;
#24973 = DIRECTION ( 'NONE',  ( 0.000000000000000000, -0.000000000000000000, 1.000000000000000000 ) ) ;
#24974 = CIRCLE ( 'NONE', #62130, 6.936499999999987232 ) ;
#24975 = ORIENTED_EDGE ( 'NONE', *, *, #6642, .T. ) ;
#24976 = CARTESIAN_POINT ( 'NONE',  ( 0.3057689695767517035, 10.73077184758791702, 5.928746590069615685 ) ) ;
#24977 = FILL_AREA_STYLE_COLOUR ( '', #46743 ) ;
#24978 = DIRECTION ( 'NONE',  ( -1.000000000000000000, 0.000000000000000000, -0.000000000000000000 ) ) ;
#24979 = CARTESIAN_POINT ( 'NONE',  ( 2.249013661412013754, -3.714035584818559332, -6.673008335691601012 ) ) ;
#24980 = CARTESIAN_POINT ( 'NONE',  ( 10.55727017642485954, 11.97188460455015502, -0.8507229460849952130 ) ) ;
#24981 = ORIENTED_EDGE ( 'NONE', *, *, #17374, .T. ) ;
#24982 = DIRECTION ( 'NONE',  ( 0.000000000000000000, 0.7790879021242528291, -0.6269146997507959451 ) ) ;
#24983 = DIRECTION ( 'NONE',  ( -1.000000000000000000, -0.000000000000000000, 0.000000000000000000 ) ) ;
#24984 = CARTESIAN_POINT ( 'NONE',  ( 2.655192694324727487, -2.234846078477053410, -9.337840456945928125 ) ) ;
#24985 = CARTESIAN_POINT ( 'NONE',  ( -35.00000000000000000, 11.16627499335650242, 3.645068577060221582 ) ) ;
#24986 = AXIS2_PLACEMENT_3D ( 'NONE', #35631, #65245, #19713 ) ;
#24987 = EDGE_CURVE ( 'NONE', #3409, #16590, #58262, .T. ) ;
#24988 = CARTESIAN_POINT ( 'NONE',  ( 0.3164563675027619039, -12.11636128244743027, -1.892265234253239115 ) ) ;
#24989 = DIRECTION ( 'NONE',  ( 0.000000000000000000, 0.000000000000000000, 1.000000000000000000 ) ) ;
#24990 = DIRECTION ( 'NONE',  ( -1.000000000000000000, 0.000000000000000000, 0.000000000000000000 ) ) ;
#24991 = B_SPLINE_CURVE_WITH_KNOTS ( 'NONE', 3,
 ( #28601, #28940, #38922, #29267, #13319, #24604, #39230, #59210, #18662, #19632 ),
 .UNSPECIFIED., .F., .F.,
 ( 4, 3, 3, 4 ),
 ( 0.000000000000000000, 6.607638129004381818E-05, 9.911389841680568337E-05, 0.0001667630577588626094 ),
 .UNSPECIFIED. ) ;
#24992 = CARTESIAN_POINT ( 'NONE',  ( 5.536195898058073439, -0.002666509901869554798, -0.008071068258923213418 ) ) ;
#24993 = DIRECTION ( 'NONE',  ( -1.000000000000000000, 0.000000000000000000, 0.000000000000000000 ) ) ;
#24994 = ADVANCED_FACE ( 'NONE', ( #22501, #54071, #27813 ), #28792, .F. ) ;
#24995 = CIRCLE ( 'NONE', #37751, 5.000000000000000888 ) ;
#24996 = EDGE_LOOP ( 'NONE', ( #58817, #5996, #13797, #25901 ) ) ;
#24997 = CARTESIAN_POINT ( 'NONE',  ( -27.08871896697732140, -1.309412067287333059, -1.896680818246855305 ) ) ;
#24998 = ORIENTED_EDGE ( 'NONE', *, *, #60031, .T. ) ;
#24999 = DIRECTION ( 'NONE',  ( 1.000000000000000000, 0.000000000000000000, 0.000000000000000000 ) ) ;
#25000 = CARTESIAN_POINT ( 'NONE',  ( 0.3665391374699472626, -9.576575648338968350, -7.691255657244390420 ) ) ;
#25001 = DIRECTION ( 'NONE',  ( -1.000000000000000000, -0.000000000000000000, 0.000000000000000000 ) ) ;
#25002 = CARTESIAN_POINT ( 'NONE',  ( 0.2638984909335716500, -0.1991813963114842101, 12.24571285024409129 ) ) ;
#25003 = ORIENTED_EDGE ( 'NONE', *, *, #10667, .F. ) ;
#25004 = EDGE_CURVE ( 'NONE', #19021, #20284, #15554, .T. ) ;
#25005 = ORIENTED_EDGE ( 'NONE', *, *, #18707, .T. ) ;
#25006 = ORIENTED_EDGE ( 'NONE', *, *, #11573, .T. ) ;
#25007 = CARTESIAN_POINT ( 'NONE',  ( 2.889800649504073782, 0.9965440656174524570, -6.039722463373529138 ) ) ;
#25008 = EDGE_CURVE ( 'NONE', #65378, #63878, #44468, .T. ) ;
#25009 = CARTESIAN_POINT ( 'NONE',  ( 3.031336079629583846, 3.582646412484484788, -7.038432939676037670 ) ) ;
#25010 = ORIENTED_EDGE ( 'NONE', *, *, #18599, .F. ) ;
#25011 = CARTESIAN_POINT ( 'NONE',  ( 35.00000000000000000, -10.92721691015452912, 4.309077947445766554 ) ) ;
#25012 = DIRECTION ( 'NONE',  ( -1.000000000000000000, 0.000000000000000000, 0.000000000000000000 ) ) ;
#25013 = CARTESIAN_POINT ( 'NONE',  ( 2.368238019615237722, -2.455958560214692721, 7.273245349264759518 ) ) ;
#25014 = ORIENTED_EDGE ( 'NONE', *, *, #5113, .T. ) ;
#25015 = CIRCLE ( 'NONE', #57962, 6.936499999999991672 ) ;
#25016 = CARTESIAN_POINT ( 'NONE',  ( 2.276905613634090386, 4.795880183929502216, -5.955225895210846332 ) ) ;
#25017 = CARTESIAN_POINT ( 'NONE',  ( -0.5153900578009920075, -26.55329395651783031, -16.22445808467987050 ) ) ;
#25018 = DIRECTION ( 'NONE',  ( -1.000000000000000000, 0.000000000000000000, 0.000000000000000000 ) ) ;
#25020 = VERTEX_POINT ( 'NONE', #7874 ) ;
#25019 = DIRECTION ( 'NONE',  ( 1.000000000000000000, 0.000000000000000000, -0.000000000000000000 ) ) ;
#25021 = CARTESIAN_POINT ( 'NONE',  ( 2.000000000000001776, -4.376687952327356079, 5.220963330856582374 ) ) ;
#25022 = EDGE_LOOP ( 'NONE', ( #53442, #39992, #59746, #35926 ) ) ;
#25023 = DIRECTION ( 'NONE',  ( 0.000000000000000000, -0.01356324068817992175, 0.9999080150203990547 ) ) ;
#25024 = ORIENTED_EDGE ( 'NONE', *, *, #31987, .F. ) ;
#25025 = CARTESIAN_POINT ( 'NONE',  ( 37.00000000000000711, -10.14433819232439049, -6.753013023069681431 ) ) ;
#25026 = LINE ( 'NONE', #15670, #62699 ) ;
#25027 = EDGE_CURVE ( 'NONE', #36952, #25258, #24312, .T. ) ;
#25028 = AXIS2_PLACEMENT_3D ( 'NONE', #37928, #38924, #54219 ) ;
#25029 = LINE ( 'NONE', #4425, #2162 ) ;
#25030 = CARTESIAN_POINT ( 'NONE',  ( 0.6473888112830274988, -6.470260187014647890, -10.54705164520785132 ) ) ;
#25031 = CARTESIAN_POINT ( 'NONE',  ( -22.27720387087365239, -0.5572161790459744246, -3.639274226782821753 ) ) ;
#25032 = CYLINDRICAL_SURFACE ( 'NONE', #56922, 5.000000000000000888 ) ;
#25033 = CARTESIAN_POINT ( 'NONE',  ( 0.2646305136544072623, -4.312539723326057839, -11.46223899740604502 ) ) ;
#25034 = CARTESIAN_POINT ( 'NONE',  ( -37.00000000000000711, -0.01609748574453131326, 11.74614673114904129 ) ) ;
#25035 = CARTESIAN_POINT ( 'NONE',  ( -4.590058209962335489, 6.612760447609789871, 25.00000000000000000 ) ) ;
#25037 = EDGE_LOOP ( 'NONE', ( #4903, #64487, #17496, #22846 ) ) ;
#25036 = DIRECTION ( 'NONE',  ( -1.000000000000000000, 0.000000000000000000, 0.000000000000000000 ) ) ;
#25038 = EDGE_CURVE ( 'NONE', #1795, #27199, #8187, .T. ) ;
#25039 = CARTESIAN_POINT ( 'NONE',  ( -35.00000000000000000, 2.021542716731397071, 12.01765980939842748 ) ) ;
#25040 = ORIENTED_EDGE ( 'NONE', *, *, #7397, .F. ) ;
#25041 = DIRECTION ( 'NONE',  ( 1.000000000000000000, 0.000000000000000000, -0.000000000000000000 ) ) ;
#25042 = EDGE_LOOP ( 'NONE', ( #57772, #34685, #42837, #57405 ) ) ;
#25043 = EDGE_CURVE ( 'NONE', #173, #38028, #45518, .T. ) ;
#25044 = EDGE_LOOP ( 'NONE', ( #21576, #14783, #32728, #1935 ) ) ;
#25045 = CARTESIAN_POINT ( 'NONE',  ( 0.5547464869798220954, -12.33891836761637073, 0.3049355384528578683 ) ) ;
#25046 = CARTESIAN_POINT ( 'NONE',  ( 5.516018279890452902, -0.0002248006052448983238, -0.006771744149385263388 ) ) ;
#25047 = DIRECTION ( 'NONE',  ( 0.000000000000000000, -0.8835120444460178302, -0.4684084406997996441 ) ) ;
#25048 = DIRECTION ( 'NONE',  ( 1.000000000000000000, 0.000000000000000000, -0.000000000000000000 ) ) ;
#25049 = CARTESIAN_POINT ( 'NONE',  ( 2.241509619876138615, -7.511759925807386828, -1.363398699156125327 ) ) ;
#25050 = EDGE_CURVE ( 'NONE', #59201, #24026, #15792, .T. ) ;
#25051 = CARTESIAN_POINT ( 'NONE',  ( 37.00000000000000711, 11.23004253107771255, 4.732539170486137259 ) ) ;
#25052 = SHAPE_REPRESENTATION ( 'main drive axle', ( #24966 ), #2684 ) ;
#25053 = VERTEX_POINT ( 'NONE', #1118 ) ;
#25054 = CARTESIAN_POINT ( 'NONE',  ( 2.705197763288540003, -6.142723737672409534, 4.789125516644094915 ) ) ;
#25055 = DIRECTION ( 'NONE',  ( -1.000000000000000000, 0.000000000000000000, 0.000000000000000000 ) ) ;
#25056 = CARTESIAN_POINT ( 'NONE',  ( 0.2652384770603646302, -7.820955051613265319, -9.423432754625816088 ) ) ;
#25057 = ORIENTED_EDGE ( 'NONE', *, *, #52715, .F. ) ;
#25058 = CIRCLE ( 'NONE', #33559, 12.18650000000000055 ) ;
#25059 = EDGE_CURVE ( 'NONE', #54185, #38600, #21051, .T. ) ;
#25060 = CIRCLE ( 'NONE', #58015, 2.899999999999994582 ) ;
#25061 =( BOUNDED_SURFACE ( )  B_SPLINE_SURFACE ( 3, 1, ( 
 ( #6396, #26666 ),
 ( #46961, #1419 ),
 ( #10711, #11689 ),
 ( #31971, #6732 ) ),
 .UNSPECIFIED., .F., .F., .F. ) 
 B_SPLINE_SURFACE_WITH_KNOTS ( ( 4, 4 ),
 ( 2, 2 ),
 ( 0.000000000000000000, 1.000000000000000000 ),
 ( 0.000000000000000000, 1.000000000000000000 ),
 .UNSPECIFIED. ) 
 GEOMETRIC_REPRESENTATION_ITEM ( )  RATIONAL_B_SPLINE_SURFACE ( (
 ( 1.000000000000000000, 1.000000000000000000),
 ( 0.6933888150995267674, 0.9895912004443193632),
 ( 0.6933888150995267674, 0.9895912004443193632),
 ( 1.000000000000000000, 1.000000000000000000) ) ) 
 REPRESENTATION_ITEM ( '' )  SURFACE ( )  );
#25062 = CARTESIAN_POINT ( 'NONE',  ( 49.66779747649341914, -0.06758380666731210462, 4.082965791224114405 ) ) ;
#25063 = DIRECTION ( 'NONE',  ( -1.000000000000000000, 0.000000000000000000, 0.000000000000000000 ) ) ;
#25064 = DIRECTION ( 'NONE',  ( -1.000000000000000000, 0.000000000000000000, 0.000000000000000000 ) ) ;
#25065 = ORIENTED_EDGE ( 'NONE', *, *, #23960, .T. ) ;
#25066 = DIRECTION ( 'NONE',  ( -1.000000000000000000, 0.000000000000000000, 0.000000000000000000 ) ) ;
#25067 = CARTESIAN_POINT ( 'NONE',  ( 16.25676674326443560, -34.36623312464853797, 6.550321452246427256 ) ) ;
#25068 = CARTESIAN_POINT ( 'NONE',  ( 2.000000000000001776, 4.444115772890187444, -5.163689623839299081 ) ) ;
#25069 = EDGE_CURVE ( 'NONE', #29278, #29745, #40197, .T. ) ;
#25070 = CIRCLE ( 'NONE', #10198, 12.18650000000000411 ) ;
#25071 = B_SPLINE_CURVE_WITH_KNOTS ( 'NONE', 3,
 ( #21471, #46099, #16487, #65680, #5539, #40421 ),
 .UNSPECIFIED., .F., .F.,
 ( 4, 2, 4 ),
 ( 0.0001654224980408457906, 0.0006219428995476565265, 0.001078463301054467154 ),
 .UNSPECIFIED. ) ;
#25072 = CYLINDRICAL_SURFACE ( 'NONE', #33123, 12.18650000000000055 ) ;
#25073 = DIRECTION ( 'NONE',  ( 0.000000000000000000, -0.9105187689795911643, 0.4134677391718608597 ) ) ;
#25074 = VERTEX_POINT ( 'NONE', #61616 ) ;
#25075 = CARTESIAN_POINT ( 'NONE',  ( -35.04660725145885891, -0.007231372203124366085, -0.009947898977309622276 ) ) ;
#25076 = CARTESIAN_POINT ( 'NONE',  ( 0.3106921474978477371, -12.11369598333778441, 1.896868624983024887 ) ) ;
#25077 = CYLINDRICAL_SURFACE ( 'NONE', #60474, 17.25474371510545879 ) ;
#25078 = ORIENTED_EDGE ( 'NONE', *, *, #32758, .F. ) ;
#25079 = CARTESIAN_POINT ( 'NONE',  ( 35.00000000000000000, 5.636262487437473823, 10.80478261802175233 ) ) ;
#25080 = CARTESIAN_POINT ( 'NONE',  ( 2.000000000000001776, 3.805198749487436416, 5.799611601383225512 ) ) ;
#25081 = EDGE_LOOP ( 'NONE', ( #20892, #11927, #47545, #21655 ) ) ;
#25082 = EDGE_CURVE ( 'NONE', #30859, #42091, #33844, .T. ) ;
#25083 = ADVANCED_FACE ( 'NONE', ( #17398 ), #41331, .T. ) ;
#25084 = EDGE_LOOP ( 'NONE', ( #48755, #23196, #23275, #20215 ) ) ;
#25085 = ORIENTED_EDGE ( 'NONE', *, *, #13216, .T. ) ;
#25086 = EDGE_CURVE ( 'NONE', #53149, #10035, #63551, .T. ) ;
#25087 = VERTEX_POINT ( 'NONE', #36358 ) ;
#25088 = DIRECTION ( 'NONE',  ( 0.000000000000000000, 0.000000000000000000, 1.000000000000000000 ) ) ;
#25089 = DIRECTION ( 'NONE',  ( 0.000000000000000000, 0.000000000000000000, -1.000000000000000000 ) ) ;
#25090 = CARTESIAN_POINT ( 'NONE',  ( 0.000000000000000000, 6.164400007374793766, -2.900694413976553143 ) ) ;
#25091 = DIRECTION ( 'NONE',  ( -1.000000000000000000, 0.000000000000000000, 0.000000000000000000 ) ) ;
#25092 = CARTESIAN_POINT ( 'NONE',  ( -17.92531974009704498, -28.72851451116432031, 8.222150688345376324 ) ) ;
#25093 = CARTESIAN_POINT ( 'NONE',  ( 35.00000000000000000, 4.705694406421931860E-17, -3.469127814946512892E-15 ) ) ;
#25095 = VERTEX_POINT ( 'NONE', #27043 ) ;
#25094 = CYLINDRICAL_SURFACE ( 'NONE', #39349, 12.74999999999999822 ) ;
#25096 = FACE_OUTER_BOUND ( 'NONE', #61398, .T. ) ;
#25097 = ORIENTED_EDGE ( 'NONE', *, *, #10374, .F. ) ;
#25098 = CARTESIAN_POINT ( 'NONE',  ( -36.00000000000000711, -11.66664283989676321, -5.143145423404404504 ) ) ;
#25099 = ORIENTED_EDGE ( 'NONE', *, *, #38369, .T. ) ;
#25100 = ORIENTED_EDGE ( 'NONE', *, *, #44272, .F. ) ;
#25101 = CARTESIAN_POINT ( 'NONE',  ( 0.3278977287071288549, 9.554671284920413399, -7.693417476735430860 ) ) ;
#25102 = CARTESIAN_POINT ( 'NONE',  ( 8.295782569430503628, -27.33295754267858158, 14.98640435465113541 ) ) ;
#25103 = EDGE_CURVE ( 'NONE', #2444, #38347, #41671, .T. ) ;
#25104 = CARTESIAN_POINT ( 'NONE',  ( 35.00000000000000000, 5.927257550915316919, -10.64792938439757641 ) ) ;
#25105 = LINE ( 'NONE', #5495, #8945 ) ;
#25106 = AXIS2_PLACEMENT_3D ( 'NONE', #3520, #17804, #33426 ) ;
#25107 = FACE_OUTER_BOUND ( 'NONE', #64573, .T. ) ;
#25108 = CARTESIAN_POINT ( 'NONE',  ( -36.00000000000000711, 2.080187960898736588, -12.57916205664479214 ) ) ;
#25109 = VERTEX_POINT ( 'NONE', #61964 ) ;
#25110 = EDGE_CURVE ( 'NONE', #1896, #39587, #21090, .T. ) ;
#25111 = AXIS2_PLACEMENT_3D ( 'NONE', #12439, #31740, #53364 ) ;
#25112 = VERTEX_POINT ( 'NONE', #1461 ) ;
#25113 = CARTESIAN_POINT ( 'NONE',  ( -27.35552965826137140, -2.548625910254533888, -1.773915698030580357 ) ) ;
#25114 = ORIENTED_EDGE ( 'NONE', *, *, #35099, .T. ) ;
#25115 = B_SPLINE_CURVE_WITH_KNOTS ( 'NONE', 3,
 ( #7422, #17755, #22070, #27709, #48015, #57672, #12093 ),
 .UNSPECIFIED., .F., .F.,
 ( 4, 3, 4 ),
 ( 2.200004060863483116E-15, 0.002398160485434652853, 0.005002426799381861841 ),
 .UNSPECIFIED. ) ;
#25116 = ORIENTED_EDGE ( 'NONE', *, *, #49877, .T. ) ;
#25117 = DIRECTION ( 'NONE',  ( 1.000000000000000000, 0.000000000000000000, -0.000000000000000000 ) ) ;
#25118 = CARTESIAN_POINT ( 'NONE',  ( 0.3223008802179278542, 10.49760329338528386, -6.343104382804205521 ) ) ;
#25119 = DIRECTION ( 'NONE',  ( 0.000000000000000000, -1.000000000000000000, 0.000000000000000000 ) ) ;
#25120 = CARTESIAN_POINT ( 'NONE',  ( 17.09299993145517860, 9.325632684014761864, 7.625298650601195050 ) ) ;
#25121 = CARTESIAN_POINT ( 'NONE',  ( 2.305787727787084407, 7.654065630109506913, 0.1666591538752955071 ) ) ;
#25122 = CARTESIAN_POINT ( 'NONE',  ( -10.37734985215438499, -3.972422271833704777, -11.32510580359292618 ) ) ;
#25123 = DIRECTION ( 'NONE',  ( 0.3771207168306929813, -0.000000000000000000, 0.9261641133930337277 ) ) ;
#25124 = EDGE_LOOP ( 'NONE', ( #36357, #1110, #31974, #19843 ) ) ;
#25125 = EDGE_LOOP ( 'NONE', ( #23968, #38597, #12629, #60193 ) ) ;
#25126 = LINE ( 'NONE', #60358, #45538 ) ;
#25127 = CARTESIAN_POINT ( 'NONE',  ( -35.00000000000000000, -9.700295462048607931, -7.376655759824990000 ) ) ;
#25128 = CARTESIAN_POINT ( 'NONE',  ( -35.00000000000000000, 0.000000000000000000, 0.000000000000000000 ) ) ;
#25129 = DIRECTION ( 'NONE',  ( 0.000000000000000000, 0.000000000000000000, 1.000000000000000000 ) ) ;
#25130 = CARTESIAN_POINT ( 'NONE',  ( -22.66110217412718342, -4.573370147466322422, 1.880032915665391879 ) ) ;
#25131 = EDGE_CURVE ( 'NONE', #56567, #44942, #42298, .T. ) ;
#25132 = CARTESIAN_POINT ( 'NONE',  ( 35.00000000000000000, 0.4993900848169179896, 12.17626345777662600 ) ) ;
#25133 = DIRECTION ( 'NONE',  ( 1.000000000000000000, 0.000000000000000000, -0.000000000000000000 ) ) ;
#25134 = CARTESIAN_POINT ( 'NONE',  ( 0.9232058338315058954, -12.34162163148532798, -1.793035206307472151 ) ) ;
#25135 = ORIENTED_EDGE ( 'NONE', *, *, #22590, .T. ) ;
#25136 = CARTESIAN_POINT ( 'NONE',  ( 2.899286259009687949, -0.3564726075923954629, 7.845618522360449987 ) ) ;
#25137 = CARTESIAN_POINT ( 'NONE',  ( 0.3040950598368152291, 10.49113473328039170, -6.347045025870654555 ) ) ;
#25138 = CARTESIAN_POINT ( 'NONE',  ( 10.63582125257018163, -33.14335888457333112, 11.52436878476033932 ) ) ;
#25139 = EDGE_CURVE ( 'NONE', #16920, #53925, #37333, .T. ) ;
#25140 = AXIS2_PLACEMENT_3D ( 'NONE', #56584, #21978, #11344 ) ;
#25141 = CARTESIAN_POINT ( 'NONE',  ( -1.754394376714002002, -31.09667363889299097, -14.37851519254829391 ) ) ;
#25142 = DIRECTION ( 'NONE',  ( 0.000000000000000000, 0.01356324068817998940, -0.9999080150203990547 ) ) ;
#25143 = VERTEX_POINT ( 'NONE', #32342 ) ;
#25144 = CARTESIAN_POINT ( 'NONE',  ( 37.00000000000000711, 8.699265615723106748, 8.534258022645994757 ) ) ;
#25145 = CARTESIAN_POINT ( 'NONE',  ( 34.00000000000000000, 15.00000000000000000, 1.836970198721028406E-15 ) ) ;
#25146 = CARTESIAN_POINT ( 'NONE',  ( 12.57831868240780082, -29.25370879966640203, -4.768001503383415773 ) ) ;
#25147 = EDGE_LOOP ( 'NONE', ( #30087, #21206, #1849, #32121 ) ) ;
#25148 = DIRECTION ( 'NONE',  ( 0.000000000000000000, 0.01356324068818000328, -0.9999080150203990547 ) ) ;
#25149 = DIRECTION ( 'NONE',  ( 0.000000000000000000, 0.01356324068817992175, -0.9999080150203990547 ) ) ;
#25150 = CARTESIAN_POINT ( 'NONE',  ( 5.514624014163232779, 0.004045310349816140343, 0.0008859786816842230061 ) ) ;
#25151 = ADVANCED_FACE ( 'NONE', ( #7080 ), #57970, .T. ) ;
#25153 = ORIENTED_EDGE ( 'NONE', *, *, #53859, .F. ) ;
#25152 = DIRECTION ( 'NONE',  ( 0.000000000000000000, 0.01356324068817998940, -0.9999080150203989437 ) ) ;
#25154 = CARTESIAN_POINT ( 'NONE',  ( -27.09030469827879628, 2.239626370111425846, 0.5638997280369931753 ) ) ;
#25155 = CARTESIAN_POINT ( 'NONE',  ( -22.71097035706202405, -4.965150228107763297, -0.4203397252017324615 ) ) ;
#25156 = ORIENTED_EDGE ( 'NONE', *, *, #30362, .T. ) ;
#25157 = CARTESIAN_POINT ( 'NONE',  ( 0.2956976708475453353, 7.708404409946655989, 9.528782683728111991 ) ) ;
#25158 = CARTESIAN_POINT ( 'NONE',  ( -8.891032880924177206, 12.93614229090409395, -3.860857758255646921 ) ) ;
#25159 = CARTESIAN_POINT ( 'NONE',  ( 37.00000000000000711, -2.905556151562703082, -11.38112321385050052 ) ) ;
#25160 = CARTESIAN_POINT ( 'NONE',  ( 9.879977921069958313, 7.798719617128603510, -11.02431057014362992 ) ) ;
#25161 = FACE_OUTER_BOUND ( 'NONE', #25670, .T. ) ;
#25162 = CARTESIAN_POINT ( 'NONE',  ( -18.01037762727211700, 3.267117315390755117, 13.10031058145693983 ) ) ;
#25163 = DIRECTION ( 'NONE',  ( 1.000000000000000000, -0.000000000000000000, 0.000000000000000000 ) ) ;
#25164 = ORIENTED_EDGE ( 'NONE', *, *, #17512, .F. ) ;
#25165 = CYLINDRICAL_SURFACE ( 'NONE', #8754, 12.18650000000000055 ) ;
#25166 = ORIENTED_EDGE ( 'NONE', *, *, #32170, .T. ) ;
#25167 = LINE ( 'NONE', #46435, #45995 ) ;
#25168 = DIRECTION ( 'NONE',  ( 0.000000000000000000, 0.01356324068817991828, -0.9999080150203990547 ) ) ;
#25169 = ORIENTED_EDGE ( 'NONE', *, *, #12852, .F. ) ;
#25170 = CARTESIAN_POINT ( 'NONE',  ( -35.00000000000000000, -11.47561260193580779, 5.556331110570367215 ) ) ;
#25171 = CARTESIAN_POINT ( 'NONE',  ( -27.27855387000350262, -12.26939275170277632, 5.631341004100471892 ) ) ;
#25172 = AXIS2_PLACEMENT_3D ( 'NONE', #29675, #19736, #60606 ) ;
#25173 = CYLINDRICAL_SURFACE ( 'NONE', #45638, 5.000000000000000888 ) ;
#25174 = EDGE_LOOP ( 'NONE', ( #56687, #6404, #23725, #47792 ) ) ;
#25175 = VERTEX_POINT ( 'NONE', #42631 ) ;
#25176 = CARTESIAN_POINT ( 'NONE',  ( 2.305787727787084407, 0.1666591538753756929, -7.654065630109506024 ) ) ;
#25177 = EDGE_CURVE ( 'NONE', #5644, #29486, #51909, .T. ) ;
#25178 = ORIENTED_EDGE ( 'NONE', *, *, #10821, .F. ) ;
#25179 = CARTESIAN_POINT ( 'NONE',  ( 23.91335571186425923, -9.465411751381743954, -7.380766550276687710 ) ) ;
#25180 = CIRCLE ( 'NONE', #16690, 5.000000000000000000 ) ;
#25181 = CARTESIAN_POINT ( 'NONE',  ( 2.000000000000001776, -6.606214214351077807, 2.114938770769887455 ) ) ;
#25182 = CARTESIAN_POINT ( 'NONE',  ( 42.50000000000000000, -2.710505431213761085E-17, 1.399999999999999911 ) ) ;
#25183 = CARTESIAN_POINT ( 'NONE',  ( 2.251152103363647239, 7.133254101175224626, -2.729599998984340470 ) ) ;
#25184 = EDGE_CURVE ( 'NONE', #25258, #57134, #50205, .T. ) ;
#25185 = CARTESIAN_POINT ( 'NONE',  ( -36.00000000000000711, -10.93004082984014147, -6.564808257521885793 ) ) ;
#25186 = DIRECTION ( 'NONE',  ( 1.000000000000000000, 0.000000000000000000, -0.000000000000000000 ) ) ;
#25187 = B_SPLINE_CURVE_WITH_KNOTS ( 'NONE', 3,
 ( #52948, #26695, #27661, #56969, #17040, #37971, #11393, #51661, #42282, #31667, #22027, #62575, #51977, #6105, #26362, #6421 ),
 .UNSPECIFIED., .F., .F.,
 ( 4, 3, 3, 3, 3, 4 ),
 ( 2.710505431213761085E-19, 0.0003017745587525231328, 0.0006035491769808708131, 0.0009053241094668120197, 0.001207275924539391717, 0.001510325902531780510 ),
 .UNSPECIFIED. ) ;
#25188 = DIRECTION ( 'NONE',  ( 1.000000000000000000, 0.000000000000000000, 0.000000000000000000 ) ) ;
#25189 = ORIENTED_EDGE ( 'NONE', *, *, #2612, .F. ) ;
#25190 = CARTESIAN_POINT ( 'NONE',  ( 1.198791140419100287, -11.96656299555083613, 3.806343609711079434 ) ) ;
#25191 = DIRECTION ( 'NONE',  ( 0.000000000000000000, 0.01356324068817992175, -0.9999080150203990547 ) ) ;
#25192 = CARTESIAN_POINT ( 'NONE',  ( 2.241352910868909643, 5.794346703933845433, 4.970878533273779709 ) ) ;
#25193 = CARTESIAN_POINT ( 'NONE',  ( 12.51553973845115841, 11.51522108451853121, -7.048732632201635262 ) ) ;
#25194 = DIRECTION ( 'NONE',  ( 0.000000000000000000, -0.01356324068817992175, 0.9999080150203990547 ) ) ;
#25195 = DIRECTION ( 'NONE',  ( -1.000000000000000000, 0.000000000000000000, 0.000000000000000000 ) ) ;
#25196 = CARTESIAN_POINT ( 'NONE',  ( 35.00000000000000000, 3.093009498343925134, -11.78745411414841016 ) ) ;
#25197 = LINE ( 'NONE', #45470, #6661 ) ;
#25198 = EDGE_CURVE ( 'NONE', #60941, #58003, #976, .T. ) ;
#25199 = ORIENTED_EDGE ( 'NONE', *, *, #36684, .T. ) ;
#25200 = DIRECTION ( 'NONE',  ( -1.000000000000000000, 0.000000000000000000, 0.000000000000000000 ) ) ;
#25201 = EDGE_CURVE ( 'NONE', #65337, #36759, #45200, .T. ) ;
#25202 = ORIENTED_EDGE ( 'NONE', *, *, #19878, .F. ) ;
#25203 = CARTESIAN_POINT ( 'NONE',  ( -3.552846699730117574, -9.406274435376895227, 7.462624784235579511 ) ) ;
#25204 = DIRECTION ( 'NONE',  ( -1.000000000000000000, 0.000000000000000000, 0.000000000000000000 ) ) ;
#25205 = CARTESIAN_POINT ( 'NONE',  ( -17.57509096728301046, 6.782429754866558191, -11.67417802825193895 ) ) ;
#25206 = CARTESIAN_POINT ( 'NONE',  ( 2.000000000000001776, 1.779948802829816490, 6.576141558201244131 ) ) ;
#25207 = EDGE_CURVE ( 'NONE', #52121, #36243, #35971, .T. ) ;
#25208 = DIRECTION ( 'NONE',  ( 0.000000000000000000, -0.9868265225415244757, -0.1617819965527746984 ) ) ;
#25209 = EDGE_LOOP ( 'NONE', ( #49391, #51343, #58626, #24772 ) ) ;
#25210 = DIRECTION ( 'NONE',  ( -1.000000000000000000, 0.000000000000000000, 0.000000000000000000 ) ) ;
#25211 = CARTESIAN_POINT ( 'NONE',  ( 2.969415267404148739, 2.326350273511913258, -7.525730903320487108 ) ) ;
#25212 = DIRECTION ( 'NONE',  ( -1.000000000000000000, 0.000000000000000000, 0.000000000000000000 ) ) ;
#25213 = CARTESIAN_POINT ( 'NONE',  ( 2.665405856346785729, 5.274989403261000298, -7.981834391067653911 ) ) ;
#25214 = CIRCLE ( 'NONE', #7216, 12.75000000000000178 ) ;
#25215 = ADVANCED_FACE ( 'NONE', ( #4316 ), #19925, .T. ) ;
#25216 = CARTESIAN_POINT ( 'NONE',  ( -17.25801985322950216, -6.481189176515793626, 10.10068109367541034 ) ) ;
#25217 = LINE ( 'NONE', #57132, #3238 ) ;
#25218 = VERTEX_POINT ( 'NONE', #63573 ) ;
#25219 = EDGE_CURVE ( 'NONE', #56892, #48293, #54030, .T. ) ;
#25220 = CARTESIAN_POINT ( 'NONE',  ( -27.08935880048797529, -0.5666837974560299251, 2.235999130319374029 ) ) ;
#25221 = EDGE_LOOP ( 'NONE', ( #61299, #56342, #3629, #47542 ) ) ;
#25222 = DIRECTION ( 'NONE',  ( 0.9606638835031803270, -0.1133241553124307438, 0.2535400141108146710 ) ) ;
#25223 = DIRECTION ( 'NONE',  ( 1.000000000000000000, 0.000000000000000000, 0.000000000000000000 ) ) ;
#25224 = CIRCLE ( 'NONE', #51781, 12.18650000000000055 ) ;
#25225 = CARTESIAN_POINT ( 'NONE',  ( 2.034671305879538483, 8.030508024280598178, -8.476347594674427555 ) ) ;
#25226 = CARTESIAN_POINT ( 'NONE',  ( 1.000000000000000888, 7.484036900328563391, 0.4890722589969403455 ) ) ;
#25227 = ORIENTED_EDGE ( 'NONE', *, *, #2419, .F. ) ;
#25228 = AXIS2_PLACEMENT_3D ( 'NONE', #48881, #28914, #49223 ) ;
#25229 = ORIENTED_EDGE ( 'NONE', *, *, #40260, .F. ) ;
#25231 = EDGE_CURVE ( 'NONE', #34941, #37781, #20051, .T. ) ;
#25230 = CARTESIAN_POINT ( 'NONE',  ( -27.10113028276028757, 2.245923868550873781, -0.6639289823109628674 ) ) ;
#25232 = EDGE_LOOP ( 'NONE', ( #59032, #7750, #33294, #38915 ) ) ;
#25233 = CARTESIAN_POINT ( 'NONE',  ( 2.247206125382826158, -6.554642244888441382, -3.917979829727982644 ) ) ;
#25235 = LINE ( 'NONE', #61146, #26827 ) ;
#25234 =( BOUNDED_SURFACE ( )  B_SPLINE_SURFACE ( 3, 1, ( 
 ( #30943, #60888 ),
 ( #703, #31592 ),
 ( #41238, #15329 ),
 ( #55896, #41572 ) ),
 .UNSPECIFIED., .F., .F., .F. ) 
 B_SPLINE_SURFACE_WITH_KNOTS ( ( 4, 4 ),
 ( 2, 2 ),
 ( 0.000000000000000000, 1.000000000000000000 ),
 ( 0.000000000000000000, 1.000000000000000000 ),
 .UNSPECIFIED. ) 
 GEOMETRIC_REPRESENTATION_ITEM ( )  RATIONAL_B_SPLINE_SURFACE ( (
 ( 1.000000000000000000, 1.000000000000000000),
 ( 0.9932032654565553509, 0.8386279382598736953),
 ( 0.9932032654565553509, 0.8386279382598736953),
 ( 1.000000000000000000, 1.000000000000000000) ) ) 
 REPRESENTATION_ITEM ( '' )  SURFACE ( )  );
#25236 = CARTESIAN_POINT ( 'NONE',  ( -22.27721056931765631, -3.486117586310729433, -1.183805672860834379 ) ) ;
#25237 = CARTESIAN_POINT ( 'NONE',  ( 1.634816307074480779, 9.253014110594536490, 8.702988562438394027 ) ) ;
#25238 = CARTESIAN_POINT ( 'NONE',  ( 35.00000000000000000, -4.986700593229777212, -10.63508530065520219 ) ) ;
#25239 = FACE_OUTER_BOUND ( 'NONE', #43389, .T. ) ;
#25240 = CARTESIAN_POINT ( 'NONE',  ( -18.56512981111246319, -11.93407345808114073, 1.298380824258862587 ) ) ;
#25241 = ORIENTED_EDGE ( 'NONE', *, *, #46475, .F. ) ;
#25242 = CARTESIAN_POINT ( 'NONE',  ( 0.2646305136544072623, -10.53923716745251404, 6.237419468587042104 ) ) ;
#25243 = ORIENTED_EDGE ( 'NONE', *, *, #38369, .F. ) ;
#25244 = DIRECTION ( 'NONE',  ( 0.000000000000000000, -0.01356324068817991828, 0.9999080150203990547 ) ) ;
#25245 = DIRECTION ( 'NONE',  ( 1.977578355587678392E-17, -0.1764146379942750364, -0.9843159429275484262 ) ) ;
#25246 = VERTEX_POINT ( 'NONE', #2443 ) ;
#25247 = CARTESIAN_POINT ( 'NONE',  ( -22.70624764888619751, -0.7939291279022604453, 5.190207123845781645 ) ) ;
#25248 = VERTEX_POINT ( 'NONE', #24926 ) ;
#25249 = DIRECTION ( 'NONE',  ( 1.000000000000000000, 0.000000000000000000, 0.000000000000000000 ) ) ;
#25250 = CARTESIAN_POINT ( 'NONE',  ( 6.520882551146788941, -4.687253057175320592, -12.66502263360881564 ) ) ;
#25251 = CARTESIAN_POINT ( 'NONE',  ( 5.514970785353741078, 0.001897634820904952127, 0.004324946436530311550 ) ) ;
#25252 = CARTESIAN_POINT ( 'NONE',  ( 3.031336079629294744, 7.268683861177205330, -3.088871717871271461 ) ) ;
#25253 = ORIENTED_EDGE ( 'NONE', *, *, #65521, .T. ) ;
#25254 = ORIENTED_EDGE ( 'NONE', *, *, #34136, .F. ) ;
#25255 = FACE_OUTER_BOUND ( 'NONE', #25642, .T. ) ;
#25256 = ORIENTED_EDGE ( 'NONE', *, *, #46210, .T. ) ;
#25257 = CARTESIAN_POINT ( 'NONE',  ( 0.3675815128205912052, 11.62724744438071056, -3.951233083390353062 ) ) ;
#25258 = VERTEX_POINT ( 'NONE', #42981 ) ;
#25259 = ORIENTED_EDGE ( 'NONE', *, *, #64177, .F. ) ;
#25260 = ORIENTED_EDGE ( 'NONE', *, *, #21842, .F. ) ;
#25261 = CARTESIAN_POINT ( 'NONE',  ( 36.00000000000000711, -10.68873102412837639, 6.950793414699901085 ) ) ;
#25263 = AXIS2_PLACEMENT_3D ( 'NONE', #43084, #5663, #16272 ) ;
#25262 = CARTESIAN_POINT ( 'NONE',  ( 19.41740522748897391, -28.99999999999999289, 5.485033347092790557 ) ) ;
#25264 = EDGE_CURVE ( 'NONE', #5329, #29772, #10483, .T. ) ;
#25265 = CARTESIAN_POINT ( 'NONE',  ( 2.573738926104376379, -1.112690714006486115, -7.664876274722925764 ) ) ;
#25266 = DIRECTION ( 'NONE',  ( 1.000000000000000000, 0.000000000000000000, -0.000000000000000000 ) ) ;
#25267 = CARTESIAN_POINT ( 'NONE',  ( -35.04643116707788408, -0.001845126042319261694, -0.01204777744935776884 ) ) ;
#25268 = ORIENTED_EDGE ( 'NONE', *, *, #8600, .F. ) ;
#25269 = CARTESIAN_POINT ( 'NONE',  ( 35.00000000000000000, -8.534258022646033837, 8.699265615723071221 ) ) ;
#25270 = ORIENTED_EDGE ( 'NONE', *, *, #44434, .F. ) ;
#25271 = CYLINDRICAL_SURFACE ( 'NONE', #54003, 3.309571291727934295 ) ;
#25272 = CARTESIAN_POINT ( 'NONE',  ( 35.00000000000000000, 4.705694406421931860E-17, -3.469127814946512892E-15 ) ) ;
#25273 = CIRCLE ( 'NONE', #32698, 12.18649999999999878 ) ;
#25274 = ORIENTED_EDGE ( 'NONE', *, *, #47530, .F. ) ;
#25275 = CARTESIAN_POINT ( 'NONE',  ( 0.3106921474978440734, -10.73438344699975389, 5.925601485921636602 ) ) ;
#25276 = DIRECTION ( 'NONE',  ( -0.000000000000000000, -0.000000000000000000, -1.000000000000000000 ) ) ;
#25277 = B_SPLINE_CURVE_WITH_KNOTS ( 'NONE', 3,
 ( #28652, #8063, #58950, #58617, #42613, #3082, #53624, #37656, #27659, #62915, #8377, #37968, #58269, #12690, #32632, #48317 ),
 .UNSPECIFIED., .F., .F.,
 ( 4, 3, 3, 3, 3, 4 ),
 ( 1.843143693225351375E-18, 6.991367980366411871E-05, 0.0001398269368981365046, 0.0002097400188389092002, 0.0002811534801551363234, 0.0003526297678872491494 ),
 .UNSPECIFIED. ) ;
#25278 = CARTESIAN_POINT ( 'NONE',  ( 2.260457164927179630, -6.685239696063459469, -3.699855525213223473 ) ) ;
#25279 = CIRCLE ( 'NONE', #7227, 7.499999999999988454 ) ;
#25280 = ADVANCED_FACE ( 'NONE', ( #38312 ), #63256, .T. ) ;
#25281 = VERTEX_POINT ( 'NONE', #19618 ) ;
#25282 = CARTESIAN_POINT ( 'NONE',  ( 2.280717697723838810, -7.645922213779908994, 0.1564731737569851899 ) ) ;
#25283 = ORIENTED_EDGE ( 'NONE', *, *, #54721, .F. ) ;
#25284 = EDGE_CURVE ( 'NONE', #9839, #42155, #25360, .T. ) ;
#25285 = DIRECTION ( 'NONE',  ( -1.000000000000000000, -0.000000000000000000, -0.000000000000000000 ) ) ;
#25286 = CARTESIAN_POINT ( 'NONE',  ( -20.79170840334646542, -12.91784323155722269, -3.921648409140116698 ) ) ;
#25287 = CARTESIAN_POINT ( 'NONE',  ( -47.00000000000000711, 0.000000000000000000, 0.000000000000000000 ) ) ;
#25288 = CARTESIAN_POINT ( 'NONE',  ( 2.251139882113692536, -3.710800524305181369, -6.675617500148306682 ) ) ;
#25289 = EDGE_CURVE ( 'NONE', #33280, #19513, #54541, .T. ) ;
#25290 = FACE_OUTER_BOUND ( 'NONE', #54695, .T. ) ;
#25291 = ORIENTED_EDGE ( 'NONE', *, *, #11842, .T. ) ;
#25292 = CARTESIAN_POINT ( 'NONE',  ( -37.00000000000000711, 0.000000000000000000, 0.000000000000000000 ) ) ;
#25293 = DIRECTION ( 'NONE',  ( 1.000000000000000000, 0.000000000000000000, -0.000000000000000000 ) ) ;
#25294 = DIRECTION ( 'NONE',  ( 0.000000000000000000, -0.01356324068817991828, 0.9999080150203990547 ) ) ;
#25295 = DIRECTION ( 'NONE',  ( -1.000000000000000000, -1.836970198721029688E-16, -0.000000000000000000 ) ) ;
#25296 = EDGE_CURVE ( 'NONE', #33192, #50535, #60481, .T. ) ;
#25297 = CYLINDRICAL_SURFACE ( 'NONE', #43507, 5.000000000000000888 ) ;
#25298 = AXIS2_PLACEMENT_3D ( 'NONE', #53905, #22992, #8033 ) ;
#25299 = EDGE_CURVE ( 'NONE', #6060, #49356, #19280, .T. ) ;
#25300 = FACE_OUTER_BOUND ( 'NONE', #34240, .T. ) ;
#25301 = EDGE_CURVE ( 'NONE', #53510, #32724, #17727, .T. ) ;
#25302 = CARTESIAN_POINT ( 'NONE',  ( 37.00000000000000711, 4.705694406421931860E-17, -3.469127814946512892E-15 ) ) ;
#25303 = LINE ( 'NONE', #45584, #28010 ) ;
#25304 = B_SPLINE_CURVE_WITH_KNOTS ( 'NONE', 3,
 ( #65579, #20049, #440, #49663, #60607, #4103 ),
 .UNSPECIFIED., .F., .F.,
 ( 4, 2, 4 ),
 ( 0.000000000000000000, 0.0004528561986909385552, 0.0009057123973818773273 ),
 .UNSPECIFIED. ) ;
#25305 = EDGE_CURVE ( 'NONE', #38593, #47315, #58289, .T. ) ;
#25306 = CIRCLE ( 'NONE', #32731, 12.18649999999999878 ) ;
#25307 = ORIENTED_EDGE ( 'NONE', *, *, #27736, .F. ) ;
#25308 = EDGE_CURVE ( 'NONE', #41673, #4686, #24589, .T. ) ;
#25309 = CIRCLE ( 'NONE', #22128, 7.938172270156617749 ) ;
#25310 = AXIS2_PLACEMENT_3D ( 'NONE', #50041, #65322, #5486 ) ;
#25311 = VERTEX_POINT ( 'NONE', #14583 ) ;
#25312 = CARTESIAN_POINT ( 'NONE',  ( 2.000000000000001776, 4.376687952327335651, 5.220963330856624118 ) ) ;
#25313 = CARTESIAN_POINT ( 'NONE',  ( 20.00005080000000035, 0.000000000000000000, 0.000000000000000000 ) ) ;
#25314 = LINE ( 'NONE', #51596, #18382 ) ;
#25315 = EDGE_CURVE ( 'NONE', #51800, #30093, #24355, .T. ) ;
#25316 = CIRCLE ( 'NONE', #18972, 5.000000000000000000 ) ;
#25317 = LINE ( 'NONE', #45591, #44563 ) ;
#25318 = ORIENTED_EDGE ( 'NONE', *, *, #14981, .T. ) ;
#25319 = ORIENTED_EDGE ( 'NONE', *, *, #7215, .T. ) ;
#25320 = CIRCLE ( 'NONE', #1986, 5.000000000000000888 ) ;
#25321 = ORIENTED_EDGE ( 'NONE', *, *, #60288, .F. ) ;
#25322 = CARTESIAN_POINT ( 'NONE',  ( 3.047904605210376427, 3.098478597269376245, -7.270585891216581054 ) ) ;
#25323 = DIRECTION ( 'NONE',  ( 0.000000000000000000, 0.9551603052523468529, -0.2960891610144545938 ) ) ;
#25324 = ORIENTED_EDGE ( 'NONE', *, *, #65588, .T. ) ;
#25325 = DIRECTION ( 'NONE',  ( 0.000000000000000000, 0.01356324068817999808, -0.9999080150203990547 ) ) ;
#25326 = CARTESIAN_POINT ( 'NONE',  ( 2.524535260912463386, -2.434550409953165850, 7.335347545455585205 ) ) ;
#25327 = ORIENTED_EDGE ( 'NONE', *, *, #14563, .T. ) ;
#25328 = FACE_OUTER_BOUND ( 'NONE', #14176, .T. ) ;
#25329 = CARTESIAN_POINT ( 'NONE',  ( 6.272189122743162315, -31.23296902231907879, -14.43357722546949162 ) ) ;
#25330 = CYLINDRICAL_SURFACE ( 'NONE', #34505, 4.999999999999999112 ) ;
#25331 = ORIENTED_EDGE ( 'NONE', *, *, #1738, .F. ) ;
#25332 = DIRECTION ( 'NONE',  ( 0.000000000000000000, 0.000000000000000000, 1.000000000000000000 ) ) ;
#25333 = ORIENTED_EDGE ( 'NONE', *, *, #47515, .F. ) ;
#25334 = CARTESIAN_POINT ( 'NONE',  ( 2.000000000000001776, 0.000000000000000000, 0.000000000000000000 ) ) ;
#25335 = VERTEX_POINT ( 'NONE', #46836 ) ;
#25336 = DIRECTION ( 'NONE',  ( 1.000000000000000000, 0.000000000000000000, 0.000000000000000000 ) ) ;
#25337 = DIRECTION ( 'NONE',  ( -1.000000000000000000, -1.836970198721029688E-16, -0.000000000000000000 ) ) ;
#25338 = CARTESIAN_POINT ( 'NONE',  ( -22.71097035706202405, -4.965150228107763297, -0.4203397252017324615 ) ) ;
#25339 = CARTESIAN_POINT ( 'NONE',  ( 1.547277799339154214, -6.911346840320659268, -10.62321481610077178 ) ) ;
#25340 = CARTESIAN_POINT ( 'NONE',  ( -22.71097035706202405, -4.089776368546547580, -2.846599994298351977 ) ) ;
#25341 = EDGE_CURVE ( 'NONE', #57308, #57915, #61518, .T. ) ;
#25343 = CARTESIAN_POINT ( 'NONE',  ( 37.00000000000000711, 4.705694406421931860E-17, -3.469127814946512892E-15 ) ) ;
#25342 = AXIS2_PLACEMENT_3D ( 'NONE', #47871, #11955, #51887 ) ;
#25344 = CARTESIAN_POINT ( 'NONE',  ( 0.2655924914740778742, -4.229867354073483021, -11.49267051747972523 ) ) ;
#25345 = CARTESIAN_POINT ( 'NONE',  ( -27.08416813689867908, 2.257587568255730037, -0.3912215308406206127 ) ) ;
#25346 = CARTESIAN_POINT ( 'NONE',  ( 36.00000000000000711, -7.238157050195554554, 10.49626516989278180 ) ) ;
#25348 = VERTEX_POINT ( 'NONE', #62134 ) ;
#25347 = CARTESIAN_POINT ( 'NONE',  ( 6.412959687766495165, -9.124421398965553820, 9.956605555149330655 ) ) ;
#25349 = CARTESIAN_POINT ( 'NONE',  ( -22.70624764888619751, -5.190207123845783421, -0.7939291279022795411 ) ) ;
#25350 = VERTEX_POINT ( 'NONE', #11266 ) ;
#25351 = VECTOR ( 'NONE', #37372, 1000.000000000000000 ) ;
#25352 = DIRECTION ( 'NONE',  ( 1.000000000000000000, 0.000000000000000000, -0.000000000000000000 ) ) ;
#25353 = ORIENTED_EDGE ( 'NONE', *, *, #916, .F. ) ;
#25354 = ORIENTED_EDGE ( 'NONE', *, *, #23204, .F. ) ;
#25355 = EDGE_CURVE ( 'NONE', #4031, #22247, #8227, .T. ) ;
#25356 = CARTESIAN_POINT ( 'NONE',  ( 0.3675815128205894289, 8.093875121226078662, 9.235491948680033758 ) ) ;
#25357 = DIRECTION ( 'NONE',  ( -1.000000000000000000, 0.000000000000000000, -0.000000000000000000 ) ) ;
#25358 = CARTESIAN_POINT ( 'NONE',  ( 5.515539859299206427, 0.005142293699651867729, -0.003193223631739272681 ) ) ;
#25359 = CARTESIAN_POINT ( 'NONE',  ( 0.2851083653049504285, -0.4107471485392698018, 13.49374991542258151 ) ) ;
#25360 = CIRCLE ( 'NONE', #7306, 7.499999999999988454 ) ;
#25361 = DIRECTION ( 'NONE',  ( 0.000000000000000000, 0.8169148498130255343, -0.5767582926624997830 ) ) ;
#25362 = ADVANCED_FACE ( 'NONE', ( #25239 ), #56842, .T. ) ;
#25363 = CARTESIAN_POINT ( 'NONE',  ( 6.361445718264521432, -4.355102044641763648, 25.00000000000000000 ) ) ;
#25364 = CIRCLE ( 'NONE', #40201, 2.899999999999995026 ) ;
#25365 = VECTOR ( 'NONE', #56594, 1000.000000000000000 ) ;
#25366 = ORIENTED_EDGE ( 'NONE', *, *, #21915, .T. ) ;
#25367 = CARTESIAN_POINT ( 'NONE',  ( 2.373367633546869193, -5.996611082971999629, 4.795703124519871352 ) ) ;
#25368 = CARTESIAN_POINT ( 'NONE',  ( 35.00000000000000000, -10.75351884295723970, 4.725891942574862448 ) ) ;
#25369 = CIRCLE ( 'NONE', #59355, 2.899999999999994582 ) ;
#25370 = CARTESIAN_POINT ( 'NONE',  ( 0.3675815128205894289, 12.04510820461659293, 2.391755495700645273 ) ) ;
#25371 = EDGE_CURVE ( 'NONE', #28701, #38380, #32790, .T. ) ;
#25372 = ORIENTED_EDGE ( 'NONE', *, *, #61870, .F. ) ;
#25373 = CIRCLE ( 'NONE', #48739, 12.18649999999999878 ) ;
#25374 = CARTESIAN_POINT ( 'NONE',  ( 0.3223008802179263554, -4.423848692584617659, -11.43958962819737124 ) ) ;
#25375 = DIRECTION ( 'NONE',  ( -1.000000000000000000, -0.000000000000000000, 0.000000000000000000 ) ) ;
#25376 = CARTESIAN_POINT ( 'NONE',  ( -37.00000000000000711, 0.4993900848167411310, 12.17626345777664021 ) ) ;
#25377 = CARTESIAN_POINT ( 'NONE',  ( -33.05588761701186939, -2.860689001541065313, -23.72276540370178566 ) ) ;
#25378 = ORIENTED_EDGE ( 'NONE', *, *, #58557, .F. ) ;
#25379 = CARTESIAN_POINT ( 'NONE',  ( 2.000000000000001776, 3.341639490130761114, 6.078525953551427996 ) ) ;
#25380 = LINE ( 'NONE', #56647, #40996 ) ;
#25381 = DIRECTION ( 'NONE',  ( -0.2415534870330798278, 0.000000000000000000, 0.9703875065674330003 ) ) ;
#25382 = EDGE_CURVE ( 'NONE', #12285, #50930, #32835, .T. ) ;
#25383 = VECTOR ( 'NONE', #28442, 1000.000000000000114 ) ;
#25384 = EDGE_CURVE ( 'NONE', #28435, #59321, #24971, .T. ) ;
#25385 = DIRECTION ( 'NONE',  ( -0.000000000000000000, -0.000000000000000000, -1.000000000000000000 ) ) ;
#25386 = DIRECTION ( 'NONE',  ( 0.000000000000000000, 0.4198891015602657650, -0.9075754196709565624 ) ) ;
#25387 = ORIENTED_EDGE ( 'NONE', *, *, #26109, .T. ) ;
#25388 = VECTOR ( 'NONE', #14542, 1000.000000000000000 ) ;
#25389 = DIRECTION ( 'NONE',  ( 0.000000000000000000, 0.01356324068817998940, -0.9999080150203990547 ) ) ;
#25390 = CARTESIAN_POINT ( 'NONE',  ( 2.320974307000889247, 2.464467181831794917, -11.75030150517671679 ) ) ;
#25391 = DIRECTION ( 'NONE',  ( 0.000000000000000000, 0.01356324068817998940, -0.9999080150203990547 ) ) ;
#25392 = EDGE_LOOP ( 'NONE', ( #11400, #1722, #15923, #20501 ) ) ;
#25393 = EDGE_CURVE ( 'NONE', #15725, #35492, #58351, .T. ) ;
#25394 = DIRECTION ( 'NONE',  ( 0.000000000000000000, 0.000000000000000000, -1.000000000000000000 ) ) ;
#25395 = DIRECTION ( 'NONE',  ( -1.000000000000000000, 0.000000000000000000, -0.000000000000000000 ) ) ;
#25396 = EDGE_LOOP ( 'NONE', ( #7301, #18145, #33342, #13948 ) ) ;
#25397 = EDGE_LOOP ( 'NONE', ( #22897, #25610 ) ) ;
#25398 = EDGE_LOOP ( 'NONE', ( #54489, #60214, #35357, #29461 ) ) ;
#25399 = AXIS2_PLACEMENT_3D ( 'NONE', #24163, #63408, #28495 ) ;
#25400 = AXIS2_PLACEMENT_3D ( 'NONE', #45512, #10589, #10936 ) ;
#25401 = EDGE_LOOP ( 'NONE', ( #3515, #29346, #32957, #59190 ) ) ;
#25402 = DIRECTION ( 'NONE',  ( 1.000000000000000000, -0.000000000000000000, 0.000000000000000000 ) ) ;
#25403 = CARTESIAN_POINT ( 'NONE',  ( 37.00000000000000711, 4.705694406421931860E-17, -3.469127814946512892E-15 ) ) ;
#25404 = AXIS2_PLACEMENT_3D ( 'NONE', #3674, #13920, #64160 ) ;
#25405 = DIRECTION ( 'NONE',  ( -1.000000000000000000, 0.000000000000000000, -0.000000000000000000 ) ) ;
#25406 = DIRECTION ( 'NONE',  ( 0.000000000000000000, 0.000000000000000000, 1.000000000000000000 ) ) ;
#25407 = CARTESIAN_POINT ( 'NONE',  ( -41.00000000000000711, -45.00200000000000244, 4.499999999999997335 ) ) ;
#25408 = CARTESIAN_POINT ( 'NONE',  ( -8.110750208426855679, -28.65453171997180348, 10.34333599818648608 ) ) ;
#25409 = CARTESIAN_POINT ( 'NONE',  ( 24.85730486487263491, 0.07226432089349320298, -13.50554067701254546 ) ) ;
#25411 = ORIENTED_EDGE ( 'NONE', *, *, #48608, .T. ) ;
#25410 = CARTESIAN_POINT ( 'NONE',  ( 0.2646305136544065406, 7.972778379581551889, 9.296005949277249769 ) ) ;
#25412 = DIRECTION ( 'NONE',  ( 0.000000000000000000, -0.9970832820307047317, -0.07632122047555403577 ) ) ;
#25413 = ORIENTED_EDGE ( 'NONE', *, *, #45284, .T. ) ;
#25414 = FACE_OUTER_BOUND ( 'NONE', #48898, .T. ) ;
#25415 = VERTEX_POINT ( 'NONE', #26547 ) ;
#25416 = AXIS2_PLACEMENT_3D ( 'NONE', #54974, #14401, #15702 ) ;
#25417 = B_SPLINE_CURVE_WITH_KNOTS ( 'NONE', 3,
 ( #55941, #10701, #61566, #21339, #5408, #20038, #5752, #26018, #30347, #41621 ),
 .UNSPECIFIED., .F., .F.,
 ( 4, 2, 2, 2, 4 ),
 ( 8.673617379884034509E-19, 0.0007817650899998000594, 0.001563530179999599251, 0.002345295269999397251, 0.003127060359999195467 ),
 .UNSPECIFIED. ) ;
#25418 = ORIENTED_EDGE ( 'NONE', *, *, #1666, .F. ) ;
#25419 = DIRECTION ( 'NONE',  ( -1.000000000000000000, 0.000000000000000000, 0.000000000000000000 ) ) ;
#25420 = CARTESIAN_POINT ( 'NONE',  ( 5.786001662380197530, -26.94056086434354924, 15.63186719136363401 ) ) ;
#25421 = CARTESIAN_POINT ( 'NONE',  ( 37.00000000000000711, 4.705694406421931860E-17, -3.469127814946512892E-15 ) ) ;
#25422 = ADVANCED_FACE ( 'NONE', ( #30547 ), #26036, .F. ) ;
#25423 = CYLINDRICAL_SURFACE ( 'NONE', #3705, 12.74999999999999822 ) ;
#25424 = CARTESIAN_POINT ( 'NONE',  ( 10.75853767213705225, 7.830989516993144051, 9.092612561015865680 ) ) ;
#25425 = CARTESIAN_POINT ( 'NONE',  ( 0.3164563675027652345, -12.03284811452138747, 2.365891945210773173 ) ) ;
#25426 = ORIENTED_EDGE ( 'NONE', *, *, #64861, .F. ) ;
#25427 = ADVANCED_FACE ( 'NONE', ( #61150 ), #15579, .T. ) ;
#25428 = ORIENTED_EDGE ( 'NONE', *, *, #55975, .T. ) ;
#25429 = DIRECTION ( 'NONE',  ( 1.000000000000000000, 0.000000000000000000, -0.000000000000000000 ) ) ;
#25430 = VERTEX_POINT ( 'NONE', #16252 ) ;
#25431 = ORIENTED_EDGE ( 'NONE', *, *, #52189, .F. ) ;
#25432 = ADVANCED_FACE ( 'NONE', ( #56147 ), #37874, .F. ) ;
#25433 = CARTESIAN_POINT ( 'NONE',  ( 35.00000000000000000, -9.430788938293991563, 7.718225330433904574 ) ) ;
#25434 = CARTESIAN_POINT ( 'NONE',  ( -27.08704841010922948, -2.291653842312380895, 0.1930432016059762668 ) ) ;
#25435 = CARTESIAN_POINT ( 'NONE',  ( -22.31328051695926007, 0.8849444482788259014, -3.685074213229314388 ) ) ;
#25436 = CARTESIAN_POINT ( 'NONE',  ( 17.75904445597924308, 6.994922235104493957, 9.764648471568612820 ) ) ;
#25437 = CARTESIAN_POINT ( 'NONE',  ( 2.276198483117260807, 7.644465698238550821, 0.1540629821338586058 ) ) ;
#25438 = DIRECTION ( 'NONE',  ( -1.000000000000000000, 0.000000000000000000, -0.000000000000000000 ) ) ;
#25439 = AXIS2_PLACEMENT_3D ( 'NONE', #55812, #4946, #26517 ) ;
#25440 = ORIENTED_EDGE ( 'NONE', *, *, #29727, .T. ) ;
#25441 =( BOUNDED_CURVE ( )  B_SPLINE_CURVE ( 3, ( #24814, #14163, #44410, #3580 ),
 .UNSPECIFIED., .F., .F. ) 
 B_SPLINE_CURVE_WITH_KNOTS ( ( 4, 4 ),
 ( 1.875920997006544022, 1.903716271183292008 ),
 .UNSPECIFIED. ) 
 CURVE ( )  GEOMETRIC_REPRESENTATION_ITEM ( )  RATIONAL_B_SPLINE_CURVE ( ( 1.000000000000000000, 0.9999356195973556627, 0.9999356195973556627, 1.000000000000000000 ) ) 
 REPRESENTATION_ITEM ( '' )  );
#25442 = AXIS2_PLACEMENT_3D ( 'NONE', #49371, #3817, #24070 ) ;
#25443 = VERTEX_POINT ( 'NONE', #57143 ) ;
#25444 = CARTESIAN_POINT ( 'NONE',  ( 37.00000000000000711, 4.705694406421931860E-17, -3.469127814946512892E-15 ) ) ;
#25445 = EDGE_CURVE ( 'NONE', #36611, #12850, #26533, .T. ) ;
#25446 = DIRECTION ( 'NONE',  ( 1.000000000000000000, 0.000000000000000000, 0.000000000000000000 ) ) ;
#25447 = DIRECTION ( 'NONE',  ( 0.000000000000000000, -0.3218879778916041157, 0.9467777615094549182 ) ) ;
#25448 = ADVANCED_FACE ( 'NONE', ( #11253 ), #6042, .F. ) ;
#25449 = CARTESIAN_POINT ( 'NONE',  ( 37.00000000000000711, 11.65150730582934635, 1.488153103997001514 ) ) ;
#25450 = FACE_OUTER_BOUND ( 'NONE', #39455, .T. ) ;
#25451 = AXIS2_PLACEMENT_3D ( 'NONE', #55980, #10415, #45026 ) ;
#25452 = DIRECTION ( 'NONE',  ( -1.000000000000000000, -0.000000000000000000, 0.000000000000000000 ) ) ;
#25453 = CARTESIAN_POINT ( 'NONE',  ( 1.010855698802849201, 0.1373453909157727193, -12.00331048781906595 ) ) ;
#25454 = CARTESIAN_POINT ( 'NONE',  ( -27.08423923533013777, -2.107995711831556651, -0.8983804370399715022 ) ) ;
#25455 = EDGE_LOOP ( 'NONE', ( #63439, #33608, #23247, #64218 ) ) ;
#25456 = CARTESIAN_POINT ( 'NONE',  ( 1.719304012340749033, -5.066286238787660601, -11.67935079956571087 ) ) ;
#25457 = CARTESIAN_POINT ( 'NONE',  ( 37.00000000000000711, 1.039216533672905785, -11.70009620280412221 ) ) ;
#25458 = DIRECTION ( 'NONE',  ( -1.000000000000000000, -1.836970198721029688E-16, -0.000000000000000000 ) ) ;
#25459 = AXIS2_PLACEMENT_3D ( 'NONE', #330, #16919, #61472 ) ;
#25460 = ADVANCED_FACE ( 'NONE', ( #5282 ), #21568, .T. ) ;
#25461 = ADVANCED_FACE ( 'NONE', ( #52153 ), #12800, .F. ) ;
#25462 = CARTESIAN_POINT ( 'NONE',  ( 0.2655924914740778742, -12.06787830249863980, -2.083162675473735792 ) ) ;
#25463 = DIRECTION ( 'NONE',  ( 0.000000000000000000, 0.01356324068818000848, -0.9999080150203990547 ) ) ;
#25464 = ORIENTED_EDGE ( 'NONE', *, *, #25296, .T. ) ;
#25465 = CARTESIAN_POINT ( 'NONE',  ( -17.16761170699768968, -6.928568383034877876, -11.59115056719998371 ) ) ;
#25466 = CARTESIAN_POINT ( 'NONE',  ( 3.152665057733995191, 6.622010822086684456, 4.377619405892240856 ) ) ;
#25467 = CARTESIAN_POINT ( 'NONE',  ( 12.80904563207495350, -29.07871018746070391, -3.648338481107154863 ) ) ;
#25468 = VERTEX_POINT ( 'NONE', #31209 ) ;
#25469 = CARTESIAN_POINT ( 'NONE',  ( 0.000000000000000000, 6.936109781200720192, -2.853135311044974198 ) ) ;
#25470 = DIRECTION ( 'NONE',  ( 0.000000000000000000, 0.000000000000000000, -1.000000000000000000 ) ) ;
#25471 = CARTESIAN_POINT ( 'NONE',  ( -22.27878402819508352, -0.9624056734348174214, -3.558531829368164257 ) ) ;
#25473 = EDGE_LOOP ( 'NONE', ( #57760, #949, #56702, #3932 ) ) ;
#25472 = CARTESIAN_POINT ( 'NONE',  ( 2.440552418640495880, 1.142369876085324476, 7.615619946579172961 ) ) ;
#25474 = DIRECTION ( 'NONE',  ( 0.000000000000000000, -0.9346839223284579834, 0.3554799084908868423 ) ) ;
#25475 = AXIS2_PLACEMENT_3D ( 'NONE', #9031, #35268, #49607 ) ;
#25476 = EDGE_CURVE ( 'NONE', #8907, #56961, #65341, .T. ) ;
#25477 = CARTESIAN_POINT ( 'NONE',  ( -27.04788180060269198, -3.218072544330550677, -0.2724356095623453045 ) ) ;
#25478 = EDGE_LOOP ( 'NONE', ( #42588, #45964, #34942, #59338 ) ) ;
#25479 = CARTESIAN_POINT ( 'NONE',  ( 0.3106921474978454056, 7.699584408545896430, 9.542334142800491747 ) ) ;
#25480 = CARTESIAN_POINT ( 'NONE',  ( 16.21117406328131949, -35.00000000000000000, 4.142385751841762165 ) ) ;
#25481 = CARTESIAN_POINT ( 'NONE',  ( -35.00000000000000000, -12.16632754454237464, 0.7008968033238341944 ) ) ;
#25482 = CARTESIAN_POINT ( 'NONE',  ( 1.287602823388152906, -1.639728374785596632, -12.47973441446222154 ) ) ;
#25483 = LINE ( 'NONE', #24501, #29060 ) ;
#25484 = FACE_OUTER_BOUND ( 'NONE', #49062, .T. ) ;
#25485 = CARTESIAN_POINT ( 'NONE',  ( 0.2767916011545413224, 11.44495079483529310, -4.367596755337330272 ) ) ;
#25486 = ORIENTED_EDGE ( 'NONE', *, *, #57420, .F. ) ;
#25487 = DIRECTION ( 'NONE',  ( -1.000000000000000000, 0.000000000000000000, 0.000000000000000000 ) ) ;
#25488 = EDGE_LOOP ( 'NONE', ( #51779, #33771, #29301, #62117 ) ) ;
#25489 = DIRECTION ( 'NONE',  ( -0.000000000000000000, -0.000000000000000000, -1.000000000000000000 ) ) ;
#25490 = VECTOR ( 'NONE', #38411, 1000.000000000000000 ) ;
#25491 = CARTESIAN_POINT ( 'NONE',  ( 3.092491956585884161, 1.813286239165800451, 7.707758057368689464 ) ) ;
#25492 = CARTESIAN_POINT ( 'NONE',  ( -18.25006854224444908, -9.443202773001939221, 9.647586298549914119 ) ) ;
#25494 = ORIENTED_EDGE ( 'NONE', *, *, #57021, .T. ) ;
#25493 = AXIS2_PLACEMENT_3D ( 'NONE', #16580, #10927, #31214 ) ;
#25495 = DIRECTION ( 'NONE',  ( -1.000000000000000000, 0.000000000000000000, 0.000000000000000000 ) ) ;
#25496 = ADVANCED_FACE ( 'NONE', ( #10575 ), #51515, .T. ) ;
#25497 = CARTESIAN_POINT ( 'NONE',  ( 12.57012137786681549, 11.47155630137818072, -3.539951925651088960 ) ) ;
#25498 = FACE_BOUND ( 'NONE', #42412, .T. ) ;
#25499 = ORIENTED_EDGE ( 'NONE', *, *, #16395, .F. ) ;
#25500 = ORIENTED_EDGE ( 'NONE', *, *, #55879, .T. ) ;
#25501 = CARTESIAN_POINT ( 'NONE',  ( 2.305787727787083519, -7.249469779319894336, -2.461236246751144829 ) ) ;
#25502 = VERTEX_POINT ( 'NONE', #25898 ) ;
#25503 = VECTOR ( 'NONE', #59780, 1000.000000000000000 ) ;
#25504 = CARTESIAN_POINT ( 'NONE',  ( 2.000000000000001776, 3.230174184210066191, 5.998318953995321223 ) ) ;
#25505 = DIRECTION ( 'NONE',  ( -1.000000000000000000, 0.000000000000000000, 0.000000000000000000 ) ) ;
#25506 = FACE_OUTER_BOUND ( 'NONE', #52743, .T. ) ;
#25507 = CARTESIAN_POINT ( 'NONE',  ( 2.260457164927187623, 7.131443009846837988, -2.742969430850449086 ) ) ;
#25509 = EDGE_CURVE ( 'NONE', #48505, #42153, #14562, .T. ) ;
#25508 = CARTESIAN_POINT ( 'NONE',  ( 0.000000000000000000, 0.000000000000000000, 0.000000000000000000 ) ) ;
#25510 = CARTESIAN_POINT ( 'NONE',  ( -36.00000000000000711, -10.23119532541078236, 7.608228585767692564 ) ) ;
#25511 = CARTESIAN_POINT ( 'NONE',  ( 37.00000000000000711, -8.029056188533749250, -8.573591947375291511 ) ) ;
#25512 = VECTOR ( 'NONE', #39966, 1000.000000000000000 ) ;
#25513 = VERTEX_POINT ( 'NONE', #42139 ) ;
#25514 = DIRECTION ( 'NONE',  ( 0.000000000000000000, -0.01356324068817998940, 0.9999080150203990547 ) ) ;
#25515 = CARTESIAN_POINT ( 'NONE',  ( 35.00000000000000000, -5.672855678558609505, 10.28547182238013669 ) ) ;
#25516 = ADVANCED_FACE ( 'NONE', ( #52797 ), #7228, .T. ) ;
#25517 = CARTESIAN_POINT ( 'NONE',  ( -35.00000000000000000, 0.000000000000000000, 0.000000000000000000 ) ) ;
#25518 = CARTESIAN_POINT ( 'NONE',  ( 11.92883720626436350, 13.27018586330439831, -2.496723423483149684 ) ) ;
#25519 = DIRECTION ( 'NONE',  ( -1.000000000000000000, -0.000000000000000000, 0.000000000000000000 ) ) ;
#25520 = CYLINDRICAL_SURFACE ( 'NONE', #64989, 6.936499999999988120 ) ;
#25521 = CARTESIAN_POINT ( 'NONE',  ( -36.00000000000000711, 9.076753354954126607, -8.954052073409506818 ) ) ;
#25522 = CARTESIAN_POINT ( 'NONE',  ( 37.00000000000000711, 11.54110654723649176, -2.185196060783925809 ) ) ;
#25523 = EDGE_CURVE ( 'NONE', #12164, #42779, #36010, .T. ) ;
#25524 = VECTOR ( 'NONE', #46177, 999.9999999999998863 ) ;
#25526 = ORIENTED_EDGE ( 'NONE', *, *, #39502, .F. ) ;
#25525 = AXIS2_PLACEMENT_3D ( 'NONE', #38270, #58594, #17011 ) ;
#25527 = AXIS2_PLACEMENT_3D ( 'NONE', #17965, #64796, #28269 ) ;
#25528 = LINE ( 'NONE', #51493, #30135 ) ;
#25529 = ORIENTED_EDGE ( 'NONE', *, *, #8175, .T. ) ;
#25530 = CARTESIAN_POINT ( 'NONE',  ( -35.00000000000000000, 0.000000000000000000, 0.000000000000000000 ) ) ;
#25531 = CYLINDRICAL_SURFACE ( 'NONE', #54267, 5.000000000000000888 ) ;
#25532 = CARTESIAN_POINT ( 'NONE',  ( 0.9232058338315058954, 1.793035206307509677, -12.34162163148531732 ) ) ;
#25533 = CARTESIAN_POINT ( 'NONE',  ( 2.368238019615157341, -7.589221137922671723, -1.155661230551862761 ) ) ;
#25534 = DIRECTION ( 'NONE',  ( -0.3865475372811021382, -0.8598319252293142867, 0.3335716741247162220 ) ) ;
#25535 = ORIENTED_EDGE ( 'NONE', *, *, #32996, .T. ) ;
#25536 = DIRECTION ( 'NONE',  ( -0.000000000000000000, -1.000000000000000000, -0.000000000000000000 ) ) ;
#25537 = DIRECTION ( 'NONE',  ( -1.000000000000000000, 0.000000000000000000, 0.000000000000000000 ) ) ;
#25538 = CARTESIAN_POINT ( 'NONE',  ( 1.547277799337861692, -1.534072017332991367, 12.58038279313703534 ) ) ;
#25539 = CARTESIAN_POINT ( 'NONE',  ( 24.82652845881425208, 25.00000000000000000, -8.578654028722157321 ) ) ;
#25540 = CIRCLE ( 'NONE', #47865, 7.499999999999988454 ) ;
#25541 = ADVANCED_FACE ( 'NONE', ( #12226 ), #8225, .T. ) ;
#25542 = AXIS2_PLACEMENT_3D ( 'NONE', #56962, #57281, #5437 ) ;
#25543 = CARTESIAN_POINT ( 'NONE',  ( 8.937200413559441614, 4.646453064669045396, -12.67647346021110266 ) ) ;
#25544 = VECTOR ( 'NONE', #67, 1000.000000000000000 ) ;
#25545 = FACE_OUTER_BOUND ( 'NONE', #34503, .T. ) ;
#25546 = VERTEX_POINT ( 'NONE', #47809 ) ;
#25547 = CIRCLE ( 'NONE', #10837, 2.899999999999994582 ) ;
#25548 = CARTESIAN_POINT ( 'NONE',  ( -27.09342121492660738, -0.5565043948835766141, 2.251107617623969936 ) ) ;
#25549 = VERTEX_POINT ( 'NONE', #12537 ) ;
#25550 = CARTESIAN_POINT ( 'NONE',  ( 0.2767916011545391575, -0.1897947303541993036, -12.24854187541374628 ) ) ;
#25551 = DIRECTION ( 'NONE',  ( -1.000000000000000000, 0.000000000000000000, 0.000000000000000000 ) ) ;
#25552 = B_SPLINE_CURVE_WITH_KNOTS ( 'NONE', 3,
 ( #5584, #56090, #50477, #14850, #25853, #19872, #258, #9541, #16194, #10529, #46144, #45145, #589, #20851, #35138, #61401, #45456, #65721, #20193 ),
 .UNSPECIFIED., .F., .F.,
 ( 4, 3, 3, 3, 3, 3, 4 ),
 ( 0.000000000000000000, 2.836829842860372840E-05, 4.224792512343171551E-05, 5.612066614707813677E-05, 6.998859278151645395E-05, 9.832141287888645782E-05, 0.0001178161482480164814 ),
 .UNSPECIFIED. ) ;
#25553 = CIRCLE ( 'NONE', #34042, 12.75000000000000178 ) ;
#25554 = CARTESIAN_POINT ( 'NONE',  ( -35.04709527796842394, -0.007095259204982495849, 0.01012471662512753889 ) ) ;
#25555 = CARTESIAN_POINT ( 'NONE',  ( 0.3002738374340850891, -11.59380198135585438, 3.979745968261164446 ) ) ;
#25556 = ADVANCED_FACE ( 'NONE', ( #43130 ), #17088, .F. ) ;
#25557 = ORIENTED_EDGE ( 'NONE', *, *, #24301, .T. ) ;
#25558 = ORIENTED_EDGE ( 'NONE', *, *, #31745, .T. ) ;
#25559 = ORIENTED_EDGE ( 'NONE', *, *, #18450, .F. ) ;
#25560 = AXIS2_PLACEMENT_3D ( 'NONE', #10203, #40805, #65710 ) ;
#25561 = DIRECTION ( 'NONE',  ( 1.000000000000000000, 0.000000000000000000, 0.000000000000000000 ) ) ;
#25562 = CARTESIAN_POINT ( 'NONE',  ( 0.2648978790185602672, -6.237101853238473659, -10.53870023327869987 ) ) ;
#25563 = FACE_OUTER_BOUND ( 'NONE', #49934, .T. ) ;
#25564 = CARTESIAN_POINT ( 'NONE',  ( 1.109979610368941882, 9.281420052101180929, 8.414317452281256493 ) ) ;
#25565 = CARTESIAN_POINT ( 'NONE',  ( 1.719304012341585253, 9.242227816401774376, -8.755325027795295867 ) ) ;
#25566 = CARTESIAN_POINT ( 'NONE',  ( 0.2638984909335716500, -7.718810690098997895, -9.508791614589274133 ) ) ;
#25567 = CARTESIAN_POINT ( 'NONE',  ( -7.382824176484668044, -1.433652869056799339, 11.91442981667273315 ) ) ;
#25568 = EDGE_LOOP ( 'NONE', ( #52422, #9738, #47384, #35748 ) ) ;
#25569 = VECTOR ( 'NONE', #56761, 1000.000000000000227 ) ;
#25570 = CARTESIAN_POINT ( 'NONE',  ( -8.580377709536596953, -8.097098178811418023, -8.863927581768100694 ) ) ;
#25571 = VERTEX_POINT ( 'NONE', #17560 ) ;
#25572 = CARTESIAN_POINT ( 'NONE',  ( -35.05012975565874456, -0.002073729464865227325, -0.01377677982612606281 ) ) ;
#25574 = CARTESIAN_POINT ( 'NONE',  ( -27.08456565417846207, 1.867985369021581299, -1.328664661356733445 ) ) ;
#25573 = CIRCLE ( 'NONE', #60610, 2.899999999999995026 ) ;
#25575 = VECTOR ( 'NONE', #27490, 1000.000000000000000 ) ;
#25576 = AXIS2_PLACEMENT_3D ( 'NONE', #65380, #65696, #40439 ) ;
#25577 = ORIENTED_EDGE ( 'NONE', *, *, #10709, .T. ) ;
#25578 = CARTESIAN_POINT ( 'NONE',  ( 2.034671305878982928, -6.953089744306905295, -9.380408876026439913 ) ) ;
#25579 = ORIENTED_EDGE ( 'NONE', *, *, #36913, .F. ) ;
#25580 = DIRECTION ( 'NONE',  ( 1.000000000000000000, -0.000000000000000000, 0.000000000000000000 ) ) ;
#25581 = EDGE_CURVE ( 'NONE', #47524, #51686, #13717, .T. ) ;
#25582 = DIRECTION ( 'NONE',  ( -1.000000000000000000, 0.000000000000000000, 0.000000000000000000 ) ) ;
#25583 = AXIS2_PLACEMENT_3D ( 'NONE', #6154, #826, #21440 ) ;
#25584 = LINE ( 'NONE', #40887, #57323 ) ;
#25585 = LINE ( 'NONE', #27455, #17581 ) ;
#25586 = ORIENTED_EDGE ( 'NONE', *, *, #28018, .F. ) ;
#25587 = ORIENTED_EDGE ( 'NONE', *, *, #21381, .F. ) ;
#25588 = DIRECTION ( 'NONE',  ( 0.000000000000000000, 0.01356324068817998940, -0.9999080150203990547 ) ) ;
#25589 = EDGE_CURVE ( 'NONE', #27033, #25959, #41334, .T. ) ;
#25590 = ORIENTED_EDGE ( 'NONE', *, *, #13165, .F. ) ;
#25591 = DIRECTION ( 'NONE',  ( 0.000000000000000000, 0.5767582926624970074, 0.8169148498130275327 ) ) ;
#25592 = ORIENTED_EDGE ( 'NONE', *, *, #65440, .F. ) ;
#25593 = ORIENTED_EDGE ( 'NONE', *, *, #62206, .T. ) ;
#25594 = ORIENTED_EDGE ( 'NONE', *, *, #42678, .F. ) ;
#25595 = AXIS2_PLACEMENT_3D ( 'NONE', #33186, #27880, #2641 ) ;
#25596 = CARTESIAN_POINT ( 'NONE',  ( -35.00000000000000000, 0.000000000000000000, 0.000000000000000000 ) ) ;
#25597 = CARTESIAN_POINT ( 'NONE',  ( 17.69916095700584435, -28.67478364583445938, 8.521665482016091531 ) ) ;
#25598 = AXIS2_PLACEMENT_3D ( 'NONE', #8682, #13652, #3730 ) ;
#25599 = CARTESIAN_POINT ( 'NONE',  ( 5.514970785353741078, 0.003805873180274313254, -0.002796696073589883310 ) ) ;
#25601 = EDGE_CURVE ( 'NONE', #58571, #7860, #7358, .T. ) ;
#25600 = DIRECTION ( 'NONE',  ( 0.000000000000000000, 0.7381862504171925465, -0.6745969609292691294 ) ) ;
#25602 = DIRECTION ( 'NONE',  ( 0.000000000000000000, 0.8369827122275362852, 0.5472293298355244140 ) ) ;
#25603 = ORIENTED_EDGE ( 'NONE', *, *, #2915, .T. ) ;
#25604 = CARTESIAN_POINT ( 'NONE',  ( 2.290907136832897706, -2.463690939638714106, -7.243397831411124699 ) ) ;
#25605 = ORIENTED_EDGE ( 'NONE', *, *, #5447, .F. ) ;
#25606 = CARTESIAN_POINT ( 'NONE',  ( 37.00000000000000711, -0.7536123767497623360, 11.72195762423410237 ) ) ;
#25607 = CARTESIAN_POINT ( 'NONE',  ( -27.09569413923794912, 0.6513788562879481159, 2.232620870184064188 ) ) ;
#25608 = VECTOR ( 'NONE', #52974, 1000.000000000000114 ) ;
#25609 = ADVANCED_FACE ( 'NONE', ( #27510 ), #7916, .T. ) ;
#25610 = ORIENTED_EDGE ( 'NONE', *, *, #51656, .T. ) ;
#25611 = FACE_OUTER_BOUND ( 'NONE', #37539, .T. ) ;
#25612 = DIRECTION ( 'NONE',  ( 1.000000000000000000, -0.000000000000000000, -0.000000000000000000 ) ) ;
#25613 = DIRECTION ( 'NONE',  ( -1.000000000000000000, 0.000000000000000000, 0.000000000000000000 ) ) ;
#25614 = ORIENTED_EDGE ( 'NONE', *, *, #65648, .F. ) ;
#25615 = LINE ( 'NONE', #36582, #65113 ) ;
#25616 = EDGE_CURVE ( 'NONE', #62364, #59342, #9432, .T. ) ;
#25617 = VECTOR ( 'NONE', #61177, 1000.000000000000000 ) ;
#25618 = ORIENTED_EDGE ( 'NONE', *, *, #27172, .T. ) ;
#25619 = CARTESIAN_POINT ( 'NONE',  ( -24.29873642282455393, -10.29150269569643150, 8.745998899381449476 ) ) ;
#25620 = CARTESIAN_POINT ( 'NONE',  ( 35.00000000000000000, -11.23004253107767880, -4.732539170486222524 ) ) ;
#25621 = CARTESIAN_POINT ( 'NONE',  ( -5.041025311761524463, -26.84022127302798921, 15.79220748139831265 ) ) ;
#25622 = CARTESIAN_POINT ( 'NONE',  ( 2.368238019615120926, 3.992969450835595069, 6.556525400300555084 ) ) ;
#25623 = DIRECTION ( 'NONE',  ( 0.000000000000000000, 0.01356324068817998940, -0.9999080150203990547 ) ) ;
#25624 = ORIENTED_EDGE ( 'NONE', *, *, #45293, .T. ) ;
#25625 = CARTESIAN_POINT ( 'NONE',  ( 3.152665057735807075, 3.546019893115007537, -7.102135024646828221 ) ) ;
#25626 = CARTESIAN_POINT ( 'NONE',  ( 35.00000000000000000, -9.908974237959688125, -6.307491713048997362 ) ) ;
#25627 = CARTESIAN_POINT ( 'NONE',  ( 0.000000000000000000, 244.9489742783177917, -23.99999999999999289 ) ) ;
#25628 = CARTESIAN_POINT ( 'NONE',  ( 3.047904605210341789, 3.577928268982092597, 7.047014837597028958 ) ) ;
#25629 = AXIS2_PLACEMENT_3D ( 'NONE', #32322, #31661, #7060 ) ;
#25630 = AXIS2_PLACEMENT_3D ( 'NONE', #30128, #50430, #45410 ) ;
#25631 = CARTESIAN_POINT ( 'NONE',  ( 0.2915757698887279092, 12.25305747416128455, -0.2147157799035241121 ) ) ;
#25632 =( BOUNDED_CURVE ( )  B_SPLINE_CURVE ( 3, ( #190, #19151, #35419, #49744 ),
 .UNSPECIFIED., .F., .F. ) 
 B_SPLINE_CURVE_WITH_KNOTS ( ( 4, 4 ),
 ( 1.242321100838241765, 1.259206054522467477 ),
 .UNSPECIFIED. ) 
 CURVE ( )  GEOMETRIC_REPRESENTATION_ITEM ( )  RATIONAL_B_SPLINE_CURVE ( ( 1.000000000000000000, 0.9999762416693727118, 0.9999762416693727118, 1.000000000000000000 ) ) 
 REPRESENTATION_ITEM ( '' )  );
#25633 = CYLINDRICAL_SURFACE ( 'NONE', #10487, 12.74999999999999822 ) ;
#25634 = CARTESIAN_POINT ( 'NONE',  ( 2.269879328256728446, -5.949827370243832014, -4.798845682294102133 ) ) ;
#25635 = DIRECTION ( 'NONE',  ( -1.000000000000000000, 0.000000000000000000, -0.000000000000000000 ) ) ;
#25636 = DIRECTION ( 'NONE',  ( 0.000000000000000000, 0.01356324068817998940, -0.9999080150203989437 ) ) ;
#25637 = VECTOR ( 'NONE', #48016, 1000.000000000000000 ) ;
#25638 = ADVANCED_FACE ( 'NONE', ( #63732 ), #18213, .T. ) ;
#25639 = AXIS2_PLACEMENT_3D ( 'NONE', #52314, #6753, #27660 ) ;
#25640 = ORIENTED_EDGE ( 'NONE', *, *, #63652, .F. ) ;
#25641 = CIRCLE ( 'NONE', #59645, 2.899999999999996358 ) ;
#25642 = EDGE_LOOP ( 'NONE', ( #29364, #47467, #13617, #2020 ) ) ;
#25643 = DIRECTION ( 'NONE',  ( -1.000000000000000000, -0.000000000000000000, 0.000000000000000000 ) ) ;
#25644 = DIRECTION ( 'NONE',  ( 1.000000000000000000, -0.000000000000000000, -0.000000000000000000 ) ) ;
#25645 = CARTESIAN_POINT ( 'NONE',  ( 2.000000000000001776, -6.470132594555817462, 2.133363481234057168 ) ) ;
#25646 = VECTOR ( 'NONE', #10050, 1000.000000000000000 ) ;
#25647 = CARTESIAN_POINT ( 'NONE',  ( -10.90165637462999726, -7.508992741355383416, 25.00000000000000000 ) ) ;
#25648 = ORIENTED_EDGE ( 'NONE', *, *, #49925, .T. ) ;
#25649 = AXIS2_PLACEMENT_3D ( 'NONE', #61025, #6479, #36405 ) ;
#25650 = ORIENTED_EDGE ( 'NONE', *, *, #41966, .F. ) ;
#25651 = ORIENTED_EDGE ( 'NONE', *, *, #8928, .T. ) ;
#25652 = CARTESIAN_POINT ( 'NONE',  ( -37.00000000000000711, 0.000000000000000000, 0.000000000000000000 ) ) ;
#25653 = CARTESIAN_POINT ( 'NONE',  ( 37.00000000000000711, 1.591260454995240714, -12.08216339958901564 ) ) ;
#25654 = EDGE_CURVE ( 'NONE', #10868, #7257, #56207, .T. ) ;
#25655 = ORIENTED_EDGE ( 'NONE', *, *, #20580, .F. ) ;
#25656 = CARTESIAN_POINT ( 'NONE',  ( 37.00000000000000711, -8.258652103341374229, 8.352657516904754331 ) ) ;
#25657 = DIRECTION ( 'NONE',  ( 0.000000000000000000, -0.4935949184179135862, 0.8696919319575254770 ) ) ;
#25658 = AXIS2_PLACEMENT_3D ( 'NONE', #25596, #51861, #41202 ) ;
#25659 = CARTESIAN_POINT ( 'NONE',  ( 2.430348790457294683, -2.448665558939157272, 7.297553103283471287 ) ) ;
#25660 = ORIENTED_EDGE ( 'NONE', *, *, #2192, .F. ) ;
#25661 = DIRECTION ( 'NONE',  ( 0.000000000000000000, 0.000000000000000000, 1.000000000000000000 ) ) ;
#25662 = EDGE_CURVE ( 'NONE', #51152, #47570, #56650, .T. ) ;
#25663 = CARTESIAN_POINT ( 'NONE',  ( -10.70822065730027184, -29.54386645810234313, -10.21044671110655777 ) ) ;
#25664 = ORIENTED_EDGE ( 'NONE', *, *, #24245, .T. ) ;
#25665 = AXIS2_PLACEMENT_3D ( 'NONE', #34327, #3451, #43986 ) ;
#25666 = CYLINDRICAL_SURFACE ( 'NONE', #4454, 13.50000000000000178 ) ;
#25667 = EDGE_CURVE ( 'NONE', #28861, #48679, #18563, .T. ) ;
#25668 = ORIENTED_EDGE ( 'NONE', *, *, #921, .F. ) ;
#25669 = LINE ( 'NONE', #65251, #28397 ) ;
#25670 = EDGE_LOOP ( 'NONE', ( #22450, #9281, #53950, #13285 ) ) ;
#25671 = CARTESIAN_POINT ( 'NONE',  ( -35.00000000000000000, -7.882940143791844712, 10.02106554660705839 ) ) ;
#25672 = CARTESIAN_POINT ( 'NONE',  ( -37.00000000000000711, 0.000000000000000000, 0.000000000000000000 ) ) ;
#25673 = DIRECTION ( 'NONE',  ( 0.000000000000000000, 8.881784197001252323E-16, 1.000000000000000000 ) ) ;
#25674 = DIRECTION ( 'NONE',  ( 0.000000000000000000, 0.01356324068817992175, -0.9999080150203990547 ) ) ;
#25675 = CIRCLE ( 'NONE', #24635, 6.936499999999989008 ) ;
#25677 = CIRCLE ( 'NONE', #4472, 5.000000000000000888 ) ;
#25676 = CARTESIAN_POINT ( 'NONE',  ( 35.00000000000000000, -9.557269938331497627, 7.561043153948066475 ) ) ;
#25679 = EDGE_CURVE ( 'NONE', #50432, #53297, #49140, .T. ) ;
#25678 = DIRECTION ( 'NONE',  ( 1.000000000000000000, 0.000000000000000000, 0.000000000000000000 ) ) ;
#25680 = LINE ( 'NONE', #426, #2786 ) ;
#25681 = DIRECTION ( 'NONE',  ( 1.000000000000000000, 0.000000000000000000, 0.000000000000000000 ) ) ;
#25683 = ORIENTED_EDGE ( 'NONE', *, *, #54655, .T. ) ;
#25682 = DIRECTION ( 'NONE',  ( 1.000000000000000000, 0.000000000000000000, -0.000000000000000000 ) ) ;
#25684 = DIRECTION ( 'NONE',  ( -1.000000000000000000, 0.000000000000000000, 0.000000000000000000 ) ) ;
#25685 = ORIENTED_EDGE ( 'NONE', *, *, #1755, .F. ) ;
#25686 = CARTESIAN_POINT ( 'NONE',  ( 10.12522915465333462, -13.48295319373161760, -0.6855729276752927648 ) ) ;
#25687 = ORIENTED_EDGE ( 'NONE', *, *, #61486, .T. ) ;
#25688 = ADVANCED_FACE ( 'NONE', ( #28833 ), #14182, .T. ) ;
#25689 = DIRECTION ( 'NONE',  ( 1.000000000000000000, 0.000000000000000000, 0.000000000000000000 ) ) ;
#25690 = EDGE_LOOP ( 'NONE', ( #44245, #36099, #6436, #12096 ) ) ;
#25691 = DIRECTION ( 'NONE',  ( -1.000000000000000000, 0.000000000000000000, 0.000000000000000000 ) ) ;
#25692 = DIRECTION ( 'NONE',  ( -1.000000000000000000, 0.000000000000000000, 0.000000000000000000 ) ) ;
#25693 = DIRECTION ( 'NONE',  ( -1.000000000000000000, 0.000000000000000000, -0.000000000000000000 ) ) ;
#25695 = CIRCLE ( 'NONE', #14004, 7.499999999999988454 ) ;
#25694 = CARTESIAN_POINT ( 'NONE',  ( -22.31328051695926007, 1.671726071983979711, -3.401210163132561082 ) ) ;
#25696 = CIRCLE ( 'NONE', #35211, 5.000000000000000888 ) ;
#25697 = CARTESIAN_POINT ( 'NONE',  ( 5.514624014163232779, -0.003946330869975010931, 0.001255375129358063304 ) ) ;
#25698 = EDGE_LOOP ( 'NONE', ( #22650, #14933, #40263, #12062 ) ) ;
#25699 = FACE_OUTER_BOUND ( 'NONE', #45103, .T. ) ;
#25701 = EDGE_CURVE ( 'NONE', #8767, #4893, #14744, .T. ) ;
#25700 = AXIS2_PLACEMENT_3D ( 'NONE', #16477, #31737, #36745 ) ;
#25702 = ORIENTED_EDGE ( 'NONE', *, *, #39710, .T. ) ;
#25703 = CARTESIAN_POINT ( 'NONE',  ( 0.000000000000000000, 5.097042323172538580, -5.501832381651401427 ) ) ;
#25704 = AXIS2_PLACEMENT_3D ( 'NONE', #2725, #8027, #58911 ) ;
#25705 = ADVANCED_FACE ( 'NONE', ( #35100 ), #29792, .F. ) ;
#25706 = PLANE ( 'NONE',  #10087 ) ;
#25707 = CARTESIAN_POINT ( 'NONE',  ( 0.000000000000000000, -6.906413915731192787, 0.6453518998147164121 ) ) ;
#25708 = ORIENTED_EDGE ( 'NONE', *, *, #33239, .F. ) ;
#25709 = AXIS2_PLACEMENT_3D ( 'NONE', #33553, #53843, #23583 ) ;
#25710 = CARTESIAN_POINT ( 'NONE',  ( -27.09048036756547972, -0.9969423855787317157, 2.083857239072904211 ) ) ;
#25711 = CIRCLE ( 'NONE', #9748, 7.499999999999988454 ) ;
#25712 = CARTESIAN_POINT ( 'NONE',  ( 48.39008813825011401, -0.3233266992476154233, -8.863930066451532142 ) ) ;
#25713 = DIRECTION ( 'NONE',  ( 0.000000000000000000, 0.01356324068817998940, -0.9999080150203990547 ) ) ;
#25714 = DIRECTION ( 'NONE',  ( 0.000000000000000000, -0.01356324068818000328, 0.9999080150203990547 ) ) ;
#25715 = VERTEX_POINT ( 'NONE', #30142 ) ;
#25716 = CARTESIAN_POINT ( 'NONE',  ( 35.00000000000000000, 5.428340790341703581, -10.91072401419412685 ) ) ;
#25717 = CARTESIAN_POINT ( 'NONE',  ( 7.188828048480045751, -31.44854185097605637, 14.13838964164171585 ) ) ;
#25718 = CARTESIAN_POINT ( 'NONE',  ( 1.109979610371585101, -3.830786822172526307, -11.92772269523408468 ) ) ;
#25719 = AXIS2_PLACEMENT_3D ( 'NONE', #1754, #54516, #28567 ) ;
#25720 = EDGE_CURVE ( 'NONE', #45412, #51182, #40098, .T. ) ;
#25721 = EDGE_CURVE ( 'NONE', #14018, #56624, #21795, .T. ) ;
#25722 = AXIS2_PLACEMENT_3D ( 'NONE', #60443, #4935, #35154 ) ;
#25723 = B_SPLINE_CURVE_WITH_KNOTS ( 'NONE', 3,
 ( #37579, #11965, #17298, #17633, #31908, #57876, #2342, #52868, #37896, #32246, #7298, #43202, #42206, #62495, #63478, #27583 ),
 .UNSPECIFIED., .F., .F.,
 ( 4, 2, 2, 2, 2, 2, 2, 4 ),
 ( 2.485638410533990448E-17, 0.002410354704749657039, 0.003615532057124472981, 0.004820709409499289791, 0.006025886761874103999, 0.007231064114248917339, 0.008436241466623731547, 0.009641418818998544887 ),
 .UNSPECIFIED. ) ;
#25724 = DIRECTION ( 'NONE',  ( 0.000000000000000000, -0.9635499925192253512, 0.2675283385292120397 ) ) ;
#25725 = CARTESIAN_POINT ( 'NONE',  ( -37.00000000000000711, 0.000000000000000000, 0.000000000000000000 ) ) ;
#25726 = ORIENTED_EDGE ( 'NONE', *, *, #46394, .F. ) ;
#25727 = CARTESIAN_POINT ( 'NONE',  ( 1.937114397841935398, 3.111612666690077855, 12.45230409340482503 ) ) ;
#25728 = DIRECTION ( 'NONE',  ( -1.000000000000000000, 0.000000000000000000, 0.000000000000000000 ) ) ;
#25729 = CARTESIAN_POINT ( 'NONE',  ( 34.38695973621796043, 25.00000000000000000, 3.530690241644829364 ) ) ;
#25730 = ORIENTED_EDGE ( 'NONE', *, *, #59024, .T. ) ;
#25731 = CARTESIAN_POINT ( 'NONE',  ( -18.58686583997225839, 5.151216734910813777, 10.83812558286603789 ) ) ;
#25732 = CARTESIAN_POINT ( 'NONE',  ( 35.00000000000000000, -11.65150730582935523, -1.488153103996925797 ) ) ;
#25733 = EDGE_LOOP ( 'NONE', ( #50760, #24523, #17841, #48545 ) ) ;
#25734 = EDGE_CURVE ( 'NONE', #23284, #59054, #30701, .T. ) ;
#25735 = ORIENTED_EDGE ( 'NONE', *, *, #36346, .T. ) ;
#25736 = VERTEX_POINT ( 'NONE', #9191 ) ;
#25737 = CIRCLE ( 'NONE', #62893, 5.000000000000000000 ) ;
#25738 = VECTOR ( 'NONE', #9503, 1000.000000000000000 ) ;
#25739 = ADVANCED_FACE ( 'NONE', ( #9851 ), #29470, .T. ) ;
#25740 = ORIENTED_EDGE ( 'NONE', *, *, #18582, .F. ) ;
#25741 = CARTESIAN_POINT ( 'NONE',  ( 2.177405672432406902, 10.01846874164783152, 5.005033771130518616 ) ) ;
#25742 = CARTESIAN_POINT ( 'NONE',  ( 2.305787727787083519, -5.756228004061423320, -5.047606869483115766 ) ) ;
#25743 = DIRECTION ( 'NONE',  ( 0.000000000000000000, -0.01356324068817998940, 0.9999080150203990547 ) ) ;
#25744 = CARTESIAN_POINT ( 'NONE',  ( 9.150528470156286787, 5.807572156255496054, 10.50730673458101450 ) ) ;
#25745 = CIRCLE ( 'NONE', #38505, 7.499999999999988454 ) ;
#25746 = CARTESIAN_POINT ( 'NONE',  ( 3.152665057735501097, 6.622010822086128456, -4.377619405893580229 ) ) ;
#25747 = AXIS2_PLACEMENT_3D ( 'NONE', #24865, #24520, #9536 ) ;
#25748 = CARTESIAN_POINT ( 'NONE',  ( -8.269707202464745777, -26.46746146559253532, 14.47885724100708416 ) ) ;
#25749 = CARTESIAN_POINT ( 'NONE',  ( 24.90067624556555259, -0.3238485137761343835, -13.50202336863869235 ) ) ;
#25751 = ORIENTED_EDGE ( 'NONE', *, *, #20855, .F. ) ;
#25750 = DIRECTION ( 'NONE',  ( -0.000000000000000000, -1.000000000000000000, -0.000000000000000000 ) ) ;
#25752 = CARTESIAN_POINT ( 'NONE',  ( 47.00000000000000711, 4.705694406421931860E-17, -3.469127814946512892E-15 ) ) ;
#25753 = EDGE_CURVE ( 'NONE', #19363, #26831, #65047, .T. ) ;
#25754 = EDGE_LOOP ( 'NONE', ( #22005, #52187, #19548, #6609, #17194, #6904 ) ) ;
#25755 = DIRECTION ( 'NONE',  ( -1.000000000000000000, 0.000000000000000000, 0.000000000000000000 ) ) ;
#25756 = ORIENTED_EDGE ( 'NONE', *, *, #57044, .F. ) ;
#25757 = ORIENTED_EDGE ( 'NONE', *, *, #50128, .F. ) ;
#25758 = CARTESIAN_POINT ( 'NONE',  ( -22.27710395300133328, -0.9764373854729024860, 3.549456197028676208 ) ) ;
#25759 = CARTESIAN_POINT ( 'NONE',  ( 17.02556425888772296, -29.48112685930881227, 9.540979227922154138 ) ) ;
#25760 = CARTESIAN_POINT ( 'NONE',  ( -27.45775109278351067, 10.51123867646838583, -8.471355351200609007 ) ) ;
#25761 = CARTESIAN_POINT ( 'NONE',  ( 37.00000000000000711, 9.621072037176993774, -8.366449238204399563 ) ) ;
#25762 = FACE_OUTER_BOUND ( 'NONE', #40715, .T. ) ;
#25763 = DIRECTION ( 'NONE',  ( 1.000000000000000000, 0.000000000000000000, 0.000000000000000000 ) ) ;
#25764 = ORIENTED_EDGE ( 'NONE', *, *, #33828, .T. ) ;
#25765 = AXIS2_PLACEMENT_3D ( 'NONE', #40140, #45465, #30500 ) ;
#25766 = ORIENTED_EDGE ( 'NONE', *, *, #24021, .F. ) ;
#25767 = CARTESIAN_POINT ( 'NONE',  ( 0.3218525148189825269, 12.03385614540604109, 2.370084734146256977 ) ) ;
#25768 = ORIENTED_EDGE ( 'NONE', *, *, #50269, .T. ) ;
#25769 = EDGE_CURVE ( 'NONE', #7682, #37677, #60431, .T. ) ;
#25770 = EDGE_CURVE ( 'NONE', #51848, #59884, #6715, .T. ) ;
#25771 = CIRCLE ( 'NONE', #4561, 5.000000000000000888 ) ;
#25772 = ORIENTED_EDGE ( 'NONE', *, *, #61991, .F. ) ;
#25773 = CARTESIAN_POINT ( 'NONE',  ( -37.00000000000000711, 3.340853584269533716, 11.26103545359857350 ) ) ;
#25774 = CARTESIAN_POINT ( 'NONE',  ( 35.00000000000000000, -11.17622378668003691, 3.614449339633606595 ) ) ;
#25775 = CARTESIAN_POINT ( 'NONE',  ( -22.28694879868232803, 0.9088670759108249397, -3.597828382597549446 ) ) ;
#25776 = CARTESIAN_POINT ( 'NONE',  ( 1.459561108993354006, -12.32692860927468459, 2.815016945600703036 ) ) ;
#25777 = EDGE_CURVE ( 'NONE', #35536, #39745, #554, .T. ) ;
#25778 = CARTESIAN_POINT ( 'NONE',  ( 2.268878695253354394, 7.642144312464374423, 0.1481365927653814363 ) ) ;
#25779 = VECTOR ( 'NONE', #23851, 1000.000000000000000 ) ;
#25780 = DIRECTION ( 'NONE',  ( 0.000000000000000000, 0.4134677391718449835, 0.9105187689795983808 ) ) ;
#25781 = AXIS2_PLACEMENT_3D ( 'NONE', #9115, #30049, #29394 ) ;
#25782 = ADVANCED_FACE ( 'NONE', ( #56054 ), #6193, .T. ) ;
#25783 = ORIENTED_EDGE ( 'NONE', *, *, #61056, .F. ) ;
#25784 = ADVANCED_FACE ( 'NONE', ( #15808 ), #60731, .T. ) ;
#25785 = DIRECTION ( 'NONE',  ( -1.000000000000000000, 0.000000000000000000, 0.000000000000000000 ) ) ;
#25786 = CARTESIAN_POINT ( 'NONE',  ( 2.256373768223411957, 7.499124080223153577, -1.457292142211135122 ) ) ;
#25787 = VECTOR ( 'NONE', #48043, 1000.000000000000000 ) ;
#25788 = CARTESIAN_POINT ( 'NONE',  ( -35.00000000000000000, -9.321877890560388735, -7.146664589318012517 ) ) ;
#25789 = CIRCLE ( 'NONE', #31097, 5.000000000000001776 ) ;
#25790 = DIRECTION ( 'NONE',  ( 1.000000000000000000, 0.000000000000000000, 0.000000000000000000 ) ) ;
#25791 = PLANE ( 'NONE',  #57644 ) ;
#25792 = CARTESIAN_POINT ( 'NONE',  ( -36.00000000000000711, 6.564808257521927537, -10.93004082984011482 ) ) ;
#25793 = CARTESIAN_POINT ( 'NONE',  ( 0.6605806670570022465, -0.1501238075117865833, -12.00189431062279688 ) ) ;
#25794 = CIRCLE ( 'NONE', #36418, 5.000000000000000000 ) ;
#25795 = CARTESIAN_POINT ( 'NONE',  ( -35.04643116707788408, -0.002453861112623398344, -0.01193867652721398998 ) ) ;
#25796 = VERTEX_POINT ( 'NONE', #20818 ) ;
#25797 = CARTESIAN_POINT ( 'NONE',  ( 0.2650492594609224484, 10.54996119777445429, 6.218173512054799623 ) ) ;
#25798 = CARTESIAN_POINT ( 'NONE',  ( -37.00000000000000711, 0.000000000000000000, 0.000000000000000000 ) ) ;
#25799 = CARTESIAN_POINT ( 'NONE',  ( 15.04427341497070714, -34.74416750921062658, 6.992747701482930012 ) ) ;
#25800 = EDGE_CURVE ( 'NONE', #30228, #5306, #45756, .T. ) ;
#25801 = B_SPLINE_CURVE_WITH_KNOTS ( 'NONE', 3,
 ( #4529, #49739, #35064, #44727, #50068, #14143, #10150 ),
 .UNSPECIFIED., .F., .F.,
 ( 4, 3, 4 ),
 ( 7.221291777193456067E-15, 0.002398160485434789463, 0.005002426799383989479 ),
 .UNSPECIFIED. ) ;
#25802 = CARTESIAN_POINT ( 'NONE',  ( -13.24204686117535879, -34.10419274375227872, -9.367294588217838225 ) ) ;
#25803 = DIRECTION ( 'NONE',  ( 1.000000000000000000, 0.000000000000000000, 0.000000000000000000 ) ) ;
#25804 = VERTEX_POINT ( 'NONE', #50755 ) ;
#25805 = DIRECTION ( 'NONE',  ( -1.000000000000000000, -0.000000000000000000, 0.000000000000000000 ) ) ;
#25806 = CARTESIAN_POINT ( 'NONE',  ( 0.9232058338315048962, -12.46548196349785798, -0.3773051331669288744 ) ) ;
#25807 = CARTESIAN_POINT ( 'NONE',  ( 15.04222346523121168, -34.74354600359600909, -6.996510958921167145 ) ) ;
#25808 = ORIENTED_EDGE ( 'NONE', *, *, #51482, .T. ) ;
#25809 = CARTESIAN_POINT ( 'NONE',  ( 2.655192694323460945, -6.969384012965772257, 6.604353705985055001 ) ) ;
#25810 = CARTESIAN_POINT ( 'NONE',  ( 0.3665391374699464300, -12.27992639892678106, -0.2638605131388451763 ) ) ;
#25811 = CARTESIAN_POINT ( 'NONE',  ( 35.00000000000000000, 0.1414404973753909389, 12.74921544981110344 ) ) ;
#25812 = AXIS2_PLACEMENT_3D ( 'NONE', #7579, #32501, #1630 ) ;
#25813 = ADVANCED_FACE ( 'NONE', ( #46418 ), #36764, .T. ) ;
#25814 = VECTOR ( 'NONE', #37101, 1000.000000000000114 ) ;
#25816 = ORIENTED_EDGE ( 'NONE', *, *, #59977, .F. ) ;
#25815 = DIRECTION ( 'NONE',  ( -1.000000000000000000, 0.000000000000000000, 0.000000000000000000 ) ) ;
#25817 = DIRECTION ( 'NONE',  ( 1.000000000000000000, -0.000000000000000000, -0.000000000000000000 ) ) ;
#25818 = CIRCLE ( 'NONE', #26914, 6.936499999999990784 ) ;
#25819 = AXIS2_PLACEMENT_3D ( 'NONE', #5974, #46198, #19616 ) ;
#25820 = LINE ( 'NONE', #16160, #29756 ) ;
#25821 = EDGE_LOOP ( 'NONE', ( #11651, #44880, #33232, #39771 ) ) ;
#25822 = CARTESIAN_POINT ( 'NONE',  ( 0.2676618633000453773, 7.748413788583214945, 9.484212776852357862 ) ) ;
#25824 = CARTESIAN_POINT ( 'NONE',  ( -27.28573687977896611, -2.862048090118451071, -0.4470060700698573197 ) ) ;
#25823 =( BOUNDED_CURVE ( )  B_SPLINE_CURVE ( 3, ( #43791, #54095, #60068, #14487 ),
 .UNSPECIFIED., .F., .F. ) 
 B_SPLINE_CURVE_WITH_KNOTS ( ( 4, 4 ),
 ( 5.002748361502479924, 5.006749598811624402 ),
 .UNSPECIFIED. ) 
 CURVE ( )  GEOMETRIC_REPRESENTATION_ITEM ( )  RATIONAL_B_SPLINE_CURVE ( ( 1.000000000000000000, 0.9999986658421111674, 0.9999986658421111674, 1.000000000000000000 ) ) 
 REPRESENTATION_ITEM ( '' )  );
#25825 = CARTESIAN_POINT ( 'NONE',  ( 1.549075743846619613, -1.533250336941883063, -12.58108552526800850 ) ) ;
#25826 = DIRECTION ( 'NONE',  ( 0.000000000000000000, 0.1081190184239417817, -0.9941379571543595972 ) ) ;
#25827 = VECTOR ( 'NONE', #35974, 1000.000000000000000 ) ;
#25828 = CARTESIAN_POINT ( 'NONE',  ( 37.00000000000000711, -5.814360711498364864, -10.70999494708490829 ) ) ;
#25829 = CARTESIAN_POINT ( 'NONE',  ( 0.2958664285830449603, 11.43993536884562623, -4.398464391600207080 ) ) ;
#25830 = EDGE_CURVE ( 'NONE', #31862, #38335, #37064, .T. ) ;
#25831 = ORIENTED_EDGE ( 'NONE', *, *, #47305, .F. ) ;
#25832 = CARTESIAN_POINT ( 'NONE',  ( -35.00000000000000000, -8.839356091079983102, -8.389074212634382022 ) ) ;
#25833 = VECTOR ( 'NONE', #40847, 1000.000000000000000 ) ;
#25834 = ORIENTED_EDGE ( 'NONE', *, *, #7077, .T. ) ;
#25835 = CARTESIAN_POINT ( 'NONE',  ( 35.04999999999999716, -19.99999999999999289, 4.363913744254155347E-15 ) ) ;
#25836 = EDGE_CURVE ( 'NONE', #34412, #30073, #33893, .T. ) ;
#25837 = FACE_OUTER_BOUND ( 'NONE', #39062, .T. ) ;
#25838 = AXIS2_PLACEMENT_3D ( 'NONE', #3521, #62680, #42724 ) ;
#25839 = CARTESIAN_POINT ( 'NONE',  ( 0.2676618633000434344, 11.45242956837287629, 4.339362305359467875 ) ) ;
#25840 = DIRECTION ( 'NONE',  ( -1.000000000000000000, 0.000000000000000000, -0.000000000000000000 ) ) ;
#25841 = VERTEX_POINT ( 'NONE', #15165 ) ;
#25842 = CARTESIAN_POINT ( 'NONE',  ( 0.000000000000000000, 0.000000000000000000, 0.000000000000000000 ) ) ;
#25843 = AXIS2_PLACEMENT_3D ( 'NONE', #43311, #54302, #58645 ) ;
#25844 = DIRECTION ( 'NONE',  ( 1.000000000000000000, 0.000000000000000000, 0.000000000000000000 ) ) ;
#25845 = CARTESIAN_POINT ( 'NONE',  ( -22.27709082389155171, -1.005749854561698298, 3.541295940224338246 ) ) ;
#25846 = ORIENTED_EDGE ( 'NONE', *, *, #51205, .F. ) ;
#25847 = AXIS2_PLACEMENT_3D ( 'NONE', #28304, #28962, #23984 ) ;
#25848 = VERTEX_POINT ( 'NONE', #61061 ) ;
#25849 = CARTESIAN_POINT ( 'NONE',  ( 29.10683426066285051, -10.83754748704998505, 8.060616254555327487 ) ) ;
#25850 = VERTEX_POINT ( 'NONE', #10497 ) ;
#25851 = CARTESIAN_POINT ( 'NONE',  ( 21.97522221603474080, -11.76847154110449623, -2.374955909613984506 ) ) ;
#25852 = DIRECTION ( 'NONE',  ( 0.000000000000000000, -0.01356324068817998940, 0.9999080150203990547 ) ) ;
#25853 = CARTESIAN_POINT ( 'NONE',  ( -27.09729107899853062, 2.324833743198347236, -0.1622107421537140326 ) ) ;
#25854 = ADVANCED_FACE ( 'NONE', ( #55748 ), #5206, .T. ) ;
#25855 = CARTESIAN_POINT ( 'NONE',  ( -28.80182618048087662, 2.759540267861917862, 11.68534817325614661 ) ) ;
#25856 = DIRECTION ( 'NONE',  ( -1.000000000000000000, 0.000000000000000000, 0.000000000000000000 ) ) ;
#25857 = CARTESIAN_POINT ( 'NONE',  ( 2.000000000000001776, -0.4804830611969332366, -6.919838746524582085 ) ) ;
#25858 = AXIS2_PLACEMENT_3D ( 'NONE', #5185, #61674, #30752 ) ;
#25859 = ADVANCED_FACE ( 'NONE', ( #61363 ), #30459, .T. ) ;
#25860 = DIRECTION ( 'NONE',  ( -1.000000000000000000, -0.000000000000000000, -0.000000000000000000 ) ) ;
#25861 = ORIENTED_EDGE ( 'NONE', *, *, #57818, .F. ) ;
#25862 = CARTESIAN_POINT ( 'NONE',  ( -37.00000000000000711, -7.379373053628941470, 10.39746860227888270 ) ) ;
#25863 = ADVANCED_FACE ( 'NONE', ( #61696 ), #16156, .T. ) ;
#25864 = DIRECTION ( 'NONE',  ( 0.000000000000000000, 0.01356324068817991828, -0.9999080150203990547 ) ) ;
#25865 = CARTESIAN_POINT ( 'NONE',  ( 36.00000000000000711, 3.640372113593552061, -12.21925492305363647 ) ) ;
#25867 = CARTESIAN_POINT ( 'NONE',  ( -9.142358947343478093, 11.11112337110911774, -4.548091552537131932 ) ) ;
#25866 = AXIS2_PLACEMENT_3D ( 'NONE', #45257, #60881, #19981 ) ;
#25868 = DIRECTION ( 'NONE',  ( -1.000000000000000000, 0.000000000000000000, 0.000000000000000000 ) ) ;
#25869 = CARTESIAN_POINT ( 'NONE',  ( 0.3006302518452070860, -10.72687985734938465, -5.932248915294272784 ) ) ;
#25870 = DIRECTION ( 'NONE',  ( -1.000000000000000000, 0.000000000000000000, 0.000000000000000000 ) ) ;
#25871 = FACE_OUTER_BOUND ( 'NONE', #63952, .T. ) ;
#25872 = CIRCLE ( 'NONE', #63016, 12.18650000000000055 ) ;
#25873 = ORIENTED_EDGE ( 'NONE', *, *, #4380, .T. ) ;
#25874 = DIRECTION ( 'NONE',  ( -1.000000000000000000, -0.000000000000000000, -0.000000000000000000 ) ) ;
#25875 = EDGE_CURVE ( 'NONE', #21538, #54100, #37080, .T. ) ;
#25876 = ORIENTED_EDGE ( 'NONE', *, *, #1884, .T. ) ;
#25877 = CARTESIAN_POINT ( 'NONE',  ( -22.28629837673887693, -3.697248502489102417, 0.2936941584814368733 ) ) ;
#25878 = DIRECTION ( 'NONE',  ( 1.000000000000000000, 0.000000000000000000, 0.000000000000000000 ) ) ;
#25879 = AXIS2_PLACEMENT_3D ( 'NONE', #26510, #61420, #920 ) ;
#25880 = FACE_OUTER_BOUND ( 'NONE', #45381, .T. ) ;
#25881 = CARTESIAN_POINT ( 'NONE',  ( 1.452237505248552996, -5.807998527925814614, -11.24427360515648289 ) ) ;
#25882 = VERTEX_POINT ( 'NONE', #22120 ) ;
#25883 = AXIS2_PLACEMENT_3D ( 'NONE', #8865, #64063, #3583 ) ;
#25884 = DIRECTION ( 'NONE',  ( 0.000000000000000000, 0.000000000000000000, -1.000000000000000000 ) ) ;
#25885 = CARTESIAN_POINT ( 'NONE',  ( 2.000000000000001776, -0.3246585432985730213, -6.805031400696120336 ) ) ;
#25886 = CARTESIAN_POINT ( 'NONE',  ( 1.549075743845170106, -12.58108552526744184, 1.533250336942571401 ) ) ;
#25887 = CARTESIAN_POINT ( 'NONE',  ( -22.49803948133828513, 3.817825231362860450, 2.073427785788346522 ) ) ;
#25888 = CIRCLE ( 'NONE', #37562, 7.499999999999988454 ) ;
#25889 = CARTESIAN_POINT ( 'NONE',  ( 5.516018279890452902, -0.003580555109620835435, 0.005752102158674384652 ) ) ;
#25890 = EDGE_CURVE ( 'NONE', #60382, #31853, #4241, .T. ) ;
#25891 = CARTESIAN_POINT ( 'NONE',  ( 2.000000000000001776, 6.253963800348250501, 4.139799123621038746 ) ) ;
#25892 = ORIENTED_EDGE ( 'NONE', *, *, #50552, .T. ) ;
#25893 = AXIS2_PLACEMENT_3D ( 'NONE', #23830, #34092, #58411 ) ;
#25894 = DIRECTION ( 'NONE',  ( -1.000000000000000000, 0.000000000000000000, -0.000000000000000000 ) ) ;
#25895 = EDGE_LOOP ( 'NONE', ( #2923, #23093, #31640, #43105 ) ) ;
#25896 = DIRECTION ( 'NONE',  ( -1.000000000000000000, 0.000000000000000000, -0.000000000000000000 ) ) ;
#25897 = CARTESIAN_POINT ( 'NONE',  ( 2.241352910868908754, 7.145045428366577411, 2.689314586382375527 ) ) ;
#25898 = CARTESIAN_POINT ( 'NONE',  ( -37.00000000000000711, -1.286231064351400555, 12.68495603654571369 ) ) ;
#25899 = FACE_OUTER_BOUND ( 'NONE', #57597, .T. ) ;
#25900 = AXIS2_PLACEMENT_3D ( 'NONE', #38843, #54472, #63756 ) ;
#25901 = ORIENTED_EDGE ( 'NONE', *, *, #51289, .T. ) ;
#25902 = ORIENTED_EDGE ( 'NONE', *, *, #22345, .T. ) ;
#25903 = CARTESIAN_POINT ( 'NONE',  ( -29.06834935496808470, 3.365517089803128137, 11.52551889874833080 ) ) ;
#25904 = EDGE_LOOP ( 'NONE', ( #3190, #8820, #36540, #48666 ) ) ;
#25905 = CARTESIAN_POINT ( 'NONE',  ( 2.268878695253351285, -6.544222817598194020, -3.949362208797132734 ) ) ;
#25906 = CARTESIAN_POINT ( 'NONE',  ( 2.241352910868909643, -3.744764251557037849, 6.652881166698498383 ) ) ;
#25907 = CARTESIAN_POINT ( 'NONE',  ( -22.27715526084302056, -3.395518526174221563, -1.423304177213884580 ) ) ;
#25908 = LINE ( 'NONE', #15898, #57678 ) ;
#25909 = FACE_OUTER_BOUND ( 'NONE', #55848, .T. ) ;
#25910 = CARTESIAN_POINT ( 'NONE',  ( 1.198791140420808921, 11.12379938352781927, -5.826488554585463220 ) ) ;
#25911 = DIRECTION ( 'NONE',  ( 0.000000000000000000, -0.01356324068817991828, 0.9999080150203990547 ) ) ;
#25912 = ORIENTED_EDGE ( 'NONE', *, *, #51716, .F. ) ;
#25913 = EDGE_CURVE ( 'NONE', #42570, #10611, #55158, .T. ) ;
#25914 = VECTOR ( 'NONE', #30778, 1000.000000000000000 ) ;
#25915 = CARTESIAN_POINT ( 'NONE',  ( -9.145100072270180291, -9.360112017720965127, -7.518496054314849353 ) ) ;
#25916 = EDGE_LOOP ( 'NONE', ( #27561, #58260, #65644, #3529 ) ) ;
#25917 = CARTESIAN_POINT ( 'NONE',  ( 1.375507693220405780, 4.865932489132489991, -11.64019206974694320 ) ) ;
#25918 = ADVANCED_FACE ( 'NONE', ( #13374 ), #29011, .T. ) ;
#25919 = DIRECTION ( 'NONE',  ( 0.000000000000000000, -0.3554799084909035511, -0.9346839223284514331 ) ) ;
#25920 = CARTESIAN_POINT ( 'NONE',  ( 19.28625800530496903, 1.699513388191793428, 11.87904264843580471 ) ) ;
#25921 = ORIENTED_EDGE ( 'NONE', *, *, #46024, .T. ) ;
#25922 = VERTEX_POINT ( 'NONE', #19028 ) ;
#25923 = FACE_OUTER_BOUND ( 'NONE', #33568, .T. ) ;
#25924 = AXIS2_PLACEMENT_3D ( 'NONE', #45419, #14495, #35098 ) ;
#25925 = CARTESIAN_POINT ( 'NONE',  ( 3.152665057734040488, 0.000000000000000000, 0.000000000000000000 ) ) ;
#25926 = FACE_OUTER_BOUND ( 'NONE', #10247, .T. ) ;
#25927 = CARTESIAN_POINT ( 'NONE',  ( -45.77739315166650869, -0.8244463642989293684, -12.03838484699752875 ) ) ;
#25928 = VERTEX_POINT ( 'NONE', #13692 ) ;
#25929 = AXIS2_PLACEMENT_3D ( 'NONE', #9481, #50081, #44403 ) ;
#25930 = VERTEX_POINT ( 'NONE', #16802 ) ;
#25931 = FACE_OUTER_BOUND ( 'NONE', #18976, .T. ) ;
#25932 = ORIENTED_EDGE ( 'NONE', *, *, #57218, .T. ) ;
#25933 = DIRECTION ( 'NONE',  ( 0.000000000000000000, 0.6745969609292663538, 0.7381862504171952111 ) ) ;
#25934 = ORIENTED_EDGE ( 'NONE', *, *, #5578, .F. ) ;
#25935 = AXIS2_PLACEMENT_3D ( 'NONE', #37378, #833, #27087 ) ;
#25936 = ORIENTED_EDGE ( 'NONE', *, *, #54218, .T. ) ;
#25937 = ORIENTED_EDGE ( 'NONE', *, *, #11482, .F. ) ;
#25938 = DIRECTION ( 'NONE',  ( 0.3939253465568944290, -0.7910971609033203844, -0.4679616473074870719 ) ) ;
#25939 = EDGE_CURVE ( 'NONE', #38363, #16604, #55818, .T. ) ;
#25940 = AXIS2_PLACEMENT_3D ( 'NONE', #48049, #2510, #42357 ) ;
#25941 = CARTESIAN_POINT ( 'NONE',  ( 1.287602823384975226, 11.62763122279957528, 4.819820779358876983 ) ) ;
#25942 = LINE ( 'NONE', #670, #4471 ) ;
#25943 = CARTESIAN_POINT ( 'NONE',  ( 2.305787727787084407, 2.774453000917245671, -7.135468203929955067 ) ) ;
#25944 = DIRECTION ( 'NONE',  ( 1.000000000000000000, 0.000000000000000000, 0.000000000000000000 ) ) ;
#25945 = ORIENTED_EDGE ( 'NONE', *, *, #32170, .F. ) ;
#25946 = CARTESIAN_POINT ( 'NONE',  ( 35.00000000000000000, -9.926225166346981155, 6.280308599560240346 ) ) ;
#25947 = ORIENTED_EDGE ( 'NONE', *, *, #5335, .F. ) ;
#25948 = DIRECTION ( 'NONE',  ( -1.000000000000000000, 0.000000000000000000, 0.000000000000000000 ) ) ;
#25949 = VECTOR ( 'NONE', #32370, 1000.000000000000000 ) ;
#25950 = CARTESIAN_POINT ( 'NONE',  ( -3.476444485811618801, 10.54985286295970504, 8.431306331566823076 ) ) ;
#25951 = B_SPLINE_CURVE_WITH_KNOTS ( 'NONE', 3,
 ( #43927, #17997, #49581, #48288, #58922, #18679, #28621, #59883, #8035, #3723, #23982, #2735, #14305, #38938, #13006, #44242 ),
 .UNSPECIFIED., .F., .F.,
 ( 4, 3, 3, 3, 3, 4 ),
 ( 0.000000000000000000, 0.0002999043160758550850, 0.0005998071753053377904, 0.0008997092107378087695, 0.001204458948196017627, 0.001510329163476902947 ),
 .UNSPECIFIED. ) ;
#25952 = CARTESIAN_POINT ( 'NONE',  ( -37.00000000000000711, -11.65150730582933392, -1.488153103997089888 ) ) ;
#25953 = B_SPLINE_CURVE_WITH_KNOTS ( 'NONE', 3,
 ( #59488, #60140, #29867, #19592, #9572, #29235, #28904, #50177, #4637, #49214, #39192, #13592, #59822, #65438, #24899, #19902, #40165, #13914 ),
 .UNSPECIFIED., .F., .F.,
 ( 4, 2, 2, 2, 2, 2, 2, 2, 4 ),
 ( 1.788112030672749005E-18, 0.0007433925613402978666, 0.001486785122680593998, 0.002230177684020890130, 0.002973570245361186262, 0.003716962806701481527, 0.004460355368041777659, 0.005203747929382072056, 0.005947140490722368188 ),
 .UNSPECIFIED. ) ;
#25954 = CARTESIAN_POINT ( 'NONE',  ( 0.3160775863651059669, -10.73821170199159525, 5.922381034681560408 ) ) ;
#25955 = CARTESIAN_POINT ( 'NONE',  ( -28.66013792860432119, 1.490739498621024284, -1.071635578228289587 ) ) ;
#25956 = CARTESIAN_POINT ( 'NONE',  ( 145.1370849898475797, 3.309064568108273190E-14, 0.000000000000000000 ) ) ;
#25957 = ADVANCED_FACE ( 'NONE', ( #32087, #48641 ), #43972, .F. ) ;
#25958 = VECTOR ( 'NONE', #15308, 1000.000000000000000 ) ;
#25959 = VERTEX_POINT ( 'NONE', #59270 ) ;
#25960 = DIRECTION ( 'NONE',  ( -1.000000000000000000, -0.000000000000000000, 0.000000000000000000 ) ) ;
#25961 = VERTEX_POINT ( 'NONE', #44283 ) ;
#25962 = CARTESIAN_POINT ( 'NONE',  ( -37.91369172636191820, -26.91879662985438415, -4.500000000000000888 ) ) ;
#25963 = CARTESIAN_POINT ( 'NONE',  ( 3.967932057708486671, -25.89885127696171452, -15.40358068932206237 ) ) ;
#25964 = CARTESIAN_POINT ( 'NONE',  ( 10.86013604962553991, -13.40624585479074327, -1.591185651104887411 ) ) ;
#25965 = CARTESIAN_POINT ( 'NONE',  ( -35.00000000000000000, -8.854740511458796703, -7.717887834988336415 ) ) ;
#25966 = CARTESIAN_POINT ( 'NONE',  ( -35.04834644901396956, -0.01183641858481921869, 0.007161132384413747970 ) ) ;
#25967 = VERTEX_POINT ( 'NONE', #28345 ) ;
#25968 = AXIS2_PLACEMENT_3D ( 'NONE', #40700, #10426, #51013 ) ;
#25969 = AXIS2_PLACEMENT_3D ( 'NONE', #9188, #65371, #29466 ) ;
#25970 = DIRECTION ( 'NONE',  ( 1.000000000000000000, 0.000000000000000000, 0.000000000000000000 ) ) ;
#25971 = FACE_OUTER_BOUND ( 'NONE', #7109, .T. ) ;
#25972 = CARTESIAN_POINT ( 'NONE',  ( 22.83374636504741773, 9.761338926624789636, -6.987695329749072037 ) ) ;
#25973 = CYLINDRICAL_SURFACE ( 'NONE', #21029, 12.75000000000000178 ) ;
#25974 = EDGE_CURVE ( 'NONE', #10303, #42026, #57893, .T. ) ;
#25975 = FACE_OUTER_BOUND ( 'NONE', #55543, .T. ) ;
#25976 = CLOSED_SHELL ( 'NONE', ( #44643, #48558, #19661, #49991, #41586, #24334, #121, #36034, #56988, #30685, #43062, #24819, #53057, #24105, #59164, #3853, #49242, #5907, #28079, #16221, #60409, #50074, #52039, #24651, #43527, #52939, #48320, #35051, #10833, #4790, #40205, #57600, #34532, #50567, #14351, #16199, #15692, #33869, #48533, #32955, #51344, #35186, #43275, #25957, #24994, #63281, #64931, #11328, #57523, #8437, #49612, #14855, #12672, #44814, #63865, #1709, #51455, #30245 ) ) ;
#25977 = DIRECTION ( 'NONE',  ( 0.000000000000000000, -0.01356324068817991828, 0.9999080150203990547 ) ) ;
#25978 = EDGE_CURVE ( 'NONE', #32947, #42367, #46408, .T. ) ;
#25979 = CARTESIAN_POINT ( 'NONE',  ( 1.452237505248555660, -11.67686475128083323, 4.880303821310969958 ) ) ;
#25980 = CARTESIAN_POINT ( 'NONE',  ( -35.00000000000000000, 10.28547182238008162, 5.672855678558722303 ) ) ;
#25981 = CARTESIAN_POINT ( 'NONE',  ( 2.284126774967659479, 0.1584898568958950094, -7.647017279602161821 ) ) ;
#25982 = EDGE_CURVE ( 'NONE', #56883, #62291, #38159, .T. ) ;
#25983 = VERTEX_POINT ( 'NONE', #62668 ) ;
#25984 = EDGE_LOOP ( 'NONE', ( #39881, #3857, #14914, #29747 ) ) ;
#25985 = FACE_OUTER_BOUND ( 'NONE', #46201, .T. ) ;
#25986 = CARTESIAN_POINT ( 'NONE',  ( 47.72075422404364531, -0.4543357781461463962, -7.770873616088282532 ) ) ;
#25987 = DIRECTION ( 'NONE',  ( 1.000000000000000000, 0.000000000000000000, 0.000000000000000000 ) ) ;
#25988 = FACE_OUTER_BOUND ( 'NONE', #29976, .T. ) ;
#25989 = EDGE_LOOP ( 'NONE', ( #11723, #57394, #27063, #24288 ) ) ;
#25990 = EDGE_CURVE ( 'NONE', #54859, #7383, #29640, .T. ) ;
#25991 = EDGE_LOOP ( 'NONE', ( #11051, #28611, #31300, #58088 ) ) ;
#25992 = VERTEX_POINT ( 'NONE', #53637 ) ;
#25993 = B_SPLINE_CURVE_WITH_KNOTS ( 'NONE', 3,
 ( #52420, #63342, #27132, #22134, #17152, #37424, #57738, #7163, #12157, #3183, #24106, #18138, #23450, #8158, #18492, #28761 ),
 .UNSPECIFIED., .F., .F.,
 ( 4, 3, 3, 3, 3, 4 ),
 ( 0.000000000000000000, 0.0003017745587525266023, 0.0006035491769808768846, 0.0009053241094668210186, 0.001207275924539022655, 0.001510325902531030025 ),
 .UNSPECIFIED. ) ;
#25994 = CARTESIAN_POINT ( 'NONE',  ( 3.152665057734036491, 7.923639299009025194, 0.4801242025592407647 ) ) ;
#25995 = VECTOR ( 'NONE', #2495, 1000.000000000000000 ) ;
#25996 = DIRECTION ( 'NONE',  ( 0.000000000000000000, -0.3554799084909036067, -0.9346839223284515441 ) ) ;
#25997 = ORIENTED_EDGE ( 'NONE', *, *, #29378, .T. ) ;
#25998 = CARTESIAN_POINT ( 'NONE',  ( 37.25000000000000000, -27.41745588273159839, 3.011965929904362405 ) ) ;
#25999 = CARTESIAN_POINT ( 'NONE',  ( 0.000000000000000000, 3.937687286050817193, 6.383151168292468647 ) ) ;
#26000 = ORIENTED_EDGE ( 'NONE', *, *, #40687, .F. ) ;
#26001 = CARTESIAN_POINT ( 'NONE',  ( 2.242418902652064006, 4.830735118999549549, -5.912154560271766002 ) ) ;
#26002 = CARTESIAN_POINT ( 'NONE',  ( 10.20102756488483209, -27.72270395345653782, -14.27139701651662129 ) ) ;
#26003 = CARTESIAN_POINT ( 'NONE',  ( -37.00000000000000711, -12.68495603654570836, -1.286231064351444742 ) ) ;
#26004 = ORIENTED_EDGE ( 'NONE', *, *, #44218, .F. ) ;
#26005 = DIRECTION ( 'NONE',  ( 0.000000000000000000, 0.4198891015602590482, 0.9075754196709594490 ) ) ;
#26006 = VERTEX_POINT ( 'NONE', #9685 ) ;
#26007 = CARTESIAN_POINT ( 'NONE',  ( 2.000000000000001776, 6.883677378339475794, 0.8544109087186002593 ) ) ;
#26008 = EDGE_LOOP ( 'NONE', ( #48570, #50931, #3205, #51706, #48330, #17429, #4065, #49625, #41861, #33137, #41287, #9084, #56667, #25526, #54387, #47115, #16661, #30618, #16906, #23628, #57780, #39034, #6760, #2475, #46310, #46136, #62298, #6308, #4441, #18335, #53532, #65397, #31712, #18814, #64076, #15158, #27089, #6243, #60907, #23937, #24727, #4673, #32067, #54325, #13693, #34057, #2958, #8255, #47149, #39498, #1085, #51368, #40960, #44295, #23155, #48973, #39931, #59758, #47156, #62195, #54555, #41100, #64267, #2856, #57613, #17885, #57912, #7183, #9588, #29828, #19457, #2195, #63964, #47003, #28600, #28410, #60773, #8483, #45079, #32377, #31695, #30090, #21924, #55890, #47026, #29242, #27295, #47332, #2034, #61438, #63011, #5731, #64265, #65584, #16157, #44669, #65219, #50526, #53086, #21636, #9082, #36770, #61314, #895, #49528, #8966, #11886, #33948, #41876, #46355, #57712, #48822, #49644, #25772, #34311, #7308, #34596, #48506, #49426, #10953, #52065, #22780, #34756, #31189, #50968, #15313, #21598, #51115, #65195, #19773, #12255, #17696, #25202, #37800, #37526, #60840, #31407, #7310, #41550, #43510, #22147, #24411, #20525, #14293, #55603, #18164, #32340, #35674, #56805, #39446, #15650, #59924, #45852, #53580, #61965, #5866, #41998, #33371, #25740, #34400, #9052, #50860, #60420, #38842, #57269, #2596, #51827, #64502, #48277, #52856, #14576, #16110, #3724, #44447, #59431, #11227, #40424, #26212, #18829, #15584, #51311, #56865, #40376, #59361, #42905, #1734, #34390, #1967, #62222, #43556, #19399, #51306, #38615, #15797, #41847, #41354, #25846, #10416, #22621, #27603, #55204, #22068, #6772, #55150, #59229, #23043, #41982, #62703, #11049, #56173, #56576, #18503, #9995, #53436, #17196, #22750, #17003, #31466, #47822, #35286, #9624, #43122, #64804, #46324, #31246, #3376, #54212, #14198, #13489, #41528, #12475, #19427, #27682, #59232, #59537, #15448, #42372, #49353, #24425, #20436, #61076, #37349, #11235, #26486, #35010, #61203, #30535, #20945, #60897, #4439, #36720, #6091, #44063, #54563, #55182, #51135, #51025, #49954, #47306, #3343, #57296, #49096, #20563, #36691, #58185, #11670, #53519, #26446, #50024, #9523, #37958, #50309, #29376, #10049, #9368, #19402, #28501, #36837, #38993, #53946, #37191, #33467, #39869, #61582, #34844, #47338, #29176, #43835, #56925, #26460, #25178, #11216, #8613, #21680, #30333, #33437, #57908, #363, #15971, #22009, #44056, #29223, #44252, #30162, #30920, #23786, #26634, #43296, #25378, #59530, #36818, #42475, #40549, #59370, #1954, #8393, #5915, #42490, #30832, #51355, #49203, #31499, #3578, #5499, #50329, #40155, #15476, #8538, #58291, #38586, #3013, #56854, #8908, #29121, #17883, #6977, #6686, #56583, #1960, #63650, #64052, #26875, #50870, #43941, #8735, #51829, #16783, #30799, #49358, #23047, #6875, #40008, #34166, #29635, #30697, #9619, #57519, #27826, #6310, #63424, #62060, #64011, #65002, #65154, #47327, #39418, #673, #5760, #18680, #12017, #10945, #11822, #33692, #27845, #32940, #20903, #32626, #59407, #64824, #1, #37178, #31037, #45708, #62039, #8957, #45775, #57408, #44545, #33256, #7319, #15346, #7509, #13256, #61132, #4667, #8143, #23808, #25372, #20672, #55209, #12781, #156, #1811, #59630, #59852 ) ) ;
#26009 = EDGE_LOOP ( 'NONE', ( #63350, #41635, #28795, #18896 ) ) ;
#26010 = CARTESIAN_POINT ( 'NONE',  ( 10.13605210956113822, -11.98069853244876803, -0.6880458654474965741 ) ) ;
#26011 = DIRECTION ( 'NONE',  ( -1.000000000000000000, 0.000000000000000000, 0.000000000000000000 ) ) ;
#26012 = DIRECTION ( 'NONE',  ( -1.000000000000000000, -1.836970198721029688E-16, 0.000000000000000000 ) ) ;
#26013 = CARTESIAN_POINT ( 'NONE',  ( -22.65999102136919419, -3.858590659383846155, -2.911035239830930710 ) ) ;
#26014 = CARTESIAN_POINT ( 'NONE',  ( 0.3665391374699472626, 9.237363111276875927, -8.095513416941138019 ) ) ;
#26015 = CARTESIAN_POINT ( 'NONE',  ( 9.215727626607732148, 1.931385612058147849, 11.84600384405800000 ) ) ;
#26016 = CARTESIAN_POINT ( 'NONE',  ( -27.08418179957658367, 2.244544746853584627, -0.4604195552868197705 ) ) ;
#26017 = CARTESIAN_POINT ( 'NONE',  ( 8.437200413559441614, 4.673024714880076758, -11.05476227139408252 ) ) ;
#26019 = VERTEX_POINT ( 'NONE', #9348 ) ;
#26018 = CARTESIAN_POINT ( 'NONE',  ( -18.56056789867630030, 4.666091029268902624, -12.67058235225230511 ) ) ;
#26020 = CARTESIAN_POINT ( 'NONE',  ( -35.05175862995318425, -0.007207337213509246165, -0.01030783735685852909 ) ) ;
#26021 = AXIS2_PLACEMENT_3D ( 'NONE', #15470, #45731, #50080 ) ;
#26022 = VERTEX_POINT ( 'NONE', #39628 ) ;
#26023 = CARTESIAN_POINT ( 'NONE',  ( -35.00000000000000000, 11.39945968423479883, -5.710938531231587234 ) ) ;
#26024 = CYLINDRICAL_SURFACE ( 'NONE', #53527, 12.18650000000000055 ) ;
#26025 = CIRCLE ( 'NONE', #55733, 5.000000000000000888 ) ;
#26027 = ORIENTED_EDGE ( 'NONE', *, *, #15444, .T. ) ;
#26026 = EDGE_CURVE ( 'NONE', #10792, #57938, #45616, .T. ) ;
#26028 = DIRECTION ( 'NONE',  ( -1.000000000000000000, 0.000000000000000000, 0.000000000000000000 ) ) ;
#26029 = CARTESIAN_POINT ( 'NONE',  ( -35.00000000000000000, -11.23004253107761130, -4.732539170486383284 ) ) ;
#26030 = CYLINDRICAL_SURFACE ( 'NONE', #15310, 12.75000000000000178 ) ;
#26031 = FACE_OUTER_BOUND ( 'NONE', #53821, .T. ) ;
#26032 = EDGE_CURVE ( 'NONE', #15657, #14146, #59824, .T. ) ;
#26033 = CARTESIAN_POINT ( 'NONE',  ( 0.2655924914740778742, 10.58356227062117938, -6.161287456391572270 ) ) ;
#26034 = EDGE_LOOP ( 'NONE', ( #48639, #60190, #52149, #2973 ) ) ;
#26035 = CARTESIAN_POINT ( 'NONE',  ( -17.82060864339548090, -5.188839051198853802, -10.82117449455721570 ) ) ;
#26036 =( BOUNDED_SURFACE ( )  B_SPLINE_SURFACE ( 3, 1, ( 
 ( #30868, #15263 ),
 ( #20595, #25566 ),
 ( #35542, #50850 ),
 ( #41845, #5296 ) ),
 .UNSPECIFIED., .F., .F., .F. ) 
 B_SPLINE_SURFACE_WITH_KNOTS ( ( 4, 4 ),
 ( 2, 2 ),
 ( 0.000000000000000000, 1.000000000000000000 ),
 ( 0.000000000000000000, 1.000000000000000000 ),
 .UNSPECIFIED. ) 
 GEOMETRIC_REPRESENTATION_ITEM ( )  RATIONAL_B_SPLINE_SURFACE ( (
 ( 1.000000000000000000, 1.000000000000000000),
 ( 0.9942764183789327692, 0.8450855930916580938),
 ( 0.9942764183789327692, 0.8450855930916580938),
 ( 1.000000000000000000, 1.000000000000000000) ) ) 
 REPRESENTATION_ITEM ( '' )  SURFACE ( )  );
#26037 = ORIENTED_EDGE ( 'NONE', *, *, #51308, .F. ) ;
#26038 = CARTESIAN_POINT ( 'NONE',  ( 2.556980015512995585, 0.2307166419793596213, 7.736177238086449748 ) ) ;
#26039 = CYLINDRICAL_SURFACE ( 'NONE', #26043, 4.999999999999999112 ) ;
#26040 = CARTESIAN_POINT ( 'NONE',  ( 5.516018279890452902, 0.005752102158673841684, -0.003580555109620817654 ) ) ;
#26041 = ORIENTED_EDGE ( 'NONE', *, *, #44633, .T. ) ;
#26042 = CARTESIAN_POINT ( 'NONE',  ( 0.3474126878361827875, -4.439989671676146443, -11.44231427242454657 ) ) ;
#26043 = AXIS2_PLACEMENT_3D ( 'NONE', #25368, #19417, #20058 ) ;
#26044 = EDGE_CURVE ( 'NONE', #15993, #64802, #54920, .T. ) ;
#26045 = EDGE_CURVE ( 'NONE', #17119, #37122, #55248, .T. ) ;
#26046 = FACE_OUTER_BOUND ( 'NONE', #65307, .T. ) ;
#26047 = CARTESIAN_POINT ( 'NONE',  ( 49.02672294760360927, -0.1966872720628251858, -6.919866740913554359 ) ) ;
#26048 = EDGE_CURVE ( 'NONE', #56404, #28290, #9478, .T. ) ;
#26049 = CYLINDRICAL_SURFACE ( 'NONE', #45872, 12.75000000000000178 ) ;
#26050 = LINE ( 'NONE', #5449, #8373 ) ;
#26051 = EDGE_CURVE ( 'NONE', #39184, #31059, #5055, .T. ) ;
#26052 = CARTESIAN_POINT ( 'NONE',  ( 0.2650492433740076481, 2.017984765249233092, -12.07870441534853789 ) ) ;
#26053 = PRESENTATION_LAYER_ASSIGNMENT (  '', '', ( #52641 ) ) ;
#26054 = CARTESIAN_POINT ( 'NONE',  ( 2.941278708680199916, -4.048809123187966819, 4.615461433467243246 ) ) ;
#26055 = CARTESIAN_POINT ( 'NONE',  ( -26.74023318801843629, -1.916028097164416133, 2.752802096869872983 ) ) ;
#26056 = EDGE_CURVE ( 'NONE', #56916, #53395, #32888, .T. ) ;
#26057 = ORIENTED_EDGE ( 'NONE', *, *, #33046, .T. ) ;
#26058 = CARTESIAN_POINT ( 'NONE',  ( -15.45667515140707415, 7.965149195100730495, 10.89992138575203029 ) ) ;
#26059 = CARTESIAN_POINT ( 'NONE',  ( 17.77583356546081106, -10.71851000382461017, 8.238550139072438938 ) ) ;
#26060 = ORIENTED_EDGE ( 'NONE', *, *, #50558, .T. ) ;
#26061 = LINE ( 'NONE', #41663, #38531 ) ;
#26062 = EDGE_CURVE ( 'NONE', #59647, #62046, #22268, .T. ) ;
#26063 = CARTESIAN_POINT ( 'NONE',  ( -22.27715526084302056, 3.395518526174225560, 1.423304177213846167 ) ) ;
#26064 = DIRECTION ( 'NONE',  ( 1.000000000000000000, 0.000000000000000000, -0.000000000000000000 ) ) ;
#26065 = ORIENTED_EDGE ( 'NONE', *, *, #21027, .F. ) ;
#26066 = CARTESIAN_POINT ( 'NONE',  ( 2.288423627607478306, -6.543055113184245819, 3.963881558061940424 ) ) ;
#26067 = DIRECTION ( 'NONE',  ( 0.000000000000000000, 0.01356324068817991828, -0.9999080150203990547 ) ) ;
#26068 = ORIENTED_EDGE ( 'NONE', *, *, #16143, .F. ) ;
#26069 = ORIENTED_EDGE ( 'NONE', *, *, #33920, .F. ) ;
#26070 = ORIENTED_EDGE ( 'NONE', *, *, #38763, .T. ) ;
#26071 = CIRCLE ( 'NONE', #22898, 5.000000000000001776 ) ;
#26072 = FACE_OUTER_BOUND ( 'NONE', #63336, .T. ) ;
#26073 = ORIENTED_EDGE ( 'NONE', *, *, #45712, .T. ) ;
#26074 = ADVANCED_FACE ( 'NONE', ( #50286 ), #53213, .F. ) ;
#26075 = CARTESIAN_POINT ( 'NONE',  ( 2.000000000000001776, -6.164400007374799095, 2.900694413976478536 ) ) ;
#26076 = CARTESIAN_POINT ( 'NONE',  ( 0.3040950598368152291, -7.687624643091494292, 9.552450779732085451 ) ) ;
#26077 = LINE ( 'NONE', #56314, #34371 ) ;
#26078 = CARTESIAN_POINT ( 'NONE',  ( 2.000000000000001776, 5.860254403322073813, -3.474373880649762381 ) ) ;
#26079 = ORIENTED_EDGE ( 'NONE', *, *, #33263, .T. ) ;
#26080 = LINE ( 'NONE', #46035, #55518 ) ;
#26081 = CARTESIAN_POINT ( 'NONE',  ( 6.734959099364806079, -31.93290117444115594, 13.38585010773448580 ) ) ;
#26082 = CARTESIAN_POINT ( 'NONE',  ( 3.092491956585981860, -7.905533744258676165, 0.4473002062012166880 ) ) ;
#26084 = ORIENTED_EDGE ( 'NONE', *, *, #37561, .T. ) ;
#26083 = CARTESIAN_POINT ( 'NONE',  ( 35.00000000000000000, 4.705694406421931860E-17, -3.469127814946512892E-15 ) ) ;
#26085 = FACE_OUTER_BOUND ( 'NONE', #55753, .T. ) ;
#26086 = ORIENTED_EDGE ( 'NONE', *, *, #50509, .F. ) ;
#26087 = DIRECTION ( 'NONE',  ( -1.000000000000000000, 0.000000000000000000, 0.000000000000000000 ) ) ;
#26088 = ORIENTED_EDGE ( 'NONE', *, *, #34947, .F. ) ;
#26089 = ORIENTED_EDGE ( 'NONE', *, *, #22016, .F. ) ;
#26090 = CARTESIAN_POINT ( 'NONE',  ( 0.2648978790185593790, 9.465406350830713578, -7.769924372105106336 ) ) ;
#26091 = CARTESIAN_POINT ( 'NONE',  ( 18.18435566811206527, -29.77699652454509760, 8.006764386360600838 ) ) ;
#26092 = CARTESIAN_POINT ( 'NONE',  ( 2.253265082352431836, -7.637296367516837492, -0.1282654837135493442 ) ) ;
#26093 = VECTOR ( 'NONE', #50170, 1000.000000000000000 ) ;
#26094 = EDGE_LOOP ( 'NONE', ( #54251, #12026, #26027, #24468 ) ) ;
#26095 = DIRECTION ( 'NONE',  ( 0.000000000000000000, -0.01356324068817992175, 0.9999080150203990547 ) ) ;
#26096 = DIRECTION ( 'NONE',  ( 0.000000000000000000, -0.01356324068818000328, 0.9999080150203990547 ) ) ;
#26097 = DIRECTION ( 'NONE',  ( 0.000000000000000000, -0.1118654143051685257, -0.9937233664769753450 ) ) ;
#26098 = VERTEX_POINT ( 'NONE', #10032 ) ;
#26099 = B_SPLINE_CURVE_WITH_KNOTS ( 'NONE', 3,
 ( #34826, #35159, #64766, #8940, #14871, #24221, #55132, #4624, #9911, #24888, #49519, #48860, #9560, #45164, #23588, #44828, #9243, #49828, #19891, #34525, #4277, #14241 ),
 .UNSPECIFIED., .F., .F.,
 ( 4, 3, 3, 3, 3, 3, 3, 4 ),
 ( 1.203659747349087626E-18, 4.449119708436788016E-05, 6.626296329540349705E-05, 8.803456484962513971E-05, 0.0001098060367612775466, 0.0001315774408628478463, 0.0001760698110411114653, 0.0001829697163287828600 ),
 .UNSPECIFIED. ) ;
#26100 = ORIENTED_EDGE ( 'NONE', *, *, #13728, .T. ) ;
#26101 = CARTESIAN_POINT ( 'NONE',  ( 0.3160775863651096307, 12.03278055228170373, 2.365582350580104798 ) ) ;
#26102 = VERTEX_POINT ( 'NONE', #50606 ) ;
#26103 = ORIENTED_EDGE ( 'NONE', *, *, #3331, .F. ) ;
#26104 = DIRECTION ( 'NONE',  ( 0.000000000000000000, 0.6051742151937661296, -0.7960930657056429771 ) ) ;
#26105 = CARTESIAN_POINT ( 'NONE',  ( 37.00000000000000711, 4.705694406421931860E-17, -3.469127814946512892E-15 ) ) ;
#26106 = CARTESIAN_POINT ( 'NONE',  ( 2.034671305879700576, -9.742055912617322733, -6.436604249851277437 ) ) ;
#26107 = CARTESIAN_POINT ( 'NONE',  ( 18.77703285501462815, 0.5575356882853835794, 11.99009668352191760 ) ) ;
#26108 = CARTESIAN_POINT ( 'NONE',  ( 5.514970785353741078, -0.0003039746380524631733, 0.004713149585127259823 ) ) ;
#26109 = EDGE_CURVE ( 'NONE', #37925, #29278, #25317, .T. ) ;
#26110 = CARTESIAN_POINT ( 'NONE',  ( -10.25776720149870336, -3.790424196025902859, -11.38713284139628712 ) ) ;
#26111 = DIRECTION ( 'NONE',  ( 0.000000000000000000, 0.01356324068817998940, -0.9999080150203990547 ) ) ;
#26112 = VECTOR ( 'NONE', #6834, 1000.000000000000114 ) ;
#26113 = ORIENTED_EDGE ( 'NONE', *, *, #29562, .F. ) ;
#26114 = DIRECTION ( 'NONE',  ( 0.000000000000000000, -0.01356324068817998940, 0.9999080150203990547 ) ) ;
#26115 = CIRCLE ( 'NONE', #22953, 12.75000000000000178 ) ;
#26116 = CARTESIAN_POINT ( 'NONE',  ( 37.00000000000000711, 7.110831038798420600, 9.896810808925309288 ) ) ;
#26117 = EDGE_CURVE ( 'NONE', #54418, #10113, #32264, .T. ) ;
#26118 = CARTESIAN_POINT ( 'NONE',  ( -35.00000000000000000, -5.428340790341781741, 10.91072401419408777 ) ) ;
#26119 = DIRECTION ( 'NONE',  ( 0.000000000000000000, 0.01356324068817992175, -0.9999080150203990547 ) ) ;
#26120 = ADVANCED_FACE ( 'NONE', ( #52580 ), #37250, .T. ) ;
#26121 = CARTESIAN_POINT ( 'NONE',  ( 1.634816307077716191, 2.910502128621766271, -12.36483956257058203 ) ) ;
#26122 = DIRECTION ( 'NONE',  ( -0.9029087107030919768, 0.4298323628305345534, 0.000000000000000000 ) ) ;
#26123 = EDGE_CURVE ( 'NONE', #50717, #42378, #5284, .T. ) ;
#26124 = ORIENTED_EDGE ( 'NONE', *, *, #18758, .T. ) ;
#26125 = LINE ( 'NONE', #56734, #6979 ) ;
#26126 = CARTESIAN_POINT ( 'NONE',  ( 2.491965175174699176, 1.130870800982706204, -7.634639040875287996 ) ) ;
#26127 = DIRECTION ( 'NONE',  ( 0.000000000000000000, 0.3193015301359806712, -0.9476531711828022342 ) ) ;
#26128 = B_SPLINE_CURVE_WITH_KNOTS ( 'NONE', 3,
 ( #58382, #39391, #29419, #8821, #28434, #64336, #49714, #33096, #59053, #7849, #29110, #48417, #3189 ),
 .UNSPECIFIED., .F., .F.,
 ( 4, 3, 3, 3, 4 ),
 ( 6.254869361644796591E-18, 6.607593386745547301E-05, 0.0001321518677373515664, 0.0001982171734706181764, 0.0002642860854759457897 ),
 .UNSPECIFIED. ) ;
#26129 = CARTESIAN_POINT ( 'NONE',  ( 10.28941146347812108, 1.468011129749627663, -13.42080671719455509 ) ) ;
#26130 = CARTESIAN_POINT ( 'NONE',  ( 37.00000000000000711, -4.561791185930327508, 11.90598845858538013 ) ) ;
#26131 = VERTEX_POINT ( 'NONE', #51266 ) ;
#26132 = CARTESIAN_POINT ( 'NONE',  ( -17.69283485052123694, -9.508998116294153036, -9.587601754173576296 ) ) ;
#26133 = CARTESIAN_POINT ( 'NONE',  ( -27.69376440589343247, -12.79244479394529144, -4.322498630235340755 ) ) ;
#26134 = ADVANCED_FACE ( 'NONE', ( #11981 ), #31604, .T. ) ;
#26135 = CARTESIAN_POINT ( 'NONE',  ( 7.742519806647712777, -28.58895386040138220, -10.54525737088771287 ) ) ;
#26136 = EDGE_LOOP ( 'NONE', ( #40226, #32352, #52699, #65366 ) ) ;
#26137 = CARTESIAN_POINT ( 'NONE',  ( -9.197602943758385052, -12.97439165539571526, -3.730917860933688157 ) ) ;
#26138 = CARTESIAN_POINT ( 'NONE',  ( 5.515539859299206427, 0.003740028639278347548, -0.004759416711442189703 ) ) ;
#26139 = B_SPLINE_CURVE_WITH_KNOTS ( 'NONE', 3,
 ( #9233, #28878, #39500, #50153, #24210, #39170, #44171, #13568, #58850, #19568, #59463, #49509, #13888, #38863, #48849, #3949, #8271, #3647, #44476, #29514, #23912, #64754 ),
 .UNSPECIFIED., .F., .F.,
 ( 4, 2, 2, 2, 2, 2, 2, 2, 2, 2, 4 ),
 ( 0.002692368623994594382, 0.003420944312408854843, 0.004149520000823115305, 0.004878095689237376201, 0.005606671377651636229, 0.005970959221858770580, 0.006335247066065904931, 0.006699534910273039282, 0.007063822754480173632, 0.007792398442894443202, 0.008520974131308712771 ),
 .UNSPECIFIED. ) ;
#26140 = DIRECTION ( 'NONE',  ( -1.000000000000000000, 0.000000000000000000, -0.000000000000000000 ) ) ;
#26141 = ADVANCED_FACE ( 'NONE', ( #42220 ), #36924, .T. ) ;
#26143 = ORIENTED_EDGE ( 'NONE', *, *, #3253, .F. ) ;
#26142 = CARTESIAN_POINT ( 'NONE',  ( 2.000000000000001776, -6.539067737394485214, -2.314222412769890713 ) ) ;
#26144 = DIRECTION ( 'NONE',  ( -1.000000000000000000, 0.000000000000000000, 0.000000000000000000 ) ) ;
#26145 = EDGE_CURVE ( 'NONE', #25549, #3364, #42181, .T. ) ;
#26146 = AXIS2_PLACEMENT_3D ( 'NONE', #22069, #52680, #1492 ) ;
#26147 = DIRECTION ( 'NONE',  ( -1.000000000000000000, 0.000000000000000000, 0.000000000000000000 ) ) ;
#26148 = ORIENTED_EDGE ( 'NONE', *, *, #30507, .T. ) ;
#26149 = EDGE_CURVE ( 'NONE', #3825, #28939, #47569, .T. ) ;
#26150 = CARTESIAN_POINT ( 'NONE',  ( -35.05012975565874456, 0.009279204628448394984, 0.01039213056761046847 ) ) ;
#26151 = CARTESIAN_POINT ( 'NONE',  ( -37.00000000000000711, -11.42599468261432527, 4.237620530777758354 ) ) ;
#26153 = AXIS2_PLACEMENT_3D ( 'NONE', #37658, #27339, #16710 ) ;
#26152 = DIRECTION ( 'NONE',  ( 1.000000000000000000, 0.000000000000000000, 0.000000000000000000 ) ) ;
#26154 = CARTESIAN_POINT ( 'NONE',  ( 18.00005080000000035, 0.000000000000000000, 0.000000000000000000 ) ) ;
#26155 = CARTESIAN_POINT ( 'NONE',  ( -9.391855009251028008, 8.630551682975259098, -8.347810229187485831 ) ) ;
#26156 = EDGE_CURVE ( 'NONE', #56181, #634, #51918, .T. ) ;
#26157 = CARTESIAN_POINT ( 'NONE',  ( 2.241449424704145876, 2.553400830064077809, -7.194804211893820245 ) ) ;
#26159 = ORIENTED_EDGE ( 'NONE', *, *, #48874, .T. ) ;
#26158 = CARTESIAN_POINT ( 'NONE',  ( 0.3006302518452032557, 11.43947177966008510, -4.404090606399768681 ) ) ;
#26160 = ORIENTED_EDGE ( 'NONE', *, *, #11098, .F. ) ;
#26161 = DIRECTION ( 'NONE',  ( -1.000000000000000000, 0.000000000000000000, 0.000000000000000000 ) ) ;
#26162 = ORIENTED_EDGE ( 'NONE', *, *, #50547, .F. ) ;
#26163 =( NAMED_UNIT ( * ) PLANE_ANGLE_UNIT ( ) SI_UNIT ( $, .RADIAN. ) );
#26164 = DIRECTION ( 'NONE',  ( 1.000000000000000000, 0.000000000000000000, 0.000000000000000000 ) ) ;
#26165 = CARTESIAN_POINT ( 'NONE',  ( 0.3675815128205894289, 11.44679196252409348, 4.447030445008218535 ) ) ;
#26166 = DIRECTION ( 'NONE',  ( 1.000000000000000000, 0.000000000000000000, 0.000000000000000000 ) ) ;
#26167 = ORIENTED_EDGE ( 'NONE', *, *, #37311, .F. ) ;
#26168 = FACE_OUTER_BOUND ( 'NONE', #27551, .T. ) ;
#26169 = CARTESIAN_POINT ( 'NONE',  ( -24.55259447788195359, -9.550149982066713505, 7.269203354856432320 ) ) ;
#26170 = DIRECTION ( 'NONE',  ( 0.000000000000000000, -0.4698238015817428059, -0.8827602140260282226 ) ) ;
#26171 = EDGE_LOOP ( 'NONE', ( #24208, #46932, #65492, #53054 ) ) ;
#26172 = ORIENTED_EDGE ( 'NONE', *, *, #25050, .T. ) ;
#26173 = LINE ( 'NONE', #46444, #53437 ) ;
#26174 = ORIENTED_EDGE ( 'NONE', *, *, #6326, .T. ) ;
#26175 = DIRECTION ( 'NONE',  ( 0.000000000000000000, -0.01356324068817998940, 0.9999080150203990547 ) ) ;
#26176 = CARTESIAN_POINT ( 'NONE',  ( -27.09030469827880339, 0.5638997280370295906, -2.239626370111434284 ) ) ;
#26177 = CARTESIAN_POINT ( 'NONE',  ( 0.3040950598368144520, -8.072385578287534003, 9.229598020917661572 ) ) ;
#26178 = CARTESIAN_POINT ( 'NONE',  ( -27.09252613521593744, 1.005681546875665466, -2.086468883257839746 ) ) ;
#26179 = EDGE_CURVE ( 'NONE', #325, #17303, #56571, .T. ) ;
#26180 = CARTESIAN_POINT ( 'NONE',  ( -35.04709527796842394, -0.01120703303052195121, 0.005220632200989699934 ) ) ;
#26181 = DIRECTION ( 'NONE',  ( 0.000000000000000000, 0.000000000000000000, 1.000000000000000000 ) ) ;
#26182 = CARTESIAN_POINT ( 'NONE',  ( 3.459614771489464946, -11.09853614738469396, -7.685863346768205595 ) ) ;
#26183 = ORIENTED_EDGE ( 'NONE', *, *, #17590, .F. ) ;
#26184 = DIRECTION ( 'NONE',  ( 0.000000000000000000, -0.8169148498130212044, 0.5767582926625060002 ) ) ;
#26185 = CARTESIAN_POINT ( 'NONE',  ( 2.305787727787083519, 3.971363876084056166, -6.545285700970486786 ) ) ;
#26186 = CARTESIAN_POINT ( 'NONE',  ( 2.000000000000001776, -0.4804830611970390408, 6.919838746524553663 ) ) ;
#26187 = DIRECTION ( 'NONE',  ( 0.000000000000000000, 0.01356324068817992175, -0.9999080150203990547 ) ) ;
#26188 = LINE ( 'NONE', #45467, #14819 ) ;
#26189 = CARTESIAN_POINT ( 'NONE',  ( 2.000000000000001776, 0.000000000000000000, 0.000000000000000000 ) ) ;
#26190 = FACE_OUTER_BOUND ( 'NONE', #1756, .T. ) ;
#26191 = ADVANCED_FACE ( 'NONE', ( #25988 ), #26964, .T. ) ;
#26192 = AXIS2_PLACEMENT_3D ( 'NONE', #61724, #27147, #26817 ) ;
#26193 = CARTESIAN_POINT ( 'NONE',  ( 36.00000000000000711, 12.16893194857555116, 3.805206332242343947 ) ) ;
#26194 = ORIENTED_EDGE ( 'NONE', *, *, #27308, .T. ) ;
#26195 = VERTEX_POINT ( 'NONE', #21308 ) ;
#26196 = DIRECTION ( 'NONE',  ( 1.000000000000000000, 0.000000000000000000, -0.000000000000000000 ) ) ;
#26197 = AXIS2_PLACEMENT_3D ( 'NONE', #25403, #30394, #35025 ) ;
#26198 = ORIENTED_EDGE ( 'NONE', *, *, #63275, .T. ) ;
#26199 = CARTESIAN_POINT ( 'NONE',  ( 0.2646305136544065406, 12.24595685781654453, 0.1321451301298271763 ) ) ;
#26200 = CARTESIAN_POINT ( 'NONE',  ( -15.46066504888353954, 7.965027411696084414, -10.90001387300706526 ) ) ;
#26201 = CARTESIAN_POINT ( 'NONE',  ( 2.284126774967687457, 4.793997684221357858, 5.959830409747688407 ) ) ;
#26202 = CARTESIAN_POINT ( 'NONE',  ( 35.00000000000000000, 4.705694406421931860E-17, -3.469127814946512892E-15 ) ) ;
#26203 = EDGE_CURVE ( 'NONE', #61612, #28181, #61877, .T. ) ;
#26204 = ORIENTED_EDGE ( 'NONE', *, *, #16787, .T. ) ;
#26205 = DIRECTION ( 'NONE',  ( 0.000000000000000000, 0.01356324068817998940, -0.9999080150203990547 ) ) ;
#26206 = DIRECTION ( 'NONE',  ( 1.000000000000000000, 0.000000000000000000, 0.000000000000000000 ) ) ;
#26207 = CARTESIAN_POINT ( 'NONE',  ( 2.907497136251100400, -1.009055026157924084, 7.791429554169944538 ) ) ;
#26208 = CARTESIAN_POINT ( 'NONE',  ( 37.00000000000000711, 11.56998259273182583, 3.827046518384956020 ) ) ;
#26209 = DIRECTION ( 'NONE',  ( -1.000000000000000000, 0.000000000000000000, 0.000000000000000000 ) ) ;
#26210 = CARTESIAN_POINT ( 'NONE',  ( 2.244591118396557672, 2.712243649838700144, 7.137527852925261485 ) ) ;
#26211 =( BOUNDED_SURFACE ( )  B_SPLINE_SURFACE ( 3, 1, ( 
 ( #16642, #11642 ),
 ( #57213, #46568 ),
 ( #61210, #31913 ),
 ( #30603, #52235 ) ),
 .UNSPECIFIED., .F., .F., .T. ) 
 B_SPLINE_SURFACE_WITH_KNOTS ( ( 4, 4 ),
 ( 2, 2 ),
 ( 0.000000000000000000, 1.000000000000000000 ),
 ( 0.000000000000000000, 1.000000000000000000 ),
 .UNSPECIFIED. ) 
 GEOMETRIC_REPRESENTATION_ITEM ( )  RATIONAL_B_SPLINE_SURFACE ( (
 ( 1.000000000000000000, 1.000000000000000000),
 ( 0.6933888150995267674, 0.9895912004443193632),
 ( 0.6933888150995267674, 0.9895912004443193632),
 ( 1.000000000000000000, 1.000000000000000000) ) ) 
 REPRESENTATION_ITEM ( '' )  SURFACE ( )  );
#26212 = ORIENTED_EDGE ( 'NONE', *, *, #29363, .F. ) ;
#26213 = CYLINDRICAL_SURFACE ( 'NONE', #53028, 12.74999999999999822 ) ;
#26214 = VERTEX_POINT ( 'NONE', #46920 ) ;
#26215 = DIRECTION ( 'NONE',  ( -1.000000000000000000, 0.000000000000000000, 0.000000000000000000 ) ) ;
#26216 = DIRECTION ( 'NONE',  ( -1.000000000000000000, 0.000000000000000000, 0.000000000000000000 ) ) ;
#26217 = CARTESIAN_POINT ( 'NONE',  ( 5.514970785353741078, -0.003929719953530088142, 0.002619824551223743064 ) ) ;
#26218 = CARTESIAN_POINT ( 'NONE',  ( -35.04660725145885891, -0.004999447127056843958, 0.01123650152079029053 ) ) ;
#26219 = CARTESIAN_POINT ( 'NONE',  ( -7.000263073075360332, -1.818388804573970452, 11.86162824919947312 ) ) ;
#26220 = EDGE_CURVE ( 'NONE', #48023, #33594, #18011, .T. ) ;
#26221 = ORIENTED_EDGE ( 'NONE', *, *, #15529, .T. ) ;
#26222 = ORIENTED_EDGE ( 'NONE', *, *, #52709, .F. ) ;
#26223 = CARTESIAN_POINT ( 'NONE',  ( -35.00000000000000000, -7.817492529713920391, 9.348667969174380588 ) ) ;
#26224 = ADVANCED_FACE ( 'NONE', ( #43548 ), #59199, .T. ) ;
#26225 = ORIENTED_EDGE ( 'NONE', *, *, #54203, .F. ) ;
#26226 = DIRECTION ( 'NONE',  ( -1.000000000000000000, 0.000000000000000000, 0.000000000000000000 ) ) ;
#26227 = CARTESIAN_POINT ( 'NONE',  ( 3.489700430103022555, 6.891615640558352851, -11.63886720449249346 ) ) ;
#26228 = FACE_OUTER_BOUND ( 'NONE', #41580, .T. ) ;
#26229 = CARTESIAN_POINT ( 'NONE',  ( 3.459614771489464946, -11.09853614738469396, 25.00000000000000000 ) ) ;
#26230 = CARTESIAN_POINT ( 'NONE',  ( 22.88594695219327235, 3.421158645304719137, 11.50198563395281148 ) ) ;
#26231 = ADVANCED_FACE ( 'NONE', ( #53878 ), #26411, .F. ) ;
#26232 = CARTESIAN_POINT ( 'NONE',  ( 37.00000000000000711, -10.75351884295723970, 4.725891942574862448 ) ) ;
#26233 = CARTESIAN_POINT ( 'NONE',  ( -10.69899791063849648, -4.515810463815420839, 11.12485491063779897 ) ) ;
#26234 = VERTEX_POINT ( 'NONE', #12627 ) ;
#26235 = CARTESIAN_POINT ( 'NONE',  ( 0.4626703367445784698, -10.80124546303564337, 5.909149965570969165 ) ) ;
#26236 = VERTEX_POINT ( 'NONE', #7666 ) ;
#26237 = AXIS2_PLACEMENT_3D ( 'NONE', #20623, #61178, #40898 ) ;
#26238 = CARTESIAN_POINT ( 'NONE',  ( -36.00000000000000711, 11.59605747147786836, 5.300372733891682842 ) ) ;
#26239 = CARTESIAN_POINT ( 'NONE',  ( -35.00000000000000000, 10.75351884295727700, -4.725891942574793170 ) ) ;
#26240 = EDGE_LOOP ( 'NONE', ( #64200, #47777, #18383, #16369 ) ) ;
#26241 = AXIS2_PLACEMENT_3D ( 'NONE', #2716, #63506, #12985 ) ;
#26242 = CARTESIAN_POINT ( 'NONE',  ( -27.09833916700336687, 1.689564470273831276, 1.609723001518200247 ) ) ;
#26243 = DIRECTION ( 'NONE',  ( 0.000000000000000000, 0.6876994588534194319, 0.7259954919231345061 ) ) ;
#26244 = ORIENTED_EDGE ( 'NONE', *, *, #38232, .F. ) ;
#26245 = LINE ( 'NONE', #35556, #61968 ) ;
#26246 = CARTESIAN_POINT ( 'NONE',  ( -12.92674250727295870, -33.23908083897963905, -10.84893670414234279 ) ) ;
#26247 = CARTESIAN_POINT ( 'NONE',  ( 2.000000000000001776, -6.906413915731171471, -0.6453518998148326524 ) ) ;
#26248 = VERTEX_POINT ( 'NONE', #64176 ) ;
#26249 = ORIENTED_EDGE ( 'NONE', *, *, #7922, .T. ) ;
#26250 = CARTESIAN_POINT ( 'NONE',  ( 2.284736133211987319, 2.405285213157656976, 13.28910238183927639 ) ) ;
#26251 = VERTEX_POINT ( 'NONE', #12306 ) ;
#26252 = FACE_OUTER_BOUND ( 'NONE', #57063, .T. ) ;
#26253 = ORIENTED_EDGE ( 'NONE', *, *, #22003, .T. ) ;
#26254 = VERTEX_POINT ( 'NONE', #23953 ) ;
#26255 = ORIENTED_EDGE ( 'NONE', *, *, #24289, .T. ) ;
#26256 = CARTESIAN_POINT ( 'NONE',  ( 0.2647959493198551173, 4.326188315749736724, 11.45640103018460110 ) ) ;
#26257 = CARTESIAN_POINT ( 'NONE',  ( -13.26546321032140163, -27.53582555932709397, 12.33704161722047488 ) ) ;
#26258 = EDGE_CURVE ( 'NONE', #56858, #62784, #17316, .T. ) ;
#26259 = CARTESIAN_POINT ( 'NONE',  ( 2.899286259009688393, -1.011320371384287986, -7.788326766693360881 ) ) ;
#26260 = FACE_OUTER_BOUND ( 'NONE', #19698, .T. ) ;
#26261 = DIRECTION ( 'NONE',  ( -1.000000000000000000, -0.000000000000000000, 0.000000000000000000 ) ) ;
#26262 = ORIENTED_EDGE ( 'NONE', *, *, #32541, .T. ) ;
#26263 = CARTESIAN_POINT ( 'NONE',  ( 0.2648978790185619880, 2.256510822326142751, 12.03635331166812783 ) ) ;
#26264 = ADVANCED_FACE ( 'NONE', ( #32576 ), #7779, .F. ) ;
#26265 = ORIENTED_EDGE ( 'NONE', *, *, #7656, .F. ) ;
#26266 = FACE_OUTER_BOUND ( 'NONE', #4418, .T. ) ;
#26267 = B_SPLINE_CURVE_WITH_KNOTS ( 'NONE', 3,
 ( #3690, #23952, #44211, #19279, #59509, #29254, #39548, #59848, #34556, #49865, #44866, #4658, #29895, #40189, #65145, #30545 ),
 .UNSPECIFIED., .F., .F.,
 ( 4, 3, 3, 3, 3, 4 ),
 ( 3.599098170511143196E-15, 0.0002126834539179629465, 0.0004253519300366106863, 0.0006380165497223922117, 0.0007442707582427973267, 0.0009453531351419906022 ),
 .UNSPECIFIED. ) ;
#26268 = CARTESIAN_POINT ( 'NONE',  ( -27.08639648637140951, 0.6092497698725228839, 2.215564006614428205 ) ) ;
#26269 = DIRECTION ( 'NONE',  ( -0.000000000000000000, -1.000000000000000000, -0.000000000000000000 ) ) ;
#26270 = CARTESIAN_POINT ( 'NONE',  ( 0.2648321136542672316, -2.265911310221893515, 12.03456865502705497 ) ) ;
#26271 = CARTESIAN_POINT ( 'NONE',  ( -35.00000000000000000, 12.26766708251996540, -3.473736367725128726 ) ) ;
#26272 = DIRECTION ( 'NONE',  ( -1.000000000000000000, 0.000000000000000000, 0.000000000000000000 ) ) ;
#26273 = EDGE_CURVE ( 'NONE', #51107, #10675, #3359, .T. ) ;
#26274 = ORIENTED_EDGE ( 'NONE', *, *, #57127, .F. ) ;
#26275 = CARTESIAN_POINT ( 'NONE',  ( -35.00000000000000000, -10.63508530065525370, 4.986700593229667078 ) ) ;
#26276 = ORIENTED_EDGE ( 'NONE', *, *, #5895, .F. ) ;
#26277 = CARTESIAN_POINT ( 'NONE',  ( 0.2638984909335716500, -4.375449752477210907, 11.43908195192328137 ) ) ;
#26278 = LINE ( 'NONE', #25620, #38289 ) ;
#26279 = CARTESIAN_POINT ( 'NONE',  ( 3.100650473569739329, 6.348250400753959077, -4.737096019059198859 ) ) ;
#26280 = CYLINDRICAL_SURFACE ( 'NONE', #27729, 5.000000000000000888 ) ;
#26281 = CARTESIAN_POINT ( 'NONE',  ( 2.241526690369556096, 7.521460607153596101, 1.308664175663794227 ) ) ;
#26282 = EDGE_CURVE ( 'NONE', #36705, #44008, #58549, .T. ) ;
#26283 = EDGE_CURVE ( 'NONE', #55188, #13695, #53081, .T. ) ;
#26284 = VERTEX_POINT ( 'NONE', #19926 ) ;
#26285 = DIRECTION ( 'NONE',  ( -1.000000000000000000, 0.000000000000000000, 0.000000000000000000 ) ) ;
#26286 = CARTESIAN_POINT ( 'NONE',  ( 0.3278977287071200841, 2.374069413450301536, -12.03512402322220609 ) ) ;
#26287 = DIRECTION ( 'NONE',  ( -1.000000000000000000, 0.000000000000000000, 0.000000000000000000 ) ) ;
#26288 = AXIS2_PLACEMENT_3D ( 'NONE', #1406, #13001, #12650 ) ;
#26289 = CARTESIAN_POINT ( 'NONE',  ( 37.00000000000000711, 9.821084925794670184, 7.215058775251142364 ) ) ;
#26290 = ADVANCED_FACE ( 'NONE', ( #9599 ), #54856, .T. ) ;
#26291 = CARTESIAN_POINT ( 'NONE',  ( 16.78263030916553333, 25.00000000000000000, 5.836879698929882565 ) ) ;
#26292 = DIRECTION ( 'NONE',  ( 1.000000000000000000, 0.000000000000000000, 0.000000000000000000 ) ) ;
#26293 = DIRECTION ( 'NONE',  ( 0.000000000000000000, 0.000000000000000000, -1.000000000000000000 ) ) ;
#26294 = CARTESIAN_POINT ( 'NONE',  ( -19.68842116273439657, -11.76428741321061899, -2.390220401484857149 ) ) ;
#26295 = CARTESIAN_POINT ( 'NONE',  ( 37.00000000000000711, 4.705694406421931860E-17, -3.469127814946512892E-15 ) ) ;
#26296 = ADVANCED_FACE ( 'NONE', ( #65146 ), #13938, .T. ) ;
#26297 = VERTEX_POINT ( 'NONE', #24255 ) ;
#26298 = ADVANCED_FACE ( 'NONE', ( #45201 ), #14584, .T. ) ;
#26299 = ORIENTED_EDGE ( 'NONE', *, *, #6034, .F. ) ;
#26300 = CARTESIAN_POINT ( 'NONE',  ( 3.092491956585816215, -6.622742949902576726, 4.340140213817473835 ) ) ;
#26301 = CARTESIAN_POINT ( 'NONE',  ( 48.96282442591977713, -0.2094399512627206916, 1.553366803981121480 ) ) ;
#26302 = CARTESIAN_POINT ( 'NONE',  ( -37.00000000000000711, -6.950793414699719008, -10.68873102412850074 ) ) ;
#26303 = CARTESIAN_POINT ( 'NONE',  ( 0.3474126878361844528, -1.876013288000134116, 12.12932967384299765 ) ) ;
#26304 = ORIENTED_EDGE ( 'NONE', *, *, #59950, .T. ) ;
#26305 = ORIENTED_EDGE ( 'NONE', *, *, #11458, .F. ) ;
#26306 = ORIENTED_EDGE ( 'NONE', *, *, #42690, .F. ) ;
#26307 = CARTESIAN_POINT ( 'NONE',  ( 26.34661844826604593, -11.53221627053866527, 3.317828791472333005 ) ) ;
#26308 = VECTOR ( 'NONE', #38091, 1000.000000000000000 ) ;
#26309 = DIRECTION ( 'NONE',  ( 0.000000000000000000, 0.8989688749565142301, 0.4380125133594005016 ) ) ;
#26310 = ORIENTED_EDGE ( 'NONE', *, *, #12585, .F. ) ;
#26311 = DIRECTION ( 'NONE',  ( 0.000000000000000000, 0.01356324068817998940, -0.9999080150203990547 ) ) ;
#26312 = DIRECTION ( 'NONE',  ( -1.000000000000000000, 0.000000000000000000, 0.000000000000000000 ) ) ;
#26314 = ORIENTED_EDGE ( 'NONE', *, *, #31188, .T. ) ;
#26313 = AXIS2_PLACEMENT_3D ( 'NONE', #51356, #27356, #31377 ) ;
#26315 = CARTESIAN_POINT ( 'NONE',  ( -22.29115169517546136, 0.2790989024813086417, 3.712980101756706564 ) ) ;
#26316 = CARTESIAN_POINT ( 'NONE',  ( 14.79723931605636444, -33.90329588773487757, -8.884483617263549959 ) ) ;
#26317 = CARTESIAN_POINT ( 'NONE',  ( -47.00000000000000711, 0.000000000000000000, 0.000000000000000000 ) ) ;
#26318 = ORIENTED_EDGE ( 'NONE', *, *, #50641, .T. ) ;
#26319 = CARTESIAN_POINT ( 'NONE',  ( 0.3002738374340877536, 12.10874171309341918, -1.906042098268892371 ) ) ;
#26320 = ORIENTED_EDGE ( 'NONE', *, *, #48480, .T. ) ;
#26321 = CARTESIAN_POINT ( 'NONE',  ( 0.3675815128205894289, 7.689697408877401941, -9.574637318041888889 ) ) ;
#26322 = CARTESIAN_POINT ( 'NONE',  ( 2.241506898688418126, 4.937416071751840718, 5.822995664778275682 ) ) ;
#26323 = DIRECTION ( 'NONE',  ( 0.000000000000000000, 0.01356324068817998940, -0.9999080150203990547 ) ) ;
#26324 = CARTESIAN_POINT ( 'NONE',  ( 2.241352910868908754, 3.889181972941450738, 6.569501556381455387 ) ) ;
#26325 = CARTESIAN_POINT ( 'NONE',  ( -35.00000000000000000, 0.000000000000000000, 0.000000000000000000 ) ) ;
#26326 = CARTESIAN_POINT ( 'NONE',  ( 2.241352910868908754, -6.652881166698538351, 3.744764251556969903 ) ) ;
#26327 = CIRCLE ( 'NONE', #39040, 2.899999999999995026 ) ;
#26328 = CARTESIAN_POINT ( 'NONE',  ( -37.00000000000000711, -0.3025107581132014389, 11.74226168163341200 ) ) ;
#26329 = CARTESIAN_POINT ( 'NONE',  ( 0.3665391374699464300, -6.368473106897203806, 10.50279796150434564 ) ) ;
#26330 = CARTESIAN_POINT ( 'NONE',  ( 0.2653519890518161728, 4.188454465438684160, 11.50765826381078760 ) ) ;
#26332 = VERTEX_POINT ( 'NONE', #4317 ) ;
#26331 = CYLINDRICAL_SURFACE ( 'NONE', #43718, 12.74999999999999822 ) ;
#26333 = CARTESIAN_POINT ( 'NONE',  ( -36.00000000000000711, -7.608228585767650820, -10.23119532541081078 ) ) ;
#26334 = EDGE_CURVE ( 'NONE', #44332, #52979, #54913, .T. ) ;
#26335 = ORIENTED_EDGE ( 'NONE', *, *, #58452, .T. ) ;
#26336 = DIRECTION ( 'NONE',  ( -1.000000000000000000, 0.000000000000000000, 0.000000000000000000 ) ) ;
#26337 = DIRECTION ( 'NONE',  ( -1.000000000000000000, -0.000000000000000000, -0.000000000000000000 ) ) ;
#26338 = ORIENTED_EDGE ( 'NONE', *, *, #46571, .F. ) ;
#26339 = CARTESIAN_POINT ( 'NONE',  ( 2.491965175174414959, 7.322278065136198499, 2.439431489055664315 ) ) ;
#26340 = FACE_OUTER_BOUND ( 'NONE', #33661, .T. ) ;
#26341 = CARTESIAN_POINT ( 'NONE',  ( -27.10307689719059709, -2.250862122746733807, 0.6678239540327238766 ) ) ;
#26342 = CARTESIAN_POINT ( 'NONE',  ( 1.719304012341582588, 7.017415949614099979, -10.62216384465570762 ) ) ;
#26343 = DIRECTION ( 'NONE',  ( 1.000000000000000000, 0.000000000000000000, 0.000000000000000000 ) ) ;
#26344 = EDGE_CURVE ( 'NONE', #3284, #21988, #4169, .T. ) ;
#26345 = ORIENTED_EDGE ( 'NONE', *, *, #38025, .F. ) ;
#26346 = CARTESIAN_POINT ( 'NONE',  ( 6.361445718264521432, -4.355102044641763648, 12.77822703589027320 ) ) ;
#26347 = VERTEX_POINT ( 'NONE', #55841 ) ;
#26348 = CARTESIAN_POINT ( 'NONE',  ( -35.04660725145885891, -0.009947898977292157080, 0.007231372203115632620 ) ) ;
#26349 = DIRECTION ( 'NONE',  ( 1.000000000000000000, 0.000000000000000000, 0.000000000000000000 ) ) ;
#26350 = B_SPLINE_CURVE_WITH_KNOTS ( 'NONE', 3,
 ( #55200, #45893, #40901, #29590, #61180, #39905, #64831, #5327, #14612, #34894 ),
 .UNSPECIFIED., .F., .F.,
 ( 4, 3, 3, 4 ),
 ( 5.401523115762579325E-05, 0.0008136511341527786004, 0.004068255670953081077, 0.005063778443040918738 ),
 .UNSPECIFIED. ) ;
#26351 = DIRECTION ( 'NONE',  ( -1.000000000000000000, 0.000000000000000000, 0.000000000000000000 ) ) ;
#26352 = EDGE_CURVE ( 'NONE', #33280, #44784, #49908, .T. ) ;
#26353 = VERTEX_POINT ( 'NONE', #60160 ) ;
#26354 = DIRECTION ( 'NONE',  ( 0.000000000000000000, -0.9635499925192254622, 0.2675283385292119842 ) ) ;
#26355 = AXIS2_PLACEMENT_3D ( 'NONE', #42505, #26261, #16615 ) ;
#26356 = VECTOR ( 'NONE', #25295, 1000.000000000000000 ) ;
#26357 = CARTESIAN_POINT ( 'NONE',  ( 3.618571554686948577, 8.318316264554038497, 8.649151353875890180 ) ) ;
#26358 = CARTESIAN_POINT ( 'NONE',  ( 37.00000000000000711, 10.07641281632177588, -6.036400161834603928 ) ) ;
#26360 = CIRCLE ( 'NONE', #39079, 7.499999999999988454 ) ;
#26359 = CARTESIAN_POINT ( 'NONE',  ( -37.00000000000000711, -10.64792938439751424, -5.927257550915432383 ) ) ;
#26361 = CARTESIAN_POINT ( 'NONE',  ( -22.31328051695926007, 0.8849444482788259014, -3.685074213229314388 ) ) ;
#26362 = CARTESIAN_POINT ( 'NONE',  ( 1.633930747250947002, 5.012862767613547987, 11.67150509329667685 ) ) ;
#26363 = CARTESIAN_POINT ( 'NONE',  ( 1.375507693219673255, -3.754650692913064525, -12.04466556545244771 ) ) ;
#26364 = VECTOR ( 'NONE', #44996, 1000.000000000000114 ) ;
#26365 = EDGE_CURVE ( 'NONE', #62061, #41285, #51993, .T. ) ;
#26366 = ORIENTED_EDGE ( 'NONE', *, *, #13430, .T. ) ;
#26367 = CARTESIAN_POINT ( 'NONE',  ( -18.08686583997218733, 5.151216734910788908, 12.47858029384653733 ) ) ;
#26368 = CARTESIAN_POINT ( 'NONE',  ( 6.788772321873702609, -6.731768924035796964, 11.70805477083968782 ) ) ;
#26369 = VERTEX_POINT ( 'NONE', #24927 ) ;
#26370 = CARTESIAN_POINT ( 'NONE',  ( 0.7446945582506641070, 10.56139717223413577, 6.508900271375134494 ) ) ;
#26371 = CARTESIAN_POINT ( 'NONE',  ( -22.27720387087365239, 3.430312021254886989, 1.337073746937850860 ) ) ;
#26372 = CARTESIAN_POINT ( 'NONE',  ( -9.810797966268966164, 12.34121403900716984, -5.475695573403694283 ) ) ;
#26373 = ORIENTED_EDGE ( 'NONE', *, *, #9872, .T. ) ;
#26374 = CARTESIAN_POINT ( 'NONE',  ( 2.266490820343228130, -6.544980046121050776, 3.946561086901452686 ) ) ;
#26375 = FACE_OUTER_BOUND ( 'NONE', #29781, .T. ) ;
#26376 = EDGE_LOOP ( 'NONE', ( #64627, #38131, #58238, #50321 ) ) ;
#26377 = CARTESIAN_POINT ( 'NONE',  ( 0.2872850955227745917, -5.944938343726327012, 10.71476594226531986 ) ) ;
#26378 = ORIENTED_EDGE ( 'NONE', *, *, #16393, .T. ) ;
#26379 = EDGE_LOOP ( 'NONE', ( #879, #35259, #39572, #17219 ) ) ;
#26380 = B_SPLINE_CURVE_WITH_KNOTS ( 'NONE', 3,
 ( #8944, #59813, #54507, #4943, #49524, #30201, #54827, #24225, #14246, #4281, #45167, #39516, #29528, #49832, #24553, #64145, #18922, #44833, #8608 ),
 .UNSPECIFIED., .F., .F.,
 ( 4, 3, 3, 3, 3, 3, 4 ),
 ( 0.000000000000000000, 2.831840207499405278E-05, 4.217266859840229838E-05, 5.602024318395587826E-05, 6.290810167968577719E-05, 9.120440630944289440E-05, 0.0001153103026479761575 ),
 .UNSPECIFIED. ) ;
#26381 = EDGE_CURVE ( 'NONE', #47012, #4327, #59851, .T. ) ;
#26382 = CYLINDRICAL_SURFACE ( 'NONE', #54977, 13.50000000000000178 ) ;
#26383 = CIRCLE ( 'NONE', #44452, 4.999999999999999112 ) ;
#26384 = VERTEX_POINT ( 'NONE', #9277 ) ;
#26385 = FACE_OUTER_BOUND ( 'NONE', #13519, .T. ) ;
#26386 = CARTESIAN_POINT ( 'NONE',  ( 2.000000000000001776, 0.000000000000000000, 0.000000000000000000 ) ) ;
#26387 = CARTESIAN_POINT ( 'NONE',  ( -37.00000000000000711, 3.213188559034398040, -11.29812557209473667 ) ) ;
#26388 = CARTESIAN_POINT ( 'NONE',  ( -47.00000000000000711, 0.000000000000000000, 0.000000000000000000 ) ) ;
#26389 = ORIENTED_EDGE ( 'NONE', *, *, #64345, .T. ) ;
#26390 = DIRECTION ( 'NONE',  ( -1.000000000000000000, 0.000000000000000000, 0.000000000000000000 ) ) ;
#26391 = CARTESIAN_POINT ( 'NONE',  ( 5.911253750797971662, -28.27393032148221863, 11.47047724608643371 ) ) ;
#26392 = DIRECTION ( 'NONE',  ( 0.000000000000000000, -0.7381862504171878836, 0.6745969609292743474 ) ) ;
#26394 = ORIENTED_EDGE ( 'NONE', *, *, #23838, .F. ) ;
#26393 = CARTESIAN_POINT ( 'NONE',  ( 0.3040950598368152291, 8.072385578287471830, 9.229598020917713086 ) ) ;
#26395 = CARTESIAN_POINT ( 'NONE',  ( -28.15409021793930933, 11.30913317806512985, -4.025053242516860585 ) ) ;
#26396 = ORIENTED_EDGE ( 'NONE', *, *, #32715, .T. ) ;
#26397 = LINE ( 'NONE', #62609, #61422 ) ;
#26398 = VERTEX_POINT ( 'NONE', #35204 ) ;
#26399 = ORIENTED_EDGE ( 'NONE', *, *, #48260, .T. ) ;
#26400 = CARTESIAN_POINT ( 'NONE',  ( 0.2648321136542691190, 9.471460387169383210, -7.762514728657997409 ) ) ;
#26401 = CARTESIAN_POINT ( 'NONE',  ( -35.00000000000000000, 0.000000000000000000, 0.000000000000000000 ) ) ;
#26402 = AXIS2_PLACEMENT_3D ( 'NONE', #32130, #27159, #17181 ) ;
#26403 = DIRECTION ( 'NONE',  ( 0.000000000000000000, 0.01356324068817998940, -0.9999080150203989437 ) ) ;
#26404 = VERTEX_POINT ( 'NONE', #50206 ) ;
#26405 = DIRECTION ( 'NONE',  ( 1.000000000000000000, -0.000000000000000000, 0.000000000000000000 ) ) ;
#26406 = CARTESIAN_POINT ( 'NONE',  ( 3.152665057734040488, 0.000000000000000000, 0.000000000000000000 ) ) ;
#26407 = DIRECTION ( 'NONE',  ( -1.000000000000000000, -0.000000000000000000, 0.000000000000000000 ) ) ;
#26408 = EDGE_LOOP ( 'NONE', ( #27932, #65536, #44316, #13171 ) ) ;
#26409 = VECTOR ( 'NONE', #36914, 1000.000000000000000 ) ;
#26410 = ADVANCED_FACE ( 'NONE', ( #34862 ), #40191, .T. ) ;
#26411 =( BOUNDED_SURFACE ( )  B_SPLINE_SURFACE ( 3, 1, ( 
 ( #3691, #63496 ),
 ( #38574, #58892 ),
 ( #28929, #37595 ),
 ( #3352, #23621 ) ),
 .UNSPECIFIED., .F., .F., .F. ) 
 B_SPLINE_SURFACE_WITH_KNOTS ( ( 4, 4 ),
 ( 2, 2 ),
 ( 0.000000000000000000, 1.000000000000000000 ),
 ( 0.000000000000000000, 1.000000000000000000 ),
 .UNSPECIFIED. ) 
 GEOMETRIC_REPRESENTATION_ITEM ( )  RATIONAL_B_SPLINE_SURFACE ( (
 ( 1.000000000000000000, 1.000000000000000000),
 ( 0.6933888150995267674, 0.9895912004443193632),
 ( 0.6933888150995267674, 0.9895912004443193632),
 ( 1.000000000000000000, 1.000000000000000000) ) ) 
 REPRESENTATION_ITEM ( '' )  SURFACE ( )  );
#26412 = ORIENTED_EDGE ( 'NONE', *, *, #29617, .F. ) ;
#26413 = ADVANCED_FACE ( 'NONE', ( #44868 ), #55511, .T. ) ;
#26414 = DIRECTION ( 'NONE',  ( 1.000000000000000000, 0.000000000000000000, 0.000000000000000000 ) ) ;
#26415 = ORIENTED_EDGE ( 'NONE', *, *, #18769, .T. ) ;
#26416 = EDGE_CURVE ( 'NONE', #8847, #8493, #64728, .T. ) ;
#26417 = ORIENTED_EDGE ( 'NONE', *, *, #33147, .T. ) ;
#26418 = LINE ( 'NONE', #20453, #14732 ) ;
#26419 = DIRECTION ( 'NONE',  ( -1.000000000000000000, 0.000000000000000000, -0.000000000000000000 ) ) ;
#26420 = DIRECTION ( 'NONE',  ( 0.000000000000000000, 0.000000000000000000, 1.000000000000000000 ) ) ;
#26421 = DIRECTION ( 'NONE',  ( 0.000000000000000000, 0.9651210252299803338, 0.2618041379715600470 ) ) ;
#26422 = FACE_OUTER_BOUND ( 'NONE', #36086, .T. ) ;
#26423 = CARTESIAN_POINT ( 'NONE',  ( -25.00000000000000355, -28.99999999999999645, 1.530808498934191521E-15 ) ) ;
#26424 = EDGE_CURVE ( 'NONE', #52497, #41192, #16039, .T. ) ;
#26425 = LINE ( 'NONE', #20785, #46108 ) ;
#26426 = VERTEX_POINT ( 'NONE', #52507 ) ;
#26427 = CARTESIAN_POINT ( 'NONE',  ( 5.514970785353741078, 0.0003039746380524305930, -0.004713149585127262425 ) ) ;
#26428 = DIRECTION ( 'NONE',  ( 1.000000000000000000, 0.000000000000000000, 0.000000000000000000 ) ) ;
#26429 = CARTESIAN_POINT ( 'NONE',  ( 0.2648321136542688414, 4.321267941897666276, -11.45826514585339062 ) ) ;
#26430 = DIRECTION ( 'NONE',  ( -1.000000000000000000, -0.000000000000000000, 0.000000000000000000 ) ) ;
#26431 = B_SPLINE_CURVE_WITH_KNOTS ( 'NONE', 3,
 ( #15467, #10469, #24803, #51061, #10154, #9818, #50730, #838, #55380, #40399, #14788, #35069, #25786, #20465, #30111, #50415, #4859, #46077, #51408 ),
 .UNSPECIFIED., .F., .F.,
 ( 4, 3, 3, 3, 3, 3, 4 ),
 ( 7.298863197736074879E-18, 2.825908398831414518E-05, 4.208813692484295868E-05, 5.591713746944392975E-05, 6.279584083232444592E-05, 9.105792820297390646E-05, 0.0001153131102488855946 ),
 .UNSPECIFIED. ) ;
#26432 = EDGE_CURVE ( 'NONE', #57595, #2022, #9574, .T. ) ;
#26433 = AXIS2_PLACEMENT_3D ( 'NONE', #22079, #16457, #53343 ) ;
#26434 = CARTESIAN_POINT ( 'NONE',  ( 24.05910844200719367, -2.469428917447811678, -13.27331698206481292 ) ) ;
#26435 = CARTESIAN_POINT ( 'NONE',  ( -25.00000000000000355, -9.999999999999998224, 24.00000000000000000 ) ) ;
#26436 = CYLINDRICAL_SURFACE ( 'NONE', #29909, 12.74999999999999822 ) ;
#26437 = VERTEX_POINT ( 'NONE', #16903 ) ;
#26438 = DIRECTION ( 'NONE',  ( -0.000000000000000000, -0.000000000000000000, -1.000000000000000000 ) ) ;
#26439 = CARTESIAN_POINT ( 'NONE',  ( 2.903928887687730942, -3.491800274469421428, -8.044738195290898730 ) ) ;
#26440 = CYLINDRICAL_SURFACE ( 'NONE', #28955, 5.000000000000000888 ) ;
#26441 = DIRECTION ( 'NONE',  ( 0.000000000000000000, 0.8835120444460210498, 0.4684084406997938155 ) ) ;
#26442 = CIRCLE ( 'NONE', #46628, 12.18649999999999878 ) ;
#26443 = CARTESIAN_POINT ( 'NONE',  ( 9.382075856650567758, 2.626741102731213306, -13.24370663063512765 ) ) ;
#26444 = CARTESIAN_POINT ( 'NONE',  ( 5.536195898058073439, 0.001726268814999623981, 0.008323005098841079058 ) ) ;
#26445 = AXIS2_PLACEMENT_3D ( 'NONE', #22793, #27425, #57374 ) ;
#26446 = ORIENTED_EDGE ( 'NONE', *, *, #49969, .F. ) ;
#26447 = CARTESIAN_POINT ( 'NONE',  ( -17.56015734194049216, -5.645012286831811998, -12.26409170071914012 ) ) ;
#26448 = DIRECTION ( 'NONE',  ( -0.000000000000000000, 0.000000000000000000, 1.000000000000000000 ) ) ;
#26449 = DIRECTION ( 'NONE',  ( 1.000000000000000000, 0.000000000000000000, 0.000000000000000000 ) ) ;
#26450 = ORIENTED_EDGE ( 'NONE', *, *, #61641, .T. ) ;
#26451 = CARTESIAN_POINT ( 'NONE',  ( 2.907497136250849934, 6.976431712756603787, 3.613027414876627041 ) ) ;
#26452 = CARTESIAN_POINT ( 'NONE',  ( 35.00000000000000000, 10.75351884295727345, -4.725891942574794058 ) ) ;
#26453 = CARTESIAN_POINT ( 'NONE',  ( 5.516018279890452902, -0.001397286410094361001, 0.006629829924290971295 ) ) ;
#26454 = AXIS2_PLACEMENT_3D ( 'NONE', #35068, #61339, #26114 ) ;
#26456 = ORIENTED_EDGE ( 'NONE', *, *, #54178, .F. ) ;
#26455 = CARTESIAN_POINT ( 'NONE',  ( 2.507146904658097419, 1.127530020444497572, 7.640248566386898865 ) ) ;
#26457 = DIRECTION ( 'NONE',  ( 0.000000000000000000, -0.9868265225415276953, 0.1617819965527551584 ) ) ;
#26458 = EDGE_CURVE ( 'NONE', #21944, #18385, #60525, .T. ) ;
#26459 = CARTESIAN_POINT ( 'NONE',  ( 0.2646305136544072623, 9.296005949277336811, -7.972778379581457742 ) ) ;
#26460 = ORIENTED_EDGE ( 'NONE', *, *, #50156, .F. ) ;
#26461 = CARTESIAN_POINT ( 'NONE',  ( 0.2759803524722195811, 7.727919584673444753, 9.504501710971627659 ) ) ;
#26462 = CYLINDRICAL_SURFACE ( 'NONE', #18130, 12.75000000000000178 ) ;
#26463 = DIRECTION ( 'NONE',  ( -1.000000000000000000, 0.000000000000000000, 0.000000000000000000 ) ) ;
#26464 = CARTESIAN_POINT ( 'NONE',  ( -4.050991451692300238, -11.17498730987891875, 7.585040469053804912 ) ) ;
#26465 = DIRECTION ( 'NONE',  ( 0.000000000000000000, 0.000000000000000000, -1.000000000000000000 ) ) ;
#26467 = ORIENTED_EDGE ( 'NONE', *, *, #2867, .T. ) ;
#26466 = LINE ( 'NONE', #46754, #57354 ) ;
#26468 = VERTEX_POINT ( 'NONE', #21229 ) ;
#26469 = CARTESIAN_POINT ( 'NONE',  ( -29.60265935865812637, -3.677894516095094879, 12.98940028976120509 ) ) ;
#26470 = ORIENTED_EDGE ( 'NONE', *, *, #21661, .T. ) ;
#26471 = CARTESIAN_POINT ( 'NONE',  ( -8.625915963927961390E-16, -25.52675992528908466, -4.096732089186954621E-16 ) ) ;
#26472 = DIRECTION ( 'NONE',  ( -1.000000000000000000, 0.000000000000000000, 0.000000000000000000 ) ) ;
#26473 = FACE_OUTER_BOUND ( 'NONE', #18985, .T. ) ;
#26474 = CIRCLE ( 'NONE', #63628, 12.74999999999999822 ) ;
#26475 = EDGE_CURVE ( 'NONE', #50103, #10610, #9525, .T. ) ;
#26476 = CARTESIAN_POINT ( 'NONE',  ( -35.00000000000000000, -10.49626516989265923, -7.238157050195740183 ) ) ;
#26477 = VERTEX_POINT ( 'NONE', #37174 ) ;
#26478 = CARTESIAN_POINT ( 'NONE',  ( 0.3665391374699464300, -10.50279796150432432, -6.368473106897240221 ) ) ;
#26479 = CARTESIAN_POINT ( 'NONE',  ( 0.2655924914740778187, 11.52280271232876352, -4.147079829127140016 ) ) ;
#26480 = ADVANCED_FACE ( 'NONE', ( #35847 ), #30869, .T. ) ;
#26481 = CARTESIAN_POINT ( 'NONE',  ( 37.00000000000000711, 4.705694406421931860E-17, -3.469127814946512892E-15 ) ) ;
#26482 = VERTEX_POINT ( 'NONE', #31535 ) ;
#26483 = ORIENTED_EDGE ( 'NONE', *, *, #52025, .F. ) ;
#26484 = CARTESIAN_POINT ( 'NONE',  ( 29.23219761849493281, -9.462903118444481620, 9.637299545766000008 ) ) ;
#26485 = EDGE_CURVE ( 'NONE', #20918, #28876, #14498, .T. ) ;
#26486 = ORIENTED_EDGE ( 'NONE', *, *, #5687, .F. ) ;
#26487 = DIRECTION ( 'NONE',  ( -1.000000000000000000, 0.000000000000000000, 0.000000000000000000 ) ) ;
#26488 = DIRECTION ( 'NONE',  ( 0.000000000000000000, -0.01356324068817992175, 0.9999080150203990547 ) ) ;
#26489 = CARTESIAN_POINT ( 'NONE',  ( 12.52750123246316072, 0.4973700281276248192, 11.98968819674307618 ) ) ;
#26491 = VECTOR ( 'NONE', #62200, 1000.000000000000000 ) ;
#26490 = DIRECTION ( 'NONE',  ( 0.000000000000000000, -0.01356324068817998940, 0.9999080150203990547 ) ) ;
#26492 = DIRECTION ( 'NONE',  ( 0.000000000000000000, 0.1387779952735819222, -0.9903235168508549569 ) ) ;
#26493 = LINE ( 'NONE', #21524, #34868 ) ;
#26494 = EDGE_CURVE ( 'NONE', #4396, #15089, #4292, .T. ) ;
#26495 = DIRECTION ( 'NONE',  ( 1.000000000000000000, 0.000000000000000000, -0.000000000000000000 ) ) ;
#26496 = AXIS2_PLACEMENT_3D ( 'NONE', #64316, #48714, #63645 ) ;
#26497 = ORIENTED_EDGE ( 'NONE', *, *, #2001, .F. ) ;
#26498 = CARTESIAN_POINT ( 'NONE',  ( 0.7400311444011739015, 12.39937114182724009, -0.3548322008127505200 ) ) ;
#26499 = ADVANCED_FACE ( 'NONE', ( #38496 ), #58464, .T. ) ;
#26500 = CARTESIAN_POINT ( 'NONE',  ( 35.00000000000000000, 10.14408668126221613, 5.921969905510239940 ) ) ;
#26501 = LINE ( 'NONE', #27166, #11506 ) ;
#26502 = CARTESIAN_POINT ( 'NONE',  ( -35.00000000000000000, 0.000000000000000000, 0.000000000000000000 ) ) ;
#26503 = DIRECTION ( 'NONE',  ( -1.000000000000000000, 0.000000000000000000, 0.000000000000000000 ) ) ;
#26504 = CARTESIAN_POINT ( 'NONE',  ( 35.00000000000000000, -4.824807283154205706, -11.80185301892979055 ) ) ;
#26505 = B_SPLINE_CURVE_WITH_KNOTS ( 'NONE', 3,
 ( #17543, #12518, #21878, #32798, #7897, #38465, #7544, #2598, #38123, #28172, #48465, #6587, #43437 ),
 .UNSPECIFIED., .F., .F.,
 ( 4, 3, 3, 3, 4 ),
 ( 1.734723475976807094E-18, 6.607593386745461920E-05, 0.0001321518677373516206, 0.0001982171734706201550, 0.0002642860854759486629 ),
 .UNSPECIFIED. ) ;
#26506 = LINE ( 'NONE', #26193, #31896 ) ;
#26507 = ADVANCED_FACE ( 'NONE', ( #53486 ), #28201, .T. ) ;
#26508 = ORIENTED_EDGE ( 'NONE', *, *, #20813, .T. ) ;
#26509 = ORIENTED_EDGE ( 'NONE', *, *, #57969, .T. ) ;
#26510 = CARTESIAN_POINT ( 'NONE',  ( -37.00000000000000711, 0.000000000000000000, 0.000000000000000000 ) ) ;
#26511 = EDGE_CURVE ( 'NONE', #7359, #20437, #18053, .T. ) ;
#26512 = ORIENTED_EDGE ( 'NONE', *, *, #11976, .T. ) ;
#26513 = CARTESIAN_POINT ( 'NONE',  ( 12.93723047338301058, 4.476360154859203355, 25.00000000000000000 ) ) ;
#26514 = CARTESIAN_POINT ( 'NONE',  ( -14.74485252626585741, 7.912425174792709015, -10.93822032635975994 ) ) ;
#26515 = EDGE_CURVE ( 'NONE', #16301, #41303, #1944, .T. ) ;
#26516 = CARTESIAN_POINT ( 'NONE',  ( 2.245754705088401693, 4.822435078157734090, 5.920355780195118101 ) ) ;
#26517 = DIRECTION ( 'NONE',  ( 0.000000000000000000, 0.9246979985058709772, 0.3807014730195252272 ) ) ;
#26518 = ORIENTED_EDGE ( 'NONE', *, *, #8039, .F. ) ;
#26519 = DIRECTION ( 'NONE',  ( 0.000000000000000000, 0.000000000000000000, 1.000000000000000000 ) ) ;
#26520 = DIRECTION ( 'NONE',  ( 1.000000000000000000, 0.000000000000000000, 0.000000000000000000 ) ) ;
#26521 = CARTESIAN_POINT ( 'NONE',  ( 1.633930747250948112, -1.494486044209850428, 12.61425129500116604 ) ) ;
#26522 = DIRECTION ( 'NONE',  ( 0.000000000000000000, 0.1387779952735818945, -0.9903235168508549569 ) ) ;
#26523 = AXIS2_PLACEMENT_3D ( 'NONE', #58948, #3080, #18026 ) ;
#26524 = DIRECTION ( 'NONE',  ( -1.000000000000000000, 0.000000000000000000, -0.000000000000000000 ) ) ;
#26525 = LINE ( 'NONE', #1279, #2176 ) ;
#26526 = ORIENTED_EDGE ( 'NONE', *, *, #35088, .T. ) ;
#26527 = AXIS2_PLACEMENT_3D ( 'NONE', #53269, #26680, #2411 ) ;
#26528 = DIRECTION ( 'NONE',  ( -1.000000000000000000, 0.000000000000000000, 0.000000000000000000 ) ) ;
#26529 = ORIENTED_EDGE ( 'NONE', *, *, #51797, .T. ) ;
#26530 = CARTESIAN_POINT ( 'NONE',  ( 0.2648978790185584908, 10.53870023327863770, 6.237101853238585569 ) ) ;
#26531 = CARTESIAN_POINT ( 'NONE',  ( -35.00000000000000000, 12.21925492305362049, 3.640372113593593806 ) ) ;
#26532 = DIRECTION ( 'NONE',  ( -1.000000000000000000, 0.000000000000000000, 0.000000000000000000 ) ) ;
#26533 = LINE ( 'NONE', #31522, #4191 ) ;
#26534 = DIRECTION ( 'NONE',  ( 1.000000000000000000, 0.000000000000000000, 0.000000000000000000 ) ) ;
#26535 = AXIS2_PLACEMENT_3D ( 'NONE', #23207, #47502, #47821 ) ;
#26536 = EDGE_CURVE ( 'NONE', #46522, #61135, #24446, .T. ) ;
#26537 = ADVANCED_FACE ( 'NONE', ( #58813 ), #33210, .F. ) ;
#26538 = VERTEX_POINT ( 'NONE', #8239 ) ;
#26539 = ORIENTED_EDGE ( 'NONE', *, *, #9452, .T. ) ;
#26540 = CARTESIAN_POINT ( 'NONE',  ( -30.18541646480307250, -1.190103380016452217, 11.94300686747243745 ) ) ;
#26541 = EDGE_LOOP ( 'NONE', ( #47503, #44418, #24958, #3836 ) ) ;
#26542 = DIRECTION ( 'NONE',  ( 0.000000000000000000, -0.01356324068817991828, 0.9999080150203990547 ) ) ;
#26543 = DIRECTION ( 'NONE',  ( 0.000000000000000000, 0.000000000000000000, 1.000000000000000000 ) ) ;
#26544 = CARTESIAN_POINT ( 'NONE',  ( 35.00000000000000000, 10.39746860227901060, 7.379373053628749624 ) ) ;
#26545 = LINE ( 'NONE', #51526, #31120 ) ;
#26546 = CARTESIAN_POINT ( 'NONE',  ( 2.969415267402681025, 7.867532449842534525, -0.3878973768010711698 ) ) ;
#26547 = CARTESIAN_POINT ( 'NONE',  ( 35.00000000000000000, -12.42372387097884179, -2.865935305911583519 ) ) ;
#26548 = CARTESIAN_POINT ( 'NONE',  ( -35.00000000000000000, 0.000000000000000000, 0.000000000000000000 ) ) ;
#26549 = ORIENTED_EDGE ( 'NONE', *, *, #13151, .T. ) ;
#26550 = ADVANCED_FACE ( 'NONE', ( #22561 ), #27870, .T. ) ;
#26551 = DIRECTION ( 'NONE',  ( 1.000000000000000000, 0.000000000000000000, 0.000000000000000000 ) ) ;
#26552 = CIRCLE ( 'NONE', #37131, 4.999999999999999112 ) ;
#26553 = VERTEX_POINT ( 'NONE', #7241 ) ;
#26554 = DIRECTION ( 'NONE',  ( 0.000000000000000000, -0.01356324068817998940, 0.9999080150203990547 ) ) ;
#26555 = B_SPLINE_CURVE_WITH_KNOTS ( 'NONE', 3,
 ( #42617, #38643, #53941, #37659, #53286, #57957, #2427, #12050, #27340, #22704, #32328, #7067, #13364, #8381, #42967, #23028, #17385, #17714, #33651, #47325, #47634, #53628 ),
 .UNSPECIFIED., .F., .F.,
 ( 4, 3, 3, 3, 3, 3, 3, 4 ),
 ( 1.371419323662817635E-18, 4.455945684386977945E-05, 6.636307477204154645E-05, 8.816671873159025760E-05, 0.0001099660380492627801, 0.0001317545563165332175, 0.0001762613022895079989, 0.0001867992666138373426 ),
 .UNSPECIFIED. ) ;
#26556 = CARTESIAN_POINT ( 'NONE',  ( 0.5572780756291629833, 8.165890079445782490, -9.256402261579136592 ) ) ;
#26557 = EDGE_CURVE ( 'NONE', #34540, #39315, #12411, .T. ) ;
#26558 = ORIENTED_EDGE ( 'NONE', *, *, #36975, .T. ) ;
#26559 = CARTESIAN_POINT ( 'NONE',  ( -27.10719052120871098, 1.714424047991082389, 1.622102031466668093 ) ) ;
#26560 = ORIENTED_EDGE ( 'NONE', *, *, #22552, .F. ) ;
#26561 = DIRECTION ( 'NONE',  ( 1.000000000000000000, 0.000000000000000000, 0.000000000000000000 ) ) ;
#26562 = CARTESIAN_POINT ( 'NONE',  ( -22.49803948133827092, 2.073427785788399813, -3.817825231362854677 ) ) ;
#26563 = CARTESIAN_POINT ( 'NONE',  ( 2.589278595513498704, 2.875840518181537409, 7.197074516942346456 ) ) ;
#26564 = ORIENTED_EDGE ( 'NONE', *, *, #40860, .T. ) ;
#26565 = ORIENTED_EDGE ( 'NONE', *, *, #55697, .F. ) ;
#26566 = CARTESIAN_POINT ( 'NONE',  ( 3.489268527502659811, 6.893366482496841918, 11.63752349626312288 ) ) ;
#26567 = EDGE_CURVE ( 'NONE', #39182, #5675, #63692, .T. ) ;
#26568 = ORIENTED_EDGE ( 'NONE', *, *, #50566, .T. ) ;
#26569 = LINE ( 'NONE', #11286, #23132 ) ;
#26570 = ORIENTED_EDGE ( 'NONE', *, *, #30968, .F. ) ;
#26571 = VERTEX_POINT ( 'NONE', #62773 ) ;
#26572 = ORIENTED_EDGE ( 'NONE', *, *, #60296, .F. ) ;
#26573 = CARTESIAN_POINT ( 'NONE',  ( -22.27721688985630522, -2.843753050855867937, 2.338410344701243648 ) ) ;
#26574 = CARTESIAN_POINT ( 'NONE',  ( 2.262775599885885391, 5.019217486250719062, -5.761998514039260222 ) ) ;
#26576 = CIRCLE ( 'NONE', #48903, 2.899999999999994582 ) ;
#26575 = CARTESIAN_POINT ( 'NONE',  ( 0.2646305136544072623, -4.064188116014627816, 11.55263159009957441 ) ) ;
#26577 = CARTESIAN_POINT ( 'NONE',  ( 1.452237505248552996, 5.807998527925892773, 11.24427360515644203 ) ) ;
#26578 = DIRECTION ( 'NONE',  ( 0.000000000000000000, 0.5987040770935676548, -0.8009703041134167423 ) ) ;
#26579 = AXIS2_PLACEMENT_3D ( 'NONE', #18644, #59506, #13934 ) ;
#26580 = VERTEX_POINT ( 'NONE', #48179 ) ;
#26581 = CARTESIAN_POINT ( 'NONE',  ( 0.000000000000000000, 0.000000000000000000, 0.000000000000000000 ) ) ;
#26582 = ORIENTED_EDGE ( 'NONE', *, *, #36510, .T. ) ;
#26583 = B_SPLINE_CURVE_WITH_KNOTS ( 'NONE', 3,
 ( #37167, #22554, #41495, #57476, #12544, #61791, #56836, #51833, #6281, #11901, #52500, #6933, #27203, #47495, #62766, #48170 ),
 .UNSPECIFIED., .F., .F.,
 ( 4, 3, 3, 3, 3, 4 ),
 ( 6.079513230985732741E-18, 6.991367980366406450E-05, 0.0001398269368981362064, 0.0002097400188389093899, 0.0002811534801551362692, 0.0003526297678872492036 ),
 .UNSPECIFIED. ) ;
#26584 = EDGE_CURVE ( 'NONE', #4143, #39990, #30790, .T. ) ;
#26585 = CARTESIAN_POINT ( 'NONE',  ( -35.00000000000000000, -10.49591321039677005, -5.273331777780449592 ) ) ;
#26586 = CARTESIAN_POINT ( 'NONE',  ( 0.2652384770603652409, 0.06606665821615019529, -12.24598129987882444 ) ) ;
#26587 = ADVANCED_FACE ( 'NONE', ( #38828 ), #57820, .T. ) ;
#26588 = CARTESIAN_POINT ( 'NONE',  ( 0.2911222467163550598, -2.338869407810943990, 12.02952766044174382 ) ) ;
#26589 = CARTESIAN_POINT ( 'NONE',  ( 35.00000000000000000, 5.130401251914885385, 11.05394794832823813 ) ) ;
#26590 = DIRECTION ( 'NONE',  ( -1.000000000000000000, -1.836970198721029688E-16, 0.000000000000000000 ) ) ;
#26591 = ADVANCED_FACE ( 'NONE', ( #59128 ), #12241, .T. ) ;
#26592 = ORIENTED_EDGE ( 'NONE', *, *, #44339, .T. ) ;
#26593 = CARTESIAN_POINT ( 'NONE',  ( 5.514970785353741078, -0.004324946436530173639, -0.001897634820904526036 ) ) ;
#26594 = EDGE_CURVE ( 'NONE', #25848, #45204, #7446, .T. ) ;
#26595 =( BOUNDED_CURVE ( )  B_SPLINE_CURVE ( 3, ( #47171, #21889, #62421, #52489 ),
 .UNSPECIFIED., .F., .F. ) 
 B_SPLINE_CURVE_WITH_KNOTS ( ( 4, 4 ),
 ( 0.9133032884833093279, 0.9519776552476308940 ),
 .UNSPECIFIED. ) 
 CURVE ( )  GEOMETRIC_REPRESENTATION_ITEM ( )  RATIONAL_B_SPLINE_CURVE ( ( 1.000000000000000000, 0.9998753616634872277, 0.9998753616634872277, 1.000000000000000000 ) ) 
 REPRESENTATION_ITEM ( '' )  );
#26596 = ORIENTED_EDGE ( 'NONE', *, *, #41275, .F. ) ;
#26597 = DIRECTION ( 'NONE',  ( 0.000000000000000000, -0.01356324068817998940, 0.9999080150203990547 ) ) ;
#26598 = CARTESIAN_POINT ( 'NONE',  ( -14.48921874744988614, -27.84739049628998231, -11.52341872854555405 ) ) ;
#26599 = CARTESIAN_POINT ( 'NONE',  ( 16.79789036561813020, -29.41979974037718648, 9.796743230926852064 ) ) ;
#26600 = ADVANCED_FACE ( 'NONE', ( #20172 ), #55427, .F. ) ;
#26601 = CARTESIAN_POINT ( 'NONE',  ( -27.10719052120871098, -0.6736837626858844796, -2.261993590776034235 ) ) ;
#26602 = FACE_OUTER_BOUND ( 'NONE', #24401, .T. ) ;
#26603 = VERTEX_POINT ( 'NONE', #50120 ) ;
#26604 = DIRECTION ( 'NONE',  ( -1.000000000000000000, -0.000000000000000000, -0.000000000000000000 ) ) ;
#26606 = VECTOR ( 'NONE', #65260, 1000.000000000000000 ) ;
#26605 = CARTESIAN_POINT ( 'NONE',  ( 0.2956976708475440585, 2.344604179391573062, -12.02996380804951748 ) ) ;
#26607 = CYLINDRICAL_SURFACE ( 'NONE', #53470, 6.936499999999988120 ) ;
#26608 = DIRECTION ( 'NONE',  ( -1.000000000000000000, 0.000000000000000000, 0.000000000000000000 ) ) ;
#26609 = AXIS2_PLACEMENT_3D ( 'NONE', #14840, #41106, #29821 ) ;
#26610 = CARTESIAN_POINT ( 'NONE',  ( -20.92021774235402276, 12.94977746786777395, -3.816457577290518266 ) ) ;
#26611 = CARTESIAN_POINT ( 'NONE',  ( 1.000000000000000888, 3.073484823194434057, -6.841322316745026555 ) ) ;
#26612 = CIRCLE ( 'NONE', #51070, 12.18649999999999878 ) ;
#26613 = CARTESIAN_POINT ( 'NONE',  ( 1.109979610371588210, -5.843815872356387331, -11.08130463534545385 ) ) ;
#26614 = LINE ( 'NONE', #58114, #11011 ) ;
#26615 = CARTESIAN_POINT ( 'NONE',  ( 35.00000000000000000, -1.456211999474423369, -11.65554240571057143 ) ) ;
#26616 = AXIS2_PLACEMENT_3D ( 'NONE', #28910, #9576, #35178 ) ;
#26617 = EDGE_CURVE ( 'NONE', #44861, #2869, #55341, .T. ) ;
#26618 = CIRCLE ( 'NONE', #16026, 5.000000000000000000 ) ;
#26619 = CIRCLE ( 'NONE', #48955, 3.999999999999999556 ) ;
#26620 = ORIENTED_EDGE ( 'NONE', *, *, #25103, .T. ) ;
#26621 = ADVANCED_FACE ( 'NONE', ( #60742 ), #60089, .T. ) ;
#26622 = ORIENTED_EDGE ( 'NONE', *, *, #12940, .T. ) ;
#26623 = CARTESIAN_POINT ( 'NONE',  ( -22.31328051695926007, 3.633840107626944871, -1.076152733467184985 ) ) ;
#26624 = CARTESIAN_POINT ( 'NONE',  ( 45.77110135055801265, -0.8256172497425009471, -12.04909734191306114 ) ) ;
#26625 = DIRECTION ( 'NONE',  ( 1.000000000000000000, 0.000000000000000000, 0.000000000000000000 ) ) ;
#26626 = DIRECTION ( 'NONE',  ( -1.000000000000000000, -0.000000000000000000, -0.000000000000000000 ) ) ;
#26627 = ORIENTED_EDGE ( 'NONE', *, *, #13093, .T. ) ;
#26628 = EDGE_CURVE ( 'NONE', #7491, #48365, #13802, .T. ) ;
#26629 = ORIENTED_EDGE ( 'NONE', *, *, #9171, .T. ) ;
#26630 = ORIENTED_EDGE ( 'NONE', *, *, #56639, .T. ) ;
#26631 = CARTESIAN_POINT ( 'NONE',  ( -35.00000000000000000, -1.771820996347237331, 11.61175578952785692 ) ) ;
#26632 = AXIS2_PLACEMENT_3D ( 'NONE', #64264, #34641, #65246 ) ;
#26633 = CARTESIAN_POINT ( 'NONE',  ( -27.05874794189610455, -0.3907329275428090276, -2.180117559290211116 ) ) ;
#26634 = ORIENTED_EDGE ( 'NONE', *, *, #15262, .F. ) ;
#26635 = LINE ( 'NONE', #46929, #758 ) ;
#26636 = CIRCLE ( 'NONE', #56353, 2.899999999999995026 ) ;
#26637 = AXIS2_PLACEMENT_3D ( 'NONE', #30980, #62223, #61556 ) ;
#26638 = DIRECTION ( 'NONE',  ( 1.000000000000000000, 0.000000000000000000, -0.000000000000000000 ) ) ;
#26639 = VERTEX_POINT ( 'NONE', #24178 ) ;
#26640 = CARTESIAN_POINT ( 'NONE',  ( 47.00000000000000711, 4.705694406421931860E-17, -3.469127814946512892E-15 ) ) ;
#26641 = CARTESIAN_POINT ( 'NONE',  ( 16.93571557946454931, -34.49999999976442666, -4.804977935186947491 ) ) ;
#26642 = CARTESIAN_POINT ( 'NONE',  ( 2.261269890823172979, 7.131324074141454084, 2.744033622444998155 ) ) ;
#26643 = ORIENTED_EDGE ( 'NONE', *, *, #24762, .F. ) ;
#26644 = AXIS2_PLACEMENT_3D ( 'NONE', #38912, #54206, #8649 ) ;
#26645 = CARTESIAN_POINT ( 'NONE',  ( 0.2759803524722246881, 12.09509972435083291, -1.940323823244534562 ) ) ;
#26646 = EDGE_CURVE ( 'NONE', #32268, #36353, #12760, .T. ) ;
#26647 = ORIENTED_EDGE ( 'NONE', *, *, #46386, .T. ) ;
#26648 = CARTESIAN_POINT ( 'NONE',  ( 35.00000000000000000, 6.657191900728455458, 9.677500615117825333 ) ) ;
#26649 = CYLINDRICAL_SURFACE ( 'NONE', #58514, 2.899999999999994582 ) ;
#26650 = ADVANCED_FACE ( 'NONE', ( #8895 ), #18878, .T. ) ;
#26651 = CARTESIAN_POINT ( 'NONE',  ( 37.00000000000000711, 4.705694406421931860E-17, -3.469127814946512892E-15 ) ) ;
#26652 = CARTESIAN_POINT ( 'NONE',  ( -14.47334165536099881, 5.400000000000000355, -1.000000000000000000 ) ) ;
#26653 = CARTESIAN_POINT ( 'NONE',  ( -35.00000000000000000, 7.238157050195777487, -10.49626516989263614 ) ) ;
#26654 = CARTESIAN_POINT ( 'NONE',  ( 8.437200413559441614, 4.476360154859203355, 11.13383131558893346 ) ) ;
#26655 = CARTESIAN_POINT ( 'NONE',  ( -27.32337605527166957, -2.404211887218375754, -1.812546145273364662 ) ) ;
#26656 = CARTESIAN_POINT ( 'NONE',  ( -28.66013792860432119, 0.1826938850344184129, 1.826836065344823457 ) ) ;
#26657 = VERTEX_POINT ( 'NONE', #23879 ) ;
#26658 = CARTESIAN_POINT ( 'NONE',  ( -35.05012975565874456, 0.004360246756751652575, -0.01323209221895734096 ) ) ;
#26659 = CIRCLE ( 'NONE', #53200, 7.499999999999988454 ) ;
#26660 = EDGE_LOOP ( 'NONE', ( #46389, #22055, #9497, #46924 ) ) ;
#26661 = DIRECTION ( 'NONE',  ( -1.000000000000000000, 0.000000000000000000, 0.000000000000000000 ) ) ;
#26662 = CARTESIAN_POINT ( 'NONE',  ( 2.931247277082689173, -5.779735553870066767, -5.333206743525307658 ) ) ;
#26663 = CIRCLE ( 'NONE', #11785, 4.999999999999998224 ) ;
#26664 = ORIENTED_EDGE ( 'NONE', *, *, #16291, .T. ) ;
#26665 = CARTESIAN_POINT ( 'NONE',  ( 2.969415267404787784, 7.525730903320808629, 2.326350273511627709 ) ) ;
#26666 = CARTESIAN_POINT ( 'NONE',  ( 1.937114397841935398, 10.38782037574616801, 7.538912286488381298 ) ) ;
#26667 = CARTESIAN_POINT ( 'NONE',  ( -35.00000000000000000, -8.699265615722922007, -8.534258022646191932 ) ) ;
#26668 = CARTESIAN_POINT ( 'NONE',  ( 37.00000000000000711, 4.705694406421931860E-17, -3.469127814946512892E-15 ) ) ;
#26669 = ADVANCED_FACE ( 'NONE', ( #44445 ), #40111, .T. ) ;
#26670 = ORIENTED_EDGE ( 'NONE', *, *, #51670, .T. ) ;
#26671 = CARTESIAN_POINT ( 'NONE',  ( -27.08423805673873375, 1.573803011992720435, 1.665498649074229842 ) ) ;
#26672 = AXIS2_PLACEMENT_3D ( 'NONE', #42365, #7144, #52717 ) ;
#26673 = VECTOR ( 'NONE', #56727, 1000.000000000000000 ) ;
#26674 = AXIS2_PLACEMENT_3D ( 'NONE', #48625, #38639, #48960 ) ;
#26675 = ORIENTED_EDGE ( 'NONE', *, *, #20799, .T. ) ;
#26676 = CARTESIAN_POINT ( 'NONE',  ( -19.47984447937493613, -3.750539801530005768, -11.39883551934754102 ) ) ;
#26677 = ADVANCED_FACE ( 'NONE', ( #39803 ), #55089, .T. ) ;
#26678 = AXIS2_PLACEMENT_3D ( 'NONE', #47125, #36475, #26488 ) ;
#26679 = ORIENTED_EDGE ( 'NONE', *, *, #52132, .F. ) ;
#26680 = DIRECTION ( 'NONE',  ( -1.000000000000000000, 0.000000000000000000, -0.000000000000000000 ) ) ;
#26681 = CYLINDRICAL_SURFACE ( 'NONE', #27085, 12.18649999999999878 ) ;
#26682 = EDGE_CURVE ( 'NONE', #22226, #64219, #49154, .T. ) ;
#26683 = CARTESIAN_POINT ( 'NONE',  ( -14.11589373245165469, 8.250315036047107142, 25.00000000000000000 ) ) ;
#26684 = ORIENTED_EDGE ( 'NONE', *, *, #63346, .F. ) ;
#26685 = B_SPLINE_CURVE_WITH_KNOTS ( 'NONE', 3,
 ( #14291, #44884, #25252, #50548, #56164, #24606, #19635, #9970, #10603, #39893, #4680, #45529, #65793, #24943, #40546, #45878 ),
 .UNSPECIFIED., .F., .F.,
 ( 4, 3, 3, 3, 3, 4 ),
 ( 2.328959703873127122E-15, 0.0002126834539179888047, 0.0004253519300366621859, 0.0006380165497224692985, 0.0007442707582428857976, 0.0009453531351414204203 ),
 .UNSPECIFIED. ) ;
#26686 = CIRCLE ( 'NONE', #6477, 12.74999999999999822 ) ;
#26687 = AXIS2_PLACEMENT_3D ( 'NONE', #54274, #28994, #22702 ) ;
#26688 = EDGE_CURVE ( 'NONE', #56983, #14040, #30304, .T. ) ;
#26689 = AXIS2_PLACEMENT_3D ( 'NONE', #25965, #50585, #35257 ) ;
#26690 = DIRECTION ( 'NONE',  ( -1.000000000000000000, 0.000000000000000000, 0.000000000000000000 ) ) ;
#26691 = CARTESIAN_POINT ( 'NONE',  ( 2.903928887688508098, 0.5297564406061431308, 8.753847148605441220 ) ) ;
#26692 = AXIS2_PLACEMENT_3D ( 'NONE', #63833, #12980, #48574 ) ;
#26693 = CARTESIAN_POINT ( 'NONE',  ( -35.00000000000000000, 8.624332853796195408, -9.390600770287898413 ) ) ;
#26694 = DIRECTION ( 'NONE',  ( 1.000000000000000000, 0.000000000000000000, 0.000000000000000000 ) ) ;
#26695 = CARTESIAN_POINT ( 'NONE',  ( 0.4613984246114870014, 4.475519447653987015, 11.46927345719238112 ) ) ;
#26696 = CARTESIAN_POINT ( 'NONE',  ( -35.00000000000000000, 1.463443770872774774, 12.09831040184924866 ) ) ;
#26697 = VECTOR ( 'NONE', #42417, 1000.000000000000000 ) ;
#26698 = EDGE_LOOP ( 'NONE', ( #54293, #35362, #34095, #50712 ) ) ;
#26699 = CARTESIAN_POINT ( 'NONE',  ( -14.47334165536099881, 0.000000000000000000, 0.000000000000000000 ) ) ;
#26700 = CARTESIAN_POINT ( 'NONE',  ( 35.00000000000000000, 12.46157735505189024, -2.696588552979104492 ) ) ;
#26701 = VECTOR ( 'NONE', #20927, 1000.000000000000114 ) ;
#26702 = EDGE_CURVE ( 'NONE', #47803, #4063, #65062, .T. ) ;
#26703 = ORIENTED_EDGE ( 'NONE', *, *, #40168, .T. ) ;
#26704 = CARTESIAN_POINT ( 'NONE',  ( 5.530133899448235191, 0.01589823604557701053, -0.001661287012794096735 ) ) ;
#26705 = CARTESIAN_POINT ( 'NONE',  ( 0.9296196016850856170, -9.278306863859519638, -8.327938962580805793 ) ) ;
#26706 = EDGE_LOOP ( 'NONE', ( #9250, #32520, #59922, #62870 ) ) ;
#26707 = AXIS2_PLACEMENT_3D ( 'NONE', #38986, #49333, #54304 ) ;
#26708 = AXIS2_PLACEMENT_3D ( 'NONE', #24586, #38310, #19614 ) ;
#26709 = LINE ( 'NONE', #1459, #33055 ) ;
#26710 = ORIENTED_EDGE ( 'NONE', *, *, #11402, .F. ) ;
#26711 = DIRECTION ( 'NONE',  ( -1.000000000000000000, 0.000000000000000000, 0.000000000000000000 ) ) ;
#26712 = ORIENTED_EDGE ( 'NONE', *, *, #28460, .F. ) ;
#26713 = ORIENTED_EDGE ( 'NONE', *, *, #15533, .T. ) ;
#26714 = AXIS2_PLACEMENT_3D ( 'NONE', #29546, #23943, #49226 ) ;
#26715 = DIRECTION ( 'NONE',  ( -0.3865475372811021937, 0.2971585806051969536, -0.8730852074079709091 ) ) ;
#26716 = AXIS2_PLACEMENT_3D ( 'NONE', #11360, #62231, #42250 ) ;
#26717 = B_SPLINE_CURVE_WITH_KNOTS ( 'NONE', 3,
 ( #1446, #53940, #58619, #8380, #53627, #64234, #18709, #3421, #33650, #12692, #13039, #23027, #13363, #28654, #9035, #24011, #63903, #8065, #14011, #33325, #48628, #29313 ),
 .UNSPECIFIED., .F., .F.,
 ( 4, 2, 2, 2, 2, 2, 2, 2, 2, 2, 4 ),
 ( 0.000000000000000000, 0.0006972416122780116313, 0.001394483224556023263, 0.002788966449112044790, 0.004183449673668066318, 0.004880691285946077949, 0.005577932898224087846, 0.006972416122780110241, 0.008366899347336134371, 0.009761382571892159368, 0.01115586579644818437 ),
 .UNSPECIFIED. ) ;
#26718 = AXIS2_PLACEMENT_3D ( 'NONE', #52789, #26209, #6265 ) ;
#26719 = ORIENTED_EDGE ( 'NONE', *, *, #61614, .F. ) ;
#26720 = CARTESIAN_POINT ( 'NONE',  ( -25.28055712087207496, -6.343239884292907860, 10.19231694478317785 ) ) ;
#26721 = CARTESIAN_POINT ( 'NONE',  ( -22.28284753389937478, -3.563226652211058720, 0.9912969289936491846 ) ) ;
#26722 = CARTESIAN_POINT ( 'NONE',  ( 35.00000000000000000, 0.6593684648220492495, -12.73293890771483738 ) ) ;
#26723 = CARTESIAN_POINT ( 'NONE',  ( 8.621148270653568702, 25.00000000000000000, -5.251012286260225537 ) ) ;
#26724 = ORIENTED_EDGE ( 'NONE', *, *, #2640, .F. ) ;
#26725 = DIRECTION ( 'NONE',  ( -0.000000000000000000, -1.000000000000000000, -0.000000000000000000 ) ) ;
#26726 = CARTESIAN_POINT ( 'NONE',  ( -2.112161198359963521, -25.77267402162640408, 15.59357793625674660 ) ) ;
#26727 = CARTESIAN_POINT ( 'NONE',  ( 2.969415267405027148, -7.867532449843256614, 0.3878973768021006241 ) ) ;
#26729 = VERTEX_POINT ( 'NONE', #16168 ) ;
#26728 = CARTESIAN_POINT ( 'NONE',  ( -25.19743177864295447, 5.013274974602487610, 10.93390578225709397 ) ) ;
#26730 = B_SPLINE_CURVE_WITH_KNOTS ( 'NONE', 3,
 ( #306, #10254, #10922, #30534, #46497, #50837, #5283, #46188, #25555, #48162, #23194, #53473, #2617, #42459, #23528, #53793, #7569, #22880, #32492 ),
 .UNSPECIFIED., .F., .F.,
 ( 4, 3, 3, 3, 3, 3, 4 ),
 ( 8.523235939525396438E-18, 4.457896483014807333E-05, 6.639290541542042386E-05, 8.820687556478697556E-05, 0.0001100173248778895513, 0.0001545671401658104489, 0.0001830328308068584413 ),
 .UNSPECIFIED. ) ;
#26731 = DIRECTION ( 'NONE',  ( -1.000000000000000000, 0.000000000000000000, 0.000000000000000000 ) ) ;
#26732 = EDGE_CURVE ( 'NONE', #40151, #743, #26466, .T. ) ;
#26733 = VERTEX_POINT ( 'NONE', #20509 ) ;
#26734 = CARTESIAN_POINT ( 'NONE',  ( 0.000000000000000000, 6.750946897830741200, -1.593658756657007514 ) ) ;
#26735 = ORIENTED_EDGE ( 'NONE', *, *, #49036, .F. ) ;
#26736 = FACE_OUTER_BOUND ( 'NONE', #20586, .T. ) ;
#26737 = VECTOR ( 'NONE', #22823, 1000.000000000000000 ) ;
#26738 = CARTESIAN_POINT ( 'NONE',  ( 2.241352910868909643, -4.970878533273721978, -5.794346703933896059 ) ) ;
#26739 = ADVANCED_FACE ( 'NONE', ( #30784 ), #61378, .T. ) ;
#26740 = CARTESIAN_POINT ( 'NONE',  ( 2.255723233588950549, -7.638048593862504454, -0.1321982600348033388 ) ) ;
#26741 = ORIENTED_EDGE ( 'NONE', *, *, #34192, .T. ) ;
#26742 = CARTESIAN_POINT ( 'NONE',  ( 35.00000000000000000, 4.705694406421931860E-17, -3.469127814946512892E-15 ) ) ;
#26743 = CARTESIAN_POINT ( 'NONE',  ( 0.2767916011545386579, -12.02950149294535187, 2.313848297676409427 ) ) ;
#26744 = VERTEX_POINT ( 'NONE', #35462 ) ;
#26745 = EDGE_LOOP ( 'NONE', ( #54769, #1227, #22853, #64110 ) ) ;
#26746 = CARTESIAN_POINT ( 'NONE',  ( 0.2648978790185584908, 12.03635331166812250, 2.256510822326184940 ) ) ;
#26747 = VERTEX_POINT ( 'NONE', #5218 ) ;
#26748 = AXIS2_PLACEMENT_3D ( 'NONE', #33434, #3186, #61633 ) ;
#26749 = ORIENTED_EDGE ( 'NONE', *, *, #44204, .F. ) ;
#26750 = CIRCLE ( 'NONE', #63905, 12.18650000000000233 ) ;
#26751 = DIRECTION ( 'NONE',  ( 1.000000000000000000, -0.000000000000000000, 0.000000000000000000 ) ) ;
#26752 = CARTESIAN_POINT ( 'NONE',  ( -28.66013792860432119, -0.4631296695479288905, -1.776574787184034498 ) ) ;
#26753 = CARTESIAN_POINT ( 'NONE',  ( 37.00000000000000711, 12.08151691381189963, -4.074242145636052470 ) ) ;
#26754 = CARTESIAN_POINT ( 'NONE',  ( -28.66013792860432119, 1.776574787184030946, -0.4631296695479306114 ) ) ;
#26755 = FACE_OUTER_BOUND ( 'NONE', #53636, .T. ) ;
#26756 = ADVANCED_FACE ( 'NONE', ( #62359 ), #60381, .F. ) ;
#26757 = CARTESIAN_POINT ( 'NONE',  ( 35.00000000000000000, 4.705694406421931860E-17, -3.469127814946512892E-15 ) ) ;
#26758 = DIRECTION ( 'NONE',  ( 0.9703875065674330003, 0.000000000000000000, 0.2415534870330798278 ) ) ;
#26759 = ORIENTED_EDGE ( 'NONE', *, *, #37561, .F. ) ;
#26760 = CARTESIAN_POINT ( 'NONE',  ( -22.28776923226071105, -3.061913732988072567, 2.100802264239994610 ) ) ;
#26761 = CARTESIAN_POINT ( 'NONE',  ( -4.045887249688725262, -9.479482157611457183, 7.361438422396102688 ) ) ;
#26762 = CIRCLE ( 'NONE', #28903, 2.899999999999995470 ) ;
#26763 = EDGE_CURVE ( 'NONE', #136, #43267, #21273, .T. ) ;
#26764 = CIRCLE ( 'NONE', #63922, 12.18649999999999878 ) ;
#26765 = CARTESIAN_POINT ( 'NONE',  ( 12.52750123246316072, 0.4973700281276248192, -11.98968819674306374 ) ) ;
#26766 = CIRCLE ( 'NONE', #43703, 2.899999999999995914 ) ;
#26767 = CARTESIAN_POINT ( 'NONE',  ( 2.241526690369557873, 3.802233103835260586, -6.620271521148390903 ) ) ;
#26768 = LINE ( 'NONE', #27099, #46846 ) ;
#26769 = CARTESIAN_POINT ( 'NONE',  ( 12.19544574952904803, 0.02891895647919810047, -11.99999999999999645 ) ) ;
#26770 = VERTEX_POINT ( 'NONE', #61711 ) ;
#26771 = CARTESIAN_POINT ( 'NONE',  ( -27.08417473062937120, 0.4370481938669439903, 2.249064769433617883 ) ) ;
#26772 = CARTESIAN_POINT ( 'NONE',  ( 0.2911222467163546712, -1.916522451062455668, -12.10399882413662276 ) ) ;
#26773 = CARTESIAN_POINT ( 'NONE',  ( 2.844750968616420295, 1.031816958530457740, -7.767336242081033681 ) ) ;
#26774 = CARTESIAN_POINT ( 'NONE',  ( 2.781367136452763678, -1.659348694504719335, -7.636197200465970170 ) ) ;
#26775 = VECTOR ( 'NONE', #25682, 1000.000000000000000 ) ;
#26776 = LINE ( 'NONE', #42364, #19272 ) ;
#26777 = CARTESIAN_POINT ( 'NONE',  ( -27.27855387000350262, -12.26939275170277632, 5.631341004100471892 ) ) ;
#26778 = EDGE_CURVE ( 'NONE', #62894, #9194, #51763, .T. ) ;
#26779 = ORIENTED_EDGE ( 'NONE', *, *, #49302, .F. ) ;
#26780 = DIRECTION ( 'NONE',  ( 1.000000000000000000, -0.000000000000000000, 0.000000000000000000 ) ) ;
#26781 = CARTESIAN_POINT ( 'NONE',  ( 29.03457606387295087, 25.00000000000000000, 10.97436308512422265 ) ) ;
#26782 = CIRCLE ( 'NONE', #63954, 20.19615242270663558 ) ;
#26783 = DIRECTION ( 'NONE',  ( -1.000000000000000000, 0.000000000000000000, -0.000000000000000000 ) ) ;
#26784 = ORIENTED_EDGE ( 'NONE', *, *, #38652, .F. ) ;
#26785 = EDGE_CURVE ( 'NONE', #28685, #7744, #18443, .T. ) ;
#26786 = CARTESIAN_POINT ( 'NONE',  ( -35.00000000000000000, 0.000000000000000000, 0.000000000000000000 ) ) ;
#26787 = FACE_OUTER_BOUND ( 'NONE', #45312, .T. ) ;
#26788 = CARTESIAN_POINT ( 'NONE',  ( 2.000000000000001776, -6.160607635185433750, 4.277489166005560506 ) ) ;
#26790 = ORIENTED_EDGE ( 'NONE', *, *, #36659, .T. ) ;
#26789 = CARTESIAN_POINT ( 'NONE',  ( 0.2653141334712576516, -12.24612529725264665, 0.04405251235376458907 ) ) ;
#26791 = DIRECTION ( 'NONE',  ( 1.000000000000000000, 1.685093406416449860E-16, -1.011030131491573426E-17 ) ) ;
#26792 = EDGE_CURVE ( 'NONE', #32084, #44729, #569, .T. ) ;
#26793 = DIRECTION ( 'NONE',  ( -1.000000000000000000, 0.000000000000000000, 0.000000000000000000 ) ) ;
#26794 = ORIENTED_EDGE ( 'NONE', *, *, #36296, .F. ) ;
#26795 = DIRECTION ( 'NONE',  ( 1.000000000000000000, -0.000000000000000000, -0.000000000000000000 ) ) ;
#26796 = CARTESIAN_POINT ( 'NONE',  ( 37.00000000000000711, 4.705694406421931860E-17, -3.469127814946512892E-15 ) ) ;
#26797 = CARTESIAN_POINT ( 'NONE',  ( 0.2653519991613825790, -7.888569541500585203, 9.366979519113323605 ) ) ;
#26798 = DIRECTION ( 'NONE',  ( 0.000000000000000000, 0.4935949184179261873, -0.8696919319575183716 ) ) ;
#26799 =( BOUNDED_SURFACE ( )  B_SPLINE_SURFACE ( 3, 1, ( 
 ( #44263, #34919 ),
 ( #55229, #64536 ),
 ( #19007, #39273 ),
 ( #59570, #14002 ) ),
 .UNSPECIFIED., .F., .F., .T. ) 
 B_SPLINE_SURFACE_WITH_KNOTS ( ( 4, 4 ),
 ( 2, 2 ),
 ( 0.000000000000000000, 1.000000000000000000 ),
 ( 0.000000000000000000, 1.000000000000000000 ),
 .UNSPECIFIED. ) 
 GEOMETRIC_REPRESENTATION_ITEM ( )  RATIONAL_B_SPLINE_SURFACE ( (
 ( 1.000000000000000000, 1.000000000000000000),
 ( 0.8716676215708681896, 0.8964445200148164483),
 ( 0.8716676215708681896, 0.8964445200148164483),
 ( 1.000000000000000000, 1.000000000000000000) ) ) 
 REPRESENTATION_ITEM ( '' )  SURFACE ( )  );
#26800 = CARTESIAN_POINT ( 'NONE',  ( -9.808575974122994978, 9.959513386048705286, -6.707583712996705749 ) ) ;
#26801 = DIRECTION ( 'NONE',  ( -1.000000000000000000, -0.000000000000000000, -0.000000000000000000 ) ) ;
#26803 = ORIENTED_EDGE ( 'NONE', *, *, #38318, .T. ) ;
#26802 = CARTESIAN_POINT ( 'NONE',  ( 5.514970785353741078, -0.004713149585127531307, 0.0003039746380528782601 ) ) ;
#26804 = EDGE_CURVE ( 'NONE', #14742, #11008, #15221, .T. ) ;
#26805 = ORIENTED_EDGE ( 'NONE', *, *, #57808, .F. ) ;
#26806 = CARTESIAN_POINT ( 'NONE',  ( 2.241451721903216399, -0.06083185034801423530, 7.634225434981129155 ) ) ;
#26808 = ORIENTED_EDGE ( 'NONE', *, *, #29801, .F. ) ;
#26807 = B_SPLINE_CURVE_WITH_KNOTS ( 'NONE', 3,
 ( #43885, #43215, #17961, #8003, #28267, #49545, #3985, #50196, #29250, #44515, #64479, #4652, #4306, #13609, #4968, #25230, #49229, #64170, #23947 ),
 .UNSPECIFIED., .F., .F.,
 ( 4, 3, 3, 3, 3, 3, 4 ),
 ( 0.000000000000000000, 2.832085443540605422E-05, 4.217789847394686647E-05, 5.603488375046026924E-05, 6.989180858579268122E-05, 9.821094829918735453E-05, 0.0001178165571465090750 ),
 .UNSPECIFIED. ) ;
#26809 = AXIS2_PLACEMENT_3D ( 'NONE', #20675, #5726, #25996 ) ;
#26810 = CARTESIAN_POINT ( 'NONE',  ( 0.7400311444011716810, -11.53023780418229904, 4.574267895796811700 ) ) ;
#26812 = CARTESIAN_POINT ( 'NONE',  ( -17.90332768477131609, 4.129650048207996527, 11.26888906344803587 ) ) ;
#26811 = AXIS2_PLACEMENT_3D ( 'NONE', #34058, #54372, #19447 ) ;
#26813 = CIRCLE ( 'NONE', #15073, 12.18650000000000233 ) ;
#26814 = DIRECTION ( 'NONE',  ( -1.000000000000000000, 0.000000000000000000, 0.000000000000000000 ) ) ;
#26815 = ORIENTED_EDGE ( 'NONE', *, *, #32256, .F. ) ;
#26816 = DIRECTION ( 'NONE',  ( -1.000000000000000000, 0.000000000000000000, -0.000000000000000000 ) ) ;
#26817 = DIRECTION ( 'NONE',  ( 0.000000000000000000, 0.000000000000000000, 1.000000000000000000 ) ) ;
#26818 = CARTESIAN_POINT ( 'NONE',  ( -22.27713295444592845, -1.050517974989007008, 3.528329525272660749 ) ) ;
#26819 = ORIENTED_EDGE ( 'NONE', *, *, #62677, .T. ) ;
#26820 = VERTEX_POINT ( 'NONE', #37094 ) ;
#26821 = CARTESIAN_POINT ( 'NONE',  ( 2.491965175174103653, 7.560994562509278261, -1.548529392253994441 ) ) ;
#26822 = ORIENTED_EDGE ( 'NONE', *, *, #58759, .F. ) ;
#26823 = DIRECTION ( 'NONE',  ( 0.000000000000000000, 0.000000000000000000, 1.000000000000000000 ) ) ;
#26824 = CARTESIAN_POINT ( 'NONE',  ( -22.59983133926798970, 4.058100437359467350, -2.272383229042361119 ) ) ;
#26825 = LINE ( 'NONE', #47126, #15061 ) ;
#26826 = CARTESIAN_POINT ( 'NONE',  ( 0.4613984246114869459, 12.17044190070617482, 1.858723191796512353 ) ) ;
#26827 = VECTOR ( 'NONE', #45507, 1000.000000000000000 ) ;
#26828 = CARTESIAN_POINT ( 'NONE',  ( 35.00000000000000000, -7.817610399097575602, -8.766823244861962294 ) ) ;
#26829 = CARTESIAN_POINT ( 'NONE',  ( 3.152665057734108878, -7.886634106564198277, 0.9030954876737806725 ) ) ;
#26830 = DIRECTION ( 'NONE',  ( 1.000000000000000000, 0.000000000000000000, -0.000000000000000000 ) ) ;
#26831 = VERTEX_POINT ( 'NONE', #57393 ) ;
#26832 = VECTOR ( 'NONE', #35935, 1000.000000000000000 ) ;
#26833 = DIRECTION ( 'NONE',  ( 0.000000000000000000, -0.01356324068817992175, 0.9999080150203990547 ) ) ;
#26834 = ORIENTED_EDGE ( 'NONE', *, *, #54520, .F. ) ;
#26835 = VECTOR ( 'NONE', #27544, 1000.000000000000000 ) ;
#26836 = CARTESIAN_POINT ( 'NONE',  ( 0.3675815128205894289, 0.2638082659428422350, 12.27743992903066328 ) ) ;
#26837 = CARTESIAN_POINT ( 'NONE',  ( 42.50000000000000000, -2.710505431213761085E-17, 1.399999999999999911 ) ) ;
#26838 = CARTESIAN_POINT ( 'NONE',  ( -9.340672490813821227, 10.24685145699743494, -6.257124625858472733 ) ) ;
#26839 = CARTESIAN_POINT ( 'NONE',  ( 2.258463476536645143, -3.937122681832530002, 6.547539277368021438 ) ) ;
#26840 = DIRECTION ( 'NONE',  ( 1.000000000000000000, 0.000000000000000000, 0.000000000000000000 ) ) ;
#26841 = DIRECTION ( 'NONE',  ( -1.000000000000000000, 0.000000000000000000, 0.000000000000000000 ) ) ;
#26842 = ORIENTED_EDGE ( 'NONE', *, *, #18122, .F. ) ;
#26843 = ADVANCED_FACE ( 'NONE', ( #22810 ), #48083, .T. ) ;
#26844 = VERTEX_POINT ( 'NONE', #48731 ) ;
#26845 = DIRECTION ( 'NONE',  ( 0.000000000000000000, -0.01356324068817999808, 0.9999080150203990547 ) ) ;
#26846 = VECTOR ( 'NONE', #32462, 1000.000000000000000 ) ;
#26847 = EDGE_LOOP ( 'NONE', ( #16273, #53161, #61074, #40563 ) ) ;
#26848 = CARTESIAN_POINT ( 'NONE',  ( -35.00000000000000000, -11.13736569743278082, 4.946702696913133579 ) ) ;
#26849 = CARTESIAN_POINT ( 'NONE',  ( 5.514624014163232779, 0.0008859786816846886709, 0.004045310349816156822 ) ) ;
#26850 = CARTESIAN_POINT ( 'NONE',  ( 2.305787727787083519, 4.792270232040894307, 5.970480882365237996 ) ) ;
#26851 = CARTESIAN_POINT ( 'NONE',  ( 2.268878695253352173, 1.472930498387372777, -7.500319319173564203 ) ) ;
#26852 = EDGE_LOOP ( 'NONE', ( #5607, #3040, #31290, #15422 ) ) ;
#26853 = CIRCLE ( 'NONE', #47043, 12.18650000000000233 ) ;
#26854 = FACE_OUTER_BOUND ( 'NONE', #61691, .T. ) ;
#26855 = CARTESIAN_POINT ( 'NONE',  ( 2.241534463349552198, -1.511811348926356884E-18, -7.634462073473343935 ) ) ;
#26856 = DIRECTION ( 'NONE',  ( 0.000000000000000000, -0.01356324068817998940, 0.9999080150203990547 ) ) ;
#26857 = CARTESIAN_POINT ( 'NONE',  ( -49.02672294760359506, -0.1966872720628178584, 6.919866740913558800 ) ) ;
#26858 = AXIS2_PLACEMENT_3D ( 'NONE', #52137, #56816, #1272 ) ;
#26859 = CIRCLE ( 'NONE', #56581, 5.000000000000000888 ) ;
#26860 = EDGE_CURVE ( 'NONE', #50602, #12850, #53125, .T. ) ;
#26861 = CARTESIAN_POINT ( 'NONE',  ( -35.00000000000000000, -11.65150730582933392, -1.488153103997089888 ) ) ;
#26862 = CARTESIAN_POINT ( 'NONE',  ( 2.305787727787084407, -7.654065630109508689, 0.1666591538752418555 ) ) ;
#26863 = ORIENTED_EDGE ( 'NONE', *, *, #39540, .T. ) ;
#26864 = EDGE_CURVE ( 'NONE', #31963, #2241, #47741, .T. ) ;
#26865 = AXIS2_PLACEMENT_3D ( 'NONE', #759, #22012, #11695 ) ;
#26866 = DIRECTION ( 'NONE',  ( 1.000000000000000000, 0.000000000000000000, 0.000000000000000000 ) ) ;
#26867 = ORIENTED_EDGE ( 'NONE', *, *, #61393, .T. ) ;
#26868 = EDGE_CURVE ( 'NONE', #11644, #63443, #32932, .T. ) ;
#26869 = CARTESIAN_POINT ( 'NONE',  ( -25.54417658651491863, -4.240019242199836391, 11.22596262356930197 ) ) ;
#26870 = DIRECTION ( 'NONE',  ( 1.000000000000000000, 0.000000000000000000, 0.000000000000000000 ) ) ;
#26871 = DIRECTION ( 'NONE',  ( 0.000000000000000000, 0.01356324068817991828, -0.9999080150203990547 ) ) ;
#26872 = CIRCLE ( 'NONE', #64033, 2.899999999999995470 ) ;
#26873 = DIRECTION ( 'NONE',  ( -1.000000000000000000, 0.000000000000000000, 0.000000000000000000 ) ) ;
#26874 = CIRCLE ( 'NONE', #64039, 7.499999999999988454 ) ;
#26875 = ORIENTED_EDGE ( 'NONE', *, *, #15162, .F. ) ;
#26877 = ORIENTED_EDGE ( 'NONE', *, *, #26628, .F. ) ;
#26876 = EDGE_CURVE ( 'NONE', #37186, #54640, #43728, .T. ) ;
#26878 = CARTESIAN_POINT ( 'NONE',  ( 0.3401186441510242742, 1.878666403202333246, 12.12646044229290254 ) ) ;
#26879 = ORIENTED_EDGE ( 'NONE', *, *, #38104, .F. ) ;
#26880 = CARTESIAN_POINT ( 'NONE',  ( 3.355386238882536620, 7.941827888624184872, 9.005989223246164244 ) ) ;
#26881 = CARTESIAN_POINT ( 'NONE',  ( 2.700868940011170949, 3.106162501881789773, -13.16183552361884779 ) ) ;
#26882 = CARTESIAN_POINT ( 'NONE',  ( 22.21053567399755835, -13.47268488964859046, -0.8606552803710496580 ) ) ;
#26883 = CARTESIAN_POINT ( 'NONE',  ( -37.00000000000000711, 0.000000000000000000, 0.000000000000000000 ) ) ;
#26884 = CARTESIAN_POINT ( 'NONE',  ( 2.305787727787084407, 7.654065630109506913, -0.1666591538752953128 ) ) ;
#26885 = ADVANCED_FACE ( 'NONE', ( #37425 ), #47430, .T. ) ;
#26886 = AXIS2_PLACEMENT_3D ( 'NONE', #55630, #35648, #46305 ) ;
#26887 = CARTESIAN_POINT ( 'NONE',  ( 2.305787727787085295, 5.756228004061457959, 5.047606869483074910 ) ) ;
#26888 = CARTESIAN_POINT ( 'NONE',  ( -11.14943813774385539, -5.657473984827134039, 10.59121631773951222 ) ) ;
#26889 = ORIENTED_EDGE ( 'NONE', *, *, #25139, .F. ) ;
#26890 = CARTESIAN_POINT ( 'NONE',  ( 0.4613984246114883891, -5.909164750631109797, 10.80075367333620662 ) ) ;
#26891 = ORIENTED_EDGE ( 'NONE', *, *, #15545, .T. ) ;
#26892 = DIRECTION ( 'NONE',  ( 1.000000000000000000, 0.000000000000000000, 0.000000000000000000 ) ) ;
#26893 = CARTESIAN_POINT ( 'NONE',  ( 22.02145101462502197, -12.24345070192289775, -5.700244587874106372 ) ) ;
#26894 = CARTESIAN_POINT ( 'NONE',  ( 0.9296196016855220456, 8.327938962581047377, -9.278306863859516085 ) ) ;
#26895 = AXIS2_PLACEMENT_3D ( 'NONE', #49750, #59730, #55730 ) ;
#26896 = EDGE_CURVE ( 'NONE', #58655, #37233, #39297, .T. ) ;
#26897 = CARTESIAN_POINT ( 'NONE',  ( 2.000000000000001776, 4.915517050588409376, 4.717154614762108622 ) ) ;
#26898 = ORIENTED_EDGE ( 'NONE', *, *, #13488, .F. ) ;
#26899 = DIRECTION ( 'NONE',  ( 0.000000000000000000, 0.000000000000000000, 1.000000000000000000 ) ) ;
#26900 = CARTESIAN_POINT ( 'NONE',  ( 2.305787727787083519, 6.545285700970583598, -3.971363876083895850 ) ) ;
#26901 = DIRECTION ( 'NONE',  ( 1.000000000000000000, 0.000000000000000000, 0.000000000000000000 ) ) ;
#26902 = ORIENTED_EDGE ( 'NONE', *, *, #46756, .F. ) ;
#26904 = EDGE_CURVE ( 'NONE', #31041, #3171, #7845, .T. ) ;
#26903 = ORIENTED_EDGE ( 'NONE', *, *, #26365, .T. ) ;
#26905 = CARTESIAN_POINT ( 'NONE',  ( 35.00000000000000000, 9.821084925794670184, 7.215058775251142364 ) ) ;
#26906 = ORIENTED_EDGE ( 'NONE', *, *, #26985, .T. ) ;
#26907 = VERTEX_POINT ( 'NONE', #62685 ) ;
#26908 = CIRCLE ( 'NONE', #43893, 12.18649999999999878 ) ;
#26909 = CIRCLE ( 'NONE', #57721, 12.74999999999999822 ) ;
#26910 = ORIENTED_EDGE ( 'NONE', *, *, #21503, .F. ) ;
#26911 = VERTEX_POINT ( 'NONE', #43066 ) ;
#26912 = CARTESIAN_POINT ( 'NONE',  ( 0.3057689695767474847, 4.409323295154205624, 11.43929056598607374 ) ) ;
#26913 = DIRECTION ( 'NONE',  ( 0.000000000000000000, 0.01356324068817992175, -0.9999080150203990547 ) ) ;
#26914 = AXIS2_PLACEMENT_3D ( 'NONE', #1447, #51336, #6422 ) ;
#26915 = CIRCLE ( 'NONE', #64066, 12.18650000000000055 ) ;
#26916 = CARTESIAN_POINT ( 'NONE',  ( -19.61329546411680624, -11.94675665305282841, -1.284421273215466508 ) ) ;
#26917 = CARTESIAN_POINT ( 'NONE',  ( -25.00000000000000355, -9.999999999999998224, -5.000000000000000888 ) ) ;
#26918 = CARTESIAN_POINT ( 'NONE',  ( 36.00000000000000711, 9.913596905230228629, 8.017674001891673896 ) ) ;
#26919 = VERTEX_POINT ( 'NONE', #17153 ) ;
#26920 = LINE ( 'NONE', #42183, #29025 ) ;
#26921 = ORIENTED_EDGE ( 'NONE', *, *, #57887, .F. ) ;
#26922 = FACE_OUTER_BOUND ( 'NONE', #43189, .T. ) ;
#26924 = FACE_OUTER_BOUND ( 'NONE', #41953, .T. ) ;
#26923 = AXIS2_PLACEMENT_3D ( 'NONE', #6578, #57438, #31811 ) ;
#26925 = CARTESIAN_POINT ( 'NONE',  ( 2.242418902652060453, 3.730710532462696349, -6.661183998168035636 ) ) ;
#26926 = CARTESIAN_POINT ( 'NONE',  ( 37.00000000000000711, -8.496612874013091954, 9.506317355798454827 ) ) ;
#26927 = DIRECTION ( 'NONE',  ( 0.000000000000000000, 0.01356324068817992175, -0.9999080150203990547 ) ) ;
#26928 = DIRECTION ( 'NONE',  ( 0.000000000000000000, -0.01356324068817991828, 0.9999080150203990547 ) ) ;
#26929 = CIRCLE ( 'NONE', #12052, 2.899999999999994582 ) ;
#26930 = EDGE_CURVE ( 'NONE', #48396, #50472, #28429, .T. ) ;
#26931 = VERTEX_POINT ( 'NONE', #12158 ) ;
#26932 = CARTESIAN_POINT ( 'NONE',  ( 0.000000000000000000, -5.997115278587591192, -3.485633455389576696 ) ) ;
#26933 = AXIS2_PLACEMENT_3D ( 'NONE', #26388, #11419, #16080 ) ;
#26934 = ORIENTED_EDGE ( 'NONE', *, *, #59826, .F. ) ;
#26935 = LINE ( 'NONE', #1012, #49793 ) ;
#26936 = CARTESIAN_POINT ( 'NONE',  ( 15.64771680208055749, -28.15000396670248151, -10.66347899870799942 ) ) ;
#26937 = FACE_OUTER_BOUND ( 'NONE', #28140, .T. ) ;
#26938 = DIRECTION ( 'NONE',  ( -0.000000000000000000, -1.000000000000000000, -0.000000000000000000 ) ) ;
#26939 = CARTESIAN_POINT ( 'NONE',  ( 2.781367136451477151, 7.743208838465175603, 1.052455537429972221 ) ) ;
#26940 = ORIENTED_EDGE ( 'NONE', *, *, #56271, .F. ) ;
#26941 = EDGE_CURVE ( 'NONE', #63262, #16803, #1372, .T. ) ;
#26942 = FACE_OUTER_BOUND ( 'NONE', #7046, .T. ) ;
#26943 = CARTESIAN_POINT ( 'NONE',  ( 0.3675815128205894289, 2.391755495700764289, -12.04510820461657161 ) ) ;
#26944 = CARTESIAN_POINT ( 'NONE',  ( 1.948354844646954964, 2.783443994771086505, 11.63671644762409763 ) ) ;
#26945 = DIRECTION ( 'NONE',  ( 0.000000000000000000, 0.9551603052523489623, -0.2960891610144475439 ) ) ;
#26946 = VECTOR ( 'NONE', #49249, 999.9999999999997726 ) ;
#26947 = EDGE_CURVE ( 'NONE', #1614, #57966, #63343, .T. ) ;
#26948 = DIRECTION ( 'NONE',  ( 0.000000000000000000, -0.01356324068817998940, 0.9999080150203990547 ) ) ;
#26949 = ORIENTED_EDGE ( 'NONE', *, *, #32115, .F. ) ;
#26950 = CARTESIAN_POINT ( 'NONE',  ( 2.000000000000001776, -4.915517050588371184, -4.717154614762162801 ) ) ;
#26951 = ADVANCED_FACE ( 'NONE', ( #38074 ), #27443, .T. ) ;
#26952 = PLANE ( 'NONE',  #14986 ) ;
#26953 = VECTOR ( 'NONE', #58809, 1000.000000000000000 ) ;
#26954 = AXIS2_PLACEMENT_3D ( 'NONE', #49805, #64114, #18595 ) ;
#26955 = CIRCLE ( 'NONE', #43955, 4.999999999999999112 ) ;
#26956 = ORIENTED_EDGE ( 'NONE', *, *, #34591, .T. ) ;
#26957 = ORIENTED_EDGE ( 'NONE', *, *, #47772, .T. ) ;
#26959 = AXIS2_PLACEMENT_3D ( 'NONE', #47078, #52057, #52396 ) ;
#26958 = CARTESIAN_POINT ( 'NONE',  ( 0.2648978790185619880, 2.256510822326142751, 12.03635331166812783 ) ) ;
#26960 = CYLINDRICAL_SURFACE ( 'NONE', #5665, 1.500000000000000444 ) ;
#26961 = LINE ( 'NONE', #21969, #11991 ) ;
#26962 = EDGE_CURVE ( 'NONE', #20989, #815, #57400, .T. ) ;
#26963 = CIRCLE ( 'NONE', #26923, 2.899999999999996803 ) ;
#26964 = CYLINDRICAL_SURFACE ( 'NONE', #2096, 12.74999999999999822 ) ;
#26965 = ORIENTED_EDGE ( 'NONE', *, *, #28261, .T. ) ;
#26966 = EDGE_CURVE ( 'NONE', #21913, #36610, #28120, .T. ) ;
#26967 = AXIS2_PLACEMENT_3D ( 'NONE', #41072, #36750, #40412 ) ;
#26968 = ORIENTED_EDGE ( 'NONE', *, *, #55702, .F. ) ;
#26969 = VERTEX_POINT ( 'NONE', #45045 ) ;
#26970 = DIRECTION ( 'NONE',  ( 1.000000000000000000, 0.000000000000000000, -0.000000000000000000 ) ) ;
#26971 = ADVANCED_FACE ( 'NONE', ( #64008 ), #33740, .T. ) ;
#26972 = CIRCLE ( 'NONE', #56753, 12.18649999999999878 ) ;
#26973 = DIRECTION ( 'NONE',  ( -0.000000000000000000, -0.000000000000000000, -1.000000000000000000 ) ) ;
#26974 = VERTEX_POINT ( 'NONE', #8817 ) ;
#26975 = EDGE_CURVE ( 'NONE', #28034, #51695, #44693, .T. ) ;
#26976 = CARTESIAN_POINT ( 'NONE',  ( 37.25000000000000711, -27.21021009056489603, 4.499999999999997335 ) ) ;
#26977 = EDGE_CURVE ( 'NONE', #24332, #6547, #18148, .T. ) ;
#26978 = FACE_OUTER_BOUND ( 'NONE', #10260, .T. ) ;
#26979 = ORIENTED_EDGE ( 'NONE', *, *, #26977, .T. ) ;
#26980 = CARTESIAN_POINT ( 'NONE',  ( -37.00000000000000711, 3.287724142101577485, -11.73463472867572932 ) ) ;
#26981 = CIRCLE ( 'NONE', #24844, 12.74999999999999822 ) ;
#26982 = CARTESIAN_POINT ( 'NONE',  ( 11.58535936493772311, -28.03978107659439090, -13.63905399333256341 ) ) ;
#26983 = CARTESIAN_POINT ( 'NONE',  ( -35.00000000000000000, 11.81949347079751256, -2.968224442958276921 ) ) ;
#26984 = VERTEX_POINT ( 'NONE', #50380 ) ;
#26985 = EDGE_CURVE ( 'NONE', #64016, #11018, #17673, .T. ) ;
#26986 = CARTESIAN_POINT ( 'NONE',  ( -35.00000000000000000, 5.556331110570408960, 11.47561260193578825 ) ) ;
#26987 = EDGE_LOOP ( 'NONE', ( #40289, #58254, #35105, #32523, #52893, #17874 ) ) ;
#26988 = CARTESIAN_POINT ( 'NONE',  ( 35.00000000000000000, 12.60630747491662973, -1.908798535168425792 ) ) ;
#26989 = ORIENTED_EDGE ( 'NONE', *, *, #44290, .F. ) ;
#26990 = CARTESIAN_POINT ( 'NONE',  ( -17.77096676138755527, -6.470721604686525907, 11.85175806654005903 ) ) ;
#26991 = DIRECTION ( 'NONE',  ( 1.000000000000000000, -0.000000000000000000, 0.000000000000000000 ) ) ;
#26992 = DIRECTION ( 'NONE',  ( 0.000000000000000000, 0.01356324068817991828, -0.9999080150203990547 ) ) ;
#26993 = CARTESIAN_POINT ( 'NONE',  ( 5.516018279890452902, -0.006440244342253015342, -0.002104829434640740401 ) ) ;
#26994 = DIRECTION ( 'NONE',  ( 0.000000000000000000, 0.000000000000000000, 1.000000000000000000 ) ) ;
#26995 = CARTESIAN_POINT ( 'NONE',  ( 35.00000000000000000, 3.340853584269691368, 11.26103545359851665 ) ) ;
#26996 = CARTESIAN_POINT ( 'NONE',  ( 2.941278708680199916, 4.615461433467258345, 4.048809123187951720 ) ) ;
#26997 = ORIENTED_EDGE ( 'NONE', *, *, #53933, .F. ) ;
#26998 = LINE ( 'NONE', #52285, #13072 ) ;
#26999 =( BOUNDED_SURFACE ( )  B_SPLINE_SURFACE ( 3, 1, ( 
 ( #45357, #45038 ),
 ( #44687, #40701 ),
 ( #40035, #30063 ),
 ( #60993, #50374 ) ),
 .UNSPECIFIED., .F., .F., .F. ) 
 B_SPLINE_SURFACE_WITH_KNOTS ( ( 4, 4 ),
 ( 2, 2 ),
 ( 0.000000000000000000, 1.000000000000000000 ),
 ( 0.000000000000000000, 1.000000000000000000 ),
 .UNSPECIFIED. ) 
 GEOMETRIC_REPRESENTATION_ITEM ( )  RATIONAL_B_SPLINE_SURFACE ( (
 ( 1.000000000000000000, 1.000000000000000000),
 ( 0.8716676215708681896, 0.8964445200148164483),
 ( 0.8716676215708681896, 0.8964445200148164483),
 ( 1.000000000000000000, 1.000000000000000000) ) ) 
 REPRESENTATION_ITEM ( '' )  SURFACE ( )  );
#27000 = ORIENTED_EDGE ( 'NONE', *, *, #47667, .F. ) ;
#27001 = FACE_OUTER_BOUND ( 'NONE', #33330, .T. ) ;
#27002 = DIRECTION ( 'NONE',  ( 1.000000000000000000, -0.000000000000000000, 0.000000000000000000 ) ) ;
#27003 = VECTOR ( 'NONE', #26795, 1000.000000000000000 ) ;
#27004 = VERTEX_POINT ( 'NONE', #4827 ) ;
#27006 = CIRCLE ( 'NONE', #64165, 7.499999999999988454 ) ;
#27005 = CARTESIAN_POINT ( 'NONE',  ( -17.67713918426279918, 7.443964916031736045, 9.415221461658108026 ) ) ;
#27007 = CARTESIAN_POINT ( 'NONE',  ( -21.24030193723618609, 25.00000000000000000, -5.230344621181295395 ) ) ;
#27008 = DIRECTION ( 'NONE',  ( 0.000000000000000000, 0.000000000000000000, 1.000000000000000000 ) ) ;
#27009 = ORIENTED_EDGE ( 'NONE', *, *, #10726, .T. ) ;
#27010 = ADVANCED_FACE ( 'NONE', ( #3526 ), #4498, .T. ) ;
#27011 = ORIENTED_EDGE ( 'NONE', *, *, #32266, .T. ) ;
#27012 = DIRECTION ( 'NONE',  ( -1.000000000000000000, -0.000000000000000000, -0.000000000000000000 ) ) ;
#27013 = ORIENTED_EDGE ( 'NONE', *, *, #41177, .F. ) ;
#27014 = CARTESIAN_POINT ( 'NONE',  ( 2.903928887688490779, -8.407112942776166165, -2.496183838365682028 ) ) ;
#27015 = CARTESIAN_POINT ( 'NONE',  ( 35.00000000000000000, 4.705694406421931860E-17, -3.469127814946512892E-15 ) ) ;
#27016 = CARTESIAN_POINT ( 'NONE',  ( -3.491682519919724115, -11.78917057717144345, 6.588009498355533289 ) ) ;
#27017 = DIRECTION ( 'NONE',  ( 0.000000000000000000, -0.01356324068818000848, 0.9999080150203990547 ) ) ;
#27018 = ORIENTED_EDGE ( 'NONE', *, *, #12007, .T. ) ;
#27019 = CIRCLE ( 'NONE', #63083, 12.75000000000000178 ) ;
#27020 = EDGE_CURVE ( 'NONE', #38810, #39229, #25540, .T. ) ;
#27021 = CARTESIAN_POINT ( 'NONE',  ( 0.000000000000000000, 3.224464355699941720, -6.771471746881976728 ) ) ;
#27022 = CIRCLE ( 'NONE', #34458, 12.18650000000000055 ) ;
#27023 = CYLINDRICAL_SURFACE ( 'NONE', #10615, 2.899999999999994582 ) ;
#27024 = DIRECTION ( 'NONE',  ( -1.000000000000000000, 0.000000000000000000, 0.000000000000000000 ) ) ;
#27025 = AXIS2_PLACEMENT_3D ( 'NONE', #49323, #23045, #37988 ) ;
#27026 = DIRECTION ( 'NONE',  ( 0.000000000000000000, -0.6745969609292555846, -0.7381862504172049810 ) ) ;
#27027 = CARTESIAN_POINT ( 'NONE',  ( 37.00000000000000711, -7.146664589317845540, 9.321877890560507751 ) ) ;
#27028 = ADVANCED_FACE ( 'NONE', ( #64643 ), #38748, .T. ) ;
#27029 = CARTESIAN_POINT ( 'NONE',  ( 0.2646305136544072623, 4.312539723326133334, 11.46223899740601659 ) ) ;
#27030 = CARTESIAN_POINT ( 'NONE',  ( 2.276905613633647629, -5.757134111949723021, 5.031956778294114585 ) ) ;
#27031 = CARTESIAN_POINT ( 'NONE',  ( 2.990245332647882837, -8.465748356453849155, -0.5125330575220410356 ) ) ;
#27032 = VECTOR ( 'NONE', #39837, 1000.000000000000000 ) ;
#27033 = VERTEX_POINT ( 'NONE', #9784 ) ;
#27034 = DIRECTION ( 'NONE',  ( 0.000000000000000000, 0.01356324068817992175, -0.9999080150203990547 ) ) ;
#27035 = DIRECTION ( 'NONE',  ( -0.6845106172691086677, 0.000000000000000000, -0.7290028908350527637 ) ) ;
#27036 = VERTEX_POINT ( 'NONE', #24765 ) ;
#27037 = CARTESIAN_POINT ( 'NONE',  ( 1.375507693217084659, 10.61839108744976556, 6.813306181534342976 ) ) ;
#27038 = CARTESIAN_POINT ( 'NONE',  ( 2.903928887688064009, -4.835706109686843668, -7.316175791236489090 ) ) ;
#27039 = ORIENTED_EDGE ( 'NONE', *, *, #17299, .T. ) ;
#27040 = FACE_OUTER_BOUND ( 'NONE', #14364, .T. ) ;
#27041 = VERTEX_POINT ( 'NONE', #44367 ) ;
#27042 = AXIS2_PLACEMENT_3D ( 'NONE', #65617, #35692, #20090 ) ;
#27043 = CARTESIAN_POINT ( 'NONE',  ( -41.00000000000000711, -25.03188948156373073, -4.500000000000008882 ) ) ;
#27044 = ORIENTED_EDGE ( 'NONE', *, *, #36104, .F. ) ;
#27045 = EDGE_LOOP ( 'NONE', ( #23122, #40099, #4581, #418 ) ) ;
#27046 = ADVANCED_FACE ( 'NONE', ( #19115 ), #25094, .T. ) ;
#27047 = EDGE_CURVE ( 'NONE', #49890, #12885, #5787, .T. ) ;
#27048 = CARTESIAN_POINT ( 'NONE',  ( -27.15511094194037867, -1.375165223101520784, -2.092607239484544746 ) ) ;
#27049 = EDGE_LOOP ( 'NONE', ( #59286, #52429, #64425, #65605 ) ) ;
#27050 = EDGE_CURVE ( 'NONE', #14653, #46044, #59538, .T. ) ;
#27051 = CARTESIAN_POINT ( 'NONE',  ( -26.56525829975939956, -10.48173858536018699, 5.842830346974275280 ) ) ;
#27052 = CARTESIAN_POINT ( 'NONE',  ( -22.30398854582847790, -3.608860109585138254, 1.062335901716044750 ) ) ;
#27053 = DIRECTION ( 'NONE',  ( -1.000000000000000000, -1.836970198721029688E-16, 0.000000000000000000 ) ) ;
#27054 = CARTESIAN_POINT ( 'NONE',  ( 2.000000000000001776, 0.000000000000000000, 0.000000000000000000 ) ) ;
#27055 = EDGE_LOOP ( 'NONE', ( #1781, #27076, #15542, #37802 ) ) ;
#27056 = DIRECTION ( 'NONE',  ( 1.000000000000000000, 0.000000000000000000, -0.000000000000000000 ) ) ;
#27057 = CARTESIAN_POINT ( 'NONE',  ( -1.704253825401055966, -31.09323697348121129, 14.38225808330797584 ) ) ;
#27058 = CARTESIAN_POINT ( 'NONE',  ( 2.844750968616406972, -7.828506085988760077, 0.3326424433134245739 ) ) ;
#27060 = ORIENTED_EDGE ( 'NONE', *, *, #37555, .F. ) ;
#27059 = CARTESIAN_POINT ( 'NONE',  ( -24.31558339428802640, 8.695784598849996883, 8.272409342072648997 ) ) ;
#27061 = ADVANCED_FACE ( 'NONE', ( #51690 ), #55997, .T. ) ;
#27062 = CARTESIAN_POINT ( 'NONE',  ( -28.23735777670677294, 10.53122157488975574, -5.761455423850979862 ) ) ;
#27063 = ORIENTED_EDGE ( 'NONE', *, *, #41373, .T. ) ;
#27064 = CIRCLE ( 'NONE', #15382, 4.999999999999999112 ) ;
#27065 = CARTESIAN_POINT ( 'NONE',  ( 0.2653519890518152291, 9.381125756446678565, -7.871710682401816150 ) ) ;
#27066 = ORIENTED_EDGE ( 'NONE', *, *, #50713, .T. ) ;
#27067 = CARTESIAN_POINT ( 'NONE',  ( 35.00000000000000000, 9.217970097227839332, 7.971186206369370808 ) ) ;
#27068 = B_SPLINE_CURVE_WITH_KNOTS ( 'NONE', 3,
 ( #7225, #2615, #43128, #57802, #22541, #63730, #18210, #42806, #37828, #12878, #48157, #58119, #13214, #53121, #13520, #63407 ),
 .UNSPECIFIED., .F., .F.,
 ( 4, 3, 3, 3, 3, 4 ),
 ( 0.000000000000000000, 0.0002999043160757327328, 0.0005998071753050931943, 0.0008997092107374458870, 0.001204458948195583296, 0.001510329163476397491 ),
 .UNSPECIFIED. ) ;
#27069 = CARTESIAN_POINT ( 'NONE',  ( 2.241528039335007438, -4.895273998033963458, -5.858435878248560158 ) ) ;
#27070 = CARTESIAN_POINT ( 'NONE',  ( 0.8375941296792150936, -4.612912274495883480, 11.54987202580252159 ) ) ;
#27071 = ORIENTED_EDGE ( 'NONE', *, *, #30507, .F. ) ;
#27072 = LINE ( 'NONE', #42019, #32482 ) ;
#27073 = DIRECTION ( 'NONE',  ( -1.000000000000000000, -0.000000000000000000, 0.000000000000000000 ) ) ;
#27074 = CARTESIAN_POINT ( 'NONE',  ( -22.30861784526116054, -3.671054459752210786, -0.8834205920623630082 ) ) ;
#27075 = ORIENTED_EDGE ( 'NONE', *, *, #19364, .F. ) ;
#27076 = ORIENTED_EDGE ( 'NONE', *, *, #28261, .F. ) ;
#27077 = CARTESIAN_POINT ( 'NONE',  ( 2.770579946183330033, 7.633739187313475227, 1.653873933978900146 ) ) ;
#27078 = ORIENTED_EDGE ( 'NONE', *, *, #24018, .T. ) ;
#27079 = ORIENTED_EDGE ( 'NONE', *, *, #5050, .T. ) ;
#27080 = CARTESIAN_POINT ( 'NONE',  ( -27.01437459610461644, 10.69338818478080455, -8.240233560378637634 ) ) ;
#27081 = CARTESIAN_POINT ( 'NONE',  ( 35.00000000000000000, -1.908798535168467536, -12.60630747491662618 ) ) ;
#27082 = DIRECTION ( 'NONE',  ( 1.000000000000000000, 0.000000000000000000, 0.000000000000000000 ) ) ;
#27083 = CARTESIAN_POINT ( 'NONE',  ( -35.00000000000000000, 2.936739658820028520, -11.37311665002360783 ) ) ;
#27084 = DIRECTION ( 'NONE',  ( 0.000000000000000000, 0.000000000000000000, 1.000000000000000000 ) ) ;
#27085 = AXIS2_PLACEMENT_3D ( 'NONE', #16032, #11381, #36660 ) ;
#27086 = EDGE_CURVE ( 'NONE', #64921, #34336, #10434, .T. ) ;
#27087 = DIRECTION ( 'NONE',  ( 0.000000000000000000, -0.04924826701375277505, -0.9987865678893275145 ) ) ;
#27088 = ADVANCED_FACE ( 'NONE', ( #60999 ), #23910, .F. ) ;
#27089 = ORIENTED_EDGE ( 'NONE', *, *, #46763, .F. ) ;
#27090 = DIRECTION ( 'NONE',  ( -0.3865475372811021937, -0.8082200352954586053, -0.4442537292684469175 ) ) ;
#27091 = B_SPLINE_CURVE_WITH_KNOTS ( 'NONE', 3,
 ( #11931, #52195, #1968, #48201, #32210, #1328, #6643, #52835, #6960, #27895 ),
 .UNSPECIFIED., .F., .F.,
 ( 4, 3, 3, 4 ),
 ( 1.301042606982605321E-18, 6.607638129004494304E-05, 9.911389841680519547E-05, 0.0001667630577588623654 ),
 .UNSPECIFIED. ) ;
#27092 = VECTOR ( 'NONE', #3446, 1000.000000000000000 ) ;
#27093 = FACE_OUTER_BOUND ( 'NONE', #41603, .T. ) ;
#27094 = EDGE_CURVE ( 'NONE', #50042, #12300, #45690, .T. ) ;
#27095 = CARTESIAN_POINT ( 'NONE',  ( 2.305787727787084407, 7.566723232958072032, 1.164987321564758371 ) ) ;
#27096 = DIRECTION ( 'NONE',  ( 0.000000000000000000, -0.01356324068817991828, 0.9999080150203990547 ) ) ;
#27097 = CARTESIAN_POINT ( 'NONE',  ( 1.452237505248555660, -9.303501428256085504, 8.579708443906715942 ) ) ;
#27098 = CIRCLE ( 'NONE', #17569, 4.999999999999999112 ) ;
#27099 = CARTESIAN_POINT ( 'NONE',  ( -35.00000000000000000, -7.561043153947899498, -9.557269938331636183 ) ) ;
#27100 = CARTESIAN_POINT ( 'NONE',  ( -35.04643116707788408, -0.01135624435144415301, -0.004425962698870883338 ) ) ;
#27101 = EDGE_CURVE ( 'NONE', #15014, #12978, #6423, .T. ) ;
#27103 = VERTEX_POINT ( 'NONE', #493 ) ;
#27102 = ADVANCED_FACE ( 'NONE', ( #40707 ), #30400, .T. ) ;
#27104 = DIRECTION ( 'NONE',  ( -1.000000000000000000, 0.000000000000000000, 0.000000000000000000 ) ) ;
#27105 = CARTESIAN_POINT ( 'NONE',  ( 0.2956976708475456128, -1.911282699793644735, -12.10637007622315053 ) ) ;
#27106 = DIRECTION ( 'NONE',  ( -1.000000000000000000, 0.000000000000000000, -0.000000000000000000 ) ) ;
#27107 = DIRECTION ( 'NONE',  ( 1.000000000000000000, 0.000000000000000000, -0.000000000000000000 ) ) ;
#27108 = EDGE_CURVE ( 'NONE', #62166, #4778, #27663, .T. ) ;
#27109 = AXIS2_PLACEMENT_3D ( 'NONE', #28362, #58980, #39308 ) ;
#27110 = CARTESIAN_POINT ( 'NONE',  ( 10.67917606476195580, 1.165423783710027861, -13.45046084793106367 ) ) ;
#27111 = CARTESIAN_POINT ( 'NONE',  ( -25.47095544430322889, -11.72962784578977313, 6.684589422636681988 ) ) ;
#27112 = ORIENTED_EDGE ( 'NONE', *, *, #56167, .T. ) ;
#27113 = CARTESIAN_POINT ( 'NONE',  ( 18.73707042796466027, -5.248124276600211857, 10.80148738011064680 ) ) ;
#27114 = DIRECTION ( 'NONE',  ( -1.000000000000000000, 0.000000000000000000, 0.000000000000000000 ) ) ;
#27115 = CARTESIAN_POINT ( 'NONE',  ( 0.2911222467163567806, 9.248441845564686403, 8.040284153519408505 ) ) ;
#27116 = CARTESIAN_POINT ( 'NONE',  ( -35.04709527796842394, 0.01120703303052542066, -0.005220632201003577721 ) ) ;
#27117 = VERTEX_POINT ( 'NONE', #801 ) ;
#27118 = CARTESIAN_POINT ( 'NONE',  ( 0.2647959493198558945, 2.271080632828060608, 12.03358727341674950 ) ) ;
#27119 = CARTESIAN_POINT ( 'NONE',  ( -35.00000000000000000, 0.000000000000000000, 0.000000000000000000 ) ) ;
#27121 = ORIENTED_EDGE ( 'NONE', *, *, #9915, .F. ) ;
#27120 = DIRECTION ( 'NONE',  ( 0.000000000000000000, 0.000000000000000000, -1.000000000000000000 ) ) ;
#27122 = DIRECTION ( 'NONE',  ( 1.000000000000000000, -0.000000000000000000, 0.000000000000000000 ) ) ;
#27123 = EDGE_CURVE ( 'NONE', #63127, #38516, #42515, .T. ) ;
#27124 = DIRECTION ( 'NONE',  ( 0.000000000000000000, 0.9868265225415265851, -0.1617819965527619031 ) ) ;
#27125 = VERTEX_POINT ( 'NONE', #15744 ) ;
#27126 = EDGE_CURVE ( 'NONE', #48166, #33099, #34032, .T. ) ;
#27127 = FACE_OUTER_BOUND ( 'NONE', #64351, .T. ) ;
#27128 = CARTESIAN_POINT ( 'NONE',  ( 5.516018279890452902, 0.006771744149385265123, -0.0002248006052448750405 ) ) ;
#27129 = DIRECTION ( 'NONE',  ( 0.000000000000000000, 0.01356324068817992001, -0.9999080150203990547 ) ) ;
#27130 = CARTESIAN_POINT ( 'NONE',  ( -3.221163217498328901, -8.204480317174903448, 10.72779841256758360 ) ) ;
#27131 = DIRECTION ( 'NONE',  ( 0.000000000000000000, 0.000000000000000000, 1.000000000000000000 ) ) ;
#27132 = CARTESIAN_POINT ( 'NONE',  ( 0.5547464869798237608, 11.69908463509556995, 3.933612953276277580 ) ) ;
#27134 = ORIENTED_EDGE ( 'NONE', *, *, #57570, .T. ) ;
#27133 = CARTESIAN_POINT ( 'NONE',  ( -35.00000000000000000, -9.217970097227665249, -7.971186206369574201 ) ) ;
#27135 = CARTESIAN_POINT ( 'NONE',  ( -22.27713295444592845, 2.530364014314313792, 2.673940016108976803 ) ) ;
#27136 = PRODUCT_DEFINITION_FORMATION_WITH_SPECIFIED_SOURCE ( 'ANY', '', #19015, .NOT_KNOWN. ) ;
#27137 = ORIENTED_EDGE ( 'NONE', *, *, #56982, .F. ) ;
#27138 = CARTESIAN_POINT ( 'NONE',  ( 24.65820709255600818, -2.318610723833587794, -11.78042893945787384 ) ) ;
#27139 = ORIENTED_EDGE ( 'NONE', *, *, #44829, .F. ) ;
#27140 = ITEM_DEFINED_TRANSFORMATION ( 'NONE', 'NONE', #43029,  #24966 ) ;
#27141 = CARTESIAN_POINT ( 'NONE',  ( 1.459561108993333134, -11.65083230253660140, 4.912799202119202846 ) ) ;
#27142 = CARTESIAN_POINT ( 'NONE',  ( -3.620643385775215162, 10.87206787913274830, 5.083569600177869852 ) ) ;
#27143 = CARTESIAN_POINT ( 'NONE',  ( -43.04762206662383761, -1.319502909267362467, 15.89732852394791784 ) ) ;
#27144 = CARTESIAN_POINT ( 'NONE',  ( 5.514970785353741078, 0.001117786416802554229, 0.004588761610585028947 ) ) ;
#27145 = EDGE_LOOP ( 'NONE', ( #46577, #21072, #62069, #32466 ) ) ;
#27146 = AXIS2_PLACEMENT_3D ( 'NONE', #24559, #59820, #64458 ) ;
#27147 = DIRECTION ( 'NONE',  ( -1.000000000000000000, 0.000000000000000000, 0.000000000000000000 ) ) ;
#27148 = CARTESIAN_POINT ( 'NONE',  ( 2.273267844204865273, 5.758000272829378652, -5.029122824445665607 ) ) ;
#27149 = ORIENTED_EDGE ( 'NONE', *, *, #11007, .F. ) ;
#27150 = ORIENTED_EDGE ( 'NONE', *, *, #27450, .T. ) ;
#27151 = CARTESIAN_POINT ( 'NONE',  ( 3.152665057736161902, 7.719888720907650992, -1.848755561854025231 ) ) ;
#27152 = ORIENTED_EDGE ( 'NONE', *, *, #59747, .F. ) ;
#27153 = CARTESIAN_POINT ( 'NONE',  ( 29.51976981715666781, -7.690765383426355406, 11.09513982864076276 ) ) ;
#27154 = B_SPLINE_CURVE_WITH_KNOTS ( 'NONE', 3,
 ( #52848, #41215, #57194, #56536, #10979, #6015, #51879, #11619, #6656, #1673, #21941, #42188, #62478, #16942, #37209, #57524, #32227, #3303, #43850, #59467, #48852, #22930 ),
 .UNSPECIFIED., .F., .F.,
 ( 4, 3, 3, 3, 3, 3, 3, 4 ),
 ( 1.084202172485504434E-19, 4.449119708436884238E-05, 6.626296329540428309E-05, 8.803456484962676601E-05, 0.0001098060367612800945, 0.0001315774408628517765, 0.0001760698110411190547, 0.0001829697163287842695 ),
 .UNSPECIFIED. ) ;
#27155 = CARTESIAN_POINT ( 'NONE',  ( 10.67791943353093309, 1.166253086089546587, 13.45039264577783023 ) ) ;
#27156 = AXIS2_PLACEMENT_3D ( 'NONE', #53235, #18328, #44228 ) ;
#27157 = CARTESIAN_POINT ( 'NONE',  ( 37.00000000000000711, -12.54989509947652415, -2.250029553613715372 ) ) ;
#27158 = DIRECTION ( 'NONE',  ( 1.000000000000000000, -0.000000000000000000, -0.000000000000000000 ) ) ;
#27159 = DIRECTION ( 'NONE',  ( -1.000000000000000000, 0.000000000000000000, 0.000000000000000000 ) ) ;
#27160 = CARTESIAN_POINT ( 'NONE',  ( 35.00000000000000000, 7.238157050195628273, -10.49626516989273384 ) ) ;
#27161 = EDGE_CURVE ( 'NONE', #20299, #5276, #56321, .T. ) ;
#27162 = EDGE_LOOP ( 'NONE', ( #9787, #47859, #47354, #11666 ) ) ;
#27163 = DIRECTION ( 'NONE',  ( 1.000000000000000000, 0.000000000000000000, -0.000000000000000000 ) ) ;
#27164 = ORIENTED_EDGE ( 'NONE', *, *, #22220, .T. ) ;
#27165 = CARTESIAN_POINT ( 'NONE',  ( 35.00000000000000000, 10.80478261802181628, -5.636262487437359248 ) ) ;
#27166 = CARTESIAN_POINT ( 'NONE',  ( 2.889800649504073782, 3.882893708502047847, 4.732281052280325362 ) ) ;
#27167 = CARTESIAN_POINT ( 'NONE',  ( -27.78468958554971380, 25.00000000000000000, 8.565911087387465983 ) ) ;
#27168 = CARTESIAN_POINT ( 'NONE',  ( -35.00000000000000000, 1.030638227056741574, -12.14284015767849034 ) ) ;
#27169 = ORIENTED_EDGE ( 'NONE', *, *, #27217, .F. ) ;
#27170 = B_SPLINE_CURVE_WITH_KNOTS ( 'NONE', 3,
 ( #63840, #54214, #59208, #2028, #63195, #43558, #47579, #18322, #64187, #12987, #33269, #18659, #53574, #8020, #7325, #28282, #38919, #12319, #17661 ),
 .UNSPECIFIED., .F., .F.,
 ( 4, 3, 3, 3, 3, 3, 4 ),
 ( 0.000000000000000000, 2.831840207499574684E-05, 4.217266859840548322E-05, 5.602024318395963231E-05, 6.290810167969062899E-05, 9.120440630945090394E-05, 0.0001153103026479756018 ),
 .UNSPECIFIED. ) ;
#27171 = VERTEX_POINT ( 'NONE', #31058 ) ;
#27172 = EDGE_CURVE ( 'NONE', #35706, #53805, #37213, .T. ) ;
#27173 = CARTESIAN_POINT ( 'NONE',  ( -27.09150307427447757, 0.1754204729056442480, 2.306459590995622477 ) ) ;
#27174 =( BOUNDED_SURFACE ( )  B_SPLINE_SURFACE ( 3, 1, ( 
 ( #56372, #52390 ),
 ( #21804, #42053 ),
 ( #20804, #22105 ),
 ( #31108, #62333 ) ),
 .UNSPECIFIED., .F., .F., .F. ) 
 B_SPLINE_SURFACE_WITH_KNOTS ( ( 4, 4 ),
 ( 2, 2 ),
 ( 0.000000000000000000, 1.000000000000000000 ),
 ( 0.000000000000000000, 1.000000000000000000 ),
 .UNSPECIFIED. ) 
 GEOMETRIC_REPRESENTATION_ITEM ( )  RATIONAL_B_SPLINE_SURFACE ( (
 ( 1.000000000000000000, 1.000000000000000000),
 ( 0.9942764183789327692, 0.8450855930916585379),
 ( 0.9942764183789327692, 0.8450855930916585379),
 ( 1.000000000000000000, 1.000000000000000000) ) ) 
 REPRESENTATION_ITEM ( '' )  SURFACE ( )  );
#27175 = ORIENTED_EDGE ( 'NONE', *, *, #18767, .F. ) ;
#27176 = CARTESIAN_POINT ( 'NONE',  ( -7.489022030332961322, 8.034049540753141372, -10.84914964302385521 ) ) ;
#27177 = CARTESIAN_POINT ( 'NONE',  ( 26.08439714455133185, 12.97057518889166516, 3.743551691817328386 ) ) ;
#27178 = DIRECTION ( 'NONE',  ( 1.000000000000000000, 0.000000000000000000, 0.000000000000000000 ) ) ;
#27179 = CARTESIAN_POINT ( 'NONE',  ( -37.00000000000000711, -9.196955404009360180, 8.830544224262913744 ) ) ;
#27180 = VERTEX_POINT ( 'NONE', #45362 ) ;
#27181 = CARTESIAN_POINT ( 'NONE',  ( 0.3057689695767483173, 12.11137787899271956, 1.901059295890957790 ) ) ;
#27182 = CARTESIAN_POINT ( 'NONE',  ( 26.34661844826604593, -13.08594712317289321, 3.317828791472332117 ) ) ;
#27183 = CARTESIAN_POINT ( 'NONE',  ( 0.2651627682582903822, -10.64925413290589695, -6.046625184671096775 ) ) ;
#27184 = CARTESIAN_POINT ( 'NONE',  ( -49.13724917365555456, -0.1745483773780783232, 6.524050439336994245 ) ) ;
#27185 = CIRCLE ( 'NONE', #9143, 7.938172270156617749 ) ;
#27186 = CARTESIAN_POINT ( 'NONE',  ( -35.00000000000000000, 9.733281772932279807, -8.235637554476539890 ) ) ;
#27187 = DIRECTION ( 'NONE',  ( 0.000000000000000000, 0.8696919319575200369, 0.4935949184179230786 ) ) ;
#27188 = VECTOR ( 'NONE', #44663, 1000.000000000000000 ) ;
#27189 =( BOUNDED_SURFACE ( )  B_SPLINE_SURFACE ( 3, 1, ( 
 ( #10213, #5921 ),
 ( #30492, #55110 ),
 ( #35486, #26177 ),
 ( #20533, #41118 ) ),
 .UNSPECIFIED., .F., .F., .F. ) 
 B_SPLINE_SURFACE_WITH_KNOTS ( ( 4, 4 ),
 ( 2, 2 ),
 ( 0.000000000000000000, 1.000000000000000000 ),
 ( 0.000000000000000000, 1.000000000000000000 ),
 .UNSPECIFIED. ) 
 GEOMETRIC_REPRESENTATION_ITEM ( )  RATIONAL_B_SPLINE_SURFACE ( (
 ( 1.000000000000000000, 1.000000000000000000),
 ( 0.9942764183789327692, 0.8450855930916580938),
 ( 0.9942764183789327692, 0.8450855930916580938),
 ( 1.000000000000000000, 1.000000000000000000) ) ) 
 REPRESENTATION_ITEM ( '' )  SURFACE ( )  );
#27190 = ORIENTED_EDGE ( 'NONE', *, *, #26062, .T. ) ;
#27191 = LINE ( 'NONE', #27505, #13724 ) ;
#27192 = EDGE_LOOP ( 'NONE', ( #46306, #35236, #17348, #54787 ) ) ;
#27193 = CARTESIAN_POINT ( 'NONE',  ( -4.989057617119008192, -0.9162120371760335003, -13.46887357958837406 ) ) ;
#27194 = DIRECTION ( 'NONE',  ( 0.000000000000000000, 0.3554799084908900619, 0.9346839223284566511 ) ) ;
#27195 = DIRECTION ( 'NONE',  ( 0.000000000000000000, 0.01356324068817998073, -0.9999080150203990547 ) ) ;
#27196 = CARTESIAN_POINT ( 'NONE',  ( 1.549075743843500552, 12.65619669350982157, 0.6747257554039380878 ) ) ;
#27197 = CARTESIAN_POINT ( 'NONE',  ( 3.347841273039249721, -10.61118957148187825, 8.345816669330455184 ) ) ;
#27198 = CIRCLE ( 'NONE', #16577, 5.000000000000001776 ) ;
#27199 = VERTEX_POINT ( 'NONE', #65623 ) ;
#27200 = VERTEX_POINT ( 'NONE', #46359 ) ;
#27201 = DIRECTION ( 'NONE',  ( -1.000000000000000000, 0.000000000000000000, 0.000000000000000000 ) ) ;
#27202 = ORIENTED_EDGE ( 'NONE', *, *, #14740, .F. ) ;
#27203 = CARTESIAN_POINT ( 'NONE',  ( -27.08421723179412055, -2.234476190936508733, 0.5069555058557426719 ) ) ;
#27204 = DIRECTION ( 'NONE',  ( 1.000000000000000000, 0.000000000000000000, -0.000000000000000000 ) ) ;
#27205 = CARTESIAN_POINT ( 'NONE',  ( 2.889800649504073782, 2.030191121417214806, -5.774917447012977156 ) ) ;
#27206 = DIRECTION ( 'NONE',  ( 0.000000000000000000, 0.01356324068817998940, -0.9999080150203990547 ) ) ;
#27207 = CARTESIAN_POINT ( 'NONE',  ( -37.00000000000000711, -5.644643009978993931, -10.30098186818255890 ) ) ;
#27208 = CARTESIAN_POINT ( 'NONE',  ( 2.290907136834313906, 5.755317856506293239, 5.041121061900457612 ) ) ;
#27209 = DIRECTION ( 'NONE',  ( 1.000000000000000000, -0.000000000000000000, 0.000000000000000000 ) ) ;
#27210 = ORIENTED_EDGE ( 'NONE', *, *, #50456, .F. ) ;
#27211 = VERTEX_POINT ( 'NONE', #15100 ) ;
#27212 = CARTESIAN_POINT ( 'NONE',  ( 0.000000000000000000, 6.767909380267608022, 2.119450094687897579 ) ) ;
#27213 = ORIENTED_EDGE ( 'NONE', *, *, #55883, .T. ) ;
#27214 = B_SPLINE_CURVE_WITH_KNOTS ( 'NONE', 3,
 ( #48459, #52780, #7206, #63076, #2906, #21873, #12202, #43432, #47788, #53445, #62734, #57441, #53100, #17853, #63709, #42121, #11871, #37475, #63386, #12855, #38458, #22178 ),
 .UNSPECIFIED., .F., .F.,
 ( 4, 3, 3, 3, 3, 3, 3, 4 ),
 ( 8.824766327896537836E-19, 4.449119708436589471E-05, 6.626296329540048839E-05, 8.803456484962241565E-05, 0.0001098060367612772349, 0.0001315774408628484155, 0.0001760698110411148263, 0.0001829697163287826974 ),
 .UNSPECIFIED. ) ;
#27215 =( NAMED_UNIT ( * ) PLANE_ANGLE_UNIT ( ) SI_UNIT ( $, .RADIAN. ) );
#27216 = CARTESIAN_POINT ( 'NONE',  ( 21.63322885546936192, -13.42214251193591679, -1.501346303079956090 ) ) ;
#27217 = EDGE_CURVE ( 'NONE', #19899, #62456, #8129, .T. ) ;
#27218 = DIRECTION ( 'NONE',  ( 1.000000000000000000, -0.000000000000000000, 0.000000000000000000 ) ) ;
#27219 = CARTESIAN_POINT ( 'NONE',  ( 41.00000000000000711, -25.30020925422648048, 3.022492086418942847 ) ) ;
#27220 = EDGE_LOOP ( 'NONE', ( #32016, #23769 ) ) ;
#27221 = DIRECTION ( 'NONE',  ( 1.000000000000000000, -0.000000000000000000, 0.000000000000000000 ) ) ;
#27222 = CARTESIAN_POINT ( 'NONE',  ( -22.35190811654613441, 1.736165297231020199, -3.498661567523014604 ) ) ;
#27223 = CARTESIAN_POINT ( 'NONE',  ( -37.25000000000000711, -20.00000000000000000, 2.449293598294706907E-15 ) ) ;
#27224 = VERTEX_POINT ( 'NONE', #27697 ) ;
#27225 = ORIENTED_EDGE ( 'NONE', *, *, #9524, .T. ) ;
#27226 = DIRECTION ( 'NONE',  ( -1.000000000000000000, -0.000000000000000000, 0.000000000000000000 ) ) ;
#27227 = VERTEX_POINT ( 'NONE', #7410 ) ;
#27228 = ORIENTED_EDGE ( 'NONE', *, *, #16047, .F. ) ;
#27229 = EDGE_LOOP ( 'NONE', ( #52530, #15721, #1128, #29816 ) ) ;
#27230 = ORIENTED_EDGE ( 'NONE', *, *, #63552, .F. ) ;
#27231 = CARTESIAN_POINT ( 'NONE',  ( 0.2739690278137258961, 4.360944092821455342, 11.44648082006007961 ) ) ;
#27232 = FACE_OUTER_BOUND ( 'NONE', #44951, .T. ) ;
#27233 = ADVANCED_FACE ( 'NONE', ( #38328 ), #62605, .T. ) ;
#27234 = CARTESIAN_POINT ( 'NONE',  ( -37.00000000000000711, 0.000000000000000000, 0.000000000000000000 ) ) ;
#27235 = CARTESIAN_POINT ( 'NONE',  ( 2.262775599886257094, 2.745802076335829067, -7.131180968652195418 ) ) ;
#27236 = DIRECTION ( 'NONE',  ( 0.000000000000000000, -0.01356324068817998940, 0.9999080150203990547 ) ) ;
#27237 = CONICAL_SURFACE ( 'NONE', #38916, 15.00000000000000000, 0.5235987755983000369 ) ;
#27238 = CARTESIAN_POINT ( 'NONE',  ( -22.46225619532221884, -3.746472695305363310, -1.978788174090802876 ) ) ;
#27239 = CIRCLE ( 'NONE', #38921, 12.18649999999999878 ) ;
#27240 = EDGE_CURVE ( 'NONE', #58346, #30510, #5379, .T. ) ;
#27241 = ORIENTED_EDGE ( 'NONE', *, *, #38128, .F. ) ;
#27242 = CARTESIAN_POINT ( 'NONE',  ( -35.00000000000000000, 11.99999999999999289, 1.469576158976823158E-15 ) ) ;
#27243 = EDGE_CURVE ( 'NONE', #36620, #9122, #47353, .T. ) ;
#27244 = CARTESIAN_POINT ( 'NONE',  ( 2.000000000000001776, 0.000000000000000000, 0.000000000000000000 ) ) ;
#27245 = ADVANCED_FACE ( 'NONE', ( #7765 ), #48348, .T. ) ;
#27246 = CARTESIAN_POINT ( 'NONE',  ( -14.47334165536100059, 7.347880794884120722E-16, 6.000000000000000888 ) ) ;
#27247 = CARTESIAN_POINT ( 'NONE',  ( 0.2706063244538013945, -2.299194104693162544, 12.03021891034990887 ) ) ;
#27248 = CYLINDRICAL_SURFACE ( 'NONE', #62049, 5.000000000000001776 ) ;
#27249 = CARTESIAN_POINT ( 'NONE',  ( 37.00000000000000711, 10.01317267707886494, -6.946017217729976601 ) ) ;
#27250 = ORIENTED_EDGE ( 'NONE', *, *, #49029, .T. ) ;
#27251 = EDGE_CURVE ( 'NONE', #42435, #42706, #30668, .T. ) ;
#27252 = CARTESIAN_POINT ( 'NONE',  ( 8.437200413559441614, 4.476360154859203355, 11.13383131558893346 ) ) ;
#27253 = ORIENTED_EDGE ( 'NONE', *, *, #20663, .T. ) ;
#27254 = EDGE_CURVE ( 'NONE', #43456, #44869, #14460, .T. ) ;
#27255 = CARTESIAN_POINT ( 'NONE',  ( 0.3040950598368144520, -4.428852722102808670, 11.43390362554251816 ) ) ;
#27256 = CARTESIAN_POINT ( 'NONE',  ( -35.00000000000000000, -10.28547182238004076, -5.672855678558794246 ) ) ;
#27257 = CARTESIAN_POINT ( 'NONE',  ( 2.665405856346781732, 9.171500569027793759, -2.723742051529362662 ) ) ;
#27258 = DIRECTION ( 'NONE',  ( 0.000000000000000000, 0.2006870767258890631, -0.9796553971857742127 ) ) ;
#27259 = CARTESIAN_POINT ( 'NONE',  ( 2.261269890822073414, -6.685978463722149101, 3.699080366006672449 ) ) ;
#27260 = ORIENTED_EDGE ( 'NONE', *, *, #11308, .T. ) ;
#27261 = DIRECTION ( 'NONE',  ( 0.000000000000000000, -0.2960891610144577024, -0.9551603052523457427 ) ) ;
#27262 = LINE ( 'NONE', #16958, #29093 ) ;
#27263 = CARTESIAN_POINT ( 'NONE',  ( 35.00000000000000000, 4.705694406421931860E-17, -3.469127814946512892E-15 ) ) ;
#27264 = CARTESIAN_POINT ( 'NONE',  ( 0.2652384770603652409, -2.061429379240400372, -12.07140968216696031 ) ) ;
#27265 = EDGE_CURVE ( 'NONE', #28690, #2019, #12724, .T. ) ;
#27266 = FACE_OUTER_BOUND ( 'NONE', #52357, .T. ) ;
#27267 = ORIENTED_EDGE ( 'NONE', *, *, #60811, .F. ) ;
#27268 = UNCERTAINTY_MEASURE_WITH_UNIT (LENGTH_MEASURE( 1.000000000000000082E-05 ), #60094, 'distance_accuracy_value', 'NONE');
#27269 = CARTESIAN_POINT ( 'NONE',  ( 2.305787727787084407, -0.1666591538752151269, -7.654065630109508689 ) ) ;
#27270 = CARTESIAN_POINT ( 'NONE',  ( 2.000000000000001776, 1.693411908627302509, -7.306323022404582979 ) ) ;
#27271 = APPLICATION_CONTEXT ( 'automotive_design' ) ;
#27272 = AXIS2_PLACEMENT_3D ( 'NONE', #26325, #46608, #30342 ) ;
#27273 = VERTEX_POINT ( 'NONE', #33008 ) ;
#27274 = VERTEX_POINT ( 'NONE', #42645 ) ;
#27275 = DIRECTION ( 'NONE',  ( 0.000000000000000000, 0.01356324068817998940, -0.9999080150203990547 ) ) ;
#27276 = CARTESIAN_POINT ( 'NONE',  ( 37.00000000000000711, 4.705694406421931860E-17, -3.469127814946512892E-15 ) ) ;
#27277 = CARTESIAN_POINT ( 'NONE',  ( 37.00000000000000711, 4.705694406421931860E-17, -3.469127814946512892E-15 ) ) ;
#27278 = CARTESIAN_POINT ( 'NONE',  ( 0.3223008802179258558, -1.888629463821764887, 12.11889957318023114 ) ) ;
#27279 = ORIENTED_EDGE ( 'NONE', *, *, #40054, .F. ) ;
#27280 = ORIENTED_EDGE ( 'NONE', *, *, #61867, .T. ) ;
#27281 = ORIENTED_EDGE ( 'NONE', *, *, #39196, .T. ) ;
#27282 = DIRECTION ( 'NONE',  ( -0.3939253465568944290, -0.8008152550167534356, -0.4511294145502848241 ) ) ;
#27283 = EDGE_CURVE ( 'NONE', #29745, #33694, #17413, .T. ) ;
#27284 = B_SPLINE_CURVE_WITH_KNOTS ( 'NONE', 3,
 ( #21751, #46671, #21060, #1127, #42002, #62282, #36017, #16736, #47657, #37009, #57313, #11735, #46354, #52664, #32020, #2104 ),
 .UNSPECIFIED., .F., .F.,
 ( 4, 3, 3, 3, 3, 4 ),
 ( 0.000000000000000000, 0.0003017745587525239460, 0.0006035491769808734152, 0.0009053241094668162481, 0.001207275924540911769, 0.001510325902534833840 ),
 .UNSPECIFIED. ) ;
#27285 = DIRECTION ( 'NONE',  ( -1.000000000000000000, -0.000000000000000000, -0.000000000000000000 ) ) ;
#27286 = ORIENTED_EDGE ( 'NONE', *, *, #9929, .T. ) ;
#27287 = CARTESIAN_POINT ( 'NONE',  ( -10.95212338237647920, -9.902220863987562183, 6.778349501228839280 ) ) ;
#27288 = CARTESIAN_POINT ( 'NONE',  ( -36.00000000000000711, -9.390600770287932164, -8.624332853796161658 ) ) ;
#27289 = ORIENTED_EDGE ( 'NONE', *, *, #14548, .T. ) ;
#27290 = CARTESIAN_POINT ( 'NONE',  ( 0.2653141334712578736, 11.49252672845888945, -4.229817350136297449 ) ) ;
#27291 = CARTESIAN_POINT ( 'NONE',  ( 11.89229108778294908, -32.87417574757987637, -11.69979538107606487 ) ) ;
#27292 = CARTESIAN_POINT ( 'NONE',  ( 23.96628737370385664, -3.705566309175509332, 11.41801794016889282 ) ) ;
#27293 = ORIENTED_EDGE ( 'NONE', *, *, #21806, .T. ) ;
#27294 = FACE_OUTER_BOUND ( 'NONE', #39153, .T. ) ;
#27295 = ORIENTED_EDGE ( 'NONE', *, *, #5404, .F. ) ;
#27296 = DIRECTION ( 'NONE',  ( 0.000000000000000000, 0.000000000000000000, 1.000000000000000000 ) ) ;
#27297 = CARTESIAN_POINT ( 'NONE',  ( -19.42938127781367896, -4.328328797226848934, 12.78801166805076583 ) ) ;
#27298 = DIRECTION ( 'NONE',  ( 0.000000000000000000, 0.000000000000000000, 1.000000000000000000 ) ) ;
#27299 = DIRECTION ( 'NONE',  ( -1.000000000000000000, 0.000000000000000000, -0.000000000000000000 ) ) ;
#27300 = CARTESIAN_POINT ( 'NONE',  ( 2.241506898688419014, -6.591904579673256492, 3.851253041557081591 ) ) ;
#27301 = EDGE_CURVE ( 'NONE', #32993, #23007, #41473, .T. ) ;
#27302 = DIRECTION ( 'NONE',  ( 0.000000000000000000, 0.000000000000000000, 1.000000000000000000 ) ) ;
#27303 = CARTESIAN_POINT ( 'NONE',  ( -35.00000000000000000, 0.000000000000000000, 0.000000000000000000 ) ) ;
#27304 = EDGE_LOOP ( 'NONE', ( #55202, #41540, #34484, #184 ) ) ;
#27305 = DIRECTION ( 'NONE',  ( -1.000000000000000000, 0.000000000000000000, 0.000000000000000000 ) ) ;
#27306 = ORIENTED_EDGE ( 'NONE', *, *, #61952, .T. ) ;
#27307 = CARTESIAN_POINT ( 'NONE',  ( 0.2759803524722185264, -4.367180139677396156, 11.44482553421629589 ) ) ;
#27308 = EDGE_CURVE ( 'NONE', #35192, #42088, #37473, .T. ) ;
#27309 = CARTESIAN_POINT ( 'NONE',  ( 3.152665057735933640, -5.461013642407022139, -5.761241965768077122 ) ) ;
#27310 = EDGE_CURVE ( 'NONE', #37124, #34795, #8156, .T. ) ;
#27311 = ORIENTED_EDGE ( 'NONE', *, *, #15747, .F. ) ;
#27312 = DIRECTION ( 'NONE',  ( 0.000000000000000000, -0.01356324068817992175, 0.9999080150203990547 ) ) ;
#27313 = CARTESIAN_POINT ( 'NONE',  ( 0.2767916011545383248, 12.02950149294536786, -2.313848297676325050 ) ) ;
#27314 = DIRECTION ( 'NONE',  ( 1.000000000000000000, -0.000000000000000000, -0.000000000000000000 ) ) ;
#27315 = CIRCLE ( 'NONE', #55986, 6.936499999999992561 ) ;
#27316 = ORIENTED_EDGE ( 'NONE', *, *, #54291, .F. ) ;
#27317 = ORIENTED_EDGE ( 'NONE', *, *, #18122, .T. ) ;
#27318 = CIRCLE ( 'NONE', #28376, 2.899999999999995914 ) ;
#27319 = EDGE_CURVE ( 'NONE', #57915, #50989, #2200, .T. ) ;
#27320 = CARTESIAN_POINT ( 'NONE',  ( 35.00000000000000000, -12.18632975068352664, -0.06441628369832411161 ) ) ;
#27321 = ORIENTED_EDGE ( 'NONE', *, *, #20389, .T. ) ;
#27322 = EDGE_CURVE ( 'NONE', #51686, #15952, #12812, .T. ) ;
#27323 = CARTESIAN_POINT ( 'NONE',  ( 3.100650473569670940, -6.348250400753888023, 4.737096019059257479 ) ) ;
#27324 = B_SPLINE_CURVE_WITH_KNOTS ( 'NONE', 3,
 ( #44270, #10245, #60460, #30523, #45835, #59255, #50828, #20571, #50510, #40851, #9930, #25216, #54272, #31201, #56124, #10566, #49303, #3751, #40169, #62747 ),
 .UNSPECIFIED., .F., .F.,
 ( 4, 2, 2, 2, 2, 2, 2, 2, 2, 4 ),
 ( 0.000000000000000000, 0.001056023233319194161, 0.001584034849978791133, 0.002112046466638388322, 0.003168069699957580532, 0.003696081316617175986, 0.004224092933276770573, 0.005280116166595961481, 0.006336139399915151522, 0.008448185866553530737 ),
 .UNSPECIFIED. ) ;
#27325 = CARTESIAN_POINT ( 'NONE',  ( -27.08423923533013422, 2.107995711831542884, 0.8983804370399492978 ) ) ;
#27326 = CARTESIAN_POINT ( 'NONE',  ( -22.27384469013076185, 3.358914544760244869, 1.508555848190732851 ) ) ;
#27327 = FACE_OUTER_BOUND ( 'NONE', #37046, .T. ) ;
#27328 = ADVANCED_FACE ( 'NONE', ( #59948 ), #14536, .F. ) ;
#27329 = EDGE_LOOP ( 'NONE', ( #8409, #2683, #8625, #16030 ) ) ;
#27330 = CARTESIAN_POINT ( 'NONE',  ( 37.00000000000000711, -11.68758509253247091, 1.171570255487570655 ) ) ;
#27331 = EDGE_CURVE ( 'NONE', #8685, #9789, #38677, .T. ) ;
#27332 = EDGE_CURVE ( 'NONE', #59842, #1422, #8094, .T. ) ;
#27333 = DIRECTION ( 'NONE',  ( -1.000000000000000000, 0.000000000000000000, 0.000000000000000000 ) ) ;
#27334 = CARTESIAN_POINT ( 'NONE',  ( -35.00000000000000000, 10.80478261802190154, -5.636262487437199376 ) ) ;
#27335 = ADVANCED_FACE ( 'NONE', ( #23724 ), #23377, .T. ) ;
#27336 = CARTESIAN_POINT ( 'NONE',  ( 3.291290029914074378, 8.250315036047103590, 10.68561190601527855 ) ) ;
#27337 = DIRECTION ( 'NONE',  ( -1.000000000000000000, 0.000000000000000000, 0.000000000000000000 ) ) ;
#27338 = DIRECTION ( 'NONE',  ( 0.000000000000000000, 0.01356324068817991828, -0.9999080150203990547 ) ) ;
#27339 = DIRECTION ( 'NONE',  ( -1.000000000000000000, -0.000000000000000000, 0.000000000000000000 ) ) ;
#27340 = CARTESIAN_POINT ( 'NONE',  ( -22.29018399051993526, -2.675685774027730002, -2.585196332786389384 ) ) ;
#27341 = AXIS2_PLACEMENT_3D ( 'NONE', #51936, #6378, #46939 ) ;
#27342 = ORIENTED_EDGE ( 'NONE', *, *, #64378, .T. ) ;
#27343 = CARTESIAN_POINT ( 'NONE',  ( -22.94572469358971389, 2.078200699019463915, 4.424217216616495030 ) ) ;
#27344 = DIRECTION ( 'NONE',  ( 0.000000000000000000, -0.01356324068817992175, 0.9999080150203990547 ) ) ;
#27345 = CIRCLE ( 'NONE', #18871, 12.18649999999999878 ) ;
#27346 = ORIENTED_EDGE ( 'NONE', *, *, #206, .T. ) ;
#27347 = CARTESIAN_POINT ( 'NONE',  ( -22.27719443589224113, -3.601617131804399907, 0.7635131876695111508 ) ) ;
#27348 = DIRECTION ( 'NONE',  ( 0.000000000000000000, 0.01356324068817998940, -0.9999080150203990547 ) ) ;
#27349 = ORIENTED_EDGE ( 'NONE', *, *, #27240, .T. ) ;
#27350 = CARTESIAN_POINT ( 'NONE',  ( 36.00000000000000711, -0.6593684648219547695, 12.73293890771483561 ) ) ;
#27351 = ORIENTED_EDGE ( 'NONE', *, *, #24074, .F. ) ;
#27352 = DIRECTION ( 'NONE',  ( 0.2180658516479614395, -0.9759340573753174652, 0.000000000000000000 ) ) ;
#27353 = VERTEX_POINT ( 'NONE', #44965 ) ;
#27354 = VECTOR ( 'NONE', #57685, 1000.000000000000000 ) ;
#27355 = EDGE_LOOP ( 'NONE', ( #45422, #25327, #53971, #43044 ) ) ;
#27357 = EDGE_CURVE ( 'NONE', #61328, #26747, #58509, .T. ) ;
#27356 = DIRECTION ( 'NONE',  ( -1.000000000000000000, -1.836970198721029688E-16, 0.000000000000000000 ) ) ;
#27358 = AXIS2_PLACEMENT_3D ( 'NONE', #43322, #32671, #48354 ) ;
#27359 = ORIENTED_EDGE ( 'NONE', *, *, #33573, .F. ) ;
#27360 = CARTESIAN_POINT ( 'NONE',  ( -35.00000000000000000, 0.000000000000000000, 0.000000000000000000 ) ) ;
#27361 = CYLINDRICAL_SURFACE ( 'NONE', #8121, 13.50000000000000178 ) ;
#27362 = CARTESIAN_POINT ( 'NONE',  ( 37.00000000000000711, -3.614449339633571512, -11.17622378668005290 ) ) ;
#27363 = CYLINDRICAL_SURFACE ( 'NONE', #56655, 4.785769192180104881 ) ;
#27364 = VERTEX_POINT ( 'NONE', #49336 ) ;
#27365 =( BOUNDED_SURFACE ( )  B_SPLINE_SURFACE ( 3, 1, ( 
 ( #48232, #18283 ),
 ( #59817, #53191 ),
 ( #12948, #48865 ),
 ( #33565, #33876 ) ),
 .UNSPECIFIED., .F., .F., .F. ) 
 B_SPLINE_SURFACE_WITH_KNOTS ( ( 4, 4 ),
 ( 2, 2 ),
 ( 0.000000000000000000, 1.000000000000000000 ),
 ( 0.000000000000000000, 1.000000000000000000 ),
 .UNSPECIFIED. ) 
 GEOMETRIC_REPRESENTATION_ITEM ( )  RATIONAL_B_SPLINE_SURFACE ( (
 ( 1.000000000000000000, 1.000000000000000000),
 ( 0.9932032654565553509, 0.8386279382598740284),
 ( 0.9932032654565553509, 0.8386279382598740284),
 ( 1.000000000000000000, 1.000000000000000000) ) ) 
 REPRESENTATION_ITEM ( '' )  SURFACE ( )  );
#27366 = CARTESIAN_POINT ( 'NONE',  ( 0.2958664285830415186, -7.708042451272235418, 9.529149585189916394 ) ) ;
#27367 = CARTESIAN_POINT ( 'NONE',  ( 10.57252189908326301, -33.12087690403964046, 11.56547414815872088 ) ) ;
#27368 = DIRECTION ( 'NONE',  ( -1.000000000000000000, 0.000000000000000000, 0.000000000000000000 ) ) ;
#27370 = VERTEX_POINT ( 'NONE', #24347 ) ;
#27369 = CARTESIAN_POINT ( 'NONE',  ( -24.30804329714943535, 8.222810952426842235, 8.742709031936243491 ) ) ;
#27371 = CARTESIAN_POINT ( 'NONE',  ( 35.00000000000000000, -7.215058775251181444, 9.821084925794645315 ) ) ;
#27372 = EDGE_LOOP ( 'NONE', ( #60343, #28171, #31552, #45036 ) ) ;
#27373 = DIRECTION ( 'NONE',  ( 0.000000000000000000, 0.6478160128811948359, -0.7617968321374878338 ) ) ;
#27374 = EDGE_CURVE ( 'NONE', #35285, #57971, #8546, .T. ) ;
#27375 = ORIENTED_EDGE ( 'NONE', *, *, #58338, .T. ) ;
#27376 = DIRECTION ( 'NONE',  ( 0.000000000000000000, 0.01356324068817992522, -0.9999080150203990547 ) ) ;
#27377 = CARTESIAN_POINT ( 'NONE',  ( 2.251139882113957658, -7.636654603229077409, -0.1241612276497447015 ) ) ;
#27378 = B_SPLINE_CURVE_WITH_KNOTS ( 'NONE', 3,
 ( #8456, #37396, #52713, #38383, #57706, #32401, #53024, #43698, #23096, #12127 ),
 .UNSPECIFIED., .F., .F.,
 ( 4, 3, 3, 4 ),
 ( 5.401523115762941855E-05, 0.0008136511341527816361, 0.004068255670953097557, 0.005063778443040919605 ),
 .UNSPECIFIED. ) ;
#27379 = VERTEX_POINT ( 'NONE', #44300 ) ;
#27380 = DIRECTION ( 'NONE',  ( 0.000000000000000000, 0.01356324068817991828, -0.9999080150203990547 ) ) ;
#27381 = EDGE_CURVE ( 'NONE', #22857, #28767, #45719, .T. ) ;
#27382 = CARTESIAN_POINT ( 'NONE',  ( 0.3675815128205894289, -6.367184624550092487, -10.50067073900658521 ) ) ;
#27383 = CARTESIAN_POINT ( 'NONE',  ( 12.96254931691228940, 11.37456213158350060, -7.274141147047163081 ) ) ;
#27384 = B_SPLINE_CURVE_WITH_KNOTS ( 'NONE', 3,
 ( #11250, #51513, #12534, #58120, #31520, #1619, #62120 ),
 .UNSPECIFIED., .F., .F.,
 ( 4, 3, 4 ),
 ( 5.504479493880105401E-15, 0.002398160485434731350, 0.005002426799382268634 ),
 .UNSPECIFIED. ) ;
#27385 = VERTEX_POINT ( 'NONE', #44612 ) ;
#27386 = ORIENTED_EDGE ( 'NONE', *, *, #27955, .F. ) ;
#27387 = CARTESIAN_POINT ( 'NONE',  ( 2.835339799623982415, 7.649567297875990768, 1.682641786445466803 ) ) ;
#27388 = ORIENTED_EDGE ( 'NONE', *, *, #13403, .T. ) ;
#27389 = EDGE_CURVE ( 'NONE', #19030, #60178, #53968, .T. ) ;
#27390 = ORIENTED_EDGE ( 'NONE', *, *, #60266, .F. ) ;
#27391 = CARTESIAN_POINT ( 'NONE',  ( -37.00000000000000711, -9.063649021439015740, 8.146229107149364879 ) ) ;
#27392 = CARTESIAN_POINT ( 'NONE',  ( -17.72422596690857688, -11.73861005525308343, 2.575547964227135278 ) ) ;
#27393 = DIRECTION ( 'NONE',  ( -0.3865475372811021937, -0.5778504531711091685, 0.7187975063895662986 ) ) ;
#27394 = CYLINDRICAL_SURFACE ( 'NONE', #50113, 12.75000000000000178 ) ;
#27395 = CARTESIAN_POINT ( 'NONE',  ( 47.00000000000000711, 4.705694406421931860E-17, -3.469127814946512892E-15 ) ) ;
#27396 = AXIS2_PLACEMENT_3D ( 'NONE', #14296, #60504, #50554 ) ;
#27397 = LINE ( 'NONE', #37717, #38416 ) ;
#27398 = CARTESIAN_POINT ( 'NONE',  ( -22.27720412283625961, -0.7407051501189847453, -3.606406551442380870 ) ) ;
#27399 = AXIS2_PLACEMENT_3D ( 'NONE', #27330, #12361, #32963 ) ;
#27400 = ORIENTED_EDGE ( 'NONE', *, *, #33411, .T. ) ;
#27401 = LINE ( 'NONE', #2143, #28177 ) ;
#27402 = VECTOR ( 'NONE', #60683, 1000.000000000000114 ) ;
#27403 = CARTESIAN_POINT ( 'NONE',  ( -22.31328051695926007, -3.148362328073157190, 2.109671368890621679 ) ) ;
#27404 = CIRCLE ( 'NONE', #41218, 12.75000000000000178 ) ;
#27405 = EDGE_CURVE ( 'NONE', #39189, #12727, #39969, .T. ) ;
#27406 = CARTESIAN_POINT ( 'NONE',  ( -35.04582288351658548, -0.0001464581945162154444, -0.01270482153516100908 ) ) ;
#27407 = CARTESIAN_POINT ( 'NONE',  ( -27.19357181888462094, 12.48377454417557253, 5.138615876886901468 ) ) ;
#27408 = B_SPLINE_CURVE_WITH_KNOTS ( 'NONE', 3,
 ( #51258, #40599, #35273, #19685, #10020, #35913, #44932 ),
 .UNSPECIFIED., .F., .F.,
 ( 4, 3, 4 ),
 ( 4.941165900048787626E-15, 0.002398160485434632904, 0.005002426799381740410 ),
 .UNSPECIFIED. ) ;
#27409 = FACE_OUTER_BOUND ( 'NONE', #1122, .T. ) ;
#27410 = EDGE_CURVE ( 'NONE', #28290, #50412, #43613, .T. ) ;
#27411 = ADVANCED_FACE ( 'NONE', ( #59285 ), #33993, .T. ) ;
#27412 = CARTESIAN_POINT ( 'NONE',  ( 9.373266352144048241, 2.643534358090585457, -11.70720285747480460 ) ) ;
#27413 = ORIENTED_EDGE ( 'NONE', *, *, #12459, .T. ) ;
#27414 = DIRECTION ( 'NONE',  ( 0.000000000000000000, 0.1387779952735747335, -0.9903235168508560671 ) ) ;
#27415 = FACE_OUTER_BOUND ( 'NONE', #13541, .T. ) ;
#27416 = DIRECTION ( 'NONE',  ( 0.000000000000000000, 0.01356324068817998940, -0.9999080150203990547 ) ) ;
#27417 = CARTESIAN_POINT ( 'NONE',  ( 0.000000000000000000, -5.769711778877344877, 4.791703871138500936 ) ) ;
#27418 = CARTESIAN_POINT ( 'NONE',  ( 32.00000000000000000, 12.00000000000000000, 1.469576158976823553E-15 ) ) ;
#27419 = FACE_OUTER_BOUND ( 'NONE', #27861, .T. ) ;
#27420 = EDGE_LOOP ( 'NONE', ( #3088, #19304, #46431, #28055 ) ) ;
#27421 = AXIS2_PLACEMENT_3D ( 'NONE', #23477, #44387, #3553 ) ;
#27422 = CARTESIAN_POINT ( 'NONE',  ( -37.00000000000000711, 9.060822531526156354, -7.474872387600913548 ) ) ;
#27423 = CARTESIAN_POINT ( 'NONE',  ( -27.01437459610461644, -10.69338818478079922, -8.240233560378637634 ) ) ;
#27424 = DIRECTION ( 'NONE',  ( 0.000000000000000000, 0.000000000000000000, 1.000000000000000000 ) ) ;
#27425 = DIRECTION ( 'NONE',  ( -1.000000000000000000, 0.000000000000000000, 0.000000000000000000 ) ) ;
#27426 = ORIENTED_EDGE ( 'NONE', *, *, #57069, .F. ) ;
#27427 = LINE ( 'NONE', #22448, #41461 ) ;
#27428 = CARTESIAN_POINT ( 'NONE',  ( -36.00000000000000711, 4.400442035671114027, -11.96656215839364457 ) ) ;
#27429 = VERTEX_POINT ( 'NONE', #54937 ) ;
#27430 = ORIENTED_EDGE ( 'NONE', *, *, #23005, .F. ) ;
#27431 = CARTESIAN_POINT ( 'NONE',  ( 36.00000000000000711, 3.033604067594577902, -12.38385022362083454 ) ) ;
#27432 = EDGE_CURVE ( 'NONE', #49077, #10832, #9367, .T. ) ;
#27433 = CARTESIAN_POINT ( 'NONE',  ( 35.00000000000000000, 9.348667969174517367, 7.817492529713752525 ) ) ;
#27434 = VERTEX_POINT ( 'NONE', #45291 ) ;
#27435 = CARTESIAN_POINT ( 'NONE',  ( 0.000000000000000000, -5.814643797626899868, -3.550179297009637747 ) ) ;
#27436 = EDGE_CURVE ( 'NONE', #27036, #43191, #29538, .T. ) ;
#27437 = CARTESIAN_POINT ( 'NONE',  ( 35.00000000000000000, -9.512294188640847636, 6.891188680298922620 ) ) ;
#27438 = CIRCLE ( 'NONE', #869, 2.899999999999993694 ) ;
#27439 = CYLINDRICAL_SURFACE ( 'NONE', #40736, 7.499999999999988454 ) ;
#27440 = CARTESIAN_POINT ( 'NONE',  ( -27.35552965826135008, 3.094132632038936404, 0.2619431035391969198 ) ) ;
#27441 = CARTESIAN_POINT ( 'NONE',  ( -9.829859729628957155, 10.62238046397816582, -5.599206581597568899 ) ) ;
#27442 = CARTESIAN_POINT ( 'NONE',  ( 0.3675815128205894289, 5.910255304480445560, 10.76447900494942367 ) ) ;
#27444 = VERTEX_POINT ( 'NONE', #31546 ) ;
#27443 = CYLINDRICAL_SURFACE ( 'NONE', #46808, 7.499999999999988454 ) ;
#27445 = VECTOR ( 'NONE', #31258, 1000.000000000000000 ) ;
#27446 = CYLINDRICAL_SURFACE ( 'NONE', #33045, 2.899999999999994582 ) ;
#27447 = ORIENTED_EDGE ( 'NONE', *, *, #54296, .T. ) ;
#27448 = CARTESIAN_POINT ( 'NONE',  ( 2.241534463349551753, 9.451863027432619807E-16, 7.634462073473348376 ) ) ;
#27449 = VERTEX_POINT ( 'NONE', #22224 ) ;
#27450 = EDGE_CURVE ( 'NONE', #54224, #27125, #50045, .T. ) ;
#27451 = CIRCLE ( 'NONE', #36987, 12.74999999999999822 ) ;
#27452 = CARTESIAN_POINT ( 'NONE',  ( -35.00000000000000000, 11.37311665002359540, 2.936739658820077370 ) ) ;
#27453 = CARTESIAN_POINT ( 'NONE',  ( 2.665405856346791946, -5.696318245876772934, -7.686816759402922195 ) ) ;
#27454 = DIRECTION ( 'NONE',  ( -1.000000000000000000, 0.000000000000000000, -0.000000000000000000 ) ) ;
#27455 = CARTESIAN_POINT ( 'NONE',  ( 36.00000000000000711, 5.300372733891643762, -11.59605747147788790 ) ) ;
#27456 = CARTESIAN_POINT ( 'NONE',  ( -25.00000000000000355, -30.00000000000000000, 25.00000000000000000 ) ) ;
#27457 = ORIENTED_EDGE ( 'NONE', *, *, #17642, .F. ) ;
#27458 = CARTESIAN_POINT ( 'NONE',  ( -24.29708947709745104, -8.221392171298289142, 8.752766005952057782 ) ) ;
#27459 = LINE ( 'NONE', #2883, #11724 ) ;
#27460 = ORIENTED_EDGE ( 'NONE', *, *, #28990, .T. ) ;
#27461 = ORIENTED_EDGE ( 'NONE', *, *, #50558, .F. ) ;
#27462 = DIRECTION ( 'NONE',  ( 0.000000000000000000, -0.2149704402110114709, -0.9766205557100894330 ) ) ;
#27463 = EDGE_CURVE ( 'NONE', #16604, #31565, #11307, .T. ) ;
#27464 = ORIENTED_EDGE ( 'NONE', *, *, #32386, .T. ) ;
#27465 = CARTESIAN_POINT ( 'NONE',  ( 2.241509619876138171, 1.363398699156149307, -7.511759925807389493 ) ) ;
#27466 = CARTESIAN_POINT ( 'NONE',  ( -10.90165637463001680, -7.936842980705543837, 9.017060805754692154 ) ) ;
#27467 = CARTESIAN_POINT ( 'NONE',  ( -35.00000000000000000, -7.376655759824951808, 9.700295462048636352 ) ) ;
#27468 = EDGE_CURVE ( 'NONE', #21918, #35321, #64872, .T. ) ;
#27469 = CARTESIAN_POINT ( 'NONE',  ( -27.08954555554372590, 0.9924303381770641641, -2.082904663687288771 ) ) ;
#27470 = CARTESIAN_POINT ( 'NONE',  ( 2.000000000000001776, -4.962980376314093611, 4.846014654777763830 ) ) ;
#27471 = CARTESIAN_POINT ( 'NONE',  ( -27.08430418657511751, -1.863523114788417701, 1.333569526608693767 ) ) ;
#27472 = AXIS2_PLACEMENT_3D ( 'NONE', #34603, #8052, #4037 ) ;
#27473 = CARTESIAN_POINT ( 'NONE',  ( 2.241311220309555097, 7.501736494813745715, 1.417008678104511255 ) ) ;
#27474 = ORIENTED_EDGE ( 'NONE', *, *, #50707, .F. ) ;
#27475 = DIRECTION ( 'NONE',  ( -0.000000000000000000, -0.000000000000000000, -1.000000000000000000 ) ) ;
#27476 = CIRCLE ( 'NONE', #31733, 7.499999999999988454 ) ;
#27477 = VERTEX_POINT ( 'NONE', #50304 ) ;
#27478 = CARTESIAN_POINT ( 'NONE',  ( 0.2648978790185593790, -6.237101853238620208, 10.53870023327861283 ) ) ;
#27479 = DIRECTION ( 'NONE',  ( -1.000000000000000000, -0.000000000000000000, -0.000000000000000000 ) ) ;
#27480 = CARTESIAN_POINT ( 'NONE',  ( 2.305787727787083519, -2.774453000917102230, -7.135468203930011910 ) ) ;
#27481 = CYLINDRICAL_SURFACE ( 'NONE', #9634, 5.000000000000000888 ) ;
#27482 = ADVANCED_FACE ( 'NONE', ( #11277 ), #46848, .T. ) ;
#27483 = VECTOR ( 'NONE', #54855, 1000.000000000000000 ) ;
#27484 = ORIENTED_EDGE ( 'NONE', *, *, #8280, .T. ) ;
#27485 = ORIENTED_EDGE ( 'NONE', *, *, #18034, .F. ) ;
#27486 = CARTESIAN_POINT ( 'NONE',  ( -27.10719052120871098, 0.1538293304135379680, 2.355164825213503121 ) ) ;
#27487 = EDGE_CURVE ( 'NONE', #56112, #19566, #20277, .T. ) ;
#27488 = AXIS2_PLACEMENT_3D ( 'NONE', #1364, #10330, #61522 ) ;
#27489 = VERTEX_POINT ( 'NONE', #1313 ) ;
#27490 = DIRECTION ( 'NONE',  ( -1.000000000000000000, 0.000000000000000000, 0.000000000000000000 ) ) ;
#27491 = CARTESIAN_POINT ( 'NONE',  ( 36.00000000000000711, -6.711949091238069265, 10.84030624090613237 ) ) ;
#27493 = EDGE_CURVE ( 'NONE', #50042, #58893, #19239, .T. ) ;
#27492 = AXIS2_PLACEMENT_3D ( 'NONE', #598, #11528, #30814 ) ;
#27494 = CARTESIAN_POINT ( 'NONE',  ( 1.014383007554947813, -9.851867765302131374, -7.686901933424256761 ) ) ;
#27495 = CARTESIAN_POINT ( 'NONE',  ( 3.031336079629759261, -5.388626255827020373, -5.773872239512848559 ) ) ;
#27496 = ORIENTED_EDGE ( 'NONE', *, *, #63483, .F. ) ;
#27497 = CARTESIAN_POINT ( 'NONE',  ( 3.152665057734128862, 2.258875078502223133, 7.609997527621164437 ) ) ;
#27498 = CARTESIAN_POINT ( 'NONE',  ( -26.74023318801844340, -0.2829279580741936306, 3.342010596062582106 ) ) ;
#27499 = CARTESIAN_POINT ( 'NONE',  ( 0.2650492594609232810, -10.54996119777441344, -6.218173512054875118 ) ) ;
#27500 = AXIS2_PLACEMENT_3D ( 'NONE', #25444, #30110, #9474 ) ;
#27501 = CARTESIAN_POINT ( 'NONE',  ( -25.00000000000000355, -3.797884998337192286, 24.99999999999999289 ) ) ;
#27502 = DIRECTION ( 'NONE',  ( 1.000000000000000000, 0.000000000000000000, -0.000000000000000000 ) ) ;
#27503 = DIRECTION ( 'NONE',  ( -1.000000000000000000, 0.000000000000000000, 0.000000000000000000 ) ) ;
#27504 = EDGE_LOOP ( 'NONE', ( #40861, #22581, #9579, #54000 ) ) ;
#27505 = CARTESIAN_POINT ( 'NONE',  ( 35.00000000000000000, 11.35427606708806003, -4.426194442447284771 ) ) ;
#27506 = ORIENTED_EDGE ( 'NONE', *, *, #59935, .T. ) ;
#27507 = CARTESIAN_POINT ( 'NONE',  ( -37.00000000000000711, -8.551552972817024312, -8.052525312709976291 ) ) ;
#27508 = CYLINDRICAL_SURFACE ( 'NONE', #16144, 2.899999999999994582 ) ;
#27509 = DIRECTION ( 'NONE',  ( -1.000000000000000000, 0.000000000000000000, 0.000000000000000000 ) ) ;
#27510 = FACE_OUTER_BOUND ( 'NONE', #31379, .T. ) ;
#27511 = FACE_OUTER_BOUND ( 'NONE', #7050, .T. ) ;
#27512 = VECTOR ( 'NONE', #60131, 1000.000000000000000 ) ;
#27513 = EDGE_LOOP ( 'NONE', ( #32045, #30508, #42657, #60143 ) ) ;
#27514 = EDGE_LOOP ( 'NONE', ( #58099, #32818, #2092, #54794, #61015, #30485 ) ) ;
#27515 = CARTESIAN_POINT ( 'NONE',  ( 5.520433897694421610, 0.002108682515300278320, 0.01491416502703811486 ) ) ;
#27516 = ORIENTED_EDGE ( 'NONE', *, *, #56579, .F. ) ;
#27517 = ADVANCED_FACE ( 'NONE', ( #31861 ), #6295, .T. ) ;
#27518 = CARTESIAN_POINT ( 'NONE',  ( 3.460083169609886156, 6.940591624561522011, 9.798413085330784256 ) ) ;
#27519 = DIRECTION ( 'NONE',  ( -1.000000000000000000, 0.000000000000000000, 0.000000000000000000 ) ) ;
#27520 = DIRECTION ( 'NONE',  ( 1.000000000000000000, 0.000000000000000000, -0.000000000000000000 ) ) ;
#27521 = CARTESIAN_POINT ( 'NONE',  ( 2.241534463349552198, -1.511811348926356884E-18, -7.634462073473343935 ) ) ;
#27523 = LINE ( 'NONE', #41499, #20499 ) ;
#27522 = AXIS2_PLACEMENT_3D ( 'NONE', #16687, #37292, #52290 ) ;
#27524 = B_SPLINE_CURVE_WITH_KNOTS ( 'NONE', 3,
 ( #55825, #60466, #15245, #35183, #49848, #10573, #30853, #9580, #65447, #61136, #30219, #51173, #44852 ),
 .UNSPECIFIED., .F., .F.,
 ( 4, 3, 3, 3, 4 ),
 ( 2.737610485525898696E-18, 6.607593386745464631E-05, 0.0001321518677373517562, 0.0001982171734706201821, 0.0002642860854759486629 ),
 .UNSPECIFIED. ) ;
#27525 = CARTESIAN_POINT ( 'NONE',  ( 2.273267844204866606, 7.553702825375864904, 1.178226273332969365 ) ) ;
#27526 = CARTESIAN_POINT ( 'NONE',  ( 0.3675815128205912052, 12.13672785388552811, -1.872154644481959895 ) ) ;
#27527 = ORIENTED_EDGE ( 'NONE', *, *, #24522, .T. ) ;
#27528 = VERTEX_POINT ( 'NONE', #11591 ) ;
#27529 = DIRECTION ( 'NONE',  ( 0.000000000000000000, 0.000000000000000000, 1.000000000000000000 ) ) ;
#27530 = VERTEX_POINT ( 'NONE', #6628 ) ;
#27531 = SURFACE_STYLE_USAGE ( .BOTH. , #7247 ) ;
#27532 = LINE ( 'NONE', #21235, #50391 ) ;
#27533 = AXIS2_PLACEMENT_3D ( 'NONE', #40780, #31758, #21132 ) ;
#27534 = CARTESIAN_POINT ( 'NONE',  ( 17.00164331164202736, 11.45151090621293122, 7.188808658307459076 ) ) ;
#27535 = EDGE_CURVE ( 'NONE', #20211, #62601, #63789, .T. ) ;
#27536 = DIRECTION ( 'NONE',  ( 1.000000000000000000, 0.000000000000000000, -0.000000000000000000 ) ) ;
#27538 = VERTEX_POINT ( 'NONE', #21912 ) ;
#27537 = AXIS2_PLACEMENT_3D ( 'NONE', #1848, #26449, #12138 ) ;
#27539 = CARTESIAN_POINT ( 'NONE',  ( 24.82652845881425208, 25.00000000000000000, -8.578654028722157321 ) ) ;
#27540 = DIRECTION ( 'NONE',  ( -0.2475719085175094869, 0.000000000000000000, -0.9688695217174488894 ) ) ;
#27541 = CARTESIAN_POINT ( 'NONE',  ( -35.04643116707788408, 0.009511118309135299653, -0.007621814750509436909 ) ) ;
#27542 = ORIENTED_EDGE ( 'NONE', *, *, #14689, .T. ) ;
#27543 = VERTEX_POINT ( 'NONE', #42162 ) ;
#27544 = DIRECTION ( 'NONE',  ( -0.000000000000000000, -0.000000000000000000, -1.000000000000000000 ) ) ;
#27545 = ORIENTED_EDGE ( 'NONE', *, *, #35585, .T. ) ;
#27546 = ADVANCED_FACE ( 'NONE', ( #62449 ), #42831, .T. ) ;
#27547 = VERTEX_POINT ( 'NONE', #43823 ) ;
#27548 = DIRECTION ( 'NONE',  ( 0.000000000000000000, -0.8276889981568955612, 0.5611870653623749483 ) ) ;
#27549 = VERTEX_POINT ( 'NONE', #59135 ) ;
#27550 = VECTOR ( 'NONE', #60837, 1000.000000000000000 ) ;
#27551 = EDGE_LOOP ( 'NONE', ( #47513, #11864, #55351, #27995 ) ) ;
#27552 = DIRECTION ( 'NONE',  ( 1.000000000000000000, 0.000000000000000000, 0.000000000000000000 ) ) ;
#27553 = EDGE_CURVE ( 'NONE', #44784, #50728, #23552, .T. ) ;
#27554 = DIRECTION ( 'NONE',  ( -1.000000000000000000, 0.000000000000000000, 0.000000000000000000 ) ) ;
#27555 = FACE_OUTER_BOUND ( 'NONE', #53671, .T. ) ;
#27556 = CARTESIAN_POINT ( 'NONE',  ( 16.66082797316812503, -33.00000000000000000, -4.257284274447485473 ) ) ;
#27557 = LINE ( 'NONE', #63140, #30238 ) ;
#27558 = VECTOR ( 'NONE', #25276, 1000.000000000000000 ) ;
#27559 = CARTESIAN_POINT ( 'NONE',  ( -22.38932658256920050, -3.587092141214311525, -1.810630688302303559 ) ) ;
#27560 =( BOUNDED_SURFACE ( )  B_SPLINE_SURFACE ( 3, 1, ( 
 ( #15414, #49392 ),
 ( #25075, #39366 ),
 ( #45343, #126 ),
 ( #59669, #65606 ) ),
 .UNSPECIFIED., .F., .F., .F. ) 
 B_SPLINE_SURFACE_WITH_KNOTS ( ( 4, 4 ),
 ( 2, 2 ),
 ( 0.000000000000000000, 1.000000000000000000 ),
 ( 0.000000000000000000, 1.000000000000000000 ),
 .UNSPECIFIED. ) 
 GEOMETRIC_REPRESENTATION_ITEM ( )  RATIONAL_B_SPLINE_SURFACE ( (
 ( 1.000000000000000000, 1.000000000000000000),
 ( 0.9932032654565553509, 0.8386279382598740284),
 ( 0.9932032654565553509, 0.8386279382598740284),
 ( 1.000000000000000000, 1.000000000000000000) ) ) 
 REPRESENTATION_ITEM ( '' )  SURFACE ( )  );
#27561 = ORIENTED_EDGE ( 'NONE', *, *, #4540, .T. ) ;
#27562 = CARTESIAN_POINT ( 'NONE',  ( -36.00000000000000711, 2.250029553613936528, -12.54989509947648685 ) ) ;
#27563 = CARTESIAN_POINT ( 'NONE',  ( -22.27721038036499834, 2.858424446490944959, -2.320305412324239036 ) ) ;
#27564 = CYLINDRICAL_SURFACE ( 'NONE', #52309, 7.499999999999988454 ) ;
#27565 = CARTESIAN_POINT ( 'NONE',  ( 0.3106921474978454611, -2.360654586927870557, 12.03191800497307717 ) ) ;
#27566 = DIRECTION ( 'NONE',  ( 1.000000000000000000, 0.000000000000000000, 0.000000000000000000 ) ) ;
#27567 = CARTESIAN_POINT ( 'NONE',  ( -37.00000000000000711, 11.59605747147786836, 5.300372733891681953 ) ) ;
#27568 = EDGE_CURVE ( 'NONE', #56972, #31853, #33829, .T. ) ;
#27569 = AXIS2_PLACEMENT_3D ( 'NONE', #15866, #41467, #51807 ) ;
#27570 = ORIENTED_EDGE ( 'NONE', *, *, #32455, .T. ) ;
#27571 = DIRECTION ( 'NONE',  ( -1.000000000000000000, 0.000000000000000000, 0.000000000000000000 ) ) ;
#27572 = B_SPLINE_CURVE_WITH_KNOTS ( 'NONE', 3,
 ( #25176, #60762, #8909, #29198, #35479, #60105, #14523, #29501, #9216, #55443, #50473, #49804, #4252, #65081, #29826, #19554 ),
 .UNSPECIFIED., .F., .F.,
 ( 4, 3, 3, 3, 3, 4 ),
 ( 0.000000000000000000, 0.0002176109881720242410, 0.0004352086762394595824, 0.0006528017811446875079, 0.0007615147961451692411, 0.0009453342004945818056 ),
 .UNSPECIFIED. ) ;
#27573 = ORIENTED_EDGE ( 'NONE', *, *, #45736, .T. ) ;
#27574 = CARTESIAN_POINT ( 'NONE',  ( -25.00000000000000355, -30.00000000000000000, -25.00000000000000000 ) ) ;
#27575 = CARTESIAN_POINT ( 'NONE',  ( 2.253265082352431836, 5.932955906470575691, -4.810902415501073115 ) ) ;
#27576 = CARTESIAN_POINT ( 'NONE',  ( 0.000000000000000000, -1.956810415765137368, -6.654767106875573823 ) ) ;
#27577 = LINE ( 'NONE', #41895, #64877 ) ;
#27578 = CARTESIAN_POINT ( 'NONE',  ( 2.368238019614957501, 7.589221137922601557, 1.155661230551840113 ) ) ;
#27579 = ORIENTED_EDGE ( 'NONE', *, *, #35490, .F. ) ;
#27580 = DIRECTION ( 'NONE',  ( 1.000000000000000000, 0.000000000000000000, 0.000000000000000000 ) ) ;
#27581 = CARTESIAN_POINT ( 'NONE',  ( 1.719304012338199517, 0.000000000000000000, 0.000000000000000000 ) ) ;
#27582 = FACE_OUTER_BOUND ( 'NONE', #31709, .T. ) ;
#27583 = CARTESIAN_POINT ( 'NONE',  ( -2.952869152607107139, 12.96714474214482138, 3.755417052241487585 ) ) ;
#27584 = EDGE_CURVE ( 'NONE', #65451, #33526, #23215, .T. ) ;
#27585 = AXIS2_PLACEMENT_3D ( 'NONE', #9945, #30227, #18945 ) ;
#27586 = DIRECTION ( 'NONE',  ( -1.000000000000000000, 0.000000000000000000, 0.000000000000000000 ) ) ;
#27587 = EDGE_LOOP ( 'NONE', ( #4833, #15750, #37825, #42163 ) ) ;
#27588 = CARTESIAN_POINT ( 'NONE',  ( 0.2646305136544072623, -9.296005949277279967, 7.972778379581522579 ) ) ;
#27589 = CARTESIAN_POINT ( 'NONE',  ( -2.311295102010213931, -30.63172828985172202, 15.19685615870658602 ) ) ;
#27590 = CIRCLE ( 'NONE', #18071, 12.75000000000000178 ) ;
#27591 = ORIENTED_EDGE ( 'NONE', *, *, #7516, .F. ) ;
#27592 = DIRECTION ( 'NONE',  ( 1.000000000000000000, 0.000000000000000000, 0.000000000000000000 ) ) ;
#27594 = ORIENTED_EDGE ( 'NONE', *, *, #57543, .F. ) ;
#27593 = EDGE_CURVE ( 'NONE', #59964, #34255, #17606, .T. ) ;
#27595 = CARTESIAN_POINT ( 'NONE',  ( 26.34661844826604593, -13.08594712317289321, 3.317828791472332117 ) ) ;
#27596 = CARTESIAN_POINT ( 'NONE',  ( -35.00000000000000000, -11.44858830469742017, 2.627174906296871448 ) ) ;
#27597 = DIRECTION ( 'NONE',  ( 1.000000000000000000, 0.000000000000000000, 0.000000000000000000 ) ) ;
#27598 = DIRECTION ( 'NONE',  ( -1.000000000000000000, 0.000000000000000000, 0.000000000000000000 ) ) ;
#27599 = CARTESIAN_POINT ( 'NONE',  ( -22.30078715814471479, -2.097357782488222799, -3.111489293522219146 ) ) ;
#27600 = EDGE_CURVE ( 'NONE', #60515, #32661, #26686, .T. ) ;
#27601 = ORIENTED_EDGE ( 'NONE', *, *, #61536, .T. ) ;
#27602 = ORIENTED_EDGE ( 'NONE', *, *, #16913, .F. ) ;
#27603 = ORIENTED_EDGE ( 'NONE', *, *, #23547, .F. ) ;
#27604 = CARTESIAN_POINT ( 'NONE',  ( 2.262775599886256650, 7.227769107232081325, -2.480428346600461520 ) ) ;
#27606 = DIRECTION ( 'NONE',  ( 0.000000000000000000, 0.000000000000000000, -1.000000000000000000 ) ) ;
#27605 = VECTOR ( 'NONE', #20958, 1000.000000000000000 ) ;
#27607 = CIRCLE ( 'NONE', #64764, 12.18650000000000055 ) ;
#27608 = EDGE_CURVE ( 'NONE', #14035, #62269, #41529, .T. ) ;
#27609 = VERTEX_POINT ( 'NONE', #53148 ) ;
#27610 = DIRECTION ( 'NONE',  ( 0.000000000000000000, -0.3193015301359870550, 0.9476531711828000137 ) ) ;
#27611 = CARTESIAN_POINT ( 'NONE',  ( -37.00000000000000711, -10.75351884295731253, 4.725891942574718563 ) ) ;
#27612 = VERTEX_POINT ( 'NONE', #7595 ) ;
#27613 = CARTESIAN_POINT ( 'NONE',  ( -35.00000000000000000, 11.98254675519231682, -2.220215194441768514 ) ) ;
#27614 = DIRECTION ( 'NONE',  ( -1.000000000000000000, 0.000000000000000000, 0.000000000000000000 ) ) ;
#27615 = CARTESIAN_POINT ( 'NONE',  ( 2.284126774969132523, 7.131638985093474048, 2.764365694978749399 ) ) ;
#27616 = ORIENTED_EDGE ( 'NONE', *, *, #41255, .T. ) ;
#27617 = ORIENTED_EDGE ( 'NONE', *, *, #49473, .F. ) ;
#27618 = CARTESIAN_POINT ( 'NONE',  ( 0.3278977287071230817, 12.12129679591850540, -1.885359334311841772 ) ) ;
#27619 = VERTEX_POINT ( 'NONE', #43475 ) ;
#27620 = EDGE_CURVE ( 'NONE', #46658, #65174, #63834, .T. ) ;
#27621 = CARTESIAN_POINT ( 'NONE',  ( -18.63153057747156893, 11.99999999999999822, -0.3572518721000119690 ) ) ;
#27622 = VERTEX_POINT ( 'NONE', #22902 ) ;
#27623 = CARTESIAN_POINT ( 'NONE',  ( 2.259830038565000088, 3.700395974956140144, 6.684701880279339647 ) ) ;
#27624 = AXIS2_PLACEMENT_3D ( 'NONE', #33174, #27209, #2280 ) ;
#27625 = CARTESIAN_POINT ( 'NONE',  ( 15.96337567072090380, -34.98223374851986023, -4.998641903493608041 ) ) ;
#27626 = DIRECTION ( 'NONE',  ( 0.000000000000000000, -0.01356324068817998940, 0.9999080150203990547 ) ) ;
#27627 = CARTESIAN_POINT ( 'NONE',  ( -22.29570301036918778, 3.629130197778204003, 0.8918611685730862826 ) ) ;
#27628 = FACE_OUTER_BOUND ( 'NONE', #59354, .T. ) ;
#27629 = CARTESIAN_POINT ( 'NONE',  ( 5.516018279890452902, -0.003191189039764880282, -0.005976902763919027944 ) ) ;
#27630 = CARTESIAN_POINT ( 'NONE',  ( -35.00000000000000000, 0.000000000000000000, 0.000000000000000000 ) ) ;
#27631 = VERTEX_POINT ( 'NONE', #3275 ) ;
#27632 = VECTOR ( 'NONE', #27201, 1000.000000000000000 ) ;
#27633 = CARTESIAN_POINT ( 'NONE',  ( -35.05175862995318425, -0.001087818442123411611, -0.01253051761585834145 ) ) ;
#27634 = ORIENTED_EDGE ( 'NONE', *, *, #52766, .T. ) ;
#27635 = CARTESIAN_POINT ( 'NONE',  ( -22.31328051695926007, 3.685074213229321494, 0.8849444482787824917 ) ) ;
#27636 = DIRECTION ( 'NONE',  ( 1.000000000000000000, 0.000000000000000000, 0.000000000000000000 ) ) ;
#27637 = ORIENTED_EDGE ( 'NONE', *, *, #45519, .F. ) ;
#27638 = CARTESIAN_POINT ( 'NONE',  ( -17.18936361399038404, 7.855595644171634362, 9.071939927147207428 ) ) ;
#27639 = CARTESIAN_POINT ( 'NONE',  ( -35.00000000000000000, 10.39746860227890579, 7.379373053628905943 ) ) ;
#27640 = AXIS2_PLACEMENT_3D ( 'NONE', #43404, #33108, #53418 ) ;
#27641 = LINE ( 'NONE', #43939, #38665 ) ;
#27642 = VERTEX_POINT ( 'NONE', #43155 ) ;
#27643 = ORIENTED_EDGE ( 'NONE', *, *, #17818, .T. ) ;
#27644 = DIRECTION ( 'NONE',  ( -0.000000000000000000, -1.000000000000000000, -0.000000000000000000 ) ) ;
#27645 = AXIS2_PLACEMENT_3D ( 'NONE', #45446, #24515, #50779 ) ;
#27646 = EDGE_LOOP ( 'NONE', ( #24712, #59411, #52954, #54730 ) ) ;
#27647 = CARTESIAN_POINT ( 'NONE',  ( -37.00000000000000711, -0.1652884326465054177, 12.18537902504609072 ) ) ;
#27648 = CARTESIAN_POINT ( 'NONE',  ( -27.08423805673873375, 2.195702713475279122, 0.6554626340705826948 ) ) ;
#27650 = AXIS2_PLACEMENT_3D ( 'NONE', #4824, #45041, #15737 ) ;
#27649 = CARTESIAN_POINT ( 'NONE',  ( -3.496946155113953569, -10.55788327300660079, 8.446084379147929866 ) ) ;
#27651 = CARTESIAN_POINT ( 'NONE',  ( -37.00000000000000711, 11.61976888909158490, 3.827969819614504221 ) ) ;
#27652 = EDGE_LOOP ( 'NONE', ( #26345, #44301, #57745, #17021 ) ) ;
#27653 = CARTESIAN_POINT ( 'NONE',  ( 0.2648321136542706733, -12.03456865502704254, -2.265911310221937036 ) ) ;
#27654 = EDGE_CURVE ( 'NONE', #63728, #29225, #63754, .T. ) ;
#27655 = AXIS2_PLACEMENT_3D ( 'NONE', #17866, #27503, #47802 ) ;
#27656 = CARTESIAN_POINT ( 'NONE',  ( 2.899286259009685729, -7.664525129300148620, -1.713434346771303574 ) ) ;
#27657 = CARTESIAN_POINT ( 'NONE',  ( 35.00000000000000000, -2.346765782874354667, 11.95840593935203522 ) ) ;
#27658 = DIRECTION ( 'NONE',  ( -0.000000000000000000, -0.000000000000000000, -1.000000000000000000 ) ) ;
#27659 = CARTESIAN_POINT ( 'NONE',  ( -27.08416781016246588, -0.7680651426971742968, 2.158663327075677429 ) ) ;
#27660 = DIRECTION ( 'NONE',  ( 0.000000000000000000, 0.01356324068817992175, -0.9999080150203990547 ) ) ;
#27661 = CARTESIAN_POINT ( 'NONE',  ( 0.5547464869798223175, 4.506704303875454620, 11.49049644196204945 ) ) ;
#27662 = CARTESIAN_POINT ( 'NONE',  ( -35.00000000000000000, 1.262958560998759472, 12.12087942037210198 ) ) ;
#27663 = CIRCLE ( 'NONE', #64828, 6.936499999999992561 ) ;
#27664 = EDGE_CURVE ( 'NONE', #16920, #3974, #14938, .T. ) ;
#27665 = ORIENTED_EDGE ( 'NONE', *, *, #36555, .T. ) ;
#27666 = CARTESIAN_POINT ( 'NONE',  ( 2.259830038564998311, -0.1377140217659723054, 7.639319632525574555 ) ) ;
#27667 = DIRECTION ( 'NONE',  ( 0.000000000000000000, -0.01356324068817998940, 0.9999080150203990547 ) ) ;
#27668 = VECTOR ( 'NONE', #42774, 1000.000000000000000 ) ;
#27669 = AXIS2_PLACEMENT_3D ( 'NONE', #4086, #25337, #10362 ) ;
#27670 = ORIENTED_EDGE ( 'NONE', *, *, #51752, .F. ) ;
#27671 = EDGE_CURVE ( 'NONE', #35989, #34255, #18585, .T. ) ;
#27672 = CARTESIAN_POINT ( 'NONE',  ( -22.28776923226071460, 3.702096209084097644, -0.2883912626656479072 ) ) ;
#27673 = CARTESIAN_POINT ( 'NONE',  ( -22.65999102136916221, 3.858590659383648092, 2.911035239830945365 ) ) ;
#27674 = ORIENTED_EDGE ( 'NONE', *, *, #9270, .T. ) ;
#27675 = VECTOR ( 'NONE', #34820, 1000.000000000000000 ) ;
#27676 = UNCERTAINTY_MEASURE_WITH_UNIT (LENGTH_MEASURE( 1.000000000000000082E-05 ), #5383, 'distance_accuracy_value', 'NONE');
#27677 = CARTESIAN_POINT ( 'NONE',  ( -35.00000000000000000, -9.348667969174350389, -7.817492529713957694 ) ) ;
#27678 = EDGE_CURVE ( 'NONE', #49980, #4847, #1203, .T. ) ;
#27679 = ORIENTED_EDGE ( 'NONE', *, *, #43605, .F. ) ;
#27680 = VECTOR ( 'NONE', #2391, 999.9999999999998863 ) ;
#27681 = CARTESIAN_POINT ( 'NONE',  ( -35.00000000000000000, 5.636262487437317503, 10.80478261802183937 ) ) ;
#27682 = ORIENTED_EDGE ( 'NONE', *, *, #36009, .F. ) ;
#27683 = VERTEX_POINT ( 'NONE', #4585 ) ;
#27684 = CARTESIAN_POINT ( 'NONE',  ( 2.241317068080777020, -7.142175514530106462, 2.696905536171270601 ) ) ;
#27685 = EDGE_CURVE ( 'NONE', #39732, #54691, #14926, .T. ) ;
#27686 = VERTEX_POINT ( 'NONE', #39811 ) ;
#27687 = CARTESIAN_POINT ( 'NONE',  ( -24.97754535057679348, -7.227978708121235663, 9.585722579478227701 ) ) ;
#27688 = CARTESIAN_POINT ( 'NONE',  ( 145.1370849898475797, 3.309064568108273190E-14, 0.000000000000000000 ) ) ;
#27689 = CARTESIAN_POINT ( 'NONE',  ( 35.00000000000000000, 4.705694406421931860E-17, -3.469127814946512892E-15 ) ) ;
#27690 = CIRCLE ( 'NONE', #43640, 12.74999999999999822 ) ;
#27691 = CYLINDRICAL_SURFACE ( 'NONE', #46014, 12.75000000000000178 ) ;
#27692 = ORIENTED_EDGE ( 'NONE', *, *, #54524, .F. ) ;
#27693 = CARTESIAN_POINT ( 'NONE',  ( -14.47334165536099881, 0.000000000000000000, 4.000000000000000000 ) ) ;
#27694 = ADVANCED_FACE ( 'NONE', ( #29493 ), #4910, .T. ) ;
#27695 = CARTESIAN_POINT ( 'NONE',  ( 14.81496943876074290, -34.66917994667981162, 7.369609160621835464 ) ) ;
#27696 = CARTESIAN_POINT ( 'NONE',  ( 37.00000000000000711, 3.614449339633649227, 11.17622378668002092 ) ) ;
#27698 = ORIENTED_EDGE ( 'NONE', *, *, #46318, .F. ) ;
#27697 = CARTESIAN_POINT ( 'NONE',  ( -37.00000000000000711, 12.49688848680888142, -2.527899948230500460 ) ) ;
#27700 = CIRCLE ( 'NONE', #36185, 5.000000000000000000 ) ;
#27699 = FACE_OUTER_BOUND ( 'NONE', #11, .T. ) ;
#27701 = ORIENTED_EDGE ( 'NONE', *, *, #14727, .T. ) ;
#27702 = CARTESIAN_POINT ( 'NONE',  ( -35.00000000000000000, 0.000000000000000000, 0.000000000000000000 ) ) ;
#27703 = VERTEX_POINT ( 'NONE', #59440 ) ;
#27704 = CARTESIAN_POINT ( 'NONE',  ( 2.241506898688419014, 7.160521809579532437, -2.648071636522661088 ) ) ;
#27705 = CARTESIAN_POINT ( 'NONE',  ( -29.68541646480311869, -1.416020129149132334, -13.42553116244736877 ) ) ;
#27706 = CARTESIAN_POINT ( 'NONE',  ( 0.000000000000000000, -6.250523986464001425, 3.007653927006548766 ) ) ;
#27708 = VECTOR ( 'NONE', #37088, 1000.000000000000000 ) ;
#27707 = CARTESIAN_POINT ( 'NONE',  ( -35.00000000000000000, 1.457575200925722125, -12.66641127287624258 ) ) ;
#27709 = CARTESIAN_POINT ( 'NONE',  ( 2.406456491626409733, -10.36527681095989095, -1.188938370543056733 ) ) ;
#27710 = DIRECTION ( 'NONE',  ( -1.000000000000000000, 0.000000000000000000, -0.000000000000000000 ) ) ;
#27712 = ORIENTED_EDGE ( 'NONE', *, *, #31828, .T. ) ;
#27711 = ADVANCED_FACE ( 'NONE', ( #19202 ), #37256, .T. ) ;
#27713 = VERTEX_POINT ( 'NONE', #55436 ) ;
#27714 = VECTOR ( 'NONE', #37040, 1000.000000000000000 ) ;
#27715 = CARTESIAN_POINT ( 'NONE',  ( 2.639814597422736053, 7.600559958731745169, 1.600543348184837456 ) ) ;
#27716 = VERTEX_POINT ( 'NONE', #60098 ) ;
#27717 = ADVANCED_FACE ( 'NONE', ( #45133 ), #15191, .T. ) ;
#27718 = ORIENTED_EDGE ( 'NONE', *, *, #31291, .F. ) ;
#27719 = LINE ( 'NONE', #57680, #11579 ) ;
#27720 = DIRECTION ( 'NONE',  ( -1.000000000000000000, 0.000000000000000000, 0.000000000000000000 ) ) ;
#27721 = DIRECTION ( 'NONE',  ( 0.000000000000000000, -1.000000000000000000, 0.000000000000000000 ) ) ;
#27722 = B_SPLINE_CURVE_WITH_KNOTS ( 'NONE', 3,
 ( #12205, #7209, #27495, #32796, #39431, #49752, #64689, #3232, #29152, #38795, #33786, #48463, #60059, #23503, #3576, #14477 ),
 .UNSPECIFIED., .F., .F.,
 ( 4, 3, 3, 3, 3, 4 ),
 ( 2.959248127215453983E-15, 0.0002126834539179688283, 0.0004253519300366227210, 0.0006380165497224124863, 0.0007442707582428192276, 0.0009453531351419241406 ),
 .UNSPECIFIED. ) ;
#27723 = CARTESIAN_POINT ( 'NONE',  ( -22.28236030719477512, 2.111163412226061631, 3.035028179399193782 ) ) ;
#27725 = CIRCLE ( 'NONE', #7548, 5.000000000000000000 ) ;
#27724 = CARTESIAN_POINT ( 'NONE',  ( 36.00000000000000711, 7.379373053628869528, -10.39746860227893421 ) ) ;
#27726 = AXIS2_PLACEMENT_3D ( 'NONE', #54887, #4356, #24626 ) ;
#27727 = CARTESIAN_POINT ( 'NONE',  ( 5.516018279890452902, -0.001397286410094463784, -0.006629829924290467358 ) ) ;
#27728 = CARTESIAN_POINT ( 'NONE',  ( 35.00000000000000000, -7.817492529713787164, 9.348667969174485393 ) ) ;
#27729 = AXIS2_PLACEMENT_3D ( 'NONE', #12601, #46558, #31582 ) ;
#27730 = B_SPLINE_CURVE_WITH_KNOTS ( 'NONE', 3,
 ( #29604, #9017, #39599, #49284, #64850, #4035, #3738, #65501, #14320, #49911, #44255, #30280, #19664, #50251, #50580, #44914 ),
 .UNSPECIFIED., .F., .F.,
 ( 4, 3, 3, 3, 3, 4 ),
 ( 5.421010862427522170E-19, 0.0003017745587525216691, 0.0006035491769808687531, 0.0009053241094668072492, 0.001207275924539389766, 0.001510325902531777474 ),
 .UNSPECIFIED. ) ;
#27731 = ORIENTED_EDGE ( 'NONE', *, *, #34116, .F. ) ;
#27732 = VECTOR ( 'NONE', #14283, 1000.000000000000000 ) ;
#27733 = DIRECTION ( 'NONE',  ( 1.000000000000000000, -0.000000000000000000, -0.000000000000000000 ) ) ;
#27734 = CARTESIAN_POINT ( 'NONE',  ( 37.00000000000000711, 3.213188559034240832, -11.29812557209478285 ) ) ;
#27735 = AXIS2_PLACEMENT_3D ( 'NONE', #30178, #9227, #44470 ) ;
#27736 = EDGE_CURVE ( 'NONE', #64793, #12206, #45759, .T. ) ;
#27737 = CARTESIAN_POINT ( 'NONE',  ( -22.27834755396594346, 0.5583491773602499153, 3.643689482009640379 ) ) ;
#27738 = CARTESIAN_POINT ( 'NONE',  ( -41.00000000000000711, -1.853910857666116187E-16, -1.500000000000000222 ) ) ;
#27739 = LINE ( 'NONE', #1520, #13056 ) ;
#27740 = AXIS2_PLACEMENT_3D ( 'NONE', #15525, #50144, #15840 ) ;
#27741 = CARTESIAN_POINT ( 'NONE',  ( 1.000000000000000888, -3.795144977083660720, 6.468916029978762694 ) ) ;
#27742 = FACE_OUTER_BOUND ( 'NONE', #45134, .T. ) ;
#27743 = CIRCLE ( 'NONE', #1235, 5.000000000000000000 ) ;
#27744 = ORIENTED_EDGE ( 'NONE', *, *, #25890, .F. ) ;
#27745 = CARTESIAN_POINT ( 'NONE',  ( 5.516018279890452902, 0.005752102158673841684, -0.003580555109620817654 ) ) ;
#27746 = DIRECTION ( 'NONE',  ( 0.000000000000000000, -0.4198891015602528864, -0.9075754196709624466 ) ) ;
#27747 = DIRECTION ( 'NONE',  ( -1.000000000000000000, 0.000000000000000000, 0.000000000000000000 ) ) ;
#27748 = ADVANCED_FACE ( 'NONE', ( #14514 ), #13863, .T. ) ;
#27749 = CARTESIAN_POINT ( 'NONE',  ( 1.744217550874541445, -31.08480052993808229, 14.39239673296416377 ) ) ;
#27750 = VECTOR ( 'NONE', #38037, 1000.000000000000000 ) ;
#27751 = AXIS2_PLACEMENT_3D ( 'NONE', #20883, #43958, #46176 ) ;
#27752 = ADVANCED_FACE ( 'NONE', ( #10201 ), #45444, .T. ) ;
#27753 = DIRECTION ( 'NONE',  ( -0.9606638835031803270, 0.1943236796486226547, 0.1984016392583679012 ) ) ;
#27754 = CARTESIAN_POINT ( 'NONE',  ( -47.00000000000000711, 0.000000000000000000, 0.000000000000000000 ) ) ;
#27755 =( BOUNDED_CURVE ( )  B_SPLINE_CURVE ( 3, ( #48223, #2672, #38537, #58508 ),
 .UNSPECIFIED., .F., .F. ) 
 B_SPLINE_CURVE_WITH_KNOTS ( ( 4, 4 ),
 ( 0.8924480861843639978, 0.9142464078881809009 ),
 .UNSPECIFIED. ) 
 CURVE ( )  GEOMETRIC_REPRESENTATION_ITEM ( )  RATIONAL_B_SPLINE_CURVE ( ( 1.000000000000000000, 0.9999604031562251416, 0.9999604031562251416, 1.000000000000000000 ) ) 
 REPRESENTATION_ITEM ( '' )  );
#27756 = ORIENTED_EDGE ( 'NONE', *, *, #1525, .F. ) ;
#27757 = CARTESIAN_POINT ( 'NONE',  ( 17.92615217306980568, -8.262653472663041399, 8.714354160369650160 ) ) ;
#27758 = CARTESIAN_POINT ( 'NONE',  ( -35.00000000000000000, -7.971186206369537786, 9.217970097227697224 ) ) ;
#27759 = CARTESIAN_POINT ( 'NONE',  ( 37.25000000000000711, -27.21021009056489248, -4.500000000000000888 ) ) ;
#27760 = DIRECTION ( 'NONE',  ( 0.000000000000000000, 0.000000000000000000, 1.000000000000000000 ) ) ;
#27761 = EDGE_LOOP ( 'NONE', ( #12254, #23666, #61887, #18238 ) ) ;
#27762 = CARTESIAN_POINT ( 'NONE',  ( 0.3057689695767498717, 2.355923806019203148, 12.03117299329036882 ) ) ;
#27763 = DIRECTION ( 'NONE',  ( 0.000000000000000000, 0.000000000000000000, 1.000000000000000000 ) ) ;
#27764 = ADVANCED_FACE ( 'NONE', ( #34160 ), #3132, .F. ) ;
#27765 = ORIENTED_EDGE ( 'NONE', *, *, #17577, .F. ) ;
#27766 = EDGE_LOOP ( 'NONE', ( #12788, #5662, #49155, #25593 ) ) ;
#27767 = LINE ( 'NONE', #7155, #39472 ) ;
#27768 = CIRCLE ( 'NONE', #19288, 5.000000000000000888 ) ;
#27769 = CYLINDRICAL_SURFACE ( 'NONE', #23370, 2.899999999999994582 ) ;
#27770 = ORIENTED_EDGE ( 'NONE', *, *, #3078, .T. ) ;
#27771 = AXIS2_PLACEMENT_3D ( 'NONE', #14796, #15475, #29451 ) ;
#27772 = CARTESIAN_POINT ( 'NONE',  ( -35.00000000000000000, 0.000000000000000000, 0.000000000000000000 ) ) ;
#27773 = DIRECTION ( 'NONE',  ( -1.000000000000000000, -0.000000000000000000, 0.000000000000000000 ) ) ;
#27774 = DIRECTION ( 'NONE',  ( 0.000000000000000000, 0.9847383929261610547, -0.1740410799127649344 ) ) ;
#27775 = DIRECTION ( 'NONE',  ( 0.000000000000000000, -0.01356324068817998940, 0.9999080150203990547 ) ) ;
#27776 = CARTESIAN_POINT ( 'NONE',  ( -27.74986723846695114, 10.95058365257675881, -4.916369140193016740 ) ) ;
#27777 = EDGE_CURVE ( 'NONE', #12206, #26019, #65392, .T. ) ;
#27778 = DIRECTION ( 'NONE',  ( 0.000000000000000000, -0.01356324068817992175, 0.9999080150203990547 ) ) ;
#27780 = EDGE_LOOP ( 'NONE', ( #13783, #36779, #5771, #61820 ) ) ;
#27779 = CARTESIAN_POINT ( 'NONE',  ( 1.104777566491146334, 0.4777483965053739290, 12.51694124543052311 ) ) ;
#27781 = CARTESIAN_POINT ( 'NONE',  ( 1.020182472824380682, 4.691131056023482238, -11.58401323226494561 ) ) ;
#27782 = EDGE_CURVE ( 'NONE', #21481, #43133, #3927, .T. ) ;
#27783 = ORIENTED_EDGE ( 'NONE', *, *, #8643, .F. ) ;
#27784 = CARTESIAN_POINT ( 'NONE',  ( 24.90230333882989200, -0.3472681461867982988, -12.00162445426803437 ) ) ;
#27785 = AXIS2_PLACEMENT_3D ( 'NONE', #55041, #18826, #24447 ) ;
#27786 = VERTEX_POINT ( 'NONE', #64732 ) ;
#27787 = VERTEX_POINT ( 'NONE', #14837 ) ;
#27788 = ITEM_DEFINED_TRANSFORMATION ( 'NONE', 'NONE', #39852,  #24966 ) ;
#27789 = CARTESIAN_POINT ( 'NONE',  ( -25.20868475945270504, 11.50518608263469922, 7.064184148472541835 ) ) ;
#27790 = ADVANCED_FACE ( 'NONE', ( #35124 ), #9873, .T. ) ;
#27791 = PLANE ( 'NONE',  #34229 ) ;
#27792 = CARTESIAN_POINT ( 'NONE',  ( 2.491965175174554847, 1.548529392254221593, 7.560994562509386618 ) ) ;
#27793 = CARTESIAN_POINT ( 'NONE',  ( -46.52334308975180477, -0.6843348755673336337, -10.64746346056990767 ) ) ;
#27794 = EDGE_CURVE ( 'NONE', #37233, #58655, #2252, .T. ) ;
#27795 = CARTESIAN_POINT ( 'NONE',  ( -27.08416781016246588, 0.7680651426971888407, -2.158663327075699634 ) ) ;
#27796 = ORIENTED_EDGE ( 'NONE', *, *, #59303, .F. ) ;
#27797 = AXIS2_PLACEMENT_3D ( 'NONE', #27083, #47378, #17097 ) ;
#27798 = CARTESIAN_POINT ( 'NONE',  ( 35.00000000000000000, -4.339012074899872395, 10.91536515067652324 ) ) ;
#27799 = FACE_OUTER_BOUND ( 'NONE', #5909, .T. ) ;
#27801 = ORIENTED_EDGE ( 'NONE', *, *, #1815, .F. ) ;
#27800 = CYLINDRICAL_SURFACE ( 'NONE', #25263, 4.999999999999999112 ) ;
#27802 = ORIENTED_EDGE ( 'NONE', *, *, #21963, .T. ) ;
#27803 = ADVANCED_FACE ( 'NONE', ( #40453 ), #30793, .T. ) ;
#27804 = CARTESIAN_POINT ( 'NONE',  ( -35.00000000000000000, 8.235637554476644695, 9.733281772932190989 ) ) ;
#27805 = AXIS2_PLACEMENT_3D ( 'NONE', #19189, #18571, #3609 ) ;
#27806 = ORIENTED_EDGE ( 'NONE', *, *, #42771, .F. ) ;
#27807 = LINE ( 'NONE', #48108, #3017 ) ;
#27808 = FACE_OUTER_BOUND ( 'NONE', #2316, .T. ) ;
#27809 = LINE ( 'NONE', #48110, #33106 ) ;
#27810 = CARTESIAN_POINT ( 'NONE',  ( -22.30986928587821794, 3.138878161034337921, -2.105440358094949449 ) ) ;
#27811 = VECTOR ( 'NONE', #15679, 1000.000000000000000 ) ;
#27812 = CARTESIAN_POINT ( 'NONE',  ( 0.3665391374699465965, 3.952034409876454824, -11.62960183138723025 ) ) ;
#27813 = FACE_BOUND ( 'NONE', #65535, .T. ) ;
#27814 = VECTOR ( 'NONE', #22032, 1000.000000000000227 ) ;
#27815 = DIRECTION ( 'NONE',  ( 1.000000000000000000, 0.000000000000000000, 0.000000000000000000 ) ) ;
#27816 = ORIENTED_EDGE ( 'NONE', *, *, #17726, .F. ) ;
#27817 = DIRECTION ( 'NONE',  ( -1.000000000000000000, 0.000000000000000000, 0.000000000000000000 ) ) ;
#27818 = ORIENTED_EDGE ( 'NONE', *, *, #41872, .T. ) ;
#27819 = CARTESIAN_POINT ( 'NONE',  ( -37.00000000000000711, 0.000000000000000000, 0.000000000000000000 ) ) ;
#27820 = CARTESIAN_POINT ( 'NONE',  ( 35.00000000000000000, -2.497432891016756251, 11.47758908105696740 ) ) ;
#27821 = LINE ( 'NONE', #33131, #18036 ) ;
#27822 = AXIS2_PLACEMENT_3D ( 'NONE', #3680, #44509, #40514 ) ;
#27823 = ORIENTED_EDGE ( 'NONE', *, *, #57858, .T. ) ;
#27824 = VECTOR ( 'NONE', #62754, 1000.000000000000000 ) ;
#27825 = EDGE_CURVE ( 'NONE', #23170, #12670, #27725, .T. ) ;
#27826 = ORIENTED_EDGE ( 'NONE', *, *, #39102, .F. ) ;
#27827 = CYLINDRICAL_SURFACE ( 'NONE', #43957, 12.74999999999999822 ) ;
#27828 = AXIS2_PLACEMENT_3D ( 'NONE', #58695, #33714, #37729 ) ;
#27829 = ORIENTED_EDGE ( 'NONE', *, *, #36346, .F. ) ;
#27830 = DIRECTION ( 'NONE',  ( 0.000000000000000000, -0.9635499925192201331, -0.2675283385292311911 ) ) ;
#27831 = CARTESIAN_POINT ( 'NONE',  ( 2.000000000000001776, -5.107597897712365054, 4.693343793638375061 ) ) ;
#27832 = CIRCLE ( 'NONE', #53340, 12.18649999999999878 ) ;
#27833 = CARTESIAN_POINT ( 'NONE',  ( -27.09861164373156228, -2.097104182796950322, -1.025570525057856619 ) ) ;
#27834 = CYLINDRICAL_SURFACE ( 'NONE', #55198, 12.18649999999999878 ) ;
#27835 = VERTEX_POINT ( 'NONE', #31150 ) ;
#27836 = CARTESIAN_POINT ( 'NONE',  ( 0.3474126878361820658, 12.12932967384299410, 1.876013288000094148 ) ) ;
#27838 = AXIS2_PLACEMENT_3D ( 'NONE', #50491, #45158, #19886 ) ;
#27837 = CARTESIAN_POINT ( 'NONE',  ( 37.00000000000000711, 6.036400161834703404, 10.07641281632170838 ) ) ;
#27839 = EDGE_CURVE ( 'NONE', #56608, #5051, #577, .T. ) ;
#27840 = CARTESIAN_POINT ( 'NONE',  ( -29.54910026239419807, 0.3010961243626856243, -13.50337375539546336 ) ) ;
#27841 = CARTESIAN_POINT ( 'NONE',  ( -49.43099673984272613, -0.1154732602011075832, 5.319553669056252154 ) ) ;
#27842 = CARTESIAN_POINT ( 'NONE',  ( -27.08426504710140392, -0.5533780324190645805, -2.223709847896218061 ) ) ;
#27843 = AXIS2_PLACEMENT_3D ( 'NONE', #25952, #20937, #24373 ) ;
#27844 = FACE_OUTER_BOUND ( 'NONE', #35399, .T. ) ;
#27845 = ORIENTED_EDGE ( 'NONE', *, *, #51797, .F. ) ;
#27846 = CARTESIAN_POINT ( 'NONE',  ( -35.04643116707788408, 0.009511118309135299653, -0.007621814750509436909 ) ) ;
#27847 = CARTESIAN_POINT ( 'NONE',  ( 0.2646305136544072623, 2.256625640822315759, 12.03696649559615572 ) ) ;
#27848 = CARTESIAN_POINT ( 'NONE',  ( -17.03240540343445630, -28.50880493221823286, -9.306303259374256953 ) ) ;
#27849 = ORIENTED_EDGE ( 'NONE', *, *, #49069, .T. ) ;
#27850 = CARTESIAN_POINT ( 'NONE',  ( -11.19197262092341738, -9.208027763853694481, -7.717244145212098339 ) ) ;
#27851 = DIRECTION ( 'NONE',  ( -0.000000000000000000, -1.000000000000000000, -0.000000000000000000 ) ) ;
#27852 = CARTESIAN_POINT ( 'NONE',  ( -37.00000000000000711, 6.891188680298823144, 9.512294188640927572 ) ) ;
#27853 = EDGE_CURVE ( 'NONE', #65184, #9921, #33038, .T. ) ;
#27854 = AXIS2_PLACEMENT_3D ( 'NONE', #65235, #7841, #28118 ) ;
#27855 = CARTESIAN_POINT ( 'NONE',  ( -29.25940519196071321, 2.962255644788923892, -13.17777891311915894 ) ) ;
#27856 = EDGE_CURVE ( 'NONE', #16341, #27385, #43673, .T. ) ;
#27857 = CARTESIAN_POINT ( 'NONE',  ( 0.2647959493198566161, -11.45640103018461531, 4.326188315749694091 ) ) ;
#27858 = VECTOR ( 'NONE', #25537, 1000.000000000000000 ) ;
#27859 = CIRCLE ( 'NONE', #7695, 7.499999999999988454 ) ;
#27860 = VERTEX_POINT ( 'NONE', #15828 ) ;
#27861 = EDGE_LOOP ( 'NONE', ( #37379, #32579, #50184, #25164 ) ) ;
#27862 = CARTESIAN_POINT ( 'NONE',  ( 0.9232058338315058954, -12.46548196349786508, 0.3773051331667549579 ) ) ;
#27863 = VERTEX_POINT ( 'NONE', #247 ) ;
#27864 = CARTESIAN_POINT ( 'NONE',  ( 16.94760237393643720, -10.49682181221981025, 5.815268149447256008 ) ) ;
#27865 = CARTESIAN_POINT ( 'NONE',  ( 2.994568964204213035, 7.537093683963823842, -2.317954327151149574 ) ) ;
#27866 = DIRECTION ( 'NONE',  ( 0.000000000000000000, 0.01356324068817992175, -0.9999080150203990547 ) ) ;
#27867 = CARTESIAN_POINT ( 'NONE',  ( -35.00000000000000000, 6.891188680298823144, 9.512294188640927572 ) ) ;
#27868 = DIRECTION ( 'NONE',  ( 0.000000000000000000, -0.2618041379715496664, 0.9651210252299831094 ) ) ;
#27869 = DIRECTION ( 'NONE',  ( -0.000000000000000000, -0.000000000000000000, -1.000000000000000000 ) ) ;
#27870 = CYLINDRICAL_SURFACE ( 'NONE', #40334, 5.000000000000000888 ) ;
#27871 = ORIENTED_EDGE ( 'NONE', *, *, #9491, .T. ) ;
#27872 = ORIENTED_EDGE ( 'NONE', *, *, #5028, .F. ) ;
#27873 = CARTESIAN_POINT ( 'NONE',  ( 1.719304012338701115, -5.690355757827699534, 11.38834240361771677 ) ) ;
#27874 = ORIENTED_EDGE ( 'NONE', *, *, #53933, .T. ) ;
#27875 = MECHANICAL_DESIGN_GEOMETRIC_PRESENTATION_REPRESENTATION (  '', ( #19389 ), #13019 ) ;
#27876 = EDGE_CURVE ( 'NONE', #29225, #28103, #56446, .T. ) ;
#27877 = DIRECTION ( 'NONE',  ( 0.000000000000000000, 0.000000000000000000, 1.000000000000000000 ) ) ;
#27878 = DIRECTION ( 'NONE',  ( 0.000000000000000000, 0.01356324068817992175, -0.9999080150203990547 ) ) ;
#27879 = EDGE_CURVE ( 'NONE', #61666, #8847, #8651, .T. ) ;
#27880 = DIRECTION ( 'NONE',  ( -1.000000000000000000, 0.000000000000000000, 0.000000000000000000 ) ) ;
#27881 = ORIENTED_EDGE ( 'NONE', *, *, #49913, .F. ) ;
#27882 = LINE ( 'NONE', #31863, #15251 ) ;
#27883 = AXIS2_PLACEMENT_3D ( 'NONE', #61545, #46282, #30965 ) ;
#27884 = FACE_OUTER_BOUND ( 'NONE', #33631, .T. ) ;
#27885 = CARTESIAN_POINT ( 'NONE',  ( 37.00000000000000711, 11.47561260193577048, -5.556331110570448928 ) ) ;
#27886 = ORIENTED_EDGE ( 'NONE', *, *, #21202, .T. ) ;
#27887 = AXIS2_PLACEMENT_3D ( 'NONE', #53504, #33195, #22577 ) ;
#27888 = ORIENTED_EDGE ( 'NONE', *, *, #3391, .F. ) ;
#27889 = EDGE_CURVE ( 'NONE', #33067, #29231, #21840, .T. ) ;
#27890 = DIRECTION ( 'NONE',  ( 0.000000000000000000, 0.01356324068817991828, -0.9999080150203990547 ) ) ;
#27891 = ORIENTED_EDGE ( 'NONE', *, *, #6068, .T. ) ;
#27892 = FACE_OUTER_BOUND ( 'NONE', #40310, .T. ) ;
#27893 = ORIENTED_EDGE ( 'NONE', *, *, #39857, .T. ) ;
#27894 = VERTEX_POINT ( 'NONE', #26476 ) ;
#27895 = CARTESIAN_POINT ( 'NONE',  ( 2.241352910868909643, -7.202080440908757986, 2.532612177304417678 ) ) ;
#27896 = DIRECTION ( 'NONE',  ( 0.000000000000000000, -0.9987865678893281807, 0.04924826701373505311 ) ) ;
#27897 = CARTESIAN_POINT ( 'NONE',  ( -37.25000000000000711, -45.00200000000000244, 4.499999999999997335 ) ) ;
#27898 = CARTESIAN_POINT ( 'NONE',  ( -22.71097035706202405, -4.510116093748277599, 2.118550233809401107 ) ) ;
#27899 = DIRECTION ( 'NONE',  ( -1.000000000000000000, 0.000000000000000000, 0.000000000000000000 ) ) ;
#27900 = EDGE_CURVE ( 'NONE', #9878, #17695, #18251, .T. ) ;
#27901 = CARTESIAN_POINT ( 'NONE',  ( 0.2915757698887260774, 11.58754481235186340, 3.989025639548677393 ) ) ;
#27902 = VERTEX_POINT ( 'NONE', #1567 ) ;
#27903 = CARTESIAN_POINT ( 'NONE',  ( 2.000000000000001776, 0.000000000000000000, 0.000000000000000000 ) ) ;
#27904 = FACE_OUTER_BOUND ( 'NONE', #60759, .T. ) ;
#27905 = CARTESIAN_POINT ( 'NONE',  ( 2.263328370262049916, 3.697218830763628450, -6.687792802427183325 ) ) ;
#27906 = CARTESIAN_POINT ( 'NONE',  ( 37.00000000000000711, -4.986700593229777212, -10.63508530065520219 ) ) ;
#27908 = CARTESIAN_POINT ( 'NONE',  ( 26.08439714455133185, -11.40113243194250359, 3.743551691817327942 ) ) ;
#27907 = AXIS2_PLACEMENT_3D ( 'NONE', #2520, #58358, #12778 ) ;
#27909 = LINE ( 'NONE', #62479, #29160 ) ;
#27910 = CARTESIAN_POINT ( 'NONE',  ( 2.556980015513853122, -4.067895092073517738, -6.584367695372261409 ) ) ;
#27911 = CARTESIAN_POINT ( 'NONE',  ( 37.00000000000000711, 4.705694406421931860E-17, -3.469127814946512892E-15 ) ) ;
#27912 = CIRCLE ( 'NONE', #21500, 2.899999999999994582 ) ;
#27913 = CARTESIAN_POINT ( 'NONE',  ( 0.8375941296788397272, 5.882592429484509111, 10.95781044612375688 ) ) ;
#27914 = AXIS2_PLACEMENT_3D ( 'NONE', #25457, #35082, #44749 ) ;
#27915 = CIRCLE ( 'NONE', #28958, 5.000000000000001776 ) ;
#27916 = ORIENTED_EDGE ( 'NONE', *, *, #62463, .T. ) ;
#27917 = CARTESIAN_POINT ( 'NONE',  ( 1.000000000000000888, 0.8935325819929771374, -7.446583077151355923 ) ) ;
#27918 = ADVANCED_FACE ( 'NONE', ( #52087 ), #28545, .F. ) ;
#27919 = EDGE_LOOP ( 'NONE', ( #60743, #18749, #32004, #2885 ) ) ;
#27920 = CARTESIAN_POINT ( 'NONE',  ( 5.520433897694421610, 0.01006947824912422969, -0.01120198501134839035 ) ) ;
#27921 = CARTESIAN_POINT ( 'NONE',  ( -18.83018139755648335, -28.92741097219609969, -6.858339499770067960 ) ) ;
#27922 = CARTESIAN_POINT ( 'NONE',  ( 12.90005361535634520, -12.56318921256607801, -4.945239668744613404 ) ) ;
#27923 = CARTESIAN_POINT ( 'NONE',  ( 0.2653141334712562083, 9.409392642815744168, 7.837911425448813141 ) ) ;
#27924 = CARTESIAN_POINT ( 'NONE',  ( 2.000000000000001776, -3.341639490130703827, -6.078525953551491057 ) ) ;
#27925 = ORIENTED_EDGE ( 'NONE', *, *, #13089, .T. ) ;
#27926 = CIRCLE ( 'NONE', #3551, 2.899999999999995914 ) ;
#27927 = CARTESIAN_POINT ( 'NONE',  ( 0.9232167919969077596, 10.58277433962390113, -6.587352952801042605 ) ) ;
#27928 = DIRECTION ( 'NONE',  ( -1.000000000000000000, 0.000000000000000000, 0.000000000000000000 ) ) ;
#27929 = CARTESIAN_POINT ( 'NONE',  ( 0.2653141617321010948, -2.083144498805191258, -12.06772699408310778 ) ) ;
#27930 = AXIS2_PLACEMENT_3D ( 'NONE', #39545, #54850, #313 ) ;
#27931 = DIRECTION ( 'NONE',  ( 0.000000000000000000, 0.000000000000000000, 1.000000000000000000 ) ) ;
#27932 = ORIENTED_EDGE ( 'NONE', *, *, #46187, .T. ) ;
#27933 = CIRCLE ( 'NONE', #5641, 7.938172270156617749 ) ;
#27934 = CARTESIAN_POINT ( 'NONE',  ( 0.2646305136544072623, -9.465888453933013480, 7.770320294339146727 ) ) ;
#27935 = CARTESIAN_POINT ( 'NONE',  ( 1.547277799339149329, -8.651049845884454470, -9.261681528764416527 ) ) ;
#27937 = ADVANCED_FACE ( 'NONE', ( #5908 ), #40803, .T. ) ;
#27936 = CARTESIAN_POINT ( 'NONE',  ( 2.251152103363646795, -3.926807817126149125, -6.550893877460189252 ) ) ;
#27938 = ADVANCED_FACE ( 'NONE', ( #6540 ), #51459, .T. ) ;
#27939 = EDGE_CURVE ( 'NONE', #24263, #49961, #61751, .T. ) ;
#27940 = CIRCLE ( 'NONE', #58770, 12.75000000000000178 ) ;
#27941 = ORIENTED_EDGE ( 'NONE', *, *, #5734, .F. ) ;
#27942 = CYLINDRICAL_SURFACE ( 'NONE', #5290, 4.445031439545090279 ) ;
#27943 = EDGE_LOOP ( 'NONE', ( #53914, #1151, #20911, #857 ) ) ;
#27944 = CARTESIAN_POINT ( 'NONE',  ( -35.00000000000000000, -11.74226168163341022, -0.3025107581132430723 ) ) ;
#27945 = CARTESIAN_POINT ( 'NONE',  ( 2.000000000000001776, -3.341639490130797530, 6.078525953551414673 ) ) ;
#27946 = CARTESIAN_POINT ( 'NONE',  ( 35.00000000000000000, 2.772148766916280316, 11.86701198550353098 ) ) ;
#27947 = CARTESIAN_POINT ( 'NONE',  ( 3.152665057734040488, 0.000000000000000000, 0.000000000000000000 ) ) ;
#27948 = CARTESIAN_POINT ( 'NONE',  ( -35.04683013664716640, 0.01216443238273415967, 0.002177781393181293674 ) ) ;
#27949 = ORIENTED_EDGE ( 'NONE', *, *, #7253, .F. ) ;
#27950 = VECTOR ( 'NONE', #31925, 1000.000000000000000 ) ;
#27951 = VECTOR ( 'NONE', #64102, 1000.000000000000000 ) ;
#27952 = EDGE_LOOP ( 'NONE', ( #20983, #27134, #62778, #59435 ) ) ;
#27953 = VERTEX_POINT ( 'NONE', #56774 ) ;
#27954 = FACE_OUTER_BOUND ( 'NONE', #57995, .T. ) ;
#27955 = EDGE_CURVE ( 'NONE', #4690, #28947, #61721, .T. ) ;
#27956 = AXIS2_PLACEMENT_3D ( 'NONE', #46724, #41735, #36749 ) ;
#27958 = AXIS2_PLACEMENT_3D ( 'NONE', #6689, #31926, #1703 ) ;
#27957 = DIRECTION ( 'NONE',  ( -1.000000000000000000, 0.000000000000000000, 0.000000000000000000 ) ) ;
#27959 = ORIENTED_EDGE ( 'NONE', *, *, #62847, .T. ) ;
#27960 = CYLINDRICAL_SURFACE ( 'NONE', #54906, 13.50000000000000178 ) ;
#27961 = CARTESIAN_POINT ( 'NONE',  ( -22.29290468048227680, -0.2747050847461753875, -3.718584170466891603 ) ) ;
#27962 = VERTEX_POINT ( 'NONE', #31473 ) ;
#27963 =( BOUNDED_CURVE ( )  B_SPLINE_CURVE ( 3, ( #27153, #12831, #48439, #17175 ),
 .UNSPECIFIED., .F., .F. ) 
 B_SPLINE_CURVE_WITH_KNOTS ( ( 4, 4 ),
 ( 3.747716794192935019, 3.763247559512395757 ),
 .UNSPECIFIED. ) 
 CURVE ( )  GEOMETRIC_REPRESENTATION_ITEM ( )  RATIONAL_B_SPLINE_CURVE ( ( 1.000000000000000000, 0.9999798997117221866, 0.9999798997117221866, 1.000000000000000000 ) ) 
 REPRESENTATION_ITEM ( '' )  );
#27964 = CARTESIAN_POINT ( 'NONE',  ( -41.00000000000000711, -45.00200000000000244, -4.500000000000000888 ) ) ;
#27965 = CARTESIAN_POINT ( 'NONE',  ( 2.247112776671467138, -2.720990995225260445, -7.135103076758478657 ) ) ;
#27966 = LINE ( 'NONE', #13321, #23944 ) ;
#27967 = ORIENTED_EDGE ( 'NONE', *, *, #26763, .F. ) ;
#27968 = VECTOR ( 'NONE', #19971, 1000.000000000000000 ) ;
#27969 = ORIENTED_EDGE ( 'NONE', *, *, #695, .T. ) ;
#27970 = CARTESIAN_POINT ( 'NONE',  ( 2.261269890822072970, 2.481875047312938065, 7.226741992146798133 ) ) ;
#27971 = VERTEX_POINT ( 'NONE', #51771 ) ;
#27972 = CARTESIAN_POINT ( 'NONE',  ( 8.817269919411085510, 2.645982468348137662, -13.24072998050336203 ) ) ;
#27973 = ORIENTED_EDGE ( 'NONE', *, *, #42072, .F. ) ;
#27974 = CONICAL_SURFACE ( 'NONE', #34312, 7.938172270156617749, 1.280189991382167047 ) ;
#27975 = CARTESIAN_POINT ( 'NONE',  ( 6.013273758134695335, -31.75304111242975580, -13.61309608153482031 ) ) ;
#27976 = ADVANCED_FACE ( 'NONE', ( #46764 ), #36789, .T. ) ;
#27977 = B_SPLINE_CURVE_WITH_KNOTS ( 'NONE', 3,
 ( #6284, #51188, #62132, #61794, #20593, #314, #51836 ),
 .UNSPECIFIED., .F., .F.,
 ( 4, 3, 4 ),
 ( 6.158474197255674489E-15, 0.002398160485434825892, 0.005002426799382968595 ),
 .UNSPECIFIED. ) ;
#27978 = CARTESIAN_POINT ( 'NONE',  ( 35.00000000000000000, -11.38112321385048631, 2.905556151562744382 ) ) ;
#27979 = LINE ( 'NONE', #43924, #19750 ) ;
#27980 = CYLINDRICAL_SURFACE ( 'NONE', #30855, 12.75000000000000178 ) ;
#27981 = FACE_OUTER_BOUND ( 'NONE', #9966, .T. ) ;
#27982 = CARTESIAN_POINT ( 'NONE',  ( -27.63886315033333574, -10.11438670753379299, -6.464158504329111210 ) ) ;
#27983 = VERTEX_POINT ( 'NONE', #32756 ) ;
#27984 = CARTESIAN_POINT ( 'NONE',  ( 35.00000000000000000, 6.475373545682446164, 10.32377448871660519 ) ) ;
#27985 = CIRCLE ( 'NONE', #19487, 12.74999999999999822 ) ;
#27986 = ORIENTED_EDGE ( 'NONE', *, *, #43492, .T. ) ;
#27987 =( BOUNDED_CURVE ( )  B_SPLINE_CURVE ( 3, ( #40258, #55236, #35607, #60545 ),
 .UNSPECIFIED., .F., .F. ) 
 B_SPLINE_CURVE_WITH_KNOTS ( ( 4, 4 ),
 ( 5.770121532352542104, 5.841648021086276898 ),
 .UNSPECIFIED. ) 
 CURVE ( )  GEOMETRIC_REPRESENTATION_ITEM ( )  RATIONAL_B_SPLINE_CURVE ( ( 1.000000000000000000, 0.9995737088895613187, 0.9995737088895613187, 1.000000000000000000 ) ) 
 REPRESENTATION_ITEM ( '' )  );
#27988 = DIRECTION ( 'NONE',  ( -1.000000000000000000, 0.000000000000000000, 0.000000000000000000 ) ) ;
#27989 = AXIS2_PLACEMENT_3D ( 'NONE', #43929, #63531, #33622 ) ;
#27990 = DIRECTION ( 'NONE',  ( -1.000000000000000000, 0.000000000000000000, 0.000000000000000000 ) ) ;
#27991 = ORIENTED_EDGE ( 'NONE', *, *, #22013, .F. ) ;
#27992 = DIRECTION ( 'NONE',  ( -1.000000000000000000, 0.000000000000000000, 0.000000000000000000 ) ) ;
#27993 = CARTESIAN_POINT ( 'NONE',  ( 0.3654063281920725270, 6.366443614636685844, 10.50027211615249456 ) ) ;
#27994 = CARTESIAN_POINT ( 'NONE',  ( 0.2834382757448005719, -2.326926314863231759, -12.02923522794684885 ) ) ;
#27995 = ORIENTED_EDGE ( 'NONE', *, *, #14697, .T. ) ;
#27996 = AXIS2_PLACEMENT_3D ( 'NONE', #6630, #27221, #32840 ) ;
#27997 = ORIENTED_EDGE ( 'NONE', *, *, #37919, .F. ) ;
#27998 = CARTESIAN_POINT ( 'NONE',  ( 2.717984159220037110, -6.886544461123986771, -3.648459810929770786 ) ) ;
#27999 = EDGE_CURVE ( 'NONE', #665, #46663, #63678, .T. ) ;
#28000 = ORIENTED_EDGE ( 'NONE', *, *, #37043, .T. ) ;
#28001 = CARTESIAN_POINT ( 'NONE',  ( -35.00000000000000000, -3.614449339633411196, -11.17622378668010441 ) ) ;
#28002 = CARTESIAN_POINT ( 'NONE',  ( 5.514970785353741078, 0.001326349372336578557, 0.004532877335078321253 ) ) ;
#28003 = EDGE_CURVE ( 'NONE', #47877, #33694, #36259, .T. ) ;
#28004 = DIRECTION ( 'NONE',  ( -1.000000000000000000, -0.000000000000000000, 0.000000000000000000 ) ) ;
#28005 = CARTESIAN_POINT ( 'NONE',  ( -18.81994070919206763, -4.785352002469239530, 11.00505384451766666 ) ) ;
#28006 = ORIENTED_EDGE ( 'NONE', *, *, #47419, .F. ) ;
#28007 = CIRCLE ( 'NONE', #6743, 6.936499999999986343 ) ;
#28008 = AXIS2_PLACEMENT_3D ( 'NONE', #13084, #38688, #12735 ) ;
#28009 = CARTESIAN_POINT ( 'NONE',  ( 5.516018279890452902, -0.004525000489649900863, 0.005042957932159117078 ) ) ;
#28010 = VECTOR ( 'NONE', #10021, 1000.000000000000227 ) ;
#28011 = EDGE_CURVE ( 'NONE', #19607, #56863, #3200, .T. ) ;
#28012 = CARTESIAN_POINT ( 'NONE',  ( 4.028938272669574161, -26.74124408001654629, -15.94258242224534960 ) ) ;
#28013 = VECTOR ( 'NONE', #22872, 1000.000000000000000 ) ;
#28014 = CIRCLE ( 'NONE', #58849, 12.75000000000000178 ) ;
#28015 = CARTESIAN_POINT ( 'NONE',  ( 22.11764649685935069, 13.40615838776775171, -1.629994490815044772 ) ) ;
#28016 = CARTESIAN_POINT ( 'NONE',  ( -37.00000000000000711, -0.7008968033237865658, -12.16632754454237819 ) ) ;
#28018 = EDGE_CURVE ( 'NONE', #40199, #29886, #23136, .T. ) ;
#28017 = CARTESIAN_POINT ( 'NONE',  ( 1.937114397841932290, 10.38782037574626926, -7.538912286488240966 ) ) ;
#28019 = CARTESIAN_POINT ( 'NONE',  ( -37.00000000000000711, 0.000000000000000000, 0.000000000000000000 ) ) ;
#28020 = CARTESIAN_POINT ( 'NONE',  ( 2.639814597422744047, 5.186391178752210784, -5.782006333156018307 ) ) ;
#28021 = CIRCLE ( 'NONE', #21664, 12.74999999999999822 ) ;
#28022 = CIRCLE ( 'NONE', #7855, 14.99999999999998757 ) ;
#28023 = ORIENTED_EDGE ( 'NONE', *, *, #54244, .T. ) ;
#28024 = CARTESIAN_POINT ( 'NONE',  ( 2.305787727787084407, -0.1666591538753222634, 7.654065630109506024 ) ) ;
#28025 = ORIENTED_EDGE ( 'NONE', *, *, #62981, .T. ) ;
#28026 = DIRECTION ( 'NONE',  ( 1.000000000000000000, 0.000000000000000000, -0.000000000000000000 ) ) ;
#28027 = CARTESIAN_POINT ( 'NONE',  ( 1.000000000000000888, 3.937687286050817193, 6.383151168292468647 ) ) ;
#28028 = FACE_OUTER_BOUND ( 'NONE', #10548, .T. ) ;
#28029 = AXIS2_PLACEMENT_3D ( 'NONE', #62387, #26830, #16845 ) ;
#28030 = ORIENTED_EDGE ( 'NONE', *, *, #44096, .F. ) ;
#28031 = CARTESIAN_POINT ( 'NONE',  ( 2.290907136834313018, 6.543263131934393684, 3.965134647956439551 ) ) ;
#28032 = ORIENTED_EDGE ( 'NONE', *, *, #31437, .F. ) ;
#28033 = CARTESIAN_POINT ( 'NONE',  ( 35.00000000000000000, 2.968224442958566911, 11.81949347079743440 ) ) ;
#28034 = VERTEX_POINT ( 'NONE', #2880 ) ;
#28035 = EDGE_LOOP ( 'NONE', ( #47445, #40619, #40270, #21309 ) ) ;
#28036 = CARTESIAN_POINT ( 'NONE',  ( -36.00000000000000711, 12.16893194857550142, 3.805206332242516254 ) ) ;
#28037 = CARTESIAN_POINT ( 'NONE',  ( 2.257661810676418579, -7.131864446283245229, 2.739276463085656310 ) ) ;
#28038 = ORIENTED_EDGE ( 'NONE', *, *, #52547, .F. ) ;
#28039 = CARTESIAN_POINT ( 'NONE',  ( -22.27711653538342773, -2.191780254295667696, -2.958138731383664233 ) ) ;
#28040 = CARTESIAN_POINT ( 'NONE',  ( 2.827825597296700799, 9.007857251166790036, 0.5449445831287562658 ) ) ;
#28041 = LINE ( 'NONE', #23371, #51439 ) ;
#28042 = CARTESIAN_POINT ( 'NONE',  ( 18.82686498295705135, 4.840479739905770629, 10.99031994906281540 ) ) ;
#28043 = ORIENTED_EDGE ( 'NONE', *, *, #26864, .F. ) ;
#28044 = DIRECTION ( 'NONE',  ( -1.000000000000000000, 0.000000000000000000, -0.000000000000000000 ) ) ;
#28045 = CARTESIAN_POINT ( 'NONE',  ( 15.96609733983705226, -34.98269025770574103, 4.990963945245213473 ) ) ;
#28046 = CARTESIAN_POINT ( 'NONE',  ( 2.244591118396559448, -1.431619869711802329, -7.500068934084580974 ) ) ;
#28048 = ORIENTED_EDGE ( 'NONE', *, *, #14804, .F. ) ;
#28047 = CARTESIAN_POINT ( 'NONE',  ( -24.61176285888814519, 9.685806582847478197, 7.097305586750869644 ) ) ;
#28049 = CARTESIAN_POINT ( 'NONE',  ( 5.516018279890452902, -0.006771744149385265123, 0.0002248006052448276067 ) ) ;
#28050 = ORIENTED_EDGE ( 'NONE', *, *, #13151, .F. ) ;
#28051 = VECTOR ( 'NONE', #31131, 1000.000000000000114 ) ;
#28053 = EDGE_CURVE ( 'NONE', #29988, #13694, #64930, .T. ) ;
#28052 = DIRECTION ( 'NONE',  ( -1.000000000000000000, 0.000000000000000000, 0.000000000000000000 ) ) ;
#28054 = AXIS2_PLACEMENT_3D ( 'NONE', #27507, #61778, #56472 ) ;
#28055 = ORIENTED_EDGE ( 'NONE', *, *, #26424, .T. ) ;
#28056 = CARTESIAN_POINT ( 'NONE',  ( 2.827825597296799831, 2.568788224597768455, 8.650999012440202307 ) ) ;
#28057 = FACE_OUTER_BOUND ( 'NONE', #28203, .T. ) ;
#28058 = CARTESIAN_POINT ( 'NONE',  ( -35.00000000000000000, 0.000000000000000000, 0.000000000000000000 ) ) ;
#28060 = CARTESIAN_POINT ( 'NONE',  ( 0.3654063281920773565, -3.951404032559346025, 11.62642356802260757 ) ) ;
#28059 = AXIS2_PLACEMENT_3D ( 'NONE', #54918, #44281, #9345 ) ;
#28061 = EDGE_CURVE ( 'NONE', #14288, #41167, #58068, .T. ) ;
#28062 = CARTESIAN_POINT ( 'NONE',  ( 0.3006302518452043104, 9.533790235540747560, 7.704827863860824522 ) ) ;
#28063 = CARTESIAN_POINT ( 'NONE',  ( -17.54726996257253191, 11.36053454945672847, 3.865003848717349033 ) ) ;
#28064 = CARTESIAN_POINT ( 'NONE',  ( 36.00000000000000711, -9.390600770288051180, -8.624332853796024878 ) ) ;
#28065 = VERTEX_POINT ( 'NONE', #53065 ) ;
#28066 = CARTESIAN_POINT ( 'NONE',  ( 0.9232058338315048962, -12.34162163148534930, 1.793035206307305174 ) ) ;
#28067 = ORIENTED_EDGE ( 'NONE', *, *, #23005, .T. ) ;
#28068 = ORIENTED_EDGE ( 'NONE', *, *, #1547, .T. ) ;
#28069 = CIRCLE ( 'NONE', #59921, 7.499999999999988454 ) ;
#28070 = CYLINDRICAL_SURFACE ( 'NONE', #34908, 2.899999999999994582 ) ;
#28071 = LINE ( 'NONE', #7432, #44297 ) ;
#28072 = DIRECTION ( 'NONE',  ( 1.000000000000000000, 0.000000000000000000, 0.000000000000000000 ) ) ;
#28073 = CARTESIAN_POINT ( 'NONE',  ( 0.3164563675027582401, -10.49799587805935097, 6.338687639235996762 ) ) ;
#28074 = DIRECTION ( 'NONE',  ( 0.000000000000000000, 0.01356324068817998940, -0.9999080150203990547 ) ) ;
#28075 = CIRCLE ( 'NONE', #43963, 5.000000000000000888 ) ;
#28076 = CARTESIAN_POINT ( 'NONE',  ( 1.937114397841935398, 12.33981801388257793, 3.531416430611335144 ) ) ;
#28077 = EDGE_CURVE ( 'NONE', #34425, #26744, #37433, .T. ) ;
#28078 = CYLINDRICAL_SURFACE ( 'NONE', #6849, 7.499999999999988454 ) ;
#28079 = ADVANCED_FACE ( 'NONE', ( #43079 ), #58743, .T. ) ;
#28080 = EDGE_CURVE ( 'NONE', #12197, #42153, #38764, .T. ) ;
#28081 = ORIENTED_EDGE ( 'NONE', *, *, #14318, .T. ) ;
#28082 = CIRCLE ( 'NONE', #55707, 4.999999999999998224 ) ;
#28083 = CARTESIAN_POINT ( 'NONE',  ( 0.3040950598368144520, 2.376091969481376243, -12.02925914197702895 ) ) ;
#28084 = LINE ( 'NONE', #33047, #64236 ) ;
#28085 = EDGE_CURVE ( 'NONE', #1795, #56510, #35331, .T. ) ;
#28086 = CARTESIAN_POINT ( 'NONE',  ( -17.18002655544815838, -8.043634770698369962, 10.84711994095657950 ) ) ;
#28087 = DIRECTION ( 'NONE',  ( 0.000000000000000000, 0.000000000000000000, 1.000000000000000000 ) ) ;
#28088 = EDGE_CURVE ( 'NONE', #46364, #7895, #52194, .T. ) ;
#28089 = B_SPLINE_CURVE_WITH_KNOTS ( 'NONE', 3,
 ( #21201, #45490, #20569, #65753, #35519, #20225, #40504, #55817, #10243, #30520 ),
 .UNSPECIFIED., .F., .F.,
 ( 4, 3, 3, 4 ),
 ( 1.226634733346699349E-18, 6.607638129004422475E-05, 9.911389841680472114E-05, 0.0001667630577588619047 ),
 .UNSPECIFIED. ) ;
#28090 = CARTESIAN_POINT ( 'NONE',  ( -34.00000000000000000, 15.00000000000000000, 1.836970198721029589E-15 ) ) ;
#28091 = EDGE_CURVE ( 'NONE', #52020, #31676, #63893, .T. ) ;
#28092 = CARTESIAN_POINT ( 'NONE',  ( -35.00000000000000000, 11.35427606708812753, -4.426194442447117794 ) ) ;
#28093 = ORIENTED_EDGE ( 'NONE', *, *, #43605, .T. ) ;
#28094 = CARTESIAN_POINT ( 'NONE',  ( 37.00000000000000711, -5.273331777780263074, 10.49591321039685887 ) ) ;
#28095 = CIRCLE ( 'NONE', #62078, 12.75000000000000178 ) ;
#28096 = CARTESIAN_POINT ( 'NONE',  ( -35.00000000000000000, 0.3137578094509240190, 12.74613886779085092 ) ) ;
#28097 = CYLINDRICAL_SURFACE ( 'NONE', #52409, 4.999999999999999112 ) ;
#28098 = VECTOR ( 'NONE', #22876, 1000.000000000000000 ) ;
#28099 = B_SPLINE_CURVE_WITH_KNOTS ( 'NONE', 3,
 ( #56743, #57053, #52720, #7147, #26133, #22113, #62342, #62660, #41079, #62037, #56383, #27423 ),
 .UNSPECIFIED., .F., .F.,
 ( 4, 2, 2, 2, 2, 4 ),
 ( 0.000000000000000000, 0.001701700952312556721, 0.002552551428468834756, 0.003403401904625113442, 0.005105102856937667778, 0.006806803809250222548 ),
 .UNSPECIFIED. ) ;
#28100 = EDGE_CURVE ( 'NONE', #50924, #38752, #32441, .T. ) ;
#28101 = CYLINDRICAL_SURFACE ( 'NONE', #6562, 7.499999999999988454 ) ;
#28102 = CARTESIAN_POINT ( 'NONE',  ( -25.21604033134154577, -8.971440100409701301, 10.09254481884992316 ) ) ;
#28103 = VERTEX_POINT ( 'NONE', #52751 ) ;
#28104 = CARTESIAN_POINT ( 'NONE',  ( 18.99404383257591533, 0.5703370437478672006, 12.04059188870767194 ) ) ;
#28105 = DIRECTION ( 'NONE',  ( 0.000000000000000000, 0.07632122047555797706, -0.9970832820307042876 ) ) ;
#28106 = FACE_OUTER_BOUND ( 'NONE', #24916, .T. ) ;
#28107 = EDGE_LOOP ( 'NONE', ( #37809, #26004, #18396, #2238 ) ) ;
#28108 = CARTESIAN_POINT ( 'NONE',  ( 0.3610902822527223832, 2.389900346488088800, 12.04327049858140519 ) ) ;
#28109 = CARTESIAN_POINT ( 'NONE',  ( 0.2653519890518175051, -4.188454465438607777, -11.50765826381081602 ) ) ;
#28110 = ORIENTED_EDGE ( 'NONE', *, *, #54731, .F. ) ;
#28111 = ORIENTED_EDGE ( 'NONE', *, *, #61735, .T. ) ;
#28112 = DIRECTION ( 'NONE',  ( 0.000000000000000000, -0.01356324068817998940, 0.9999080150203990547 ) ) ;
#28113 = VERTEX_POINT ( 'NONE', #33104 ) ;
#28114 = CARTESIAN_POINT ( 'NONE',  ( 0.3106921474978453501, -9.542334142800513064, 7.699584408545861791 ) ) ;
#28115 = CARTESIAN_POINT ( 'NONE',  ( -35.00000000000000000, 1.463443770872774774, 12.09831040184924866 ) ) ;
#28116 = CARTESIAN_POINT ( 'NONE',  ( 2.241352910868909643, 7.503490710578251566, -1.407733736974789762 ) ) ;
#28117 = DIRECTION ( 'NONE',  ( -1.000000000000000000, 0.000000000000000000, 0.000000000000000000 ) ) ;
#28118 = DIRECTION ( 'NONE',  ( 0.000000000000000000, 0.000000000000000000, 1.000000000000000000 ) ) ;
#28119 = CARTESIAN_POINT ( 'NONE',  ( 0.3401186441510234970, 5.912862694513716377, 10.75260364139047908 ) ) ;
#28121 = VERTEX_POINT ( 'NONE', #34725 ) ;
#28120 = LINE ( 'NONE', #43386, #9627 ) ;
#28122 = CARTESIAN_POINT ( 'NONE',  ( 0.3675815128205894289, 4.447030445008336663, -11.44679196252404729 ) ) ;
#28123 = EDGE_LOOP ( 'NONE', ( #28864, #40786, #44049, #15363 ) ) ;
#28124 = CARTESIAN_POINT ( 'NONE',  ( -35.04834644901396956, 0.0002835132723552184503, 0.01383120537647892362 ) ) ;
#28125 = EDGE_LOOP ( 'NONE', ( #25057, #61173, #59357, #58731 ) ) ;
#28126 = ORIENTED_EDGE ( 'NONE', *, *, #30555, .F. ) ;
#28127 = CARTESIAN_POINT ( 'NONE',  ( -25.21790179505041962, 8.968132426929548373, 10.09542157472211166 ) ) ;
#28128 = CARTESIAN_POINT ( 'NONE',  ( -4.228765754682471290, -26.75056327283501290, 15.92880586833495649 ) ) ;
#28129 = FACE_OUTER_BOUND ( 'NONE', #23061, .T. ) ;
#28130 = EDGE_CURVE ( 'NONE', #40566, #36018, #13792, .T. ) ;
#28131 = AXIS2_PLACEMENT_3D ( 'NONE', #41886, #21943, #15621 ) ;
#28132 = B_SPLINE_CURVE_WITH_KNOTS ( 'NONE', 3,
 ( #48329, #34554, #63254, #57967, #13053, #63914, #65143, #22362, #12378, #12704 ),
 .UNSPECIFIED., .F., .F.,
 ( 4, 3, 3, 4 ),
 ( 1.226634733346699349E-18, 6.607638129004543093E-05, 9.911389841680636099E-05, 0.0001667630577588615252 ),
 .UNSPECIFIED. ) ;
#28133 = CARTESIAN_POINT ( 'NONE',  ( -35.00000000000000000, 5.814360711498290257, 10.70999494708494559 ) ) ;
#28134 = CARTESIAN_POINT ( 'NONE',  ( -48.99862351417108641, -0.2022747408561963445, 1.593306619454956108 ) ) ;
#28135 = DIRECTION ( 'NONE',  ( -1.000000000000000000, 0.000000000000000000, 0.000000000000000000 ) ) ;
#28136 = VERTEX_POINT ( 'NONE', #65332 ) ;
#28137 = CARTESIAN_POINT ( 'NONE',  ( -22.27706485742869091, -0.3729136217355977778, -3.662257305743823022 ) ) ;
#28138 = CARTESIAN_POINT ( 'NONE',  ( 3.899857516006353553, 5.327130952939131525, -12.43655783340662779 ) ) ;
#28139 = CARTESIAN_POINT ( 'NONE',  ( 0.000000000000000000, -5.769711778877296027, -4.791703871138604853 ) ) ;
#28140 = EDGE_LOOP ( 'NONE', ( #59068, #63361, #22285, #37669 ) ) ;
#28141 = CARTESIAN_POINT ( 'NONE',  ( 0.000000000000000000, 5.396716205731493687, -4.158041573745044239 ) ) ;
#28142 = MECHANICAL_DESIGN_GEOMETRIC_PRESENTATION_REPRESENTATION (  '', ( #31316 ), #33455 ) ;
#28143 = ORIENTED_EDGE ( 'NONE', *, *, #23754, .F. ) ;
#28144 = DIRECTION ( 'NONE',  ( 0.000000000000000000, -0.01356324068817998940, 0.9999080150203990547 ) ) ;
#28145 = CARTESIAN_POINT ( 'NONE',  ( -10.85732715899702328, -8.333102996281885666, 8.651287110141016257 ) ) ;
#28146 = CARTESIAN_POINT ( 'NONE',  ( 5.514970785353741078, -0.003929719953530087274, -0.002619824551223206600 ) ) ;
#28147 = DIRECTION ( 'NONE',  ( 0.000000000000000000, 0.01356324068817992175, -0.9999080150203990547 ) ) ;
#28148 = CARTESIAN_POINT ( 'NONE',  ( 5.520433897694421610, -0.01473594271720230636, -0.003119431460922371217 ) ) ;
#28149 = CARTESIAN_POINT ( 'NONE',  ( 35.00000000000000000, 7.251710744571704836, 9.240395740215555875 ) ) ;
#28150 = EDGE_CURVE ( 'NONE', #24439, #22257, #15112, .T. ) ;
#28151 = CARTESIAN_POINT ( 'NONE',  ( 2.305787727787083519, 3.971363876084056166, -6.545285700970486786 ) ) ;
#28152 = VERTEX_POINT ( 'NONE', #55700 ) ;
#28153 = CARTESIAN_POINT ( 'NONE',  ( -18.04458733766117362, 12.91933584589294703, 3.916728392552376370 ) ) ;
#28154 = EDGE_CURVE ( 'NONE', #24332, #35410, #8831, .T. ) ;
#28155 = VERTEX_POINT ( 'NONE', #24122 ) ;
#28156 = EDGE_CURVE ( 'NONE', #13458, #57555, #39402, .T. ) ;
#28157 = CARTESIAN_POINT ( 'NONE',  ( -27.15511094194037867, 1.375165223101532108, 2.092607239484509662 ) ) ;
#28158 = CYLINDRICAL_SURFACE ( 'NONE', #7439, 5.000000000000000888 ) ;
#28159 = CARTESIAN_POINT ( 'NONE',  ( 29.36289517528272697, 4.666195979332582233, 11.05608984446922349 ) ) ;
#28160 = AXIS2_PLACEMENT_3D ( 'NONE', #50621, #40626, #10047 ) ;
#28161 = CYLINDRICAL_SURFACE ( 'NONE', #38726, 12.74999999999999822 ) ;
#28162 = FACE_OUTER_BOUND ( 'NONE', #52875, .T. ) ;
#28163 =( BOUNDED_SURFACE ( )  B_SPLINE_SURFACE ( 3, 1, ( 
 ( #47601, #47291 ),
 ( #52282, #2392 ),
 ( #53250, #17001 ),
 ( #27629, #26329 ) ),
 .UNSPECIFIED., .F., .F., .F. ) 
 B_SPLINE_SURFACE_WITH_KNOTS ( ( 4, 4 ),
 ( 2, 2 ),
 ( 0.000000000000000000, 1.000000000000000000 ),
 ( 0.000000000000000000, 1.000000000000000000 ),
 .UNSPECIFIED. ) 
 GEOMETRIC_REPRESENTATION_ITEM ( )  RATIONAL_B_SPLINE_SURFACE ( (
 ( 1.000000000000000000, 1.000000000000000000),
 ( 0.9942764183789327692, 0.8450855930916580938),
 ( 0.9942764183789327692, 0.8450855930916580938),
 ( 1.000000000000000000, 1.000000000000000000) ) ) 
 REPRESENTATION_ITEM ( '' )  SURFACE ( )  );
#28164 = ORIENTED_EDGE ( 'NONE', *, *, #57551, .F. ) ;
#28165 = DIRECTION ( 'NONE',  ( -1.000000000000000000, -0.000000000000000000, 0.000000000000000000 ) ) ;
#28166 = ADVANCED_FACE ( 'NONE', ( #18813 ), #60678, .T. ) ;
#28167 = CARTESIAN_POINT ( 'NONE',  ( 0.000000000000000000, 7.347880794884120722E-16, 6.000000000000000888 ) ) ;
#28168 = CARTESIAN_POINT ( 'NONE',  ( 1.719304012340731269, -10.22720798541492826, -7.581471372739399861 ) ) ;
#28169 = FACE_OUTER_BOUND ( 'NONE', #60371, .T. ) ;
#28170 = EDGE_CURVE ( 'NONE', #47999, #52971, #35393, .T. ) ;
#28171 = ORIENTED_EDGE ( 'NONE', *, *, #3231, .F. ) ;
#28172 = CARTESIAN_POINT ( 'NONE',  ( 0.2652384529303146721, -6.180212112237588151, -10.57229402027114062 ) ) ;
#28173 = CARTESIAN_POINT ( 'NONE',  ( 17.78300047788348337, 10.70435634735966168, 8.233749023714018733 ) ) ;
#28174 = CARTESIAN_POINT ( 'NONE',  ( 1.719304012340734378, -8.755325027794794934, -9.242227816401850760 ) ) ;
#28175 = CARTESIAN_POINT ( 'NONE',  ( -44.86048679285934782, -0.9948977233718158120, -15.27141897285095240 ) ) ;
#28176 = ADVANCED_FACE ( 'NONE', ( #29120 ), #19798, .T. ) ;
#28177 = VECTOR ( 'NONE', #22416, 1000.000000000000000 ) ;
#28178 = EDGE_CURVE ( 'NONE', #23034, #42911, #3357, .T. ) ;
#28179 = CARTESIAN_POINT ( 'NONE',  ( 2.653899356899829254, -3.657605971842851300, 6.857477569908428272 ) ) ;
#28180 = CARTESIAN_POINT ( 'NONE',  ( 1.000000000000000888, 4.472310526050767621, 6.020667617347370104 ) ) ;
#28181 = VERTEX_POINT ( 'NONE', #39073 ) ;
#28182 = FACE_OUTER_BOUND ( 'NONE', #7834, .T. ) ;
#28183 = CARTESIAN_POINT ( 'NONE',  ( 5.520433897694421610, 0.005630909886752868097, -0.01397038704729861025 ) ) ;
#28185 = EDGE_CURVE ( 'NONE', #35317, #16693, #2306, .T. ) ;
#28184 = CARTESIAN_POINT ( 'NONE',  ( 37.00000000000000711, 2.250029553613756228, -12.54989509947652060 ) ) ;
#28186 = EDGE_LOOP ( 'NONE', ( #47204, #28527, #14209, #26306 ) ) ;
#28187 = CARTESIAN_POINT ( 'NONE',  ( -8.866348673818475135, -2.306797143118023641, -13.30210064843870654 ) ) ;
#28188 = CARTESIAN_POINT ( 'NONE',  ( 2.990245332647880616, 8.248134185053359602, 1.974808303407723287 ) ) ;
#28189 = DIRECTION ( 'NONE',  ( -0.9606638835031803270, -0.06908842350339414184, -0.2689826995745334681 ) ) ;
#28190 = CARTESIAN_POINT ( 'NONE',  ( 5.530133899448235191, 0.008946569461392248762, 0.01324661008606592763 ) ) ;
#28191 = CARTESIAN_POINT ( 'NONE',  ( 0.3057689695767482618, -11.43929056598608973, 4.409323295154164768 ) ) ;
#28192 = ORIENTED_EDGE ( 'NONE', *, *, #42329, .T. ) ;
#28193 = DIRECTION ( 'NONE',  ( 0.000000000000000000, 0.000000000000000000, 1.000000000000000000 ) ) ;
#28194 = ORIENTED_EDGE ( 'NONE', *, *, #31723, .F. ) ;
#28195 = LINE ( 'NONE', #17886, #46795 ) ;
#28196 = DIRECTION ( 'NONE',  ( 0.000000000000000000, -0.2618041379715703165, 0.9651210252299775583 ) ) ;
#28197 = LINE ( 'NONE', #13533, #17070 ) ;
#28198 = DIRECTION ( 'NONE',  ( 0.6088860180392798860, 0.7932577242209933877, 0.000000000000000000 ) ) ;
#28199 = CARTESIAN_POINT ( 'NONE',  ( 2.241509619876139059, -3.850348903238759668, 6.592435552901108942 ) ) ;
#28200 = CARTESIAN_POINT ( 'NONE',  ( 2.288423627607477417, 7.560204962263206596, 1.169285315515804502 ) ) ;
#28201 = CYLINDRICAL_SURFACE ( 'NONE', #49945, 7.499999999999988454 ) ;
#28202 = ORIENTED_EDGE ( 'NONE', *, *, #32685, .T. ) ;
#28203 = EDGE_LOOP ( 'NONE', ( #40988, #7294, #31363, #32592 ) ) ;
#28204 = CARTESIAN_POINT ( 'NONE',  ( -18.69968187819808136, -4.886710041940224514, -10.96191920124609176 ) ) ;
#28205 = ORIENTED_EDGE ( 'NONE', *, *, #58899, .T. ) ;
#28207 = CARTESIAN_POINT ( 'NONE',  ( -41.00000000000000000, -25.34319448863032065, -3.012683490291699240 ) ) ;
#28206 = AXIS2_PLACEMENT_3D ( 'NONE', #24120, #64997, #49423 ) ;
#28208 = EDGE_CURVE ( 'NONE', #58059, #52387, #58060, .T. ) ;
#28209 = CARTESIAN_POINT ( 'NONE',  ( -22.28236030719477512, -1.572829798448329486, 3.345835236227606924 ) ) ;
#28210 = VERTEX_POINT ( 'NONE', #55025 ) ;
#28211 = CARTESIAN_POINT ( 'NONE',  ( 0.2801149460245130896, 5.954809120985864901, -10.70654700624296396 ) ) ;
#28212 = CARTESIAN_POINT ( 'NONE',  ( 2.639814597422737386, 1.600543348184913617, -7.600559958731728294 ) ) ;
#28213 = CARTESIAN_POINT ( 'NONE',  ( 2.931247277082686065, -1.728824746592323658, 7.672001188570254371 ) ) ;
#28214 = VERTEX_POINT ( 'NONE', #9457 ) ;
#28215 = ORIENTED_EDGE ( 'NONE', *, *, #14598, .F. ) ;
#28216 = DIRECTION ( 'NONE',  ( 0.000000000000000000, -0.5243256840888443904, -0.8515178078024941977 ) ) ;
#28217 = EDGE_LOOP ( 'NONE', ( #57017, #63008, #2367, #9521 ) ) ;
#28218 = CARTESIAN_POINT ( 'NONE',  ( 2.263328370261528999, 3.943189046766329309, 6.545781832005198808 ) ) ;
#28219 = EDGE_CURVE ( 'NONE', #43734, #23613, #20111, .T. ) ;
#28220 = VERTEX_POINT ( 'NONE', #50052 ) ;
#28221 = ORIENTED_EDGE ( 'NONE', *, *, #58271, .T. ) ;
#28222 = DIRECTION ( 'NONE',  ( 0.000000000000000000, -0.01356324068817999114, 0.9999080150203989437 ) ) ;
#28223 = CARTESIAN_POINT ( 'NONE',  ( -27.10113028276155589, -1.613062633976931837, 1.697941299269279281 ) ) ;
#28224 = AXIS2_PLACEMENT_3D ( 'NONE', #13585, #32548, #52860 ) ;
#28225 = CARTESIAN_POINT ( 'NONE',  ( -19.02967556479664069, -11.99999999999998934, 9.262893081595934602E-16 ) ) ;
#28226 = CARTESIAN_POINT ( 'NONE',  ( 0.3278977287071239699, 8.073566434006698600, -9.235688435081650383 ) ) ;
#28227 = DIRECTION ( 'NONE',  ( -1.000000000000000000, 0.000000000000000000, 0.000000000000000000 ) ) ;
#28228 = EDGE_CURVE ( 'NONE', #33360, #12400, #65637, .T. ) ;
#28229 = CARTESIAN_POINT ( 'NONE',  ( 2.665405856346779956, 5.696318245876847541, 7.686816759402912425 ) ) ;
#28230 = VERTEX_POINT ( 'NONE', #30727 ) ;
#28231 = CARTESIAN_POINT ( 'NONE',  ( 2.242819959140645913, -1.426511055719359433, 7.500446639314770181 ) ) ;
#28232 = CYLINDRICAL_SURFACE ( 'NONE', #17019, 12.74999999999999822 ) ;
#28233 = CARTESIAN_POINT ( 'NONE',  ( -2.532614230583022152, 11.30437021680556242, 4.026315189028233377 ) ) ;
#28234 = EDGE_CURVE ( 'NONE', #11746, #52407, #45815, .T. ) ;
#28235 = CARTESIAN_POINT ( 'NONE',  ( -35.05175862995318425, -0.003331684148545621671, -0.01212835938695783211 ) ) ;
#28236 = CARTESIAN_POINT ( 'NONE',  ( -22.46509356695211679, 2.840174833751863304, -3.157489876851686805 ) ) ;
#28237 = DIRECTION ( 'NONE',  ( 0.000000000000000000, -0.01356324068817992001, 0.9999080150203990547 ) ) ;
#28238 = CARTESIAN_POINT ( 'NONE',  ( 2.430348790457358632, -4.016278121583693128, -6.566563360302367869 ) ) ;
#28239 = CYLINDRICAL_SURFACE ( 'NONE', #30213, 5.000000000000000888 ) ;
#28240 = CARTESIAN_POINT ( 'NONE',  ( 0.7446945582507991102, 5.891988114924304298, 10.91757157182742510 ) ) ;
#28241 = ORIENTED_EDGE ( 'NONE', *, *, #52551, .T. ) ;
#28242 = CARTESIAN_POINT ( 'NONE',  ( 2.770579946183330478, -7.230573341413127686, -2.954332771348892273 ) ) ;
#28243 = AXIS2_PLACEMENT_3D ( 'NONE', #31955, #22306, #42247 ) ;
#28244 = EDGE_LOOP ( 'NONE', ( #46863, #35039, #61974, #22974 ) ) ;
#28245 = DIRECTION ( 'NONE',  ( 0.000000000000000000, -0.01356324068817992175, 0.9999080150203990547 ) ) ;
#28246 = CARTESIAN_POINT ( 'NONE',  ( 0.3160775863651122397, -0.2401734240703709278, 12.26075464248082802 ) ) ;
#28247 = DIRECTION ( 'NONE',  ( 0.000000000000000000, -0.1740410799127685149, -0.9847383929261604996 ) ) ;
#28248 = CARTESIAN_POINT ( 'NONE',  ( 2.000000000000001776, 5.457833520448724940, -4.281014542496488495 ) ) ;
#28249 = CARTESIAN_POINT ( 'NONE',  ( 2.963017218115627571, -4.761166637500461540, -6.272673870919139638 ) ) ;
#28250 = VERTEX_POINT ( 'NONE', #15759 ) ;
#28251 = DIRECTION ( 'NONE',  ( -1.000000000000000000, 0.000000000000000000, 0.000000000000000000 ) ) ;
#28252 = CARTESIAN_POINT ( 'NONE',  ( -41.00000000000000711, -1.694065894508600678E-18, 1.500000000000000222 ) ) ;
#28253 = CARTESIAN_POINT ( 'NONE',  ( -27.10719052120871098, 2.116547233941204809, 1.044362304621460069 ) ) ;
#28254 = DIRECTION ( 'NONE',  ( 0.000000000000000000, 0.000000000000000000, 1.000000000000000000 ) ) ;
#28255 = ADVANCED_FACE ( 'NONE', ( #164 ), #1150, .T. ) ;
#28256 = AXIS2_PLACEMENT_3D ( 'NONE', #56339, #65636, #20110 ) ;
#28257 = ADVANCED_FACE ( 'NONE', ( #42022 ), #21359, .F. ) ;
#28258 = CARTESIAN_POINT ( 'NONE',  ( -4.979815405451806676, -1.249695498034863128, -13.44307378499100913 ) ) ;
#28259 = ORIENTED_EDGE ( 'NONE', *, *, #42252, .T. ) ;
#28261 = EDGE_CURVE ( 'NONE', #19382, #63181, #57015, .T. ) ;
#28260 = LINE ( 'NONE', #53203, #9436 ) ;
#28262 = B_SPLINE_CURVE_WITH_KNOTS ( 'NONE', 3,
 ( #7988, #12606, #38886, #33570, #8297, #3326, #23599, #43869, #56119, #40164, #50506, #19590, #29865, #39854, #45487, #60139, #9570, #50176, #35517 ),
 .UNSPECIFIED., .F., .F.,
 ( 4, 3, 3, 3, 3, 3, 4 ),
 ( 7.866258489732282489E-18, 2.825908398831347771E-05, 4.208813692483994324E-05, 5.591713746943911183E-05, 6.279584083231893005E-05, 9.105792820296729282E-05, 0.0001153131102488839276 ),
 .UNSPECIFIED. ) ;
#28263 = CARTESIAN_POINT ( 'NONE',  ( 25.00000000000000355, -3.797884998337192286, 24.99999999999999289 ) ) ;
#28264 = CARTESIAN_POINT ( 'NONE',  ( -6.328161288300638176, -31.25458527548780907, 14.40172722986095977 ) ) ;
#28265 = VERTEX_POINT ( 'NONE', #36039 ) ;
#28266 = ORIENTED_EDGE ( 'NONE', *, *, #15464, .T. ) ;
#28267 = CARTESIAN_POINT ( 'NONE',  ( -27.08639648637141661, 2.215564006614429982, -0.6092497698725152233 ) ) ;
#28268 = ORIENTED_EDGE ( 'NONE', *, *, #28591, .F. ) ;
#28269 = DIRECTION ( 'NONE',  ( 0.000000000000000000, 0.000000000000000000, 1.000000000000000000 ) ) ;
#28270 = CARTESIAN_POINT ( 'NONE',  ( 2.241451721903216399, -5.809054012306823722, -4.953785420083471003 ) ) ;
#28271 = CARTESIAN_POINT ( 'NONE',  ( -27.09833916700227618, -1.689564470270175534, -1.609723001517283203 ) ) ;
#28272 = DIRECTION ( 'NONE',  ( 1.000000000000000000, 0.000000000000000000, 0.000000000000000000 ) ) ;
#28273 = CARTESIAN_POINT ( 'NONE',  ( -37.00000000000000711, -11.38112321385052716, 2.905556151562584954 ) ) ;
#28274 = ORIENTED_EDGE ( 'NONE', *, *, #46205, .T. ) ;
#28275 = ORIENTED_EDGE ( 'NONE', *, *, #47128, .T. ) ;
#28276 = VERTEX_POINT ( 'NONE', #5158 ) ;
#28277 = CARTESIAN_POINT ( 'NONE',  ( 22.36482863261543486, 11.96441317219527889, -0.9234811557364158707 ) ) ;
#28278 = EDGE_CURVE ( 'NONE', #29418, #18668, #61324, .T. ) ;
#28279 = ORIENTED_EDGE ( 'NONE', *, *, #35527, .T. ) ;
#28280 = AXIS2_PLACEMENT_3D ( 'NONE', #54706, #30705, #39380 ) ;
#28281 = FACE_OUTER_BOUND ( 'NONE', #48719, .T. ) ;
#28282 = CARTESIAN_POINT ( 'NONE',  ( 2.284126774967664364, -7.558363379199190213, 1.171808575345598902 ) ) ;
#28283 = EDGE_CURVE ( 'NONE', #3518, #42938, #15447, .T. ) ;
#28284 = EDGE_LOOP ( 'NONE', ( #4404, #49173, #4459, #54183 ) ) ;
#28285 = VECTOR ( 'NONE', #49047, 1000.000000000000000 ) ;
#28286 = DIRECTION ( 'NONE',  ( -1.000000000000000000, 0.000000000000000000, 0.000000000000000000 ) ) ;
#28287 = CARTESIAN_POINT ( 'NONE',  ( 2.257661810676420799, -2.739276463085633662, -7.131864446283250558 ) ) ;
#28288 = DIRECTION ( 'NONE',  ( 0.000000000000000000, -0.3193015301359872216, 0.9476531711827999027 ) ) ;
#28289 = ORIENTED_EDGE ( 'NONE', *, *, #20166, .T. ) ;
#28290 = VERTEX_POINT ( 'NONE', #41362 ) ;
#28291 = CARTESIAN_POINT ( 'NONE',  ( 2.241311220309554209, 2.523702734785345125, 7.205198716057793717 ) ) ;
#28292 = ORIENTED_EDGE ( 'NONE', *, *, #32203, .T. ) ;
#28293 = B_SPLINE_CURVE_WITH_KNOTS ( 'NONE', 3,
 ( #2600, #27499, #17545, #33487, #37812, #53109, #17211, #22531, #58435, #48786, #27183, #57450, #58782 ),
 .UNSPECIFIED., .F., .F.,
 ( 4, 3, 3, 3, 4 ),
 ( 3.127317220692750759E-18, 6.607593386745573051E-05, 0.0001321518677373532469, 0.0001982171734706212392, 0.0002642860854759480124 ),
 .UNSPECIFIED. ) ;
#28294 =( NAMED_UNIT ( * ) SI_UNIT ( $, .STERADIAN. ) SOLID_ANGLE_UNIT ( ) );
#28295 = ORIENTED_EDGE ( 'NONE', *, *, #37964, .F. ) ;
#28296 = EDGE_CURVE ( 'NONE', #58711, #16620, #54336, .T. ) ;
#28297 = CARTESIAN_POINT ( 'NONE',  ( 0.2650492594609250574, -4.291723947796392657, 11.46945808033132330 ) ) ;
#28298 = CARTESIAN_POINT ( 'NONE',  ( 12.62425547244439095, -33.87255953084102345, -9.995598718703821106 ) ) ;
#28299 = CARTESIAN_POINT ( 'NONE',  ( -9.668839327565212471, -32.14098936784623106, -13.07247934321342342 ) ) ;
#28300 = CARTESIAN_POINT ( 'NONE',  ( -36.00000000000000711, -5.143145423404365424, 11.66664283989678275 ) ) ;
#28301 = DIRECTION ( 'NONE',  ( 0.000000000000000000, -0.9796553971857721033, -0.2006870767258996657 ) ) ;
#28302 = CARTESIAN_POINT ( 'NONE',  ( -35.00000000000000000, -9.493370459201647904, -6.917234959366931335 ) ) ;
#28303 = ORIENTED_EDGE ( 'NONE', *, *, #32895, .F. ) ;
#28304 = CARTESIAN_POINT ( 'NONE',  ( 2.000000000000001776, 0.000000000000000000, 0.000000000000000000 ) ) ;
#28305 = ORIENTED_EDGE ( 'NONE', *, *, #36763, .T. ) ;
#28306 = CARTESIAN_POINT ( 'NONE',  ( 2.262775599886255762, -2.745802076335779329, 7.131180968652217622 ) ) ;
#28307 = DIRECTION ( 'NONE',  ( 0.000000000000000000, 0.01356324068817998940, -0.9999080150203990547 ) ) ;
#28308 = EDGE_CURVE ( 'NONE', #30406, #50365, #33438, .T. ) ;
#28309 = EDGE_CURVE ( 'NONE', #28210, #27619, #34925, .T. ) ;
#28310 = ORIENTED_EDGE ( 'NONE', *, *, #44826, .T. ) ;
#28311 = CARTESIAN_POINT ( 'NONE',  ( 5.516018279890452902, 0.006771744149385740437, 0.0002248006052446895335 ) ) ;
#28312 = CARTESIAN_POINT ( 'NONE',  ( 0.3341166715381284624, 6.352033667906601622, 10.49680960898228221 ) ) ;
#28313 = CARTESIAN_POINT ( 'NONE',  ( 2.556980015513232285, -7.578583798307022334, 1.570584617272376082 ) ) ;
#28314 = EDGE_CURVE ( 'NONE', #31078, #31872, #814, .T. ) ;
#28315 = ORIENTED_EDGE ( 'NONE', *, *, #61286, .F. ) ;
#28316 = EDGE_LOOP ( 'NONE', ( #23073, #5233, #49827, #9388 ) ) ;
#28317 = CARTESIAN_POINT ( 'NONE',  ( 35.00000000000000000, -11.10408318471055011, 6.265926637539605437 ) ) ;
#28318 = ORIENTED_EDGE ( 'NONE', *, *, #11229, .T. ) ;
#28319 = LINE ( 'NONE', #19334, #56135 ) ;
#28320 = CARTESIAN_POINT ( 'NONE',  ( -35.00000000000000000, -0.4993900848166508144, -12.17626345777664554 ) ) ;
#28321 = CARTESIAN_POINT ( 'NONE',  ( 2.241506898688419902, -1.364429914801466692, -7.511570207700573043 ) ) ;
#28322 = CARTESIAN_POINT ( 'NONE',  ( 0.2956976708475475002, -9.245952174682493308, -8.045468685197016967 ) ) ;
#28323 = CARTESIAN_POINT ( 'NONE',  ( -37.00000000000000711, -12.73293890771483028, -0.6593684648221820321 ) ) ;
#28324 = ORIENTED_EDGE ( 'NONE', *, *, #3316, .F. ) ;
#28325 = AXIS2_PLACEMENT_3D ( 'NONE', #10520, #50468, #4913 ) ;
#28326 = CARTESIAN_POINT ( 'NONE',  ( 35.00000000000000000, -10.07641281632173325, 6.036400161834665212 ) ) ;
#28327 = EDGE_CURVE ( 'NONE', #36377, #31716, #42130, .T. ) ;
#28328 = CIRCLE ( 'NONE', #45321, 5.000000000000000000 ) ;
#28329 = EDGE_CURVE ( 'NONE', #48483, #55391, #12094, .T. ) ;
#28330 = CARTESIAN_POINT ( 'NONE',  ( 3.152665057733881504, -7.719888720907738922, -1.848755561851823881 ) ) ;
#28331 = CARTESIAN_POINT ( 'NONE',  ( 35.00000000000000000, 3.307597835713413037, 12.31350058095519096 ) ) ;
#28332 = CYLINDRICAL_SURFACE ( 'NONE', #46578, 12.18649999999999878 ) ;
#28333 = CARTESIAN_POINT ( 'NONE',  ( 0.2653519789438771315, 7.888580323518872284, 9.366970421692796478 ) ) ;
#28334 = DIRECTION ( 'NONE',  ( 1.000000000000000000, -0.000000000000000000, -0.000000000000000000 ) ) ;
#28335 = CYLINDRICAL_SURFACE ( 'NONE', #37487, 7.499999999999988454 ) ;
#28336 = B_SPLINE_CURVE_WITH_KNOTS ( 'NONE', 3,
 ( #7479, #57062, #63018, #6855, #58369, #37753, #58046, #53042, #62254, #41969, #31017, #36973, #50662, #1436, #56281, #25374, #21716, #26042, #36663, #50984, #766, #51970 ),
 .UNSPECIFIED., .F., .F.,
 ( 4, 3, 3, 3, 3, 3, 3, 4 ),
 ( 1.755771606739170543E-18, 4.449119708436968942E-05, 6.626296329540460836E-05, 8.803456484962672536E-05, 0.0001098060367612812058, 0.0001315774408628522915, 0.0001760698110411187294, 0.0001829697163287838087 ),
 .UNSPECIFIED. ) ;
#28337 = VERTEX_POINT ( 'NONE', #43329 ) ;
#28338 = CARTESIAN_POINT ( 'NONE',  ( 12.84033272753670474, -11.13604314287161401, -4.475189157715393939 ) ) ;
#28339 =( BOUNDED_CURVE ( )  B_SPLINE_CURVE ( 3, ( #48945, #48615, #23675, #53611 ),
 .UNSPECIFIED., .F., .F. ) 
 B_SPLINE_CURVE_WITH_KNOTS ( ( 4, 4 ),
 ( 4.975352684836342299, 4.993910677237379581 ),
 .UNSPECIFIED. ) 
 CURVE ( )  GEOMETRIC_REPRESENTATION_ITEM ( )  RATIONAL_B_SPLINE_CURVE ( ( 1.000000000000000000, 0.9999713002824244246, 0.9999713002824244246, 1.000000000000000000 ) ) 
 REPRESENTATION_ITEM ( '' )  );
#28340 = ORIENTED_EDGE ( 'NONE', *, *, #56706, .T. ) ;
#28341 = CARTESIAN_POINT ( 'NONE',  ( 35.00000000000000000, -3.287724142101329683, 11.73463472867578972 ) ) ;
#28342 = DIRECTION ( 'NONE',  ( 0.000000000000000000, 0.01356324068817998940, -0.9999080150203989437 ) ) ;
#28343 = CARTESIAN_POINT ( 'NONE',  ( -37.25000000000000711, -1.694065894508793271E-18, 4.500000000000001776 ) ) ;
#28344 = ORIENTED_EDGE ( 'NONE', *, *, #21769, .T. ) ;
#28345 = CARTESIAN_POINT ( 'NONE',  ( 21.90174657591892071, -13.47998113580522528, -0.7349207973210680755 ) ) ;
#28346 = FACE_OUTER_BOUND ( 'NONE', #15420, .T. ) ;
#28347 = ORIENTED_EDGE ( 'NONE', *, *, #53667, .F. ) ;
#28348 = ORIENTED_EDGE ( 'NONE', *, *, #40477, .T. ) ;
#28349 = ORIENTED_EDGE ( 'NONE', *, *, #2832, .T. ) ;
#28350 = CARTESIAN_POINT ( 'NONE',  ( -35.00000000000000000, 0.000000000000000000, 0.000000000000000000 ) ) ;
#28351 = CARTESIAN_POINT ( 'NONE',  ( -22.30986928587821794, -3.392803916780404716, -1.665628047792451216 ) ) ;
#28352 = ORIENTED_EDGE ( 'NONE', *, *, #58799, .F. ) ;
#28353 = CARTESIAN_POINT ( 'NONE',  ( 2.994568964204202821, 5.775954174106932903, 5.368337437440270143 ) ) ;
#28354 = CARTESIAN_POINT ( 'NONE',  ( 3.934515826361683288, 5.928730106699989122, 12.13052178345963128 ) ) ;
#28355 = DIRECTION ( 'NONE',  ( 0.000000000000000000, 0.000000000000000000, 1.000000000000000000 ) ) ;
#28356 = CARTESIAN_POINT ( 'NONE',  ( 18.73357960737152794, 5.263351130133424149, 10.79392331976826291 ) ) ;
#28357 = EDGE_CURVE ( 'NONE', #52828, #40351, #19287, .T. ) ;
#28358 = EDGE_LOOP ( 'NONE', ( #60426, #17655, #29735, #40906 ) ) ;
#28359 = CARTESIAN_POINT ( 'NONE',  ( 0.3632410797595234664, -7.689504457927717418, 9.572936598843597267 ) ) ;
#28360 = AXIS2_PLACEMENT_3D ( 'NONE', #2133, #42670, #48369 ) ;
#28361 = CARTESIAN_POINT ( 'NONE',  ( 14.32183389819027930, -34.49933334076765590, 8.089813643623637418 ) ) ;
#28362 = CARTESIAN_POINT ( 'NONE',  ( -35.00000000000000000, -2.627174906296831480, -11.44858830469743083 ) ) ;
#28364 = VERTEX_POINT ( 'NONE', #32372 ) ;
#28363 = CARTESIAN_POINT ( 'NONE',  ( 5.520433897694421610, 0.01432141647227111458, 0.004666464468078371577 ) ) ;
#28365 = FACE_OUTER_BOUND ( 'NONE', #62688, .T. ) ;
#28366 = ORIENTED_EDGE ( 'NONE', *, *, #11066, .T. ) ;
#28367 = CARTESIAN_POINT ( 'NONE',  ( -18.87309976548205626, 13.48469254801326755, -0.9257068828140080363 ) ) ;
#28368 = ORIENTED_EDGE ( 'NONE', *, *, #13241, .T. ) ;
#28369 = AXIS2_PLACEMENT_3D ( 'NONE', #29589, #18676, #33927 ) ;
#28370 = CARTESIAN_POINT ( 'NONE',  ( 2.241537034860907163, 7.175668896091129234, -2.606707005150471268 ) ) ;
#28371 = DIRECTION ( 'NONE',  ( 0.000000000000000000, 0.01356324068817992175, -0.9999080150203990547 ) ) ;
#28372 = DIRECTION ( 'NONE',  ( 1.000000000000000000, -0.000000000000000000, 0.000000000000000000 ) ) ;
#28373 = CARTESIAN_POINT ( 'NONE',  ( 0.3632410797595285179, -3.951633449030989009, 11.62558329798850210 ) ) ;
#28374 = EDGE_CURVE ( 'NONE', #51860, #36273, #14341, .T. ) ;
#28375 = DIRECTION ( 'NONE',  ( 1.000000000000000000, 0.000000000000000000, 0.000000000000000000 ) ) ;
#28376 = AXIS2_PLACEMENT_3D ( 'NONE', #49246, #36102, #24264 ) ;
#28377 = CARTESIAN_POINT ( 'NONE',  ( -6.973115560797586099, -1.808105581326604705, -13.37853677315561285 ) ) ;
#28378 = DIRECTION ( 'NONE',  ( -1.000000000000000000, -0.000000000000000000, -0.000000000000000000 ) ) ;
#28379 = ORIENTED_EDGE ( 'NONE', *, *, #2236, .T. ) ;
#28380 = CARTESIAN_POINT ( 'NONE',  ( 35.00000000000000000, -5.273331777780263074, 10.49591321039685887 ) ) ;
#28381 = ORIENTED_EDGE ( 'NONE', *, *, #49618, .T. ) ;
#28382 = EDGE_CURVE ( 'NONE', #34331, #40350, #34114, .T. ) ;
#28383 = ORIENTED_EDGE ( 'NONE', *, *, #58285, .T. ) ;
#28384 = CARTESIAN_POINT ( 'NONE',  ( 5.514970785353741078, -0.004233694591582531745, 0.002093325033904006385 ) ) ;
#28385 = CARTESIAN_POINT ( 'NONE',  ( -22.31328051695926007, 3.401210163132566411, 1.671726071983929307 ) ) ;
#28386 = CARTESIAN_POINT ( 'NONE',  ( 1.719304012338199517, 0.000000000000000000, 0.000000000000000000 ) ) ;
#28387 = CARTESIAN_POINT ( 'NONE',  ( 0.2801149460245113687, -10.51028947658249102, 6.294737133725765155 ) ) ;
#28388 = CARTESIAN_POINT ( 'NONE',  ( 36.00000000000000711, 11.90598845858539967, 4.561791185930283099 ) ) ;
#28389 = EDGE_CURVE ( 'NONE', #52228, #19449, #51146, .T. ) ;
#28390 = DIRECTION ( 'NONE',  ( 0.000000000000000000, 0.7621620551276377942, -0.6473862847818260269 ) ) ;
#28391 = CARTESIAN_POINT ( 'NONE',  ( 2.241352910868908754, -1.243507963608043498, -7.532448145350521429 ) ) ;
#28392 = ORIENTED_EDGE ( 'NONE', *, *, #20887, .T. ) ;
#28393 = CARTESIAN_POINT ( 'NONE',  ( 37.00000000000000711, 4.705694406421931860E-17, -3.469127814946512892E-15 ) ) ;
#28394 = CARTESIAN_POINT ( 'NONE',  ( -27.08429572838383947, -1.338867938658200307, -1.859677275556420151 ) ) ;
#28395 = CARTESIAN_POINT ( 'NONE',  ( 6.511148368283224741, -4.283242813471564325, -11.20980722696366882 ) ) ;
#28396 = EDGE_CURVE ( 'NONE', #6864, #59141, #42328, .T. ) ;
#28397 = VECTOR ( 'NONE', #45962, 1000.000000000000000 ) ;
#28398 = CARTESIAN_POINT ( 'NONE',  ( 2.263328370261536548, -4.802372801874533081, 5.944174889971110431 ) ) ;
#28399 = LINE ( 'NONE', #48699, #7830 ) ;
#28400 = CARTESIAN_POINT ( 'NONE',  ( 0.3675815128205912052, -11.62724744438068569, 3.951233083390429446 ) ) ;
#28401 = CARTESIAN_POINT ( 'NONE',  ( 5.516018279890452902, -0.004525000489649737799, -0.005042957932158631355 ) ) ;
#28402 = ORIENTED_EDGE ( 'NONE', *, *, #7177, .T. ) ;
#28403 = CARTESIAN_POINT ( 'NONE',  ( 5.520433897694421610, 0.01473594271720288749, -0.003119431460922268435 ) ) ;
#28404 = CARTESIAN_POINT ( 'NONE',  ( 5.515188684475870851, 0.004893136156457782680, 0.002166413411657369063 ) ) ;
#28405 = CARTESIAN_POINT ( 'NONE',  ( -35.04582288351658548, 0.0001464581944843601751, 0.01270482153514039536 ) ) ;
#28406 = EDGE_CURVE ( 'NONE', #1560, #64905, #45330, .T. ) ;
#28407 = AXIS2_PLACEMENT_3D ( 'NONE', #27452, #26472, #11828 ) ;
#28408 = CARTESIAN_POINT ( 'NONE',  ( -27.32343372485685506, -0.1402256980610406267, 3.007804754713657047 ) ) ;
#28409 = CARTESIAN_POINT ( 'NONE',  ( 35.00000000000000000, 11.13736569743274174, -4.946702696913213515 ) ) ;
#28410 = ORIENTED_EDGE ( 'NONE', *, *, #58000, .F. ) ;
#28411 = CARTESIAN_POINT ( 'NONE',  ( -18.06472325377715649, 4.740409429902864069, 12.64225488003265774 ) ) ;
#28412 = CARTESIAN_POINT ( 'NONE',  ( 2.262775599885878730, -4.802882839669280202, -5.943524836196611538 ) ) ;
#28413 = CARTESIAN_POINT ( 'NONE',  ( 36.00000000000000711, 10.39746860227901060, 7.379373053628751400 ) ) ;
#28414 = ORIENTED_EDGE ( 'NONE', *, *, #58874, .F. ) ;
#28415 = DIRECTION ( 'NONE',  ( 0.000000000000000000, -0.9651210252299821102, -0.2618041379715529970 ) ) ;
#28416 = CARTESIAN_POINT ( 'NONE',  ( 0.2653141334712556532, -4.229817350136338305, -11.49252672845887879 ) ) ;
#28417 = ORIENTED_EDGE ( 'NONE', *, *, #36258, .F. ) ;
#28419 = ORIENTED_EDGE ( 'NONE', *, *, #64471, .T. ) ;
#28418 = B_SPLINE_CURVE_WITH_KNOTS ( 'NONE', 3,
 ( #8530, #24478, #3589, #64382, #64069, #18552, #28822, #34119, #13513, #49131, #39114, #59406, #49459, #3898, #44415, #44755, #65036, #29780, #35438 ),
 .UNSPECIFIED., .F., .F.,
 ( 4, 3, 3, 3, 3, 3, 4 ),
 ( 0.000000000000000000, 2.831840207499612970E-05, 4.217266859840534770E-05, 5.602024318396014053E-05, 6.290810167969230950E-05, 9.120440630945263866E-05, 0.0001153103026479760220 ),
 .UNSPECIFIED. ) ;
#28420 = FACE_OUTER_BOUND ( 'NONE', #37977, .T. ) ;
#28421 = VERTEX_POINT ( 'NONE', #14384 ) ;
#28422 = CARTESIAN_POINT ( 'NONE',  ( 35.00000000000000000, 7.379373053628867751, -10.39746860227893244 ) ) ;
#28423 = CYLINDRICAL_SURFACE ( 'NONE', #3895, 4.999999999999999112 ) ;
#28424 = CARTESIAN_POINT ( 'NONE',  ( 35.00000000000000000, 12.26766708251991389, -3.473736367725300589 ) ) ;
#28425 = FACE_OUTER_BOUND ( 'NONE', #12915, .T. ) ;
#28426 = EDGE_CURVE ( 'NONE', #37783, #27549, #35265, .T. ) ;
#28427 = CYLINDRICAL_SURFACE ( 'NONE', #14024, 2.899999999999994582 ) ;
#28428 = DIRECTION ( 'NONE',  ( 0.000000000000000000, 0.000000000000000000, 1.000000000000000000 ) ) ;
#28430 = ORIENTED_EDGE ( 'NONE', *, *, #56271, .T. ) ;
#28429 = LINE ( 'NONE', #22135, #7497 ) ;
#28431 = EDGE_CURVE ( 'NONE', #5947, #34267, #33690, .T. ) ;
#28432 = DIRECTION ( 'NONE',  ( -1.000000000000000000, 0.000000000000000000, 0.000000000000000000 ) ) ;
#28433 = ORIENTED_EDGE ( 'NONE', *, *, #5712, .F. ) ;
#28434 = CARTESIAN_POINT ( 'NONE',  ( 0.2653141617321038148, 10.62747662594938625, -6.084921229689308042 ) ) ;
#28435 = VERTEX_POINT ( 'NONE', #38691 ) ;
#28436 = EDGE_LOOP ( 'NONE', ( #28110, #48328, #35380, #20175 ) ) ;
#28437 = CARTESIAN_POINT ( 'NONE',  ( -26.62724309483121488, 12.18261572180475127, 5.817022916452319059 ) ) ;
#28438 = CARTESIAN_POINT ( 'NONE',  ( 1.074417311476293380, -26.55384113566742599, 16.22365110280896161 ) ) ;
#28439 = AXIS2_PLACEMENT_3D ( 'NONE', #44543, #64823, #35564 ) ;
#28440 = CARTESIAN_POINT ( 'NONE',  ( -24.31937550808052251, 10.15575759614895190, 8.896613522854025291 ) ) ;
#28441 = ADVANCED_FACE ( 'NONE', ( #23738 ), #19729, .T. ) ;
#28442 = DIRECTION ( 'NONE',  ( -0.3865475372811021937, -0.4778122177791984115, -0.7888450329201792677 ) ) ;
#28443 = CARTESIAN_POINT ( 'NONE',  ( 2.000000000000001776, 5.888698556700773246, 3.665823448873418045 ) ) ;
#28444 = CARTESIAN_POINT ( 'NONE',  ( -27.08418322526030764, 0.8335872080609603163, -2.134267017050449855 ) ) ;
#28445 = VERTEX_POINT ( 'NONE', #3799 ) ;
#28446 = AXIS2_PLACEMENT_3D ( 'NONE', #6438, #42301, #1783 ) ;
#28447 = DIRECTION ( 'NONE',  ( 0.000000000000000000, 0.8009703041134145218, 0.5987040770935704304 ) ) ;
#28448 = CARTESIAN_POINT ( 'NONE',  ( 1.372161826076017554, -3.755740169579909526, 12.04315837901270925 ) ) ;
#28449 = DIRECTION ( 'NONE',  ( 0.000000000000000000, 0.01356324068817998940, -0.9999080150203989437 ) ) ;
#28450 = VERTEX_POINT ( 'NONE', #58994 ) ;
#28451 = CYLINDRICAL_SURFACE ( 'NONE', #48121, 7.499999999999988454 ) ;
#28452 = AXIS2_PLACEMENT_3D ( 'NONE', #32046, #57676, #1813 ) ;
#28453 = ORIENTED_EDGE ( 'NONE', *, *, #59076, .T. ) ;
#28454 = LINE ( 'NONE', #18167, #50796 ) ;
#28455 = CARTESIAN_POINT ( 'NONE',  ( 0.2911222467163511185, -10.50411792397754773, -6.312159098066288720 ) ) ;
#28456 = CARTESIAN_POINT ( 'NONE',  ( 0.2638984909335720941, 12.24571285024409129, -0.1991813963114424380 ) ) ;
#28457 = CARTESIAN_POINT ( 'NONE',  ( 29.35982233226165405, 7.748204631658820674, 11.05532493772648195 ) ) ;
#28458 = FACE_OUTER_BOUND ( 'NONE', #56779, .T. ) ;
#28459 = CARTESIAN_POINT ( 'NONE',  ( -27.09150307427447757, -1.909742362151675810, 1.305148381377976730 ) ) ;
#28460 = EDGE_CURVE ( 'NONE', #29500, #39372, #2484, .T. ) ;
#28461 = DIRECTION ( 'NONE',  ( 0.000000000000000000, -0.2149704402110318713, 0.9766205557100849921 ) ) ;
#28462 = ORIENTED_EDGE ( 'NONE', *, *, #18832, .T. ) ;
#28463 = CARTESIAN_POINT ( 'NONE',  ( -17.54726996257253191, 12.93490414535030020, 3.865003848717349033 ) ) ;
#28464 = ORIENTED_EDGE ( 'NONE', *, *, #63377, .F. ) ;
#28465 = LINE ( 'NONE', #13491, #29585 ) ;
#28466 = LINE ( 'NONE', #50076, #53112 ) ;
#28467 = CARTESIAN_POINT ( 'NONE',  ( -35.00000000000000000, 0.000000000000000000, 0.000000000000000000 ) ) ;
#28468 = FACE_OUTER_BOUND ( 'NONE', #21678, .T. ) ;
#28469 = CARTESIAN_POINT ( 'NONE',  ( 37.00000000000000711, -8.766823244861932096, 7.817610399097601359 ) ) ;
#28470 = EDGE_LOOP ( 'NONE', ( #50543, #38971, #23615, #42986 ) ) ;
#28471 = AXIS2_PLACEMENT_3D ( 'NONE', #14136, #18820, #3869 ) ;
#28472 = CARTESIAN_POINT ( 'NONE',  ( 5.195242505075158057, -10.34130555456374445, -8.684426116891836855 ) ) ;
#28473 = CARTESIAN_POINT ( 'NONE',  ( -35.00000000000000000, -11.30684963584386082, -4.545979934229532837 ) ) ;
#28474 = CARTESIAN_POINT ( 'NONE',  ( 2.251152103363645463, 1.449454666117730106, 7.498874008626764009 ) ) ;
#28475 = PLANE ( 'NONE',  #3152 ) ;
#28476 = ORIENTED_EDGE ( 'NONE', *, *, #43699, .T. ) ;
#28477 = CARTESIAN_POINT ( 'NONE',  ( 2.844750968615173292, -6.210802026111876373, -4.777247819183616073 ) ) ;
#28478 = LINE ( 'NONE', #38124, #55537 ) ;
#28479 = CARTESIAN_POINT ( 'NONE',  ( -23.18047892478189098, 0.4043282704081693768, -4.776019214182026573 ) ) ;
#28480 = CARTESIAN_POINT ( 'NONE',  ( -31.50196089333760696, -3.063567359192253647, -24.19471064305901464 ) ) ;
#28481 = AXIS2_PLACEMENT_3D ( 'NONE', #3642, #28227, #48518 ) ;
#28482 = EDGE_CURVE ( 'NONE', #54635, #24055, #15046, .T. ) ;
#28483 = CARTESIAN_POINT ( 'NONE',  ( -27.08417142187571613, -0.4261087887162083865, -2.251180450989576531 ) ) ;
#28484 = CARTESIAN_POINT ( 'NONE',  ( 1.459561108994067880, -4.912799202119574105, -11.65083230253670799 ) ) ;
#28485 = CIRCLE ( 'NONE', #11493, 4.999999999999999112 ) ;
#28486 = CIRCLE ( 'NONE', #55067, 12.18650000000000055 ) ;
#28487 = ORIENTED_EDGE ( 'NONE', *, *, #4959, .F. ) ;
#28488 = CARTESIAN_POINT ( 'NONE',  ( 2.000000000000001776, -1.225832621831797420, -6.827324998361596009 ) ) ;
#28489 = CYLINDRICAL_SURFACE ( 'NONE', #13137, 5.683183579532407492 ) ;
#28490 = CARTESIAN_POINT ( 'NONE',  ( -0.5153900578009965594, -25.72562925869133821, -15.66323518044676000 ) ) ;
#28491 = EDGE_LOOP ( 'NONE', ( #25440, #64786, #8507, #57146 ) ) ;
#28492 = CIRCLE ( 'NONE', #45481, 5.000000000000000888 ) ;
#28493 = CARTESIAN_POINT ( 'NONE',  ( 5.514624014163232779, -0.003830004412313258323, -0.001574979445068878025 ) ) ;
#28494 = CARTESIAN_POINT ( 'NONE',  ( 2.350038591458374793, 10.33030559206027021, 2.471682575235019996 ) ) ;
#28495 = DIRECTION ( 'NONE',  ( 0.000000000000000000, 0.000000000000000000, -1.000000000000000000 ) ) ;
#28496 = CIRCLE ( 'NONE', #55078, 4.999999999999999112 ) ;
#28497 = DIRECTION ( 'NONE',  ( 0.000000000000000000, -0.6269146997508042718, -0.7790879021242460567 ) ) ;
#28498 = FACE_OUTER_BOUND ( 'NONE', #586, .T. ) ;
#28499 = EDGE_CURVE ( 'NONE', #62589, #7316, #49014, .T. ) ;
#28500 = CARTESIAN_POINT ( 'NONE',  ( 35.00000000000000000, -12.60630747491661552, 1.908798535168510169 ) ) ;
#28501 = ORIENTED_EDGE ( 'NONE', *, *, #47031, .F. ) ;
#28502 = CARTESIAN_POINT ( 'NONE',  ( 2.262775599886256650, -7.227769107232058232, 2.480428346600510370 ) ) ;
#28503 = DIRECTION ( 'NONE',  ( 0.000000000000000000, -1.000000000000000000, 0.000000000000000000 ) ) ;
#28504 = DIRECTION ( 'NONE',  ( 0.000000000000000000, -0.5155538571770110767, -0.8568571761675956022 ) ) ;
#28505 = CARTESIAN_POINT ( 'NONE',  ( 0.3675815128205912052, -9.235491948679950269, -8.093875121226169256 ) ) ;
#28506 = DIRECTION ( 'NONE',  ( 1.000000000000000000, 0.000000000000000000, 0.000000000000000000 ) ) ;
#28507 = DIRECTION ( 'NONE',  ( 0.000000000000000000, 0.01356324068817998940, -0.9999080150203990547 ) ) ;
#28508 = EDGE_CURVE ( 'NONE', #36243, #5675, #59963, .T. ) ;
#28509 = CARTESIAN_POINT ( 'NONE',  ( -26.43258404273187523, 2.854888342447774896, 1.987083010659142612 ) ) ;
#28510 = CARTESIAN_POINT ( 'NONE',  ( -35.00000000000000000, -2.905556151562544986, -11.38112321385053960 ) ) ;
#28511 = ORIENTED_EDGE ( 'NONE', *, *, #43176, .T. ) ;
#28512 = EDGE_CURVE ( 'NONE', #42779, #22257, #34172, .T. ) ;
#28513 = EDGE_LOOP ( 'NONE', ( #16232, #43892, #49311, #15383 ) ) ;
#28514 = FACE_OUTER_BOUND ( 'NONE', #45477, .T. ) ;
#28515 = ORIENTED_EDGE ( 'NONE', *, *, #5829, .F. ) ;
#28516 = CARTESIAN_POINT ( 'NONE',  ( -22.29978294495153790, 2.590262069787980348, -2.710748743830168284 ) ) ;
#28517 = CARTESIAN_POINT ( 'NONE',  ( 2.941278708680199916, -6.068329152486382938, 0.9331242451664794046 ) ) ;
#28518 = VECTOR ( 'NONE', #53536, 1000.000000000000000 ) ;
#28519 = EDGE_CURVE ( 'NONE', #15374, #63832, #55447, .T. ) ;
#28520 = DIRECTION ( 'NONE',  ( 0.000000000000000000, 0.01356324068817998940, -0.9999080150203990547 ) ) ;
#28521 = VERTEX_POINT ( 'NONE', #44314 ) ;
#28522 = DIRECTION ( 'NONE',  ( 0.000000000000000000, 0.01356324068817998940, -0.9999080150203990547 ) ) ;
#28523 = CARTESIAN_POINT ( 'NONE',  ( 2.705197763288546220, 1.627208841526562422, -7.617149697727725766 ) ) ;
#28524 = AXIS2_PLACEMENT_3D ( 'NONE', #55367, #5167, #51394 ) ;
#28526 = EDGE_CURVE ( 'NONE', #55514, #62548, #52239, .T. ) ;
#28525 = CARTESIAN_POINT ( 'NONE',  ( 3.047904605210430162, -1.788881754552591241, 7.698174516567103609 ) ) ;
#28527 = ORIENTED_EDGE ( 'NONE', *, *, #9097, .F. ) ;
#28528 = ORIENTED_EDGE ( 'NONE', *, *, #51808, .T. ) ;
#28529 = DIRECTION ( 'NONE',  ( 1.000000000000000000, -0.000000000000000000, 0.000000000000000000 ) ) ;
#28530 = ORIENTED_EDGE ( 'NONE', *, *, #23587, .F. ) ;
#28531 = CARTESIAN_POINT ( 'NONE',  ( 1.937114397841932290, 9.228205347192453445, 8.920887662793502315 ) ) ;
#28532 = ORIENTED_EDGE ( 'NONE', *, *, #18157, .T. ) ;
#28534 = EDGE_CURVE ( 'NONE', #18362, #4143, #31004, .T. ) ;
#28533 = ORIENTED_EDGE ( 'NONE', *, *, #27664, .F. ) ;
#28535 = CARTESIAN_POINT ( 'NONE',  ( 5.514970785353741078, -0.0003039746380524631733, 0.004713149585127259823 ) ) ;
#28537 = VECTOR ( 'NONE', #32009, 1000.000000000000000 ) ;
#28536 = CARTESIAN_POINT ( 'NONE',  ( 35.00000000000000000, 11.24036214326529048, 6.018036132182036368 ) ) ;
#28538 = CARTESIAN_POINT ( 'NONE',  ( 0.2717059086739037066, 10.51822005842002916, -6.276007891175617637 ) ) ;
#28539 = DIRECTION ( 'NONE',  ( 1.000000000000000000, 0.000000000000000000, -0.000000000000000000 ) ) ;
#28540 = DIRECTION ( 'NONE',  ( 0.000000000000000000, 1.000000000000000000, 0.000000000000000000 ) ) ;
#28541 = EDGE_CURVE ( 'NONE', #25112, #16758, #8760, .T. ) ;
#28542 = DIRECTION ( 'NONE',  ( 1.000000000000000000, 0.000000000000000000, 0.000000000000000000 ) ) ;
#28543 = CIRCLE ( 'NONE', #7172, 4.999999999999999112 ) ;
#28544 = ORIENTED_EDGE ( 'NONE', *, *, #47616, .T. ) ;
#28545 =( BOUNDED_SURFACE ( )  B_SPLINE_SURFACE ( 3, 1, ( 
 ( #16829, #56079 ),
 ( #6874, #16518 ),
 ( #56414, #41772 ),
 ( #27144, #20520 ) ),
 .UNSPECIFIED., .F., .F., .F. ) 
 B_SPLINE_SURFACE_WITH_KNOTS ( ( 4, 4 ),
 ( 2, 2 ),
 ( 0.000000000000000000, 1.000000000000000000 ),
 ( 0.000000000000000000, 1.000000000000000000 ),
 .UNSPECIFIED. ) 
 GEOMETRIC_REPRESENTATION_ITEM ( )  RATIONAL_B_SPLINE_SURFACE ( (
 ( 1.000000000000000000, 1.000000000000000000),
 ( 0.9856612449720755231, 0.9999558406602322425),
 ( 0.9856612449720755231, 0.9999558406602322425),
 ( 1.000000000000000000, 1.000000000000000000) ) ) 
 REPRESENTATION_ITEM ( '' )  SURFACE ( )  );
#28546 = CARTESIAN_POINT ( 'NONE',  ( 35.00000000000000000, 4.705694406421931860E-17, -3.469127814946512892E-15 ) ) ;
#28547 = DIRECTION ( 'NONE',  ( -1.000000000000000000, 0.000000000000000000, 0.000000000000000000 ) ) ;
#28548 = EDGE_CURVE ( 'NONE', #52495, #15087, #3411, .T. ) ;
#28549 = CARTESIAN_POINT ( 'NONE',  ( -19.62940142185039250, -13.44226311714747624, -1.286935523930725855 ) ) ;
#28550 = DIRECTION ( 'NONE',  ( 0.000000000000000000, 0.7621620551276333533, 0.6473862847818313560 ) ) ;
#28551 = CARTESIAN_POINT ( 'NONE',  ( -18.48287316985193485, 13.41107218970293147, 1.582951252990374202 ) ) ;
#28552 = CARTESIAN_POINT ( 'NONE',  ( 2.000000000000001776, 3.341639490130849488, -6.078525953551423555 ) ) ;
#28553 = CARTESIAN_POINT ( 'NONE',  ( 2.368238019615270140, -3.992969450835600398, -6.556525400300609263 ) ) ;
#28554 = DIRECTION ( 'NONE',  ( -1.000000000000000000, 0.000000000000000000, 0.000000000000000000 ) ) ;
#28555 = AXIS2_PLACEMENT_3D ( 'NONE', #14787, #5178, #65659 ) ;
#28556 = FACE_OUTER_BOUND ( 'NONE', #9511, .T. ) ;
#28557 = ORIENTED_EDGE ( 'NONE', *, *, #65090, .T. ) ;
#28558 = DIRECTION ( 'NONE',  ( -1.000000000000000000, -1.836970198721029688E-16, -0.000000000000000000 ) ) ;
#28559 = ORIENTED_EDGE ( 'NONE', *, *, #42118, .T. ) ;
#28560 = CARTESIAN_POINT ( 'NONE',  ( 2.827825597296799387, 7.528560921609640744, 4.975864478227443932 ) ) ;
#28561 = CARTESIAN_POINT ( 'NONE',  ( 0.2956976708475471116, -0.2200030809426427036, 12.25433786972505068 ) ) ;
#28562 = CARTESIAN_POINT ( 'NONE',  ( -37.00000000000000711, 0.000000000000000000, 0.000000000000000000 ) ) ;
#28563 = DIRECTION ( 'NONE',  ( -1.000000000000000000, 0.000000000000000000, 0.000000000000000000 ) ) ;
#28564 = CARTESIAN_POINT ( 'NONE',  ( 35.00000000000000000, 4.705694406421931860E-17, -3.469127814946512892E-15 ) ) ;
#28565 = ORIENTED_EDGE ( 'NONE', *, *, #18332, .F. ) ;
#28566 = CARTESIAN_POINT ( 'NONE',  ( 0.8320506296491552156, 10.57268643647783257, -6.546053790694065455 ) ) ;
#28567 = DIRECTION ( 'NONE',  ( 0.000000000000000000, 0.000000000000000000, 1.000000000000000000 ) ) ;
#28568 = DIRECTION ( 'NONE',  ( 1.000000000000000000, -0.000000000000000000, 0.000000000000000000 ) ) ;
#28569 = CARTESIAN_POINT ( 'NONE',  ( -22.31328051695926007, 2.748895659348141507, 2.608921479762082551 ) ) ;
#28570 = EDGE_CURVE ( 'NONE', #27227, #31240, #54953, .T. ) ;
#28571 = EDGE_CURVE ( 'NONE', #24263, #25850, #35956, .T. ) ;
#28572 = VECTOR ( 'NONE', #30595, 1000.000000000000000 ) ;
#28573 = DIRECTION ( 'NONE',  ( -1.000000000000000000, 0.000000000000000000, 0.000000000000000000 ) ) ;
#28574 = ORIENTED_EDGE ( 'NONE', *, *, #55147, .F. ) ;
#28575 = AXIS2_PLACEMENT_3D ( 'NONE', #55636, #20707, #30018 ) ;
#28576 = CARTESIAN_POINT ( 'NONE',  ( 37.00000000000000711, -11.53507381115584529, -2.216820770815045805 ) ) ;
#28577 = CARTESIAN_POINT ( 'NONE',  ( 1.459561108993784773, -8.601340491611450645, -9.267924853468695545 ) ) ;
#28578 = CARTESIAN_POINT ( 'NONE',  ( -35.00000000000000000, 0.000000000000000000, 0.000000000000000000 ) ) ;
#28579 = EDGE_CURVE ( 'NONE', #21209, #37865, #5533, .T. ) ;
#28580 = ADVANCED_FACE ( 'NONE', ( #15680 ), #26331, .T. ) ;
#28581 = ORIENTED_EDGE ( 'NONE', *, *, #1379, .T. ) ;
#28582 = ORIENTED_EDGE ( 'NONE', *, *, #64340, .T. ) ;
#28583 = LINE ( 'NONE', #18304, #58412 ) ;
#28584 = AXIS2_PLACEMENT_3D ( 'NONE', #46179, #45840, #36163 ) ;
#28585 = ORIENTED_EDGE ( 'NONE', *, *, #11650, .F. ) ;
#28586 = CARTESIAN_POINT ( 'NONE',  ( 0.000000000000000000, 6.936109781200682889, 2.853135311045038591 ) ) ;
#28587 = CARTESIAN_POINT ( 'NONE',  ( 2.994568964204206818, -3.591541975631920014, -7.020079750321929879 ) ) ;
#28588 = DIRECTION ( 'NONE',  ( 1.000000000000000000, -0.000000000000000000, 0.000000000000000000 ) ) ;
#28589 = CARTESIAN_POINT ( 'NONE',  ( -35.04660725145885891, 0.01184012236748180000, 0.003326400506015331823 ) ) ;
#28590 = ORIENTED_EDGE ( 'NONE', *, *, #1547, .F. ) ;
#28591 = EDGE_CURVE ( 'NONE', #37175, #27686, #36303, .T. ) ;
#28592 = ORIENTED_EDGE ( 'NONE', *, *, #60811, .T. ) ;
#28593 = ORIENTED_EDGE ( 'NONE', *, *, #442, .T. ) ;
#28594 = B_SPLINE_CURVE_WITH_KNOTS ( 'NONE', 3,
 ( #15823, #50123, #50771, #4579, #10510, #30786, #45128, #21151, #65389, #5220, #36100, #5901, #19853, #40115, #45776, #572, #60407, #46432, #55429 ),
 .UNSPECIFIED., .F., .F.,
 ( 4, 3, 3, 3, 3, 3, 4 ),
 ( 0.000000000000000000, 2.831840207499706144E-05, 4.217266859840659453E-05, 5.602024318396192946E-05, 6.290810167969514198E-05, 9.120440630945896769E-05, 0.0001153103026479763472 ),
 .UNSPECIFIED. ) ;
#28595 = CYLINDRICAL_SURFACE ( 'NONE', #12874, 7.499999999999988454 ) ;
#28596 = LINE ( 'NONE', #13313, #3490 ) ;
#28597 = EDGE_LOOP ( 'NONE', ( #23420, #54682, #21776, #52400 ) ) ;
#28598 = CARTESIAN_POINT ( 'NONE',  ( -35.00000000000000000, 0.000000000000000000, 0.000000000000000000 ) ) ;
#28599 = CARTESIAN_POINT ( 'NONE',  ( -22.31213670151049300, -0.2530575063955998738, -3.777944311993719051 ) ) ;
#28600 = ORIENTED_EDGE ( 'NONE', *, *, #30086, .F. ) ;
#28601 = CARTESIAN_POINT ( 'NONE',  ( 2.241352910868908754, 6.569501556381497132, -3.889181972941381460 ) ) ;
#28603 = EDGE_CURVE ( 'NONE', #39315, #15531, #25417, .T. ) ;
#28602 = CARTESIAN_POINT ( 'NONE',  ( 35.00000000000000000, -5.015831474386232891, 10.62137734850272786 ) ) ;
#28604 = CARTESIAN_POINT ( 'NONE',  ( 0.000000000000000000, 0.000000000000000000, 7.500000000000000000 ) ) ;
#28605 = VERTEX_POINT ( 'NONE', #35316 ) ;
#28606 = ORIENTED_EDGE ( 'NONE', *, *, #19104, .T. ) ;
#28607 = CARTESIAN_POINT ( 'NONE',  ( 2.251139882113958546, 2.495216312514881185, 7.218573619021348975 ) ) ;
#28609 = EDGE_LOOP ( 'NONE', ( #59875, #48645, #23393, #51218 ) ) ;
#28608 = EDGE_CURVE ( 'NONE', #13628, #42786, #15088, .T. ) ;
#28610 = FACE_OUTER_BOUND ( 'NONE', #10292, .T. ) ;
#28611 = ORIENTED_EDGE ( 'NONE', *, *, #13202, .T. ) ;
#28612 = ADVANCED_BREP_SHAPE_REPRESENTATION ( '', ( #29035, #24966 ), #48383 ) ;
#28613 = ORIENTED_EDGE ( 'NONE', *, *, #40748, .T. ) ;
#28614 = CARTESIAN_POINT ( 'NONE',  ( 0.2652384529303165039, -4.126283314267649160, 11.53005674806960279 ) ) ;
#28615 = EDGE_CURVE ( 'NONE', #60283, #37661, #30947, .T. ) ;
#28616 = LINE ( 'NONE', #49578, #59560 ) ;
#28617 = DIRECTION ( 'NONE',  ( 0.000000000000000000, 0.2355298848897447450, 0.9718671068226475418 ) ) ;
#28619 = CARTESIAN_POINT ( 'NONE',  ( -47.00000000000000711, 0.000000000000000000, 0.000000000000000000 ) ) ;
#28618 = VECTOR ( 'NONE', #63081, 1000.000000000000000 ) ;
#28620 = CARTESIAN_POINT ( 'NONE',  ( 2.000000000000001776, -0.2704997240204360387, -6.931223712253490987 ) ) ;
#28621 = CARTESIAN_POINT ( 'NONE',  ( 1.198791140419175338, -0.5160125886328382760, 12.54673713002897628 ) ) ;
#28622 = VERTEX_POINT ( 'NONE', #15373 ) ;
#28623 = EDGE_CURVE ( 'NONE', #12171, #32174, #50960, .T. ) ;
#28624 = CARTESIAN_POINT ( 'NONE',  ( 0.2648978790185584908, 6.008231198268983775, 10.67083876753494032 ) ) ;
#28625 = VERTEX_POINT ( 'NONE', #428 ) ;
#28626 = CIRCLE ( 'NONE', #24388, 12.18650000000000233 ) ;
#28627 = CARTESIAN_POINT ( 'NONE',  ( -47.00000000000000711, 0.000000000000000000, 0.000000000000000000 ) ) ;
#28628 = DIRECTION ( 'NONE',  ( -1.000000000000000000, 0.000000000000000000, 0.000000000000000000 ) ) ;
#28629 = EDGE_CURVE ( 'NONE', #49321, #30406, #20697, .T. ) ;
#28630 = ORIENTED_EDGE ( 'NONE', *, *, #20140, .F. ) ;
#28631 = CARTESIAN_POINT ( 'NONE',  ( 37.00000000000000711, 5.428340790341704469, -10.91072401419412863 ) ) ;
#28632 = CARTESIAN_POINT ( 'NONE',  ( 5.516018279890452902, 0.002527316374434305981, 0.006286471671801938804 ) ) ;
#28633 = CARTESIAN_POINT ( 'NONE',  ( 0.3610902822527300993, -2.389900346488009308, -12.04327049858142296 ) ) ;
#28634 = AXIS2_PLACEMENT_3D ( 'NONE', #52064, #49318, #38975 ) ;
#28635 = ORIENTED_EDGE ( 'NONE', *, *, #62031, .F. ) ;
#28636 = ORIENTED_EDGE ( 'NONE', *, *, #29089, .T. ) ;
#28637 = LINE ( 'NONE', #7713, #64029 ) ;
#28638 = AXIS2_PLACEMENT_3D ( 'NONE', #3685, #24918, #14899 ) ;
#28639 = ORIENTED_EDGE ( 'NONE', *, *, #29765, .F. ) ;
#28640 = CARTESIAN_POINT ( 'NONE',  ( -25.45090860874581296, -12.10390572719422586, 5.980235094230700987 ) ) ;
#28641 = DIRECTION ( 'NONE',  ( 0.000000000000000000, 0.01356324068817992175, -0.9999080150203990547 ) ) ;
#28642 = CARTESIAN_POINT ( 'NONE',  ( 2.241451721903216843, -1.265761656830151294, -7.528807736569459230 ) ) ;
#28643 = CARTESIAN_POINT ( 'NONE',  ( -3.138774296833683586, 10.80513712183324238, 5.223565235433476950 ) ) ;
#28644 = CARTESIAN_POINT ( 'NONE',  ( 12.58250891015083539, 8.987906597619184978, -7.961848984263494522 ) ) ;
#28645 = ORIENTED_EDGE ( 'NONE', *, *, #3335, .F. ) ;
#28646 = VECTOR ( 'NONE', #10602, 1000.000000000000000 ) ;
#28647 = CARTESIAN_POINT ( 'NONE',  ( 1.109979610370192882, 1.701361252869143748, 12.41172293674641480 ) ) ;
#28648 = ADVANCED_FACE ( 'NONE', ( #14895 ), #19268, .T. ) ;
#28649 = ADVANCED_FACE ( 'NONE', ( #59499 ), #29244, .T. ) ;
#28650 = CARTESIAN_POINT ( 'NONE',  ( 3.100650473569524390, -7.709402782713551616, -1.818095316078554902 ) ) ;
#28651 = CARTESIAN_POINT ( 'NONE',  ( 25.05309951391468459, 10.77522019223767558, -8.132934882857098202 ) ) ;
#28652 = CARTESIAN_POINT ( 'NONE',  ( -27.08429572838383947, -0.9410937941433956677, 2.089332284968712816 ) ) ;
#28653 = CARTESIAN_POINT ( 'NONE',  ( -37.00000000000000711, 10.07641281632186114, -6.036400161834460043 ) ) ;
#28654 = CARTESIAN_POINT ( 'NONE',  ( 6.848819816998693355, -8.369264212050962826, -8.610838094864671888 ) ) ;
#28655 = CARTESIAN_POINT ( 'NONE',  ( -37.00000000000000711, -3.511814412392038953, -11.66953048682403171 ) ) ;
#28656 = EDGE_CURVE ( 'NONE', #3635, #10611, #35187, .T. ) ;
#28657 = CIRCLE ( 'NONE', #25475, 12.73084802173761787 ) ;
#28658 = CIRCLE ( 'NONE', #5326, 6.936499999999990784 ) ;
#28659 = VERTEX_POINT ( 'NONE', #39866 ) ;
#28660 = CARTESIAN_POINT ( 'NONE',  ( 2.290907136833253421, -0.1622757685885619361, 7.649199419879185946 ) ) ;
#28661 = EDGE_LOOP ( 'NONE', ( #1154, #34121, #29188, #59855 ) ) ;
#28662 = CARTESIAN_POINT ( 'NONE',  ( 2.305787727787084407, 7.654065630109506913, 0.1666591538752955071 ) ) ;
#28663 = CARTESIAN_POINT ( 'NONE',  ( 37.00000000000000711, -8.927548052240835474, 8.295159312811946961 ) ) ;
#28664 = DIRECTION ( 'NONE',  ( -0.000000000000000000, -0.000000000000000000, -1.000000000000000000 ) ) ;
#28665 = CARTESIAN_POINT ( 'NONE',  ( -27.16190680910943200, 11.80725687591872841, -2.143550592226123985 ) ) ;
#28666 = ORIENTED_EDGE ( 'NONE', *, *, #65797, .T. ) ;
#28667 = EDGE_CURVE ( 'NONE', #38752, #9242, #40535, .T. ) ;
#28668 = EDGE_LOOP ( 'NONE', ( #27986, #12696, #10523, #18722 ) ) ;
#28669 = ORIENTED_EDGE ( 'NONE', *, *, #39843, .F. ) ;
#28670 = CARTESIAN_POINT ( 'NONE',  ( 0.2676618633000442116, -7.748413788583150996, -9.484212776852418258 ) ) ;
#28671 = EDGE_CURVE ( 'NONE', #22363, #4226, #20375, .T. ) ;
#28672 = VECTOR ( 'NONE', #5561, 1000.000000000000000 ) ;
#28673 = LINE ( 'NONE', #32654, #59265 ) ;
#28674 = ORIENTED_EDGE ( 'NONE', *, *, #3840, .F. ) ;
#28675 = CARTESIAN_POINT ( 'NONE',  ( 3.047904605210421281, 5.772373816836818605, 5.398304302092557627 ) ) ;
#28676 = CARTESIAN_POINT ( 'NONE',  ( 2.931247277082682956, -3.034789039497238772, 7.255238984871613894 ) ) ;
#28677 = CIRCLE ( 'NONE', #4350, 2.899999999999994582 ) ;
#28678 = CARTESIAN_POINT ( 'NONE',  ( 0.3675815128205894289, -1.872154644482002528, -12.13672785388552100 ) ) ;
#28679 = FACE_OUTER_BOUND ( 'NONE', #38175, .T. ) ;
#28680 = ORIENTED_EDGE ( 'NONE', *, *, #38674, .T. ) ;
#28681 = LINE ( 'NONE', #64567, #41557 ) ;
#28682 = CARTESIAN_POINT ( 'NONE',  ( 12.85491158824215496, -28.99999999999999645, 3.284771503683511007 ) ) ;
#28683 = CARTESIAN_POINT ( 'NONE',  ( 2.297017764050093724, -1.490897313050634665, -7.506328781223021274 ) ) ;
#28685 = VERTEX_POINT ( 'NONE', #50519 ) ;
#28684 = CARTESIAN_POINT ( 'NONE',  ( -28.67667724226168602, 0.4371157725390067972, -1.840944188131425907 ) ) ;
#28686 = CARTESIAN_POINT ( 'NONE',  ( 0.3040950598368144520, -12.11647736519422480, 1.881452845810337227 ) ) ;
#28687 = VERTEX_POINT ( 'NONE', #20235 ) ;
#28688 = CARTESIAN_POINT ( 'NONE',  ( -19.94256134539602243, 13.21349453248879868, -2.782655092070258629 ) ) ;
#28689 = AXIS2_PLACEMENT_3D ( 'NONE', #61084, #16185, #10522 ) ;
#28690 = VERTEX_POINT ( 'NONE', #3980 ) ;
#28691 = CARTESIAN_POINT ( 'NONE',  ( -35.00000000000000000, 0.000000000000000000, 0.000000000000000000 ) ) ;
#28692 = CARTESIAN_POINT ( 'NONE',  ( -35.00000000000000000, 3.287724142101577485, -11.73463472867572932 ) ) ;
#28693 = EDGE_CURVE ( 'NONE', #59877, #54376, #53328, .T. ) ;
#28694 = CARTESIAN_POINT ( 'NONE',  ( 1.452237505248552996, -8.579708443906808313, 9.303501428255998462 ) ) ;
#28695 = DIRECTION ( 'NONE',  ( 1.000000000000000000, 0.000000000000000000, 0.000000000000000000 ) ) ;
#28696 = CYLINDRICAL_SURFACE ( 'NONE', #12316, 2.899999999999994582 ) ;
#28697 = CARTESIAN_POINT ( 'NONE',  ( -9.026820310266758796, -3.106532851708875942, -13.13844627572322921 ) ) ;
#28698 = CARTESIAN_POINT ( 'NONE',  ( 11.13635633779574974, 13.44934996100431235, -1.173364222693725756 ) ) ;
#28699 = EDGE_CURVE ( 'NONE', #5463, #64491, #57112, .T. ) ;
#28700 = AXIS2_PLACEMENT_3D ( 'NONE', #63932, #23374, #29989 ) ;
#28701 = VERTEX_POINT ( 'NONE', #4646 ) ;
#28702 = DIRECTION ( 'NONE',  ( 0.000000000000000000, -0.8835120444460272671, 0.4684084406997819916 ) ) ;
#28703 = ORIENTED_EDGE ( 'NONE', *, *, #5304, .T. ) ;
#28704 = EDGE_CURVE ( 'NONE', #11282, #65463, #204, .T. ) ;
#28705 = ORIENTED_EDGE ( 'NONE', *, *, #16306, .F. ) ;
#28706 = DIRECTION ( 'NONE',  ( -1.000000000000000000, 0.000000000000000000, 0.000000000000000000 ) ) ;
#28707 = CARTESIAN_POINT ( 'NONE',  ( 5.514970785353741078, -0.003415090918276209378, -0.003262412238248218153 ) ) ;
#28708 = DIRECTION ( 'NONE',  ( 1.000000000000000000, -0.000000000000000000, 0.000000000000000000 ) ) ;
#28709 = CARTESIAN_POINT ( 'NONE',  ( 0.2717059086739011531, -10.51822005841999363, 6.276007891175692244 ) ) ;
#28710 = B_SPLINE_CURVE_WITH_KNOTS ( 'NONE', 3,
 ( #65686, #20491, #46105, #36081, #36761, #37978, #56387, #36435, #22712, #61059, #62042, #51746, #15488, #35754, #56747, #11171, #21129, #31756 ),
 .UNSPECIFIED., .F., .F.,
 ( 4, 2, 2, 2, 2, 2, 2, 2, 4 ),
 ( 0.000000000000000000, 0.0007305591798604922594, 0.001461118359720984519, 0.002191677539581471466, 0.002922236719441957328, 0.003652795899302445359, 0.004383355079162932523, 0.005113914259023420554, 0.005844473438883908585 ),
 .UNSPECIFIED. ) ;
#28711 = CARTESIAN_POINT ( 'NONE',  ( 2.000000000000001776, 6.643843315911800218, 1.507714007300793968 ) ) ;
#28712 = FACE_OUTER_BOUND ( 'NONE', #14810, .T. ) ;
#28713 = AXIS2_PLACEMENT_3D ( 'NONE', #14149, #8850, #29143 ) ;
#28714 = VECTOR ( 'NONE', #50021, 1000.000000000000000 ) ;
#28715 = ADVANCED_FACE ( 'NONE', ( #55156 ), #23942, .T. ) ;
#28716 = CARTESIAN_POINT ( 'NONE',  ( 35.00000000000000000, -7.110831038798346881, -9.896810808925367908 ) ) ;
#28717 = ORIENTED_EDGE ( 'NONE', *, *, #38351, .T. ) ;
#28718 = DIRECTION ( 'NONE',  ( 1.000000000000000000, -0.000000000000000000, -0.000000000000000000 ) ) ;
#28719 = CARTESIAN_POINT ( 'NONE',  ( -27.08418179957658367, -1.521007404704310950, -1.713622993062714928 ) ) ;
#28720 = CARTESIAN_POINT ( 'NONE',  ( 37.00000000000000711, 4.705694406421931860E-17, -3.469127814946512892E-15 ) ) ;
#28721 = VECTOR ( 'NONE', #34408, 1000.000000000000000 ) ;
#28722 = DIRECTION ( 'NONE',  ( 1.000000000000000000, 0.000000000000000000, -0.000000000000000000 ) ) ;
#28723 = CARTESIAN_POINT ( 'NONE',  ( 37.00000000000000711, -6.036400161834636791, -10.07641281632175634 ) ) ;
#28724 = B_SPLINE_CURVE_WITH_KNOTS ( 'NONE', 3,
 ( #6395, #47301, #12022, #26665, #6081, #36959, #42944, #16376, #32612, #6731, #57933, #2400, #26339, #22679, #1418, #46624 ),
 .UNSPECIFIED., .F., .F.,
 ( 4, 3, 3, 3, 3, 4 ),
 ( 2.359668567760217409E-15, 0.0002126834539179711864, 0.0004253519300366280878, 0.0006380165497224201841, 0.0007442707582428287685, 0.0009453531351417518609 ),
 .UNSPECIFIED. ) ;
#28725 = CIRCLE ( 'NONE', #32979, 12.18649999999999878 ) ;
#28726 = EDGE_CURVE ( 'NONE', #58057, #48505, #34847, .T. ) ;
#28727 =( BOUNDED_SURFACE ( )  B_SPLINE_SURFACE ( 3, 1, ( 
 ( #52115, #21863 ),
 ( #22510, #57428 ),
 ( #57108, #38109 ),
 ( #16543, #21532 ) ),
 .UNSPECIFIED., .F., .F., .F. ) 
 B_SPLINE_SURFACE_WITH_KNOTS ( ( 4, 4 ),
 ( 2, 2 ),
 ( 0.000000000000000000, 1.000000000000000000 ),
 ( 0.000000000000000000, 1.000000000000000000 ),
 .UNSPECIFIED. ) 
 GEOMETRIC_REPRESENTATION_ITEM ( )  RATIONAL_B_SPLINE_SURFACE ( (
 ( 1.000000000000000000, 1.000000000000000000),
 ( 0.8716676215708681896, 0.8964445200148164483),
 ( 0.8716676215708681896, 0.8964445200148164483),
 ( 1.000000000000000000, 1.000000000000000000) ) ) 
 REPRESENTATION_ITEM ( '' )  SURFACE ( )  );
#28728 = CARTESIAN_POINT ( 'NONE',  ( -10.21802740604751669, -3.732897637691882320, 12.97489559727909025 ) ) ;
#28729 = B_SPLINE_CURVE_WITH_KNOTS ( 'NONE', 3,
 ( #48327, #47334, #11720, #42625, #46999, #57640, #62268, #18044, #42293, #26705, #53296, #63569, #58629, #1456, #41988, #47642 ),
 .UNSPECIFIED., .F., .F.,
 ( 4, 3, 3, 3, 3, 4 ),
 ( 0.000000000000000000, 0.0002999043160758100364, 0.0005998071753052480184, 0.0008997092107376780147, 0.001204458948196762691, 0.001510329163478534020 ),
 .UNSPECIFIED. ) ;
#28730 = B_SPLINE_CURVE_WITH_KNOTS ( 'NONE', 3,
 ( #51554, #26256, #21255, #32525, #27231, #52531, #43170, #57178, #33200, #36880, #62797, #47526, #26912, #11606, #22239, #16610, #47211, #63446, #31875, #58488, #41870, #57510 ),
 .UNSPECIFIED., .F., .F.,
 ( 4, 3, 3, 3, 3, 3, 3, 4 ),
 ( 1.764953265579307567E-18, 4.449119708436791404E-05, 6.626296329540252127E-05, 8.803456484962348630E-05, 0.0001098060367612760559, 0.0001315774408628449731, 0.0001760698110411088632, 0.0001829697163287805290 ),
 .UNSPECIFIED. ) ;
#28731 = EDGE_LOOP ( 'NONE', ( #17563, #64609, #28945, #43216 ) ) ;
#28732 = DIRECTION ( 'NONE',  ( 1.000000000000000000, -0.000000000000000000, 0.000000000000000000 ) ) ;
#28733 = DIRECTION ( 'NONE',  ( -1.000000000000000000, 0.000000000000000000, 0.000000000000000000 ) ) ;
#28734 = CARTESIAN_POINT ( 'NONE',  ( -37.00000000000000711, 0.000000000000000000, 0.000000000000000000 ) ) ;
#28735 = AXIS2_PLACEMENT_3D ( 'NONE', #10618, #56179, #6646 ) ;
#28736 = FACE_OUTER_BOUND ( 'NONE', #60316, .T. ) ;
#28737 = CARTESIAN_POINT ( 'NONE',  ( 1.719304012338517706, -0.7661785589593724799, 12.70777170744426243 ) ) ;
#28738 = VECTOR ( 'NONE', #40295, 1000.000000000000000 ) ;
#28739 = ORIENTED_EDGE ( 'NONE', *, *, #41878, .F. ) ;
#28740 = DIRECTION ( 'NONE',  ( 0.000000000000000000, 0.5155538571770171830, 0.8568571761675919385 ) ) ;
#28741 = CARTESIAN_POINT ( 'NONE',  ( 2.000000000000001776, -7.414200355365264450, 1.131208685655129775 ) ) ;
#28742 = CARTESIAN_POINT ( 'NONE',  ( -22.27834755396593991, -2.876353066242412382, 2.305389312780939726 ) ) ;
#28743 = VERTEX_POINT ( 'NONE', #8630 ) ;
#28744 = CARTESIAN_POINT ( 'NONE',  ( 24.16725417678432564, 10.72501634808748605, -8.203748878436343261 ) ) ;
#28745 = VECTOR ( 'NONE', #39057, 1000.000000000000000 ) ;
#28746 = CARTESIAN_POINT ( 'NONE',  ( 35.00000000000000000, -10.80478261802177897, 5.636262487437428526 ) ) ;
#28747 = EDGE_LOOP ( 'NONE', ( #40121, #46681, #47207, #34236 ) ) ;
#28748 = EDGE_CURVE ( 'NONE', #13308, #28265, #54843, .T. ) ;
#28749 = ORIENTED_EDGE ( 'NONE', *, *, #41138, .F. ) ;
#28750 = DIRECTION ( 'NONE',  ( -1.000000000000000000, -0.000000000000000000, 0.000000000000000000 ) ) ;
#28751 = EDGE_CURVE ( 'NONE', #3064, #62086, #64473, .T. ) ;
#28752 = AXIS2_PLACEMENT_3D ( 'NONE', #36074, #56379, #31111 ) ;
#28753 = AXIS2_PLACEMENT_3D ( 'NONE', #3661, #60132, #55137 ) ;
#28754 = AXIS2_PLACEMENT_3D ( 'NONE', #42723, #36093, #16163 ) ;
#28755 = ORIENTED_EDGE ( 'NONE', *, *, #14467, .F. ) ;
#28756 = LINE ( 'NONE', #33425, #31277 ) ;
#28757 = DIRECTION ( 'NONE',  ( 0.000000000000000000, -0.4134677391718385997, -0.9105187689796011563 ) ) ;
#28758 = CARTESIAN_POINT ( 'NONE',  ( 35.00000000000000000, 4.705694406421931860E-17, -3.469127814946512892E-15 ) ) ;
#28759 = CARTESIAN_POINT ( 'NONE',  ( 25.00000000000000355, -30.00000000000000000, 1.530808498934191521E-15 ) ) ;
#28760 = CONICAL_SURFACE ( 'NONE', #37247, 5.135612550275435062, 1.249045772030607848 ) ;
#28761 = CARTESIAN_POINT ( 'NONE',  ( 1.719304012338199517, 12.20344780065974888, 3.626341562670754914 ) ) ;
#28763 = VERTEX_POINT ( 'NONE', #39205 ) ;
#28762 = CARTESIAN_POINT ( 'NONE',  ( 0.4626703367443176229, 7.694993290995472357, 9.611037151103300147 ) ) ;
#28764 = EDGE_LOOP ( 'NONE', ( #19785, #35681, #15021, #64773 ) ) ;
#28765 = DIRECTION ( 'NONE',  ( -1.000000000000000000, 0.000000000000000000, -0.000000000000000000 ) ) ;
#28766 = ORIENTED_EDGE ( 'NONE', *, *, #4620, .F. ) ;
#28767 = VERTEX_POINT ( 'NONE', #13926 ) ;
#28768 = CARTESIAN_POINT ( 'NONE',  ( -25.10024331987605706, 9.207671482944922658, 9.878016613807114155 ) ) ;
#28769 = CARTESIAN_POINT ( 'NONE',  ( -12.89187373143239945, -28.36023352766247996, 12.94763553493058872 ) ) ;
#28770 = EDGE_CURVE ( 'NONE', #41816, #32188, #42119, .T. ) ;
#28771 = CARTESIAN_POINT ( 'NONE',  ( -3.966091003153757288, 8.436959275399312119, 8.545114390545426986 ) ) ;
#28772 = DIRECTION ( 'NONE',  ( -1.000000000000000000, 0.000000000000000000, 0.000000000000000000 ) ) ;
#28773 = DIRECTION ( 'NONE',  ( -1.000000000000000000, 0.000000000000000000, 0.000000000000000000 ) ) ;
#28774 = CARTESIAN_POINT ( 'NONE',  ( 2.247112776669943468, 5.923998863710314922, 4.818685025483229190 ) ) ;
#28776 = ORIENTED_EDGE ( 'NONE', *, *, #44511, .T. ) ;
#28775 = AXIS2_PLACEMENT_3D ( 'NONE', #65508, #10992, #31274 ) ;
#28777 = CIRCLE ( 'NONE', #37262, 5.000000000000001776 ) ;
#28778 = CARTESIAN_POINT ( 'NONE',  ( -28.67667724226168602, 1.812862320140632866, -0.5419187306520724112 ) ) ;
#28779 = VERTEX_POINT ( 'NONE', #65133 ) ;
#28780 = FACE_OUTER_BOUND ( 'NONE', #40449, .T. ) ;
#28781 = CARTESIAN_POINT ( 'NONE',  ( 37.00000000000000711, -5.143145423404195782, 11.66664283989685025 ) ) ;
#28782 = AXIS2_PLACEMENT_3D ( 'NONE', #36188, #38077, #56494 ) ;
#28783 = DIRECTION ( 'NONE',  ( -1.000000000000000000, 0.000000000000000000, 0.000000000000000000 ) ) ;
#28784 = VERTEX_POINT ( 'NONE', #24911 ) ;
#28785 = AXIS2_PLACEMENT_3D ( 'NONE', #55866, #10297, #50880 ) ;
#28786 = CARTESIAN_POINT ( 'NONE',  ( 2.241536586108912932, -1.319514354261248190, 7.519576125149805890 ) ) ;
#28787 = CARTESIAN_POINT ( 'NONE',  ( 0.3053067050349188016, 0.2307671807673981057, -12.25734436043224207 ) ) ;
#28788 = CARTESIAN_POINT ( 'NONE',  ( 0.3675815128205894289, -8.093875121226139058, 9.235491948679980467 ) ) ;
#28789 = CARTESIAN_POINT ( 'NONE',  ( 37.00000000000000711, -11.91791701451268004, -2.544412758415803388 ) ) ;
#28790 = EDGE_CURVE ( 'NONE', #25468, #65390, #64289, .T. ) ;
#28791 = DIRECTION ( 'NONE',  ( 0.000000000000000000, 0.000000000000000000, 1.000000000000000000 ) ) ;
#28792 = PLANE ( 'NONE',  #38062 ) ;
#28793 = CARTESIAN_POINT ( 'NONE',  ( 35.00000000000000000, 10.70999494708492250, -5.814360711498331113 ) ) ;
#28794 = CIRCLE ( 'NONE', #30862, 7.499999999999988454 ) ;
#28795 = ORIENTED_EDGE ( 'NONE', *, *, #28154, .T. ) ;
#28796 = ORIENTED_EDGE ( 'NONE', *, *, #22945, .T. ) ;
#28797 = AXIS2_PLACEMENT_3D ( 'NONE', #45348, #44676, #55983 ) ;
#28798 = CARTESIAN_POINT ( 'NONE',  ( 0.000000000000000000, 6.606214214351110670, -2.114938770769863030 ) ) ;
#28799 = DIRECTION ( 'NONE',  ( 0.000000000000000000, -0.7617968321374946061, -0.6478160128811867313 ) ) ;
#28800 = CARTESIAN_POINT ( 'NONE',  ( 0.2653141334712571520, -11.52266042163704185, -4.147025708564540558 ) ) ;
#28801 = AXIS2_PLACEMENT_3D ( 'NONE', #60469, #54191, #61442 ) ;
#28802 = CIRCLE ( 'NONE', #17125, 250.0000000000000000 ) ;
#28803 = CARTESIAN_POINT ( 'NONE',  ( 35.00000000000000000, 1.463443770872944194, 12.09831040184922024 ) ) ;
#28804 = VECTOR ( 'NONE', #11882, 1000.000000000000000 ) ;
#28805 = CARTESIAN_POINT ( 'NONE',  ( 37.00000000000000711, 12.42372387097886488, 2.865935305911484932 ) ) ;
#28806 = EDGE_CURVE ( 'NONE', #16743, #25074, #12963, .T. ) ;
#28807 = CARTESIAN_POINT ( 'NONE',  ( -27.35552965826136429, -1.320216934008378473, -2.810569013793753346 ) ) ;
#28808 = CARTESIAN_POINT ( 'NONE',  ( 35.00000000000000000, -10.42955799785315563, 6.303578524887051948 ) ) ;
#28809 = LINE ( 'NONE', #32795, #14990 ) ;
#28810 = EDGE_CURVE ( 'NONE', #634, #29257, #25695, .T. ) ;
#28811 = DIRECTION ( 'NONE',  ( -0.8214942970785323872, -0.5702167306099040767, 0.000000000000000000 ) ) ;
#28812 = ORIENTED_EDGE ( 'NONE', *, *, #59371, .T. ) ;
#28813 = CARTESIAN_POINT ( 'NONE',  ( 2.653899356899201312, -6.118160465318636554, -4.792827201941096682 ) ) ;
#28814 = CARTESIAN_POINT ( 'NONE',  ( 0.000000000000000000, 7.484036900328569608, -0.4890722589968761191 ) ) ;
#28815 = CARTESIAN_POINT ( 'NONE',  ( 0.9232058338315058954, 12.46548196349786153, -0.3773051331668420549 ) ) ;
#28816 = VECTOR ( 'NONE', #11196, 1000.000000000000000 ) ;
#28817 = AXIS2_PLACEMENT_3D ( 'NONE', #1445, #56968, #11392 ) ;
#28818 = B_SPLINE_CURVE_WITH_KNOTS ( 'NONE', 3,
 ( #34709, #5138, #50376, #24417, #45359, #55993, #15094, #35373 ),
 .UNSPECIFIED., .F., .F.,
 ( 4, 2, 2, 4 ),
 ( 0.000000000000000000, 0.0003639104015150019687, 0.0007278208030300039374, 0.001455641606060010477 ),
 .UNSPECIFIED. ) ;
#28819 = EDGE_CURVE ( 'NONE', #43133, #43985, #1655, .T. ) ;
#28820 = AXIS2_PLACEMENT_3D ( 'NONE', #57444, #32148, #52472 ) ;
#28821 = CARTESIAN_POINT ( 'NONE',  ( -27.08419642509983305, -0.4837273216074956528, -2.239682169453958149 ) ) ;
#28822 = CARTESIAN_POINT ( 'NONE',  ( 2.251139882113958546, -5.929826121559315766, 4.813633939919417237 ) ) ;
#28823 = ORIENTED_EDGE ( 'NONE', *, *, #1040, .F. ) ;
#28824 = CARTESIAN_POINT ( 'NONE',  ( 2.305787727787083519, -2.461236246751120849, 7.249469779319902329 ) ) ;
#28825 = CARTESIAN_POINT ( 'NONE',  ( 1.937114397841932290, -0.9020203649532572143, 12.80345148322678916 ) ) ;
#28826 = CARTESIAN_POINT ( 'NONE',  ( -8.775649586809111113, -28.78513225414021903, -9.890132258253695241 ) ) ;
#28827 = ORIENTED_EDGE ( 'NONE', *, *, #11762, .F. ) ;
#28828 = CARTESIAN_POINT ( 'NONE',  ( -17.90080902915205741, 4.123225404297082619, -12.85650399841923708 ) ) ;
#28829 = FACE_OUTER_BOUND ( 'NONE', #18991, .T. ) ;
#28830 = DIRECTION ( 'NONE',  ( -0.3865475372811021382, -0.7888450329201776023, 0.4778122177792011316 ) ) ;
#28831 = EDGE_CURVE ( 'NONE', #34453, #26248, #30126, .T. ) ;
#28832 = CIRCLE ( 'NONE', #21380, 12.18649999999999700 ) ;
#28833 = FACE_OUTER_BOUND ( 'NONE', #40217, .T. ) ;
#28834 = CARTESIAN_POINT ( 'NONE',  ( -9.824294270242463156, -12.26381755720376709, -5.646954415730274235 ) ) ;
#28835 = DIRECTION ( 'NONE',  ( 1.000000000000000000, 0.000000000000000000, -0.000000000000000000 ) ) ;
#28836 = ORIENTED_EDGE ( 'NONE', *, *, #41962, .F. ) ;
#28837 = CYLINDRICAL_SURFACE ( 'NONE', #13187, 5.000000000000000888 ) ;
#28838 = CIRCLE ( 'NONE', #182, 12.18650000000000055 ) ;
#28839 = CARTESIAN_POINT ( 'NONE',  ( 35.00000000000000000, 4.705694406421931860E-17, -3.469127814946512892E-15 ) ) ;
#28840 = DIRECTION ( 'NONE',  ( -1.000000000000000000, -0.000000000000000000, -0.000000000000000000 ) ) ;
#28841 = CARTESIAN_POINT ( 'NONE',  ( 3.031336079629829872, -4.750429016921644099, 6.309383307296737797 ) ) ;
#28842 = CARTESIAN_POINT ( 'NONE',  ( 37.00000000000000711, 4.705694406421931860E-17, -3.469127814946512892E-15 ) ) ;
#28843 = LINE ( 'NONE', #33514, #39523 ) ;
#28844 = CARTESIAN_POINT ( 'NONE',  ( -23.41523303002442091, 3.856096202952873142, 2.683951991546253524 ) ) ;
#28845 = DIRECTION ( 'NONE',  ( -0.000000000000000000, -1.000000000000000000, -0.000000000000000000 ) ) ;
#28846 = AXIS2_PLACEMENT_3D ( 'NONE', #3111, #63268, #7761 ) ;
#28847 = VERTEX_POINT ( 'NONE', #15583 ) ;
#28848 = ORIENTED_EDGE ( 'NONE', *, *, #34870, .T. ) ;
#28849 = SURFACE_SIDE_STYLE ('',( #48494 ) ) ;
#28850 = ORIENTED_EDGE ( 'NONE', *, *, #35958, .F. ) ;
#28851 = DIRECTION ( 'NONE',  ( -1.000000000000000000, 0.000000000000000000, 0.000000000000000000 ) ) ;
#28852 = CARTESIAN_POINT ( 'NONE',  ( 2.350038591458111004, -10.18214835919901873, 3.024612895785461664 ) ) ;
#28853 = AXIS2_PLACEMENT_3D ( 'NONE', #7347, #19216, #54804 ) ;
#28854 = AXIS2_PLACEMENT_3D ( 'NONE', #17787, #53026, #58353 ) ;
#28855 = CARTESIAN_POINT ( 'NONE',  ( -22.28350523959500862, -1.580062893038977068, 3.346230442873244559 ) ) ;
#28856 = ORIENTED_EDGE ( 'NONE', *, *, #23736, .F. ) ;
#28857 = DIRECTION ( 'NONE',  ( 0.000000000000000000, 0.9970832820307037325, 0.07632122047556839928 ) ) ;
#28858 = CARTESIAN_POINT ( 'NONE',  ( 0.9232058338315058954, -11.84276737136198321, -3.908895078357639274 ) ) ;
#28859 = CARTESIAN_POINT ( 'NONE',  ( 2.269879328257228490, -5.026125315665611382, -5.759117113707886482 ) ) ;
#28860 = VERTEX_POINT ( 'NONE', #320 ) ;
#28861 = VERTEX_POINT ( 'NONE', #963 ) ;
#28862 = DIRECTION ( 'NONE',  ( 1.000000000000000000, -0.000000000000000000, -0.000000000000000000 ) ) ;
#28863 = DIRECTION ( 'NONE',  ( 0.000000000000000000, 0.01356324068817998940, -0.9999080150203990547 ) ) ;
#28864 = ORIENTED_EDGE ( 'NONE', *, *, #42434, .F. ) ;
#28865 = ORIENTED_EDGE ( 'NONE', *, *, #20552, .T. ) ;
#28866 = AXIS2_PLACEMENT_3D ( 'NONE', #34219, #9940, #30222 ) ;
#28867 = DIRECTION ( 'NONE',  ( -1.000000000000000000, 0.000000000000000000, 0.000000000000000000 ) ) ;
#28868 = CARTESIAN_POINT ( 'NONE',  ( -27.08639648637162267, -1.614109828501627097, 1.635407781268140237 ) ) ;
#28869 = EDGE_CURVE ( 'NONE', #19813, #21025, #51195, .T. ) ;
#28870 = AXIS2_PLACEMENT_3D ( 'NONE', #5281, #54529, #24908 ) ;
#28871 = CARTESIAN_POINT ( 'NONE',  ( -27.08456565417852246, -2.282055114149002417, 0.2166646653333839379 ) ) ;
#28872 = DIRECTION ( 'NONE',  ( 0.000000000000000000, 0.4198891015602656540, -0.9075754196709564514 ) ) ;
#28873 = CYLINDRICAL_SURFACE ( 'NONE', #24261, 1.499999999999997780 ) ;
#28874 = CIRCLE ( 'NONE', #51201, 4.999999999999998224 ) ;
#28875 = CARTESIAN_POINT ( 'NONE',  ( 1.000000000000000888, 3.224464355699941720, -6.771471746881976728 ) ) ;
#28876 = VERTEX_POINT ( 'NONE', #36539 ) ;
#28877 = CARTESIAN_POINT ( 'NONE',  ( 41.00000000000000711, -25.03188948156373783, 4.499999999999997335 ) ) ;
#28878 = CARTESIAN_POINT ( 'NONE',  ( -18.08686583997218378, 5.371948137514286792, 10.73321488716334215 ) ) ;
#28879 = CIRCLE ( 'NONE', #3416, 12.75000000000000178 ) ;
#28880 = CARTESIAN_POINT ( 'NONE',  ( 2.000000000000001776, -2.469490258309361419, -6.482025155313371201 ) ) ;
#28881 = CARTESIAN_POINT ( 'NONE',  ( -47.00000000000000711, 0.000000000000000000, 0.000000000000000000 ) ) ;
#28882 = CARTESIAN_POINT ( 'NONE',  ( 1.719304012340734822, -3.626341562669572305, -12.20344780066098345 ) ) ;
#28883 = CARTESIAN_POINT ( 'NONE',  ( -27.09229696323388481, 1.607344345646389172, -1.666734935102333948 ) ) ;
#28884 = AXIS2_PLACEMENT_3D ( 'NONE', #8504, #15127, #28791 ) ;
#28885 = CARTESIAN_POINT ( 'NONE',  ( -27.08426504710140392, 1.591094357919273117, 1.649100202714188779 ) ) ;
#28886 = CYLINDRICAL_SURFACE ( 'NONE', #53590, 12.18650000000000055 ) ;
#28887 = DIRECTION ( 'NONE',  ( 0.000000000000000000, 0.000000000000000000, 1.000000000000000000 ) ) ;
#28888 = ADVANCED_FACE ( 'NONE', ( #55513 ), #62146, .F. ) ;
#28889 = ORIENTED_EDGE ( 'NONE', *, *, #65648, .T. ) ;
#28890 = DIRECTION ( 'NONE',  ( 1.000000000000000000, -0.000000000000000000, 0.000000000000000000 ) ) ;
#28891 = AXIS2_PLACEMENT_3D ( 'NONE', #13414, #7789, #8435 ) ;
#28892 = ORIENTED_EDGE ( 'NONE', *, *, #21629, .T. ) ;
#28893 = EDGE_CURVE ( 'NONE', #60970, #13659, #39490, .T. ) ;
#28894 = CARTESIAN_POINT ( 'NONE',  ( 37.00000000000000711, 4.603882218679549609, -10.80631716521668828 ) ) ;
#28895 = CYLINDRICAL_SURFACE ( 'NONE', #9609, 4.999999999999999112 ) ;
#28896 = DIRECTION ( 'NONE',  ( 1.000000000000000000, 0.000000000000000000, -0.000000000000000000 ) ) ;
#28897 = DIRECTION ( 'NONE',  ( 0.000000000000000000, 0.6051742151937661296, -0.7960930657056429771 ) ) ;
#28898 = EDGE_CURVE ( 'NONE', #28136, #63071, #11910, .T. ) ;
#28899 = CARTESIAN_POINT ( 'NONE',  ( 2.491965175174687186, 5.121563073453788029, 5.773748672882028643 ) ) ;
#28900 = ORIENTED_EDGE ( 'NONE', *, *, #43117, .T. ) ;
#28901 = DIRECTION ( 'NONE',  ( 1.000000000000000000, 0.000000000000000000, 0.000000000000000000 ) ) ;
#28902 = CARTESIAN_POINT ( 'NONE',  ( 37.00000000000000711, 0.7536123767498499326, -11.72195762423410414 ) ) ;
#28903 = AXIS2_PLACEMENT_3D ( 'NONE', #8892, #49478, #38494 ) ;
#28904 = CARTESIAN_POINT ( 'NONE',  ( 10.67301420047229676, 1.169570914859076716, 11.94385026977490405 ) ) ;
#28905 = CARTESIAN_POINT ( 'NONE',  ( -22.28856623400852399, 2.668530796663842963, 2.585606290939587382 ) ) ;
#28906 = AXIS2_PLACEMENT_3D ( 'NONE', #33235, #18628, #38209 ) ;
#28907 = AXIS2_PLACEMENT_3D ( 'NONE', #15839, #50476, #5237 ) ;
#28908 = AXIS2_PLACEMENT_3D ( 'NONE', #43506, #58171, #64444 ) ;
#28909 = EDGE_CURVE ( 'NONE', #50699, #20343, #21464, .T. ) ;
#28910 = CARTESIAN_POINT ( 'NONE',  ( -37.00000000000000711, -9.512294188640947112, 6.891188680298791169 ) ) ;
#28911 = VERTEX_POINT ( 'NONE', #47826 ) ;
#28912 = ADVANCED_FACE ( 'NONE', ( #62137 ), #57485, .T. ) ;
#28913 = ORIENTED_EDGE ( 'NONE', *, *, #54277, .T. ) ;
#28914 = DIRECTION ( 'NONE',  ( -1.000000000000000000, 0.000000000000000000, 0.000000000000000000 ) ) ;
#28915 = CARTESIAN_POINT ( 'NONE',  ( 2.259025283528085293, -3.937899517809441807, -6.547290863799084981 ) ) ;
#28916 = CARTESIAN_POINT ( 'NONE',  ( 1.719304012341629884, 8.755325027796281745, -9.242227816402079910 ) ) ;
#28917 = PRESENTATION_LAYER_ASSIGNMENT (  '', '', ( #19389 ) ) ;
#28918 = CARTESIAN_POINT ( 'NONE',  ( 35.00000000000000000, -2.021542716731485001, -12.01765980939841327 ) ) ;
#28919 = CIRCLE ( 'NONE', #24699, 2.899999999999995026 ) ;
#28920 = ORIENTED_EDGE ( 'NONE', *, *, #41275, .T. ) ;
#28921 = EDGE_LOOP ( 'NONE', ( #49471, #36101, #58127, #39649 ) ) ;
#28923 = ADVANCED_FACE ( 'NONE', ( #33179 ), #48182, .T. ) ;
#28922 = DIRECTION ( 'NONE',  ( 0.000000000000000000, -0.01356324068817991828, 0.9999080150203990547 ) ) ;
#28924 = CARTESIAN_POINT ( 'NONE',  ( 2.247112776671282841, 4.997244136394094483, 5.774169979602185698 ) ) ;
#28925 = CARTESIAN_POINT ( 'NONE',  ( 2.899286259009683508, -3.614094927251888301, -6.972741252562093983 ) ) ;
#28926 = CARTESIAN_POINT ( 'NONE',  ( 2.000000000000001776, -4.976357229393876480, 4.652926418895529714 ) ) ;
#28927 = CARTESIAN_POINT ( 'NONE',  ( 0.3632410797595257423, 9.235006602299463907, -8.092233745354546315 ) ) ;
#28928 = AXIS2_PLACEMENT_3D ( 'NONE', #64423, #7948, #28216 ) ;
#28929 = CARTESIAN_POINT ( 'NONE',  ( 5.520433897694421610, -0.007971295965052502958, 0.01278034823631960838 ) ) ;
#28930 = ORIENTED_EDGE ( 'NONE', *, *, #6392, .T. ) ;
#28931 = ORIENTED_EDGE ( 'NONE', *, *, #9556, .F. ) ;
#28932 = EDGE_LOOP ( 'NONE', ( #37353, #2453, #7264, #49177 ) ) ;
#28933 = LINE ( 'NONE', #50855, #27732 ) ;
#28934 = CARTESIAN_POINT ( 'NONE',  ( 35.00000000000000000, 11.65150730582934635, 1.488153103997001514 ) ) ;
#28935 = ORIENTED_EDGE ( 'NONE', *, *, #34976, .T. ) ;
#28936 = CYLINDRICAL_SURFACE ( 'NONE', #60220, 4.999999999999999112 ) ;
#28937 = AXIS2_PLACEMENT_3D ( 'NONE', #26500, #270, #25191 ) ;
#28938 = CARTESIAN_POINT ( 'NONE',  ( -35.04709527796842394, -0.01016988845958625987, -0.007030359780627049027 ) ) ;
#28939 = VERTEX_POINT ( 'NONE', #22564 ) ;
#28940 = CARTESIAN_POINT ( 'NONE',  ( 2.241449424704146320, 6.580749518451852076, -3.870245369721753814 ) ) ;
#28941 =( BOUNDED_SURFACE ( )  B_SPLINE_SURFACE ( 3, 1, ( 
 ( #30796, #20182 ),
 ( #51116, #46132 ),
 ( #20841, #16183 ),
 ( #36791, #26478 ) ),
 .UNSPECIFIED., .F., .F., .T. ) 
 B_SPLINE_SURFACE_WITH_KNOTS ( ( 4, 4 ),
 ( 2, 2 ),
 ( 0.000000000000000000, 1.000000000000000000 ),
 ( 0.000000000000000000, 1.000000000000000000 ),
 .UNSPECIFIED. ) 
 GEOMETRIC_REPRESENTATION_ITEM ( )  RATIONAL_B_SPLINE_SURFACE ( (
 ( 1.000000000000000000, 1.000000000000000000),
 ( 0.9942764183789327692, 0.8450855930916580938),
 ( 0.9942764183789327692, 0.8450855930916580938),
 ( 1.000000000000000000, 1.000000000000000000) ) ) 
 REPRESENTATION_ITEM ( '' )  SURFACE ( )  );
#28942 = DIRECTION ( 'NONE',  ( 0.000000000000000000, 0.000000000000000000, 1.000000000000000000 ) ) ;
#28943 = DIRECTION ( 'NONE',  ( 1.000000000000000000, 0.000000000000000000, -0.000000000000000000 ) ) ;
#28944 = EDGE_LOOP ( 'NONE', ( #11331, #57114, #62310, #47839 ) ) ;
#28945 = ORIENTED_EDGE ( 'NONE', *, *, #37212, .T. ) ;
#28946 = CARTESIAN_POINT ( 'NONE',  ( 37.25000000000000711, -20.00000000000000000, 2.449293598294706907E-15 ) ) ;
#28947 = VERTEX_POINT ( 'NONE', #27212 ) ;
#28948 = SURFACE_STYLE_FILL_AREA ( #54225 ) ;
#28949 = ORIENTED_EDGE ( 'NONE', *, *, #12755, .T. ) ;
#28950 = AXIS2_PLACEMENT_3D ( 'NONE', #54550, #24597, #58901 ) ;
#28951 = ORIENTED_EDGE ( 'NONE', *, *, #57021, .F. ) ;
#28952 = EDGE_LOOP ( 'NONE', ( #50197, #5564, #19652, #28381 ) ) ;
#28953 = DIRECTION ( 'NONE',  ( 0.000000000000000000, 0.01356324068817998940, -0.9999080150203990547 ) ) ;
#28954 = CARTESIAN_POINT ( 'NONE',  ( -12.96770491602036834, -33.25366259606196451, -10.81293556750676466 ) ) ;
#28955 = AXIS2_PLACEMENT_3D ( 'NONE', #17122, #21462, #16481 ) ;
#28956 = EDGE_CURVE ( 'NONE', #13767, #3623, #2403, .T. ) ;
#28958 = AXIS2_PLACEMENT_3D ( 'NONE', #44671, #39367, #23778 ) ;
#28957 = CARTESIAN_POINT ( 'NONE',  ( -22.28073302975501235, 3.572053042948136969, 0.9342220484184516893 ) ) ;
#28959 = CARTESIAN_POINT ( 'NONE',  ( -35.00000000000000000, 11.90598845858533572, 4.561791185930457182 ) ) ;
#28960 = CARTESIAN_POINT ( 'NONE',  ( -22.65996813707689128, 0.2230532344361583763, -4.828298130757411322 ) ) ;
#28961 = ORIENTED_EDGE ( 'NONE', *, *, #28571, .T. ) ;
#28962 = DIRECTION ( 'NONE',  ( -1.000000000000000000, 0.000000000000000000, 0.000000000000000000 ) ) ;
#28963 = VERTEX_POINT ( 'NONE', #47505 ) ;
#28964 = FACE_OUTER_BOUND ( 'NONE', #37886, .T. ) ;
#28965 = DIRECTION ( 'NONE',  ( 0.000000000000000000, -0.01356324068817999114, 0.9999080150203989437 ) ) ;
#28966 = ORIENTED_EDGE ( 'NONE', *, *, #34677, .T. ) ;
#28967 = EDGE_CURVE ( 'NONE', #39587, #34853, #3174, .T. ) ;
#28968 = CARTESIAN_POINT ( 'NONE',  ( 0.2638984909335716500, -5.950360275954980516, -10.70468911391670375 ) ) ;
#28969 = AXIS2_PLACEMENT_3D ( 'NONE', #49295, #41726, #21797 ) ;
#28970 = CARTESIAN_POINT ( 'NONE',  ( 0.3675815128205912052, 3.951233083390468526, 11.62724744438066971 ) ) ;
#28971 = CARTESIAN_POINT ( 'NONE',  ( 3.092491956585171398, -7.707758057368747195, 1.813286239165102121 ) ) ;
#28972 = ORIENTED_EDGE ( 'NONE', *, *, #34289, .T. ) ;
#28973 = VECTOR ( 'NONE', #25643, 1000.000000000000000 ) ;
#28974 = EDGE_CURVE ( 'NONE', #1959, #64903, #61857, .T. ) ;
#28975 = ORIENTED_EDGE ( 'NONE', *, *, #16909, .T. ) ;
#28976 = CARTESIAN_POINT ( 'NONE',  ( -22.30625920655495165, 1.672644928563083333, -3.403091720605004866 ) ) ;
#28977 = ORIENTED_EDGE ( 'NONE', *, *, #376, .T. ) ;
#28978 = EDGE_CURVE ( 'NONE', #167, #57337, #57606, .T. ) ;
#28979 = DIRECTION ( 'NONE',  ( 0.000000000000000000, 0.000000000000000000, -1.000000000000000000 ) ) ;
#28980 = CARTESIAN_POINT ( 'NONE',  ( -19.30612897158720997, -13.39145038892620398, -1.740264294593142358 ) ) ;
#28981 = CIRCLE ( 'NONE', #33242, 5.000000000000000888 ) ;
#28982 = CARTESIAN_POINT ( 'NONE',  ( 36.00000000000000711, 12.31350058095523003, -3.307597835713290912 ) ) ;
#28983 = DIRECTION ( 'NONE',  ( -1.000000000000000000, 0.000000000000000000, 0.000000000000000000 ) ) ;
#28984 = EDGE_CURVE ( 'NONE', #4941, #33111, #40484, .T. ) ;
#28985 = CARTESIAN_POINT ( 'NONE',  ( 1.719304012339833099, -9.242227816401946683, 8.755325027794301107 ) ) ;
#28986 = ORIENTED_EDGE ( 'NONE', *, *, #34718, .T. ) ;
#28987 = DIRECTION ( 'NONE',  ( -1.000000000000000000, 0.000000000000000000, 0.000000000000000000 ) ) ;
#28988 = CARTESIAN_POINT ( 'NONE',  ( 35.00000000000000000, 4.705694406421931860E-17, -3.469127814946512892E-15 ) ) ;
#28989 = CARTESIAN_POINT ( 'NONE',  ( 0.3675815128205912052, -12.13672785388549080, -1.872154644482208585 ) ) ;
#28990 = EDGE_CURVE ( 'NONE', #21572, #646, #18249, .T. ) ;
#28991 = CARTESIAN_POINT ( 'NONE',  ( 1.937114397841932290, 12.80345148322679272, 0.9020203649532124723 ) ) ;
#28992 = CARTESIAN_POINT ( 'NONE',  ( -35.04683013664716640, -0.01235741808121416756, 0.0001018103929289144923 ) ) ;
#28993 = EDGE_CURVE ( 'NONE', #20288, #31780, #34113, .T. ) ;
#28994 = DIRECTION ( 'NONE',  ( -1.000000000000000000, 0.000000000000000000, 0.000000000000000000 ) ) ;
#28995 = CARTESIAN_POINT ( 'NONE',  ( 37.00000000000000711, 4.705694406421931860E-17, -3.469127814946512892E-15 ) ) ;
#28996 = DIRECTION ( 'NONE',  ( 0.000000000000000000, 0.9635499925192219095, 0.2675283385292247518 ) ) ;
#28997 = AXIS2_PLACEMENT_3D ( 'NONE', #20969, #11012, #40942 ) ;
#28998 = AXIS2_PLACEMENT_3D ( 'NONE', #3274, #58822, #33185 ) ;
#28999 = EDGE_CURVE ( 'NONE', #13921, #1587, #3923, .T. ) ;
#29000 = VECTOR ( 'NONE', #24993, 1000.000000000000000 ) ;
#29001 = AXIS2_PLACEMENT_3D ( 'NONE', #17968, #49233, #64483 ) ;
#29002 = ORIENTED_EDGE ( 'NONE', *, *, #15182, .T. ) ;
#29003 = EDGE_CURVE ( 'NONE', #6117, #53424, #24695, .T. ) ;
#29004 = CARTESIAN_POINT ( 'NONE',  ( -27.09483304420799143, -1.303111346475732679, -1.923212037696920840 ) ) ;
#29005 = EDGE_CURVE ( 'NONE', #28290, #61436, #64407, .T. ) ;
#29006 = EDGE_LOOP ( 'NONE', ( #3920, #58728, #17638, #38661 ) ) ;
#29007 = FACE_OUTER_BOUND ( 'NONE', #14924, .T. ) ;
#29008 = CARTESIAN_POINT ( 'NONE',  ( -22.27720412283625961, -3.606406551442359998, 0.7407051501189869658 ) ) ;
#29009 = CARTESIAN_POINT ( 'NONE',  ( 2.305787727787085295, -7.249469779319927198, 2.461236246751046242 ) ) ;
#29010 = ADVANCED_FACE ( 'NONE', ( #28514 ), #41741, .F. ) ;
#29011 = CYLINDRICAL_SURFACE ( 'NONE', #28634, 4.999999999999999112 ) ;
#29012 = VERTEX_POINT ( 'NONE', #49788 ) ;
#29013 = AXIS2_PLACEMENT_3D ( 'NONE', #42880, #38554, #52563 ) ;
#29014 = VERTEX_POINT ( 'NONE', #48821 ) ;
#29015 = ORIENTED_EDGE ( 'NONE', *, *, #60204, .T. ) ;
#29016 = CARTESIAN_POINT ( 'NONE',  ( 29.13270927395454990, -11.82606251486632587, 6.514588969236678295 ) ) ;
#29017 = AXIS2_PLACEMENT_3D ( 'NONE', #22463, #13454, #7483 ) ;
#29018 = ORIENTED_EDGE ( 'NONE', *, *, #51948, .T. ) ;
#29019 = CARTESIAN_POINT ( 'NONE',  ( 0.000000000000000000, -4.444115772890066651, -5.163689623839394116 ) ) ;
#29020 = DIRECTION ( 'NONE',  ( -1.000000000000000000, 0.000000000000000000, -0.000000000000000000 ) ) ;
#29021 = CARTESIAN_POINT ( 'NONE',  ( 0.3109076770649022436, -9.239379580302159667, 8.060731492642771556 ) ) ;
#29022 = CARTESIAN_POINT ( 'NONE',  ( 18.43752717680369457, 6.464745515762281514, 10.12011330815638921 ) ) ;
#29023 = ORIENTED_EDGE ( 'NONE', *, *, #26975, .T. ) ;
#29024 = CARTESIAN_POINT ( 'NONE',  ( 35.00000000000000000, 4.705694406421931860E-17, -3.469127814946512892E-15 ) ) ;
#29025 = VECTOR ( 'NONE', #52841, 1000.000000000000000 ) ;
#29026 = CARTESIAN_POINT ( 'NONE',  ( 2.000000000000001776, 3.937687286050910895, -6.383151168292449107 ) ) ;
#29027 = CARTESIAN_POINT ( 'NONE',  ( 2.241352910868908754, 6.569501556381497132, -3.889181972941381460 ) ) ;
#29029 = ORIENTED_EDGE ( 'NONE', *, *, #11650, .T. ) ;
#29028 = DIRECTION ( 'NONE',  ( -1.000000000000000000, -0.000000000000000000, -0.000000000000000000 ) ) ;
#29030 = FACE_OUTER_BOUND ( 'NONE', #35033, .T. ) ;
#29031 = ORIENTED_EDGE ( 'NONE', *, *, #44432, .T. ) ;
#29032 = DIRECTION ( 'NONE',  ( 0.000000000000000000, -0.01356324068817992175, 0.9999080150203990547 ) ) ;
#29033 = EDGE_LOOP ( 'NONE', ( #58763, #36809, #37491, #55981 ) ) ;
#29034 = CARTESIAN_POINT ( 'NONE',  ( 35.00000000000000000, -0.1414404973753014549, -12.74921544981111055 ) ) ;
#29035 = MANIFOLD_SOLID_BREP ( 'Keyway', #1534 ) ;
#29036 = CARTESIAN_POINT ( 'NONE',  ( 0.3632410797595244101, 3.951633449031067169, -11.62558329798846479 ) ) ;
#29037 = CARTESIAN_POINT ( 'NONE',  ( -35.00000000000000000, 0.000000000000000000, 0.000000000000000000 ) ) ;
#29038 = CARTESIAN_POINT ( 'NONE',  ( 0.3164563675027666778, -3.967501530099160956, 11.60369811966061704 ) ) ;
#29039 = EDGE_CURVE ( 'NONE', #9298, #7202, #24181, .T. ) ;
#29040 = AXIS2_PLACEMENT_3D ( 'NONE', #42916, #6704, #38241 ) ;
#29041 = CARTESIAN_POINT ( 'NONE',  ( 0.3341166715381361230, 9.559079491641874426, 7.691251065848372370 ) ) ;
#29042 = CARTESIAN_POINT ( 'NONE',  ( -35.00000000000000000, 7.817610399097512541, 8.766823244862019138 ) ) ;
#29044 = ORIENTED_EDGE ( 'NONE', *, *, #18360, .F. ) ;
#29043 = CARTESIAN_POINT ( 'NONE',  ( -36.00000000000000711, -12.63095688309030429, 1.738225594539952956 ) ) ;
#29045 = ORIENTED_EDGE ( 'NONE', *, *, #31657, .F. ) ;
#29046 = CARTESIAN_POINT ( 'NONE',  ( 1.937114397841932290, -12.76557247858999311, 1.334979369128383331 ) ) ;
#29047 = ORIENTED_EDGE ( 'NONE', *, *, #44495, .T. ) ;
#29048 = CIRCLE ( 'NONE', #3579, 5.000000000000000888 ) ;
#29049 = ORIENTED_EDGE ( 'NONE', *, *, #37238, .F. ) ;
#29050 = EDGE_CURVE ( 'NONE', #10275, #57905, #13234, .T. ) ;
#29052 = AXIS2_PLACEMENT_3D ( 'NONE', #4167, #60028, #65328 ) ;
#29051 = CARTESIAN_POINT ( 'NONE',  ( 0.2646305136544072623, 6.008537389229567260, -10.67138229758223389 ) ) ;
#29053 = CARTESIAN_POINT ( 'NONE',  ( -27.08421860617808008, 0.2990745872176441833, 2.271664812096779951 ) ) ;
#29054 = DIRECTION ( 'NONE',  ( -1.000000000000000000, 0.000000000000000000, 0.000000000000000000 ) ) ;
#29055 = CARTESIAN_POINT ( 'NONE',  ( -22.27706089016750113, 0.9256273512588665264, 3.562910635974977147 ) ) ;
#29056 = CARTESIAN_POINT ( 'NONE',  ( 0.2646305136544072623, -7.770320294339112976, -9.465888453933038349 ) ) ;
#29057 = AXIS2_PLACEMENT_3D ( 'NONE', #32808, #53117, #64073 ) ;
#29058 = B_SPLINE_CURVE_WITH_KNOTS ( 'NONE', 3,
 ( #58434, #64061, #59401, #2248, #48466, #49126, #44109, #27498, #32799, #48785 ),
 .UNSPECIFIED., .F., .F.,
 ( 4, 3, 3, 4 ),
 ( 5.401523115762557641E-05, 0.0008136511341527791425, 0.004068255670953093220, 0.005063778443040927411 ),
 .UNSPECIFIED. ) ;
#29059 = CARTESIAN_POINT ( 'NONE',  ( 0.2759803524722194701, 10.70204612651785325, -5.960075719898730640 ) ) ;
#29060 = VECTOR ( 'NONE', #39801, 1000.000000000000000 ) ;
#29061 = CARTESIAN_POINT ( 'NONE',  ( 37.00000000000000711, 6.950793414699941053, 10.68873102412834797 ) ) ;
#29062 = ORIENTED_EDGE ( 'NONE', *, *, #13044, .T. ) ;
#29063 = DIRECTION ( 'NONE',  ( 0.000000000000000000, 0.04924826701373895277, 0.9987865678893280696 ) ) ;
#29064 = CIRCLE ( 'NONE', #393, 2.899999999999995026 ) ;
#29065 = CARTESIAN_POINT ( 'NONE',  ( 2.305787727787083519, -5.756228004061423320, -5.047606869483115766 ) ) ;
#29066 = CARTESIAN_POINT ( 'NONE',  ( -17.16708216679437271, -6.932898597583876388, 11.58855638538233990 ) ) ;
#29067 = EDGE_CURVE ( 'NONE', #21416, #51437, #23611, .T. ) ;
#29068 = ORIENTED_EDGE ( 'NONE', *, *, #20056, .T. ) ;
#29069 = AXIS2_PLACEMENT_3D ( 'NONE', #50375, #40036, #14750 ) ;
#29070 = VECTOR ( 'NONE', #7089, 1000.000000000000000 ) ;
#29071 = LINE ( 'NONE', #24733, #30939 ) ;
#29072 = B_SPLINE_CURVE_WITH_KNOTS ( 'NONE', 3,
 ( #56141, #24584, #36177, #14579, #60476, #45856, #9593 ),
 .UNSPECIFIED., .F., .F.,
 ( 4, 3, 4 ),
 ( 3.688038945365320759E-15, 0.002398160485434608184, 0.005002426799381520968 ),
 .UNSPECIFIED. ) ;
#29073 = VECTOR ( 'NONE', #29837, 1000.000000000000000 ) ;
#29074 = CARTESIAN_POINT ( 'NONE',  ( -10.48620311856347875, -9.720786832536937538, -9.367833439828894271 ) ) ;
#29075 = VERTEX_POINT ( 'NONE', #61714 ) ;
#29076 = CARTESIAN_POINT ( 'NONE',  ( -35.00000000000000000, -2.216820770815165265, 11.53507381115582575 ) ) ;
#29077 = CARTESIAN_POINT ( 'NONE',  ( -35.00000000000000000, -11.73808581813438323, 0.4353888892047964587 ) ) ;
#29078 = CARTESIAN_POINT ( 'NONE',  ( 0.2648978790185619880, -12.08224454301447182, -1.996248716311752824 ) ) ;
#29079 = EDGE_CURVE ( 'NONE', #60763, #59719, #65018, .T. ) ;
#29080 = AXIS2_PLACEMENT_3D ( 'NONE', #35858, #10278, #55521 ) ;
#29081 = EDGE_CURVE ( 'NONE', #18385, #17578, #36361, .T. ) ;
#29082 = DIRECTION ( 'NONE',  ( -1.000000000000000000, -1.836970198721029688E-16, -0.000000000000000000 ) ) ;
#29083 = DIRECTION ( 'NONE',  ( 1.000000000000000000, 0.000000000000000000, 0.000000000000000000 ) ) ;
#29084 = ORIENTED_EDGE ( 'NONE', *, *, #59756, .F. ) ;
#29085 = DIRECTION ( 'NONE',  ( -1.000000000000000000, -0.000000000000000000, -0.000000000000000000 ) ) ;
#29086 = CARTESIAN_POINT ( 'NONE',  ( 0.2956976708475477222, -12.10637007622313632, 1.911282699793684925 ) ) ;
#29087 = CARTESIAN_POINT ( 'NONE',  ( 6.812204945636112896, -4.138731716409435712, 11.26369831714195335 ) ) ;
#29088 = ORIENTED_EDGE ( 'NONE', *, *, #6516, .F. ) ;
#29089 = EDGE_CURVE ( 'NONE', #42172, #5900, #7708, .T. ) ;
#29090 = DIRECTION ( 'NONE',  ( -1.000000000000000000, 0.000000000000000000, 0.000000000000000000 ) ) ;
#29091 = DIRECTION ( 'NONE',  ( 1.000000000000000000, 0.000000000000000000, -0.000000000000000000 ) ) ;
#29092 = ORIENTED_EDGE ( 'NONE', *, *, #62425, .F. ) ;
#29093 = VECTOR ( 'NONE', #36245, 1000.000000000000000 ) ;
#29094 = CIRCLE ( 'NONE', #48248, 2.899999999999994582 ) ;
#29095 = VERTEX_POINT ( 'NONE', #10853 ) ;
#29096 = FACE_OUTER_BOUND ( 'NONE', #23157, .T. ) ;
#29097 = AXIS2_PLACEMENT_3D ( 'NONE', #6037, #56215, #61525 ) ;
#29098 = ORIENTED_EDGE ( 'NONE', *, *, #57655, .T. ) ;
#29099 = DIRECTION ( 'NONE',  ( 0.000000000000000000, 0.01356324068817998940, -0.9999080150203989437 ) ) ;
#29100 = DIRECTION ( 'NONE',  ( 0.000000000000000000, 0.01356324068817996685, -0.9999080150203990547 ) ) ;
#29101 = DIRECTION ( 'NONE',  ( 0.000000000000000000, 0.000000000000000000, -1.000000000000000000 ) ) ;
#29102 = CARTESIAN_POINT ( 'NONE',  ( 2.305787727787084851, -7.566723232958062262, -1.164987321564809886 ) ) ;
#29103 = VECTOR ( 'NONE', #2164, 1000.000000000000000 ) ;
#29104 = AXIS2_PLACEMENT_3D ( 'NONE', #54425, #49117, #43775 ) ;
#29105 = CARTESIAN_POINT ( 'NONE',  ( -35.04683013664716640, 0.01162359816267300762, -0.004196202180977571042 ) ) ;
#29107 = VERTEX_POINT ( 'NONE', #41423 ) ;
#29106 = CARTESIAN_POINT ( 'NONE',  ( 0.8375941296788365076, 7.696026447556312711, 9.769835228043566744 ) ) ;
#29108 = FACE_OUTER_BOUND ( 'NONE', #65615, .T. ) ;
#29109 = ORIENTED_EDGE ( 'NONE', *, *, #54054, .F. ) ;
#29110 = CARTESIAN_POINT ( 'NONE',  ( 0.2651627682582915480, 10.56115808354091712, -6.199212018117330913 ) ) ;
#29111 = AXIS2_PLACEMENT_3D ( 'NONE', #48052, #27107, #22106 ) ;
#29112 = ORIENTED_EDGE ( 'NONE', *, *, #38872, .T. ) ;
#29113 = VERTEX_POINT ( 'NONE', #61382 ) ;
#29114 = CARTESIAN_POINT ( 'NONE',  ( -18.58686583997218378, 5.151216734910788908, 12.47858029384653555 ) ) ;
#29115 = CARTESIAN_POINT ( 'NONE',  ( -1.806230668642147652, -30.59323697348071747, 15.24264478004184120 ) ) ;
#29116 = DIRECTION ( 'NONE',  ( -1.000000000000000000, -0.000000000000000000, 0.000000000000000000 ) ) ;
#29117 = EDGE_CURVE ( 'NONE', #35757, #25311, #29814, .T. ) ;
#29118 = CARTESIAN_POINT ( 'NONE',  ( 24.38667543136798344, -1.087042411491959459, 11.95203068355522369 ) ) ;
#29119 = DIRECTION ( 'NONE',  ( 0.000000000000000000, 0.01356324068817998940, -0.9999080150203990547 ) ) ;
#29120 = FACE_OUTER_BOUND ( 'NONE', #8977, .T. ) ;
#29121 = ORIENTED_EDGE ( 'NONE', *, *, #34122, .F. ) ;
#29122 = ADVANCED_FACE ( 'NONE', ( #10195 ), #55763, .T. ) ;
#29123 = VERTEX_POINT ( 'NONE', #9522 ) ;
#29124 = CYLINDRICAL_SURFACE ( 'NONE', #45425, 2.899999999999994582 ) ;
#29125 = CIRCLE ( 'NONE', #459, 5.000000000000000888 ) ;
#29126 = B_SPLINE_CURVE_WITH_KNOTS ( 'NONE', 3,
 ( #8105, #9379, #33369, #38345, #54657, #28377, #18425, #24360, #19396, #8424, #44005, #28697, #54322, #44624, #53669, #59296, #58993, #3128, #49971, #23391, #38690, #33689 ),
 .UNSPECIFIED., .F., .F.,
 ( 4, 2, 2, 2, 2, 2, 2, 2, 2, 2, 4 ),
 ( 0.000000000000000000, 0.001221936687227891637, 0.001832905030841836154, 0.002443873374455780671, 0.003665810061683667537, 0.004276778405297610754, 0.004887746748911554404, 0.006109683436139443438, 0.007331620123367331605, 0.008553556810595219773, 0.009775493497823107072 ),
 .UNSPECIFIED. ) ;
#29127 = ORIENTED_EDGE ( 'NONE', *, *, #14390, .T. ) ;
#29128 = EDGE_CURVE ( 'NONE', #37857, #19254, #28594, .T. ) ;
#29129 = LINE ( 'NONE', #34086, #56097 ) ;
#29130 = CARTESIAN_POINT ( 'NONE',  ( 0.3278977287071226376, 0.2481246099269766026, -12.26453627383316025 ) ) ;
#29131 = FACE_OUTER_BOUND ( 'NONE', #47525, .T. ) ;
#29132 = DIRECTION ( 'NONE',  ( 1.000000000000000000, 0.000000000000000000, 0.000000000000000000 ) ) ;
#29133 = CARTESIAN_POINT ( 'NONE',  ( 2.655192694324043590, 6.604353705983746714, 6.969384012964340513 ) ) ;
#29134 = VECTOR ( 'NONE', #24970, 1000.000000000000000 ) ;
#29135 = CARTESIAN_POINT ( 'NONE',  ( 2.261269890822072526, 3.940687015735738097, -6.546486799463070660 ) ) ;
#29136 = ORIENTED_EDGE ( 'NONE', *, *, #61613, .F. ) ;
#29137 =( BOUNDED_SURFACE ( )  B_SPLINE_SURFACE ( 3, 1, ( 
 ( #3014, #33587 ),
 ( #18306, #39212 ),
 ( #9271, #4310 ),
 ( #64480, #54197 ) ),
 .UNSPECIFIED., .F., .F., .F. ) 
 B_SPLINE_SURFACE_WITH_KNOTS ( ( 4, 4 ),
 ( 2, 2 ),
 ( 0.000000000000000000, 1.000000000000000000 ),
 ( 0.000000000000000000, 1.000000000000000000 ),
 .UNSPECIFIED. ) 
 GEOMETRIC_REPRESENTATION_ITEM ( )  RATIONAL_B_SPLINE_SURFACE ( (
 ( 1.000000000000000000, 1.000000000000000000),
 ( 0.9942764183789327692, 0.8450855930916580938),
 ( 0.9942764183789327692, 0.8450855930916580938),
 ( 1.000000000000000000, 1.000000000000000000) ) ) 
 REPRESENTATION_ITEM ( '' )  SURFACE ( )  );
#29138 = ORIENTED_EDGE ( 'NONE', *, *, #20938, .F. ) ;
#29139 = ADVANCED_FACE ( 'NONE', ( #9867 ), #30157, .T. ) ;
#29140 = CARTESIAN_POINT ( 'NONE',  ( 1.549075743844144037, 3.694639393664535199, 12.12370443967527400 ) ) ;
#29141 = ADVANCED_FACE ( 'NONE', ( #4904 ), #25165, .T. ) ;
#29142 = CIRCLE ( 'NONE', #40811, 7.499999999999988454 ) ;
#29143 = DIRECTION ( 'NONE',  ( 0.000000000000000000, 0.01356324068817992175, -0.9999080150203990547 ) ) ;
#29144 = CIRCLE ( 'NONE', #481, 12.75000000000000178 ) ;
#29145 = DIRECTION ( 'NONE',  ( -1.000000000000000000, 0.000000000000000000, 0.000000000000000000 ) ) ;
#29146 = EDGE_CURVE ( 'NONE', #64071, #63385, #37398, .T. ) ;
#29147 = DIRECTION ( 'NONE',  ( -1.000000000000000000, 0.000000000000000000, 0.000000000000000000 ) ) ;
#29148 = DIRECTION ( 'NONE',  ( 0.000000000000000000, 0.000000000000000000, 1.000000000000000000 ) ) ;
#29149 = CARTESIAN_POINT ( 'NONE',  ( -10.25715257150912940, -4.753195267362797516, -11.02444816437827591 ) ) ;
#29150 = LINE ( 'NONE', #14795, #55575 ) ;
#29151 = CARTESIAN_POINT ( 'NONE',  ( 2.263328370261528555, 1.466596409249160127, 7.499672967744983154 ) ) ;
#29152 = CARTESIAN_POINT ( 'NONE',  ( 2.653899356900406570, -5.192946150929565796, -5.782420802795875225 ) ) ;
#29153 = ORIENTED_EDGE ( 'NONE', *, *, #4064, .T. ) ;
#29154 = AXIS2_PLACEMENT_3D ( 'NONE', #62319, #57348, #11452 ) ;
#29155 = CARTESIAN_POINT ( 'NONE',  ( 3.031336079628672575, -6.309383307296084986, -4.750429016921874137 ) ) ;
#29156 = CARTESIAN_POINT ( 'NONE',  ( 22.68177428654798433, -4.560196341733014691, -11.10067150598529473 ) ) ;
#29157 = CARTESIAN_POINT ( 'NONE',  ( 35.00000000000000000, 4.705694406421931860E-17, -3.469127814946512892E-15 ) ) ;
#29158 = EDGE_CURVE ( 'NONE', #48986, #11917, #5563, .T. ) ;
#29160 = VECTOR ( 'NONE', #18271, 1000.000000000000000 ) ;
#29159 = AXIS2_PLACEMENT_3D ( 'NONE', #6862, #11820, #27778 ) ;
#29161 = EDGE_CURVE ( 'NONE', #19944, #28113, #25737, .T. ) ;
#29162 = CARTESIAN_POINT ( 'NONE',  ( 2.556980015513593774, -3.668282146013208678, 6.815084337351732913 ) ) ;
#29163 = CARTESIAN_POINT ( 'NONE',  ( 1.014383007554953142, -4.688516792764541918, -11.58298623339619660 ) ) ;
#29164 = ORIENTED_EDGE ( 'NONE', *, *, #13250, .F. ) ;
#29165 = DIRECTION ( 'NONE',  ( 1.000000000000000000, -0.000000000000000000, -0.000000000000000000 ) ) ;
#29166 = FACE_OUTER_BOUND ( 'NONE', #5086, .T. ) ;
#29167 = CARTESIAN_POINT ( 'NONE',  ( 7.310206959902322055, -26.30114832292194649, -14.76431686918209785 ) ) ;
#29168 = VERTEX_POINT ( 'NONE', #46758 ) ;
#29169 = CARTESIAN_POINT ( 'NONE',  ( -7.353169898081519662, -1.421260117484592689, -13.42529598466177276 ) ) ;
#29170 = LINE ( 'NONE', #55746, #25738 ) ;
#29171 = CARTESIAN_POINT ( 'NONE',  ( 37.00000000000000711, 12.05416472667167760, 1.791059740004291578 ) ) ;
#29172 = DIRECTION ( 'NONE',  ( 0.000000000000000000, 0.6943713148249639477, -0.7196168960969793194 ) ) ;
#29173 = CARTESIAN_POINT ( 'NONE',  ( 2.177405672430728245, 10.27382588316567436, -4.457418613957222497 ) ) ;
#29174 = CIRCLE ( 'NONE', #37660, 5.000000000000000000 ) ;
#29175 = DIRECTION ( 'NONE',  ( -1.000000000000000000, -0.000000000000000000, 0.000000000000000000 ) ) ;
#29176 = ORIENTED_EDGE ( 'NONE', *, *, #49188, .F. ) ;
#29177 = CARTESIAN_POINT ( 'NONE',  ( 2.276198483117256810, -7.236140649716383599, 2.469789406312209668 ) ) ;
#29178 = CARTESIAN_POINT ( 'NONE',  ( 5.515539859299206427, -0.0008592514567753351158, 0.005991790098944297510 ) ) ;
#29179 = CARTESIAN_POINT ( 'NONE',  ( -18.55537666206150504, 5.673200735153683283, -12.25320171535231495 ) ) ;
#29180 = LINE ( 'NONE', #49476, #45738 ) ;
#29181 = LINE ( 'NONE', #59124, #40711 ) ;
#29182 = CARTESIAN_POINT ( 'NONE',  ( 47.00000000000000711, 4.705694406421931860E-17, -3.469127814946512892E-15 ) ) ;
#29183 = CARTESIAN_POINT ( 'NONE',  ( 2.241317068080784125, 7.533758201955892631, 1.235499051333795784 ) ) ;
#29184 = DIRECTION ( 'NONE',  ( 0.000000000000000000, -0.01356324068817999114, 0.9999080150203989437 ) ) ;
#29185 = ORIENTED_EDGE ( 'NONE', *, *, #52660, .T. ) ;
#29186 = AXIS2_PLACEMENT_3D ( 'NONE', #18056, #58972, #12715 ) ;
#29187 = ORIENTED_EDGE ( 'NONE', *, *, #37745, .F. ) ;
#29188 = ORIENTED_EDGE ( 'NONE', *, *, #5895, .T. ) ;
#29189 = LINE ( 'NONE', #28517, #57681 ) ;
#29190 = DIRECTION ( 'NONE',  ( 0.000000000000000000, 0.000000000000000000, -1.000000000000000000 ) ) ;
#29191 = ORIENTED_EDGE ( 'NONE', *, *, #64392, .T. ) ;
#29192 = DIRECTION ( 'NONE',  ( 0.000000000000000000, 0.3807014730195220631, -0.9246979985058721985 ) ) ;
#29193 = EDGE_CURVE ( 'NONE', #64221, #28784, #37766, .T. ) ;
#29194 = LINE ( 'NONE', #38506, #54988 ) ;
#29195 = CARTESIAN_POINT ( 'NONE',  ( 2.247112776671933876, -4.997244136395391223, -5.774169979601344593 ) ) ;
#29196 = ORIENTED_EDGE ( 'NONE', *, *, #40087, .F. ) ;
#29197 = ORIENTED_EDGE ( 'NONE', *, *, #64353, .T. ) ;
#29198 = CARTESIAN_POINT ( 'NONE',  ( 2.507146904658098752, 0.2163149345877656282, -7.719969556433173175 ) ) ;
#29199 = CIRCLE ( 'NONE', #37694, 5.000000000000000888 ) ;
#29200 = CARTESIAN_POINT ( 'NONE',  ( 35.00000000000000000, 4.705694406421931860E-17, -3.469127814946512892E-15 ) ) ;
#29201 = EDGE_LOOP ( 'NONE', ( #40082, #12457 ) ) ;
#29202 = DIRECTION ( 'NONE',  ( 0.000000000000000000, -0.01356324068817999114, 0.9999080150203989437 ) ) ;
#29203 = EDGE_LOOP ( 'NONE', ( #37860, #39714, #31411, #46993, #59890, #5114, #3439, #7886, #52885, #12628, #36360, #18960, #15038, #14281, #57674, #10750, #31406, #35966, #39633, #11930, #38806, #58465, #37634, #46234, #44796, #50214, #43369, #32806, #18314, #29541, #39238, #28348, #5104, #32205 ) ) ;
#29204 = CARTESIAN_POINT ( 'NONE',  ( 0.000000000000000000, 0.000000000000000000, 0.000000000000000000 ) ) ;
#29205 = VECTOR ( 'NONE', #47022, 1000.000000000000114 ) ;
#29206 = DIRECTION ( 'NONE',  ( 1.000000000000000000, 0.000000000000000000, 0.000000000000000000 ) ) ;
#29208 = EDGE_CURVE ( 'NONE', #63500, #43482, #63444, .T. ) ;
#29207 = CARTESIAN_POINT ( 'NONE',  ( 9.687175622948609899, -11.98570860552670325, -0.5854820436212360146 ) ) ;
#29209 = DIRECTION ( 'NONE',  ( -1.000000000000000000, 0.000000000000000000, 0.000000000000000000 ) ) ;
#29210 = CARTESIAN_POINT ( 'NONE',  ( -9.351388602708162523, -11.42638970207761950, -3.665735721005252135 ) ) ;
#29211 = ORIENTED_EDGE ( 'NONE', *, *, #34, .F. ) ;
#29212 = CARTESIAN_POINT ( 'NONE',  ( 2.269879328256728890, 7.642470739868882035, -0.1483462450597493598 ) ) ;
#29213 = CARTESIAN_POINT ( 'NONE',  ( 0.2652384529303125626, 7.820949643217270264, -9.423437232855587098 ) ) ;
#29214 = CARTESIAN_POINT ( 'NONE',  ( 0.2653519789438753551, -9.366970421692828452, 7.888580323518841197 ) ) ;
#29215 = EDGE_CURVE ( 'NONE', #7317, #22476, #47561, .T. ) ;
#29216 = DIRECTION ( 'NONE',  ( 0.000000000000000000, -0.01356324068817992175, 0.9999080150203990547 ) ) ;
#29217 = CARTESIAN_POINT ( 'NONE',  ( 2.241536586108911155, -7.517390684805879353, 1.331908602351616011 ) ) ;
#29218 = CARTESIAN_POINT ( 'NONE',  ( -22.49803948133826026, -3.704553751086667734, 2.269619744675254847 ) ) ;
#29219 = CARTESIAN_POINT ( 'NONE',  ( 2.000000000000001776, -3.795144977083580784, -6.468916029978842630 ) ) ;
#29220 = DIRECTION ( 'NONE',  ( -1.000000000000000000, 0.000000000000000000, -0.000000000000000000 ) ) ;
#29221 = CARTESIAN_POINT ( 'NONE',  ( 2.406456491626380423, -10.41426194695414686, 0.6290357040719805060 ) ) ;
#29222 = AXIS2_PLACEMENT_3D ( 'NONE', #30505, #45813, #51143 ) ;
#29223 = ORIENTED_EDGE ( 'NONE', *, *, #61329, .F. ) ;
#29224 = FACE_OUTER_BOUND ( 'NONE', #60049, .T. ) ;
#29225 = VERTEX_POINT ( 'NONE', #2545 ) ;
#29226 = CARTESIAN_POINT ( 'NONE',  ( 0.3675815128205894289, -4.447030445008257615, 11.44679196252407927 ) ) ;
#29227 = CYLINDRICAL_SURFACE ( 'NONE', #28753, 4.999999999999999112 ) ;
#29228 = CARTESIAN_POINT ( 'NONE',  ( 2.241506898688418570, -4.877157973187019380, 5.873558213059462574 ) ) ;
#29229 = DIRECTION ( 'NONE',  ( 0.000000000000000000, 0.000000000000000000, 1.000000000000000000 ) ) ;
#29230 = DIRECTION ( 'NONE',  ( 0.000000000000000000, 0.000000000000000000, 1.000000000000000000 ) ) ;
#29231 = VERTEX_POINT ( 'NONE', #47746 ) ;
#29232 =( GEOMETRIC_REPRESENTATION_CONTEXT ( 3 ) GLOBAL_UNCERTAINTY_ASSIGNED_CONTEXT ( ( #38928 ) ) GLOBAL_UNIT_ASSIGNED_CONTEXT ( ( #44450, #59132, #13543 ) ) REPRESENTATION_CONTEXT ( 'NONE', 'WORKASPACE' ) );
#29233 = CARTESIAN_POINT ( 'NONE',  ( 3.152665057734023613, 0.4801242025591827001, -7.923639299008664594 ) ) ;
#29234 = DIRECTION ( 'NONE',  ( 0.000000000000000000, 0.9346839223284527653, -0.3554799084909000539 ) ) ;
#29235 = CARTESIAN_POINT ( 'NONE',  ( 10.88148533521881944, 1.035935135079044001, 11.95575279693729520 ) ) ;
#29236 = CARTESIAN_POINT ( 'NONE',  ( 16.45009115226350005, -34.41505313721356885, -6.130398315945338794 ) ) ;
#29237 = EDGE_CURVE ( 'NONE', #40945, #25882, #31772, .T. ) ;
#29238 = CARTESIAN_POINT ( 'NONE',  ( 2.000000000000001776, 1.018311147294260977, -6.861346417234475581 ) ) ;
#29239 = AXIS2_PLACEMENT_3D ( 'NONE', #61204, #371, #1019 ) ;
#29240 = ORIENTED_EDGE ( 'NONE', *, *, #30978, .T. ) ;
#29241 = CARTESIAN_POINT ( 'NONE',  ( 0.000000000000000000, -6.662861565602053560, -1.421313227905724341 ) ) ;
#29242 = ORIENTED_EDGE ( 'NONE', *, *, #56311, .F. ) ;
#29243 = LINE ( 'NONE', #40176, #62844 ) ;
#29244 = CYLINDRICAL_SURFACE ( 'NONE', #56495, 7.499999999999988454 ) ;
#29245 = DIRECTION ( 'NONE',  ( 0.000000000000000000, 0.000000000000000000, 1.000000000000000000 ) ) ;
#29246 = AXIS2_PLACEMENT_3D ( 'NONE', #54558, #3707, #64192 ) ;
#29247 = EDGE_CURVE ( 'NONE', #45502, #28763, #42700, .T. ) ;
#29248 = ORIENTED_EDGE ( 'NONE', *, *, #22756, .F. ) ;
#29249 = ORIENTED_EDGE ( 'NONE', *, *, #25289, .F. ) ;
#29250 = CARTESIAN_POINT ( 'NONE',  ( -27.08935880048753120, 2.219773948423736432, -0.6272370006475047610 ) ) ;
#29251 = CARTESIAN_POINT ( 'NONE',  ( 2.241317068080784569, 4.977030124433354352, 5.789053609344733786 ) ) ;
#29252 = CARTESIAN_POINT ( 'NONE',  ( 2.931247277082680291, -3.607110715259699951, -6.988361004535472709 ) ) ;
#29253 = CYLINDRICAL_SURFACE ( 'NONE', #42787, 4.999999999999999112 ) ;
#29254 = CARTESIAN_POINT ( 'NONE',  ( 2.844750968616391429, 6.613363922490658631, -4.202329849280680207 ) ) ;
#29255 = CARTESIAN_POINT ( 'NONE',  ( -37.00000000000000711, 4.725891942574755866, 10.75351884295729477 ) ) ;
#29256 = DIRECTION ( 'NONE',  ( -0.2034311943119418153, 0.9790892447477997917, 0.000000000000000000 ) ) ;
#29257 = VERTEX_POINT ( 'NONE', #52082 ) ;
#29258 = ORIENTED_EDGE ( 'NONE', *, *, #23188, .F. ) ;
#29259 = EDGE_LOOP ( 'NONE', ( #15921, #61530, #36045, #39561 ) ) ;
#29260 = CARTESIAN_POINT ( 'NONE',  ( 2.655192694323718960, -7.714239566600834763, -5.716669423975402786 ) ) ;
#29261 = CIRCLE ( 'NONE', #28224, 12.73084802173761787 ) ;
#29262 = CARTESIAN_POINT ( 'NONE',  ( 2.177405672433373685, 11.17876532284936530, -0.6747479782256756708 ) ) ;
#29263 = ORIENTED_EDGE ( 'NONE', *, *, #50664, .T. ) ;
#29264 = DIRECTION ( 'NONE',  ( 1.000000000000000000, -0.000000000000000000, 0.000000000000000000 ) ) ;
#29265 = DIRECTION ( 'NONE',  ( 1.000000000000000000, 0.000000000000000000, 0.000000000000000000 ) ) ;
#29266 = VERTEX_POINT ( 'NONE', #32747 ) ;
#29267 = CARTESIAN_POINT ( 'NONE',  ( 2.241526690369555652, 6.602966219605691300, -3.832206765347519362 ) ) ;
#29268 = EDGE_CURVE ( 'NONE', #59070, #44987, #9895, .T. ) ;
#29269 = EDGE_CURVE ( 'NONE', #5474, #2944, #51252, .T. ) ;
#29270 = CARTESIAN_POINT ( 'NONE',  ( 37.00000000000000711, 4.725891942574903304, 10.75351884295722193 ) ) ;
#29271 = DIRECTION ( 'NONE',  ( -1.000000000000000000, 0.000000000000000000, 0.000000000000000000 ) ) ;
#29272 = ORIENTED_EDGE ( 'NONE', *, *, #8704, .F. ) ;
#29273 = ORIENTED_EDGE ( 'NONE', *, *, #14702, .F. ) ;
#29274 = CYLINDRICAL_SURFACE ( 'NONE', #56509, 12.18650000000000055 ) ;
#29275 = EDGE_CURVE ( 'NONE', #43237, #395, #31043, .T. ) ;
#29276 = ORIENTED_EDGE ( 'NONE', *, *, #61996, .F. ) ;
#29277 = DIRECTION ( 'NONE',  ( 0.000000000000000000, -0.01356324068817998940, 0.9999080150203990547 ) ) ;
#29278 = VERTEX_POINT ( 'NONE', #62689 ) ;
#29279 = ORIENTED_EDGE ( 'NONE', *, *, #49350, .T. ) ;
#29280 = ORIENTED_EDGE ( 'NONE', *, *, #14777, .F. ) ;
#29281 = DIRECTION ( 'NONE',  ( -1.000000000000000000, 0.000000000000000000, 0.000000000000000000 ) ) ;
#29282 = CARTESIAN_POINT ( 'NONE',  ( -20.79170840334646542, 25.00000000000000000, -3.921648409140116698 ) ) ;
#29284 = EDGE_CURVE ( 'NONE', #2547, #35661, #40154, .T. ) ;
#29283 = CARTESIAN_POINT ( 'NONE',  ( 35.00000000000000000, 7.251710744571704836, 9.240395740215555875 ) ) ;
#29285 = CARTESIAN_POINT ( 'NONE',  ( -22.35190811654613441, -3.898012445334715359, 0.2457675311904958526 ) ) ;
#29286 = VERTEX_POINT ( 'NONE', #17157 ) ;
#29287 = CARTESIAN_POINT ( 'NONE',  ( 1.283627346226322130, 11.16434663959558904, 5.810034161408879072 ) ) ;
#29288 = ORIENTED_EDGE ( 'NONE', *, *, #18100, .F. ) ;
#29289 = CARTESIAN_POINT ( 'NONE',  ( -15.27729454824424948, 5.151216734910788908, 25.00000000000000000 ) ) ;
#29290 = ADVANCED_FACE ( 'NONE', ( #37430 ), #50695, .F. ) ;
#29291 = CARTESIAN_POINT ( 'NONE',  ( -17.67250291340853607, -7.948201322890581011, -10.91603686538583418 ) ) ;
#29292 = VERTEX_POINT ( 'NONE', #59692 ) ;
#29293 = CARTESIAN_POINT ( 'NONE',  ( -15.94818086038523752, 8.395239208160713673, 8.574438310199999691 ) ) ;
#29294 = DIRECTION ( 'NONE',  ( -1.000000000000000000, -0.000000000000000000, 0.000000000000000000 ) ) ;
#29295 = DIRECTION ( 'NONE',  ( -1.000000000000000000, 0.000000000000000000, -0.000000000000000000 ) ) ;
#29296 = VECTOR ( 'NONE', #2810, 1000.000000000000227 ) ;
#29297 = ORIENTED_EDGE ( 'NONE', *, *, #18498, .T. ) ;
#29298 = ORIENTED_EDGE ( 'NONE', *, *, #3907, .T. ) ;
#29299 = CARTESIAN_POINT ( 'NONE',  ( -35.04660725145885891, 0.003039313842369092532, 0.01191704700713624304 ) ) ;
#29300 = EDGE_CURVE ( 'NONE', #9098, #15712, #38079, .T. ) ;
#29301 = ORIENTED_EDGE ( 'NONE', *, *, #40597, .F. ) ;
#29302 = CARTESIAN_POINT ( 'NONE',  ( -42.50000000000000000, -2.710505431213761085E-17, 1.201363017033314212E-18 ) ) ;
#29303 = DIRECTION ( 'NONE',  ( -1.000000000000000000, 0.000000000000000000, -0.000000000000000000 ) ) ;
#29304 = CARTESIAN_POINT ( 'NONE',  ( 5.029029651858286876, -26.84634345473923034, 15.78007771861068775 ) ) ;
#29305 = CARTESIAN_POINT ( 'NONE',  ( 0.3106921474978470155, -9.239619355094093933, -8.060345844326381126 ) ) ;
#29306 = CARTESIAN_POINT ( 'NONE',  ( 11.34628703507253178, 11.92903996101671460, -1.310401472515283716 ) ) ;
#29307 = EDGE_LOOP ( 'NONE', ( #15, #45129, #64623, #61979 ) ) ;
#29308 = CARTESIAN_POINT ( 'NONE',  ( 3.152665057736164123, 5.461013642407259283, 5.761241965767907480 ) ) ;
#29309 = CARTESIAN_POINT ( 'NONE',  ( 1.462291587749436683, 1.569662666436903997, 12.54737685278351655 ) ) ;
#29310 = CARTESIAN_POINT ( 'NONE',  ( -6.997870572558777091, -27.10943569200529524, -15.36011607788393540 ) ) ;
#29311 = CARTESIAN_POINT ( 'NONE',  ( 2.507146904658098308, -5.128007631637100161, 5.774795220010169317 ) ) ;
#29312 = CARTESIAN_POINT ( 'NONE',  ( 1.719304012341412724, 2.961219984259706450, -12.38166659046466300 ) ) ;
#29313 = CARTESIAN_POINT ( 'NONE',  ( 6.812204945636112896, -4.138731716409435712, -11.26369831714194092 ) ) ;
#29314 = CYLINDRICAL_SURFACE ( 'NONE', #59805, 4.999999999999999112 ) ;
#29315 = B_SPLINE_CURVE_WITH_KNOTS ( 'NONE', 3,
 ( #64522, #4029, #54891, #34904, #18993, #60524, #4707, #45241, #50248, #25278, #5015, #65192, #60201, #39595, #29939, #65498, #55212, #19659, #39259 ),
 .UNSPECIFIED., .F., .F.,
 ( 4, 3, 3, 3, 3, 3, 4 ),
 ( 8.641030098560686409E-18, 2.825908398831582569E-05, 4.208813692484607576E-05, 5.591713746944476323E-05, 6.279584083232501513E-05, 9.105792820297718617E-05, 0.0001153131102488831687 ),
 .UNSPECIFIED. ) ;
#29316 = ADVANCED_FACE ( 'NONE', ( #4161 ), #14118, .T. ) ;
#29317 = CIRCLE ( 'NONE', #51651, 12.18649999999999700 ) ;
#29318 = VERTEX_POINT ( 'NONE', #24424 ) ;
#29319 = DIRECTION ( 'NONE',  ( -1.000000000000000000, 0.000000000000000000, 0.000000000000000000 ) ) ;
#29320 = AXIS2_PLACEMENT_3D ( 'NONE', #62917, #42966, #41653 ) ;
#29321 = ORIENTED_EDGE ( 'NONE', *, *, #54536, .T. ) ;
#29323 =( BOUNDED_SURFACE ( )  B_SPLINE_SURFACE ( 3, 1, ( 
 ( #17766, #44322 ),
 ( #33378, #39335 ),
 ( #49362, #43020 ),
 ( #43338, #53677 ) ),
 .UNSPECIFIED., .F., .F., .F. ) 
 B_SPLINE_SURFACE_WITH_KNOTS ( ( 4, 4 ),
 ( 2, 2 ),
 ( 0.000000000000000000, 1.000000000000000000 ),
 ( 0.000000000000000000, 1.000000000000000000 ),
 .UNSPECIFIED. ) 
 GEOMETRIC_REPRESENTATION_ITEM ( )  RATIONAL_B_SPLINE_SURFACE ( (
 ( 1.000000000000000000, 1.000000000000000000),
 ( 0.6933888150995267674, 0.9895912004443193632),
 ( 0.6933888150995267674, 0.9895912004443193632),
 ( 1.000000000000000000, 1.000000000000000000) ) ) 
 REPRESENTATION_ITEM ( '' )  SURFACE ( )  );
#29322 = FACE_OUTER_BOUND ( 'NONE', #47447, .T. ) ;
#29324 = CARTESIAN_POINT ( 'NONE',  ( -35.04683013664716640, -0.002177781393184786973, 0.01216443238270097441 ) ) ;
#29325 = FACE_OUTER_BOUND ( 'NONE', #28284, .T. ) ;
#29326 = DIRECTION ( 'NONE',  ( -1.000000000000000000, 0.000000000000000000, 0.000000000000000000 ) ) ;
#29327 = ORIENTED_EDGE ( 'NONE', *, *, #3419, .T. ) ;
#29328 = VERTEX_POINT ( 'NONE', #23804 ) ;
#29329 = ORIENTED_EDGE ( 'NONE', *, *, #27568, .F. ) ;
#29330 = LINE ( 'NONE', #38979, #39746 ) ;
#29331 = ADVANCED_FACE ( 'NONE', ( #34413 ), #18804, .T. ) ;
#29332 = VERTEX_POINT ( 'NONE', #63349 ) ;
#29333 = CARTESIAN_POINT ( 'NONE',  ( -22.27719443589224113, -2.462030382548427543, -2.737335337013111936 ) ) ;
#29334 = DIRECTION ( 'NONE',  ( 0.000000000000000000, -0.01356324068817998940, 0.9999080150203990547 ) ) ;
#29335 = CARTESIAN_POINT ( 'NONE',  ( 0.2646305136544065406, 9.465888453933068547, -7.770320294339078337 ) ) ;
#29336 = DIRECTION ( 'NONE',  ( 0.000000000000000000, 0.9987865678893275145, -0.04924826701374940968 ) ) ;
#29337 = ORIENTED_EDGE ( 'NONE', *, *, #40744, .T. ) ;
#29338 = CARTESIAN_POINT ( 'NONE',  ( -27.19357181888462094, -10.84410562793472543, 5.138615876886901468 ) ) ;
#29339 = EDGE_CURVE ( 'NONE', #53140, #31809, #36976, .T. ) ;
#29340 = CARTESIAN_POINT ( 'NONE',  ( -7.103478058731402811, -31.43429545818153414, -14.15162322622638946 ) ) ;
#29341 = DIRECTION ( 'NONE',  ( 0.000000000000000000, 0.000000000000000000, -1.000000000000000000 ) ) ;
#29343 = ORIENTED_EDGE ( 'NONE', *, *, #7835, .T. ) ;
#29342 = DIRECTION ( 'NONE',  ( -0.3865475372811021937, -0.9220659470476462172, 0.01937500237528096830 ) ) ;
#29344 = CARTESIAN_POINT ( 'NONE',  ( -22.28506771379528573, -3.622079238249909849, -0.8783543640077282610 ) ) ;
#29345 = EDGE_CURVE ( 'NONE', #2755, #25848, #63667, .T. ) ;
#29346 = ORIENTED_EDGE ( 'NONE', *, *, #2640, .T. ) ;
#29347 = CARTESIAN_POINT ( 'NONE',  ( 1.375507693218919636, -10.03411718356142046, 7.647735792765052665 ) ) ;
#29348 = ORIENTED_EDGE ( 'NONE', *, *, #50217, .T. ) ;
#29349 = CARTESIAN_POINT ( 'NONE',  ( -29.46118758560114514, 0.7225184543564773243, -11.98011844538937787 ) ) ;
#29350 = CARTESIAN_POINT ( 'NONE',  ( -35.05175862995318425, 0.001087818442111268546, 0.01253051761584966783 ) ) ;
#29351 = CARTESIAN_POINT ( 'NONE',  ( 0.000000000000000000, -4.976357229393820525, -4.652926418895619420 ) ) ;
#29352 = CARTESIAN_POINT ( 'NONE',  ( -35.00000000000000000, -2.250029553613845934, 12.54989509947650284 ) ) ;
#29353 = DIRECTION ( 'NONE',  ( -1.000000000000000000, -0.000000000000000000, -0.000000000000000000 ) ) ;
#29354 = ADVANCED_FACE ( 'NONE', ( #38753 ), #64012, .T. ) ;
#29355 = CARTESIAN_POINT ( 'NONE',  ( -27.10128162969864007, -0.1566844438592166489, -2.337214317750539561 ) ) ;
#29356 = DIRECTION ( 'NONE',  ( 0.000000000000000000, 0.01356324068817998940, -0.9999080150203990547 ) ) ;
#29358 = EDGE_LOOP ( 'NONE', ( #10025, #52897, #38064, #10684 ) ) ;
#29357 = DIRECTION ( 'NONE',  ( 0.000000000000000000, -1.000000000000000000, 0.000000000000000000 ) ) ;
#29359 = B_SPLINE_CURVE_WITH_KNOTS ( 'NONE', 3,
 ( #58898, #22972, #7672, #23958, #53883, #2369, #59203, #18957, #22643, #53568, #44217, #8321, #27604, #3695, #3356, #37918, #43226, #8015, #3024 ),
 .UNSPECIFIED., .F., .F.,
 ( 4, 3, 3, 3, 3, 3, 4 ),
 ( 4.336808689942017736E-19, 2.831840207499692930E-05, 4.217266859840731959E-05, 5.602024318396171940E-05, 6.290810167969236371E-05, 9.120440630945234051E-05, 0.0001153103026479759542 ),
 .UNSPECIFIED. ) ;
#29360 = ORIENTED_EDGE ( 'NONE', *, *, #33515, .T. ) ;
#29361 = DIRECTION ( 'NONE',  ( 0.000000000000000000, 0.000000000000000000, -1.000000000000000000 ) ) ;
#29362 = ORIENTED_EDGE ( 'NONE', *, *, #33769, .T. ) ;
#29363 = EDGE_CURVE ( 'NONE', #64644, #13346, #22130, .T. ) ;
#29364 = ORIENTED_EDGE ( 'NONE', *, *, #53768, .T. ) ;
#29365 = CARTESIAN_POINT ( 'NONE',  ( 0.9232167919969098691, 1.756271097262231073, -12.34114433434356251 ) ) ;
#29366 = CARTESIAN_POINT ( 'NONE',  ( -35.00000000000000000, -11.24036214326516436, -6.018036132182280618 ) ) ;
#29367 = DIRECTION ( 'NONE',  ( 1.000000000000000000, 0.000000000000000000, 0.000000000000000000 ) ) ;
#29368 = TOROIDAL_SURFACE ( 'NONE', #9318, 20.19615242270663558, 4.000000000000000000 ) ;
#29369 = CARTESIAN_POINT ( 'NONE',  ( 35.00000000000000000, -10.54834585426224258, -6.102719229070642903 ) ) ;
#29370 = EDGE_CURVE ( 'NONE', #50038, #58596, #14652, .T. ) ;
#29371 = CARTESIAN_POINT ( 'NONE',  ( -22.29479313954897535, 1.627767898183768658, -3.360948587163225199 ) ) ;
#29372 = CYLINDRICAL_SURFACE ( 'NONE', #45724, 12.18650000000000055 ) ;
#29373 = VECTOR ( 'NONE', #63264, 1000.000000000000000 ) ;
#29374 = DIRECTION ( 'NONE',  ( -1.000000000000000000, 0.000000000000000000, 0.000000000000000000 ) ) ;
#29375 = EDGE_CURVE ( 'NONE', #29328, #61621, #33795, .T. ) ;
#29376 = ORIENTED_EDGE ( 'NONE', *, *, #30675, .F. ) ;
#29377 = DIRECTION ( 'NONE',  ( -0.7886918350401376232, 0.6147887355352408267, 0.000000000000000000 ) ) ;
#29378 = EDGE_CURVE ( 'NONE', #35137, #47422, #26128, .T. ) ;
#29379 = CARTESIAN_POINT ( 'NONE',  ( -27.08421860617808008, -1.394838596205207448, -1.817782142550201208 ) ) ;
#29380 = CARTESIAN_POINT ( 'NONE',  ( -17.62939896453930544, -5.509730556738257512, 12.32537139461556386 ) ) ;
#29381 = VERTEX_POINT ( 'NONE', #54047 ) ;
#29382 = CARTESIAN_POINT ( 'NONE',  ( 37.49868115534709290, -2.226531222652221143, -21.71250474234130579 ) ) ;
#29383 = DIRECTION ( 'NONE',  ( 0.000000000000000000, 0.000000000000000000, 1.000000000000000000 ) ) ;
#29384 = VERTEX_POINT ( 'NONE', #2870 ) ;
#29385 = CARTESIAN_POINT ( 'NONE',  ( 1.937114397841932290, -3.531416430611214796, -12.33981801388261346 ) ) ;
#29386 = CARTESIAN_POINT ( 'NONE',  ( -35.00000000000000000, -6.711949091238219367, 10.84030624090604178 ) ) ;
#29387 = CARTESIAN_POINT ( 'NONE',  ( 1.009264106688026130, 0.1360895039168394938, 12.00328975538737630 ) ) ;
#29388 = EDGE_CURVE ( 'NONE', #63989, #24479, #28486, .T. ) ;
#29389 = EDGE_CURVE ( 'NONE', #40279, #50140, #23126, .T. ) ;
#29390 = CARTESIAN_POINT ( 'NONE',  ( 35.00000000000000000, -11.72195762423410414, -0.7536123767498126291 ) ) ;
#29391 = CARTESIAN_POINT ( 'NONE',  ( 2.000000000000001776, 0.000000000000000000, 0.000000000000000000 ) ) ;
#29392 = ORIENTED_EDGE ( 'NONE', *, *, #23485, .F. ) ;
#29393 = LINE ( 'NONE', #24402, #24728 ) ;
#29394 = DIRECTION ( 'NONE',  ( 0.000000000000000000, 0.01356324068817992175, -0.9999080150203990547 ) ) ;
#29395 = CARTESIAN_POINT ( 'NONE',  ( -18.44728739097037007, 4.191944866150937976, -11.24471234151735999 ) ) ;
#29396 = ORIENTED_EDGE ( 'NONE', *, *, #19546, .T. ) ;
#29397 = CYLINDRICAL_SURFACE ( 'NONE', #8528, 5.000000000000000888 ) ;
#29398 = CARTESIAN_POINT ( 'NONE',  ( -2.532614230583023041, -12.88560382747352584, 4.026315189028235153 ) ) ;
#29399 = ORIENTED_EDGE ( 'NONE', *, *, #40123, .F. ) ;
#29400 = ADVANCED_FACE ( 'NONE', ( #64988 ), #5148, .T. ) ;
#29401 = ORIENTED_EDGE ( 'NONE', *, *, #13110, .T. ) ;
#29402 = CIRCLE ( 'NONE', #64426, 5.000000000000001776 ) ;
#29403 = ORIENTED_EDGE ( 'NONE', *, *, #46528, .T. ) ;
#29404 = CYLINDRICAL_SURFACE ( 'NONE', #3491, 12.18649999999999878 ) ;
#29405 = B_SPLINE_CURVE_WITH_KNOTS ( 'NONE', 3,
 ( #56065, #35764, #52074, #25824, #15816, #21828 ),
 .UNSPECIFIED., .F., .F.,
 ( 4, 2, 4 ),
 ( 0.000000000000000000, 0.0004528561986909412115, 0.0009057123973818824230 ),
 .UNSPECIFIED. ) ;
#29406 = ADVANCED_FACE ( 'NONE', ( #39730 ), #46043, .T. ) ;
#29407 = VECTOR ( 'NONE', #1713, 1000.000000000000000 ) ;
#29408 = VERTEX_POINT ( 'NONE', #40712 ) ;
#29409 = DIRECTION ( 'NONE',  ( -1.000000000000000000, 0.000000000000000000, 0.000000000000000000 ) ) ;
#29410 = DIRECTION ( 'NONE',  ( -0.000000000000000000, -1.000000000000000000, -0.000000000000000000 ) ) ;
#29411 = CARTESIAN_POINT ( 'NONE',  ( 0.2657645697724702605, -6.253766234003993674, 10.52916014490829077 ) ) ;
#29412 = DIRECTION ( 'NONE',  ( -1.000000000000000000, 0.000000000000000000, 0.000000000000000000 ) ) ;
#29413 = DIRECTION ( 'NONE',  ( 0.000000000000000000, 0.000000000000000000, -1.000000000000000000 ) ) ;
#29415 = ORIENTED_EDGE ( 'NONE', *, *, #30754, .F. ) ;
#29414 = CARTESIAN_POINT ( 'NONE',  ( 1.462291587748365540, 7.633056170898332660, 10.08151577214832173 ) ) ;
#29416 = LINE ( 'NONE', #54386, #7622 ) ;
#29417 = EDGE_CURVE ( 'NONE', #26404, #9789, #45476, .T. ) ;
#29418 = VERTEX_POINT ( 'NONE', #60023 ) ;
#29419 = CARTESIAN_POINT ( 'NONE',  ( 0.2651627923886338278, 10.64925183219501470, -6.046629261473224659 ) ) ;
#29420 = ORIENTED_EDGE ( 'NONE', *, *, #11614, .T. ) ;
#29421 = ORIENTED_EDGE ( 'NONE', *, *, #55676, .F. ) ;
#29422 = CARTESIAN_POINT ( 'NONE',  ( -22.28169757117798611, -0.9284931499057216264, 3.576542310004385605 ) ) ;
#29423 = CARTESIAN_POINT ( 'NONE',  ( -8.269707202464745777, -27.33416996378174701, 14.97774446421776240 ) ) ;
#29424 = CARTESIAN_POINT ( 'NONE',  ( -24.30799348672965010, 10.28595639659987881, 8.745824847788130185 ) ) ;
#29425 = CARTESIAN_POINT ( 'NONE',  ( 24.39805594623851093, -0.9048399250569106878, 11.96720254132417338 ) ) ;
#29426 = CARTESIAN_POINT ( 'NONE',  ( 5.530133899448235191, 0.001661287012794350655, -0.01589823604557753789 ) ) ;
#29427 = CARTESIAN_POINT ( 'NONE',  ( 2.260457164925428586, 5.941202713842286265, 4.804526096744350383 ) ) ;
#29428 = ORIENTED_EDGE ( 'NONE', *, *, #47247, .F. ) ;
#29429 = VERTEX_POINT ( 'NONE', #51374 ) ;
#29430 = CARTESIAN_POINT ( 'NONE',  ( 37.00000000000000711, -5.710938531231790627, -11.39945968423469580 ) ) ;
#29431 = ORIENTED_EDGE ( 'NONE', *, *, #57033, .F. ) ;
#29432 = FACE_OUTER_BOUND ( 'NONE', #32010, .T. ) ;
#29433 = DIRECTION ( 'NONE',  ( 1.000000000000000000, -0.000000000000000000, -0.000000000000000000 ) ) ;
#29434 = CARTESIAN_POINT ( 'NONE',  ( 35.00000000000000000, 11.26103545359850955, -3.340853584269734000 ) ) ;
#29435 = EDGE_CURVE ( 'NONE', #16609, #14915, #16812, .T. ) ;
#29436 = DIRECTION ( 'NONE',  ( -1.000000000000000000, 0.000000000000000000, 0.000000000000000000 ) ) ;
#29437 = CARTESIAN_POINT ( 'NONE',  ( 35.00000000000000000, 12.18632975068352664, 0.06441628369840225743 ) ) ;
#29438 = EDGE_CURVE ( 'NONE', #65388, #9878, #5825, .T. ) ;
#29439 = DIRECTION ( 'NONE',  ( 1.000000000000000000, 1.685093406416449860E-16, -1.011030131491573426E-17 ) ) ;
#29440 = VERTEX_POINT ( 'NONE', #30717 ) ;
#29441 = VERTEX_POINT ( 'NONE', #34716 ) ;
#29442 = EDGE_CURVE ( 'NONE', #32242, #18051, #34875, .T. ) ;
#29443 = CARTESIAN_POINT ( 'NONE',  ( -35.00000000000000000, 0.000000000000000000, 0.000000000000000000 ) ) ;
#29444 = DIRECTION ( 'NONE',  ( -1.000000000000000000, 0.000000000000000000, 0.000000000000000000 ) ) ;
#29445 = CARTESIAN_POINT ( 'NONE',  ( -37.00000000000000711, 11.66953048682404415, -3.511814412391998541 ) ) ;
#29446 = CARTESIAN_POINT ( 'NONE',  ( 3.152665057734131526, -0.9030954876737319337, -7.886634106564212487 ) ) ;
#29447 = CARTESIAN_POINT ( 'NONE',  ( -28.24722641916570254, 12.60412408455661115, -4.845634205101751135 ) ) ;
#29448 = AXIS2_PLACEMENT_3D ( 'NONE', #17159, #37100, #6211 ) ;
#29449 = DIRECTION ( 'NONE',  ( -1.000000000000000000, 0.000000000000000000, -0.000000000000000000 ) ) ;
#29450 = DIRECTION ( 'NONE',  ( 1.000000000000000000, -0.000000000000000000, -0.000000000000000000 ) ) ;
#29451 = DIRECTION ( 'NONE',  ( 0.000000000000000000, -0.2618041379715703165, 0.9651210252299775583 ) ) ;
#29452 = DIRECTION ( 'NONE',  ( 0.000000000000000000, 0.8827602140260299990, -0.4698238015817395308 ) ) ;
#29453 = ORIENTED_EDGE ( 'NONE', *, *, #59029, .T. ) ;
#29454 = DIRECTION ( 'NONE',  ( 0.2235469969004301449, -0.9746931518056330956, 0.000000000000000000 ) ) ;
#29455 = DIRECTION ( 'NONE',  ( -1.000000000000000000, 0.000000000000000000, 0.000000000000000000 ) ) ;
#29456 = CARTESIAN_POINT ( 'NONE',  ( 1.719304012338201737, 9.242227816402087015, 8.755325027793320558 ) ) ;
#29457 = EDGE_CURVE ( 'NONE', #15504, #52589, #30611, .T. ) ;
#29458 = CARTESIAN_POINT ( 'NONE',  ( 3.152665057734125309, -6.622010822086626725, -4.377619405892440696 ) ) ;
#29459 = EDGE_CURVE ( 'NONE', #48402, #32375, #41247, .T. ) ;
#29460 = CARTESIAN_POINT ( 'NONE',  ( -22.27706485742869091, -1.508175983031604606, 3.358064672837097753 ) ) ;
#29461 = ORIENTED_EDGE ( 'NONE', *, *, #33149, .T. ) ;
#29462 = CARTESIAN_POINT ( 'NONE',  ( -22.30625920655495165, 3.783486345733975131, -0.2529928606556600679 ) ) ;
#29463 = CYLINDRICAL_SURFACE ( 'NONE', #9959, 12.74999999999999822 ) ;
#29464 = CARTESIAN_POINT ( 'NONE',  ( -7.119438362040798829, -32.04078451673858297, -13.23628618373588317 ) ) ;
#29465 = ORIENTED_EDGE ( 'NONE', *, *, #39980, .T. ) ;
#29466 = DIRECTION ( 'NONE',  ( 0.000000000000000000, -0.4134677391718576955, -0.9105187689795926076 ) ) ;
#29467 = CARTESIAN_POINT ( 'NONE',  ( 37.00000000000000711, -9.733281772932102172, 8.235637554476744171 ) ) ;
#29468 = DIRECTION ( 'NONE',  ( -1.000000000000000000, 0.000000000000000000, 0.000000000000000000 ) ) ;
#29469 = ADVANCED_FACE ( 'NONE', ( #25414 ), #24771, .T. ) ;
#29470 = CYLINDRICAL_SURFACE ( 'NONE', #44512, 4.999999999999999112 ) ;
#29471 = CARTESIAN_POINT ( 'NONE',  ( -9.089039412240934368, -10.06143729587027735, -9.029120393835746938 ) ) ;
#29472 = AXIS2_PLACEMENT_3D ( 'NONE', #50871, #49574, #39898 ) ;
#29473 = CARTESIAN_POINT ( 'NONE',  ( 35.00000000000000000, 5.644643009979216863, 10.30098186818242922 ) ) ;
#29474 = ORIENTED_EDGE ( 'NONE', *, *, #18866, .F. ) ;
#29475 = DIRECTION ( 'NONE',  ( 0.000000000000000000, -0.01356324068817998940, 0.9999080150203990547 ) ) ;
#29476 = LINE ( 'NONE', #9197, #29836 ) ;
#29477 = AXIS2_PLACEMENT_3D ( 'NONE', #60162, #23709, #3442 ) ;
#29478 = CARTESIAN_POINT ( 'NONE',  ( -10.00000000000000178, 0.000000000000000000, 0.000000000000000000 ) ) ;
#29479 = CARTESIAN_POINT ( 'NONE',  ( 2.000000000000001776, -4.409940824963369366, -5.354199675985328533 ) ) ;
#29480 = LINE ( 'NONE', #38825, #55581 ) ;
#29481 = CARTESIAN_POINT ( 'NONE',  ( -22.70624764888619751, 5.249808673991985586, 0.08990180771013302208 ) ) ;
#29482 = CARTESIAN_POINT ( 'NONE',  ( -35.00000000000000000, 0.000000000000000000, 0.000000000000000000 ) ) ;
#29483 = CARTESIAN_POINT ( 'NONE',  ( -37.00000000000000711, 0.3025107581132838175, -11.74226168163341377 ) ) ;
#29484 = ORIENTED_EDGE ( 'NONE', *, *, #57818, .T. ) ;
#29485 = EDGE_CURVE ( 'NONE', #26426, #27538, #15749, .T. ) ;
#29486 = VERTEX_POINT ( 'NONE', #36028 ) ;
#29487 = CARTESIAN_POINT ( 'NONE',  ( -17.81785227179914699, -6.314196589589617936, -10.20856936847407503 ) ) ;
#29488 = ORIENTED_EDGE ( 'NONE', *, *, #40656, .F. ) ;
#29489 = CIRCLE ( 'NONE', #63477, 7.499999999999988454 ) ;
#29490 = EDGE_CURVE ( 'NONE', #32582, #62051, #51872, .T. ) ;
#29491 = CARTESIAN_POINT ( 'NONE',  ( -15.27729454824424948, 5.151216734910788908, 25.00000000000000000 ) ) ;
#29492 = AXIS2_PLACEMENT_3D ( 'NONE', #28691, #38336, #53974 ) ;
#29493 = FACE_OUTER_BOUND ( 'NONE', #44303, .T. ) ;
#29494 = EDGE_LOOP ( 'NONE', ( #58214, #6878, #16170, #61538 ) ) ;
#29495 = FACE_OUTER_BOUND ( 'NONE', #5318, .T. ) ;
#29496 =( BOUNDED_CURVE ( )  B_SPLINE_CURVE ( 3, ( #28153, #33468, #12841, #28463 ),
 .UNSPECIFIED., .F., .F. ) 
 B_SPLINE_CURVE_WITH_KNOTS ( ( 4, 4 ),
 ( 1.276435708367962052, 1.280436945677107419 ),
 .UNSPECIFIED. ) 
 CURVE ( )  GEOMETRIC_REPRESENTATION_ITEM ( )  RATIONAL_B_SPLINE_CURVE ( ( 1.000000000000000000, 0.9999986658421111674, 0.9999986658421111674, 1.000000000000000000 ) ) 
 REPRESENTATION_ITEM ( '' )  );
#29497 = CARTESIAN_POINT ( 'NONE',  ( 12.86876090758356561, 11.06400415918094993, -4.650693114441405207 ) ) ;
#29498 = CARTESIAN_POINT ( 'NONE',  ( 2.251152103364165935, -5.004701566806020629, -5.769488058190294311 ) ) ;
#29499 = ORIENTED_EDGE ( 'NONE', *, *, #64000, .T. ) ;
#29500 = VERTEX_POINT ( 'NONE', #10773 ) ;
#29501 = CARTESIAN_POINT ( 'NONE',  ( 2.770579946183334030, 0.3031629740256825967, -7.804957730865686116 ) ) ;
#29502 = DIRECTION ( 'NONE',  ( 0.000000000000000000, 0.01356324068817998940, -0.9999080150203989437 ) ) ;
#29503 = ORIENTED_EDGE ( 'NONE', *, *, #39144, .T. ) ;
#29504 = CARTESIAN_POINT ( 'NONE',  ( 6.778363379174657588, -6.828539355312321923, -9.876072021181311555 ) ) ;
#29505 = ORIENTED_EDGE ( 'NONE', *, *, #40536, .F. ) ;
#29506 = DIRECTION ( 'NONE',  ( 0.000000000000000000, -0.7790879021242574920, 0.6269146997507901720 ) ) ;
#29507 = EDGE_CURVE ( 'NONE', #36274, #13985, #19789, .T. ) ;
#29508 = CARTESIAN_POINT ( 'NONE',  ( -37.00000000000000711, 0.000000000000000000, 0.000000000000000000 ) ) ;
#29509 = DIRECTION ( 'NONE',  ( 0.000000000000000000, -0.5472293298355157543, 0.8369827122275419473 ) ) ;
#29510 = ADVANCED_FACE ( 'NONE', ( #20762 ), #5247, .F. ) ;
#29511 = DIRECTION ( 'NONE',  ( 1.000000000000000000, 0.000000000000000000, 0.000000000000000000 ) ) ;
#29512 = EDGE_LOOP ( 'NONE', ( #7035, #31368, #58944, #42551 ) ) ;
#29513 = DIRECTION ( 'NONE',  ( -1.000000000000000000, 0.000000000000000000, 0.000000000000000000 ) ) ;
#29514 = CARTESIAN_POINT ( 'NONE',  ( -14.74468430517067219, 7.920754711258918057, 9.014586841720371169 ) ) ;
#29515 = EDGE_CURVE ( 'NONE', #8204, #45350, #4832, .T. ) ;
#29516 = DIRECTION ( 'NONE',  ( 1.000000000000000000, 0.000000000000000000, -0.000000000000000000 ) ) ;
#29517 = DIRECTION ( 'NONE',  ( -1.000000000000000000, -0.000000000000000000, 0.000000000000000000 ) ) ;
#29518 = CARTESIAN_POINT ( 'NONE',  ( -37.00000000000000711, -9.060822531526103063, 7.474872387600973944 ) ) ;
#29519 = CARTESIAN_POINT ( 'NONE',  ( -27.09342121492660382, 1.607500752098853347, -1.671264186073224911 ) ) ;
#29520 = LINE ( 'NONE', #45468, #9640 ) ;
#29521 = DIRECTION ( 'NONE',  ( 0.000000000000000000, 0.01356324068817998940, -0.9999080150203989437 ) ) ;
#29522 = DIRECTION ( 'NONE',  ( -0.000000000000000000, -0.000000000000000000, -1.000000000000000000 ) ) ;
#29523 = CIRCLE ( 'NONE', #42274, 12.18650000000000233 ) ;
#29524 = VERTEX_POINT ( 'NONE', #10127 ) ;
#29525 = DIRECTION ( 'NONE',  ( -1.000000000000000000, 0.000000000000000000, 0.000000000000000000 ) ) ;
#29526 = AXIS2_PLACEMENT_3D ( 'NONE', #48239, #58527, #28254 ) ;
#29527 = ORIENTED_EDGE ( 'NONE', *, *, #15569, .T. ) ;
#29528 = CARTESIAN_POINT ( 'NONE',  ( 2.262775599886255762, -7.499645832851588700, -1.465770593192964544 ) ) ;
#29529 = FACE_OUTER_BOUND ( 'NONE', #48138, .T. ) ;
#29530 = DIRECTION ( 'NONE',  ( -1.000000000000000000, 0.000000000000000000, -0.000000000000000000 ) ) ;
#29531 = CARTESIAN_POINT ( 'NONE',  ( 2.907497136251153691, 5.319973245618665025, 5.781215374755499958 ) ) ;
#29532 = ORIENTED_EDGE ( 'NONE', *, *, #63655, .T. ) ;
#29533 = CARTESIAN_POINT ( 'NONE',  ( 12.52750123246316072, 0.4973700281276248192, 11.98968819674307618 ) ) ;
#29534 = CARTESIAN_POINT ( 'NONE',  ( 35.00000000000000000, -11.91791701451267826, -2.544412758415803388 ) ) ;
#29535 = CYLINDRICAL_SURFACE ( 'NONE', #47107, 4.999999999999999112 ) ;
#29536 = CONICAL_SURFACE ( 'NONE', #42243, 7.938172270156617749, 1.280189991382167047 ) ;
#29537 = CARTESIAN_POINT ( 'NONE',  ( 15.08189101924309128, -34.00125857029148335, -8.507794521698972545 ) ) ;
#29538 = B_SPLINE_CURVE_WITH_KNOTS ( 'NONE', 3,
 ( #10048, #16914, #16262, #36867, #41855, #9703, #62783, #40285, #50622, #61806, #30329, #5986, #11916, #1953, #26242, #37181, #52517, #60578, #26559 ),
 .UNSPECIFIED., .F., .F.,
 ( 4, 3, 3, 3, 3, 3, 4 ),
 ( 0.000000000000000000, 2.832085443685330487E-05, 4.217789847592287914E-05, 5.603488375296597566E-05, 6.989180858882679389E-05, 9.821094830335311678E-05, 0.0001178165571463684675 ),
 .UNSPECIFIED. ) ;
#29539 = ADVANCED_FACE ( 'NONE', ( #10438 ), #57989, .T. ) ;
#29540 = DIRECTION ( 'NONE',  ( 0.000000000000000000, 0.000000000000000000, 1.000000000000000000 ) ) ;
#29541 = ORIENTED_EDGE ( 'NONE', *, *, #8794, .T. ) ;
#29542 = CARTESIAN_POINT ( 'NONE',  ( 8.621148270653568702, 25.00000000000000000, -5.251012286260225537 ) ) ;
#29543 = VERTEX_POINT ( 'NONE', #21762 ) ;
#29544 = CARTESIAN_POINT ( 'NONE',  ( -35.00000000000000000, 11.73808581813437968, -0.4353888892048790038 ) ) ;
#29545 = FACE_OUTER_BOUND ( 'NONE', #40012, .T. ) ;
#29546 = CARTESIAN_POINT ( 'NONE',  ( 0.000000000000000000, -6.767909380267597363, -0.7805499053121327524 ) ) ;
#29547 = EDGE_CURVE ( 'NONE', #16066, #21159, #52009, .T. ) ;
#29548 = CONICAL_SURFACE ( 'NONE', #43512, 7.938172270156617749, 1.280189991382167047 ) ;
#29549 = VERTEX_POINT ( 'NONE', #21071 ) ;
#29550 = ORIENTED_EDGE ( 'NONE', *, *, #45767, .F. ) ;
#29551 = CARTESIAN_POINT ( 'NONE',  ( 47.00000000000000711, 4.705694406421931860E-17, -3.469127814946512892E-15 ) ) ;
#29552 = ORIENTED_EDGE ( 'NONE', *, *, #60332, .T. ) ;
#29553 = CARTESIAN_POINT ( 'NONE',  ( 2.259025283527870798, 5.014999102875606241, 5.764013728792329871 ) ) ;
#29554 = DIRECTION ( 'NONE',  ( -0.000000000000000000, -1.000000000000000000, -0.000000000000000000 ) ) ;
#29555 = DIRECTION ( 'NONE',  ( 0.000000000000000000, -0.7381862504172023165, 0.6745969609292585822 ) ) ;
#29556 = CARTESIAN_POINT ( 'NONE',  ( 0.3537226245948385528, 12.27287980220284780, 0.2609894354289943874 ) ) ;
#29558 = CARTESIAN_POINT ( 'NONE',  ( 0.3341166715381307384, 9.234320413907912695, -8.078283863465406611 ) ) ;
#29557 = AXIS2_PLACEMENT_3D ( 'NONE', #46776, #16530, #45796 ) ;
#29559 = DIRECTION ( 'NONE',  ( -1.000000000000000000, 0.000000000000000000, 0.000000000000000000 ) ) ;
#29560 = CARTESIAN_POINT ( 'NONE',  ( -35.00000000000000000, -0.3025107581132014389, 11.74226168163341200 ) ) ;
#29561 = EDGE_LOOP ( 'NONE', ( #48448, #26320, #47077, #5177 ) ) ;
#29562 = EDGE_CURVE ( 'NONE', #49868, #39894, #57188, .T. ) ;
#29563 = ORIENTED_EDGE ( 'NONE', *, *, #24901, .T. ) ;
#29564 = ORIENTED_EDGE ( 'NONE', *, *, #29791, .T. ) ;
#29565 = CARTESIAN_POINT ( 'NONE',  ( 2.903928887688380645, -7.046356840275715072, -5.221047506680895900 ) ) ;
#29566 = EDGE_CURVE ( 'NONE', #62732, #8336, #13629, .T. ) ;
#29567 = AXIS2_PLACEMENT_3D ( 'NONE', #6770, #47987, #36685 ) ;
#29568 = LINE ( 'NONE', #43554, #63971 ) ;
#29569 = VERTEX_POINT ( 'NONE', #12399 ) ;
#29570 = CARTESIAN_POINT ( 'NONE',  ( -35.05175862995318425, -0.01030783735685159019, 0.007207337213495368378 ) ) ;
#29572 = ORIENTED_EDGE ( 'NONE', *, *, #46490, .T. ) ;
#29571 = VECTOR ( 'NONE', #55656, 1000.000000000000000 ) ;
#29573 = AXIS2_PLACEMENT_3D ( 'NONE', #154, #61003, #20435 ) ;
#29574 = CARTESIAN_POINT ( 'NONE',  ( -35.00000000000000000, -0.01609748574453131326, 11.74614673114904129 ) ) ;
#29575 = CARTESIAN_POINT ( 'NONE',  ( 0.2655924914740778742, 2.083162675473772207, -12.06787830249863092 ) ) ;
#29576 = CARTESIAN_POINT ( 'NONE',  ( 5.121690992581745761, -10.38023541319821241, 6.023682858569486598 ) ) ;
#29577 = ORIENTED_EDGE ( 'NONE', *, *, #8715, .F. ) ;
#29578 = EDGE_LOOP ( 'NONE', ( #44903, #7181, #46161, #62089, #30131, #49655 ) ) ;
#29579 = CIRCLE ( 'NONE', #51917, 5.000000000000000000 ) ;
#29580 = FACE_OUTER_BOUND ( 'NONE', #58568, .T. ) ;
#29581 = ORIENTED_EDGE ( 'NONE', *, *, #8980, .F. ) ;
#29582 = CARTESIAN_POINT ( 'NONE',  ( 10.48620311856346454, 8.250315036047107142, 10.68561190601526611 ) ) ;
#29583 = VERTEX_POINT ( 'NONE', #42011 ) ;
#29584 = ORIENTED_EDGE ( 'NONE', *, *, #7230, .T. ) ;
#29585 = VECTOR ( 'NONE', #53761, 1000.000000000000000 ) ;
#29586 = VERTEX_POINT ( 'NONE', #26734 ) ;
#29587 = DIRECTION ( 'NONE',  ( 0.000000000000000000, 0.01356324068817991828, -0.9999080150203990547 ) ) ;
#29588 = EDGE_CURVE ( 'NONE', #36493, #23316, #51471, .T. ) ;
#29589 = CARTESIAN_POINT ( 'NONE',  ( -37.00000000000000711, 0.000000000000000000, 0.000000000000000000 ) ) ;
#29590 = CARTESIAN_POINT ( 'NONE',  ( -23.41523303002442091, 4.252418708693362248, -1.997501275420724864 ) ) ;
#29591 = CARTESIAN_POINT ( 'NONE',  ( 1.719304012338199517, 0.000000000000000000, 0.000000000000000000 ) ) ;
#29592 = VERTEX_POINT ( 'NONE', #62955 ) ;
#29593 = CARTESIAN_POINT ( 'NONE',  ( -36.00000000000000711, -9.196955404009360180, 8.830544224262913744 ) ) ;
#29594 = ORIENTED_EDGE ( 'NONE', *, *, #4786, .F. ) ;
#29595 = DIRECTION ( 'NONE',  ( -1.000000000000000000, 0.000000000000000000, 0.000000000000000000 ) ) ;
#29596 = DIRECTION ( 'NONE',  ( -1.000000000000000000, 0.000000000000000000, 0.000000000000000000 ) ) ;
#29597 = EDGE_LOOP ( 'NONE', ( #63586, #60879, #26759, #2526 ) ) ;
#29598 = CARTESIAN_POINT ( 'NONE',  ( 1.549075743846936026, 10.12891450359603773, -7.618376504786640524 ) ) ;
#29599 = CARTESIAN_POINT ( 'NONE',  ( 0.3106921474978474040, 3.971572160646753336, 11.60027394202199780 ) ) ;
#29600 = CARTESIAN_POINT ( 'NONE',  ( -37.00000000000000711, 0.000000000000000000, 0.000000000000000000 ) ) ;
#29602 = EDGE_CURVE ( 'NONE', #64793, #27273, #47626, .T. ) ;
#29601 = EDGE_LOOP ( 'NONE', ( #37832, #11805, #14960, #47645 ) ) ;
#29603 = ORIENTED_EDGE ( 'NONE', *, *, #34524, .F. ) ;
#29604 = CARTESIAN_POINT ( 'NONE',  ( 0.3675815128205894289, 6.367184624550164429, 10.50067073900654080 ) ) ;
#29605 = AXIS2_PLACEMENT_3D ( 'NONE', #42031, #58327, #46699 ) ;
#29606 = ORIENTED_EDGE ( 'NONE', *, *, #3241, .T. ) ;
#29607 = CARTESIAN_POINT ( 'NONE',  ( -17.54726996257253191, -12.93490414535027710, 3.865003848717349033 ) ) ;
#29608 = CARTESIAN_POINT ( 'NONE',  ( 1.283627346226359878, 9.985833283678269723, 7.660435136228929132 ) ) ;
#29609 = LINE ( 'NONE', #14966, #40937 ) ;
#29610 = CARTESIAN_POINT ( 'NONE',  ( -3.201686629783078608, 10.71899063123891516, 5.398388898813950121 ) ) ;
#29611 = CARTESIAN_POINT ( 'NONE',  ( 12.72541067165903073, 11.67533756787475241, -2.779695538651842046 ) ) ;
#29612 = ORIENTED_EDGE ( 'NONE', *, *, #41651, .T. ) ;
#29613 = CARTESIAN_POINT ( 'NONE',  ( -35.00000000000000000, 12.05416472667165806, 1.791059740004466994 ) ) ;
#29614 = CARTESIAN_POINT ( 'NONE',  ( 0.7446945582514985507, 1.802628359587814311, 12.27434006248804721 ) ) ;
#29615 = AXIS2_PLACEMENT_3D ( 'NONE', #34861, #9598, #29897 ) ;
#29616 = AXIS2_PLACEMENT_3D ( 'NONE', #38640, #22701, #7376 ) ;
#29617 = EDGE_CURVE ( 'NONE', #21666, #55845, #56110, .T. ) ;
#29618 = CARTESIAN_POINT ( 'NONE',  ( 0.2915757698887312954, -12.10419100255477787, -1.916267336493298501 ) ) ;
#29619 = CARTESIAN_POINT ( 'NONE',  ( 37.00000000000000711, 4.705694406421931860E-17, -3.469127814946512892E-15 ) ) ;
#29620 = EDGE_CURVE ( 'NONE', #14030, #35611, #35919, .T. ) ;
#29621 = CARTESIAN_POINT ( 'NONE',  ( 2.000000000000001776, 0.000000000000000000, 0.000000000000000000 ) ) ;
#29622 = CARTESIAN_POINT ( 'NONE',  ( 1.937114397841935398, 12.76557247858998423, 1.334979369128467042 ) ) ;
#29623 = DIRECTION ( 'NONE',  ( 1.000000000000000000, 0.000000000000000000, 0.000000000000000000 ) ) ;
#29624 = CIRCLE ( 'NONE', #44485, 4.999999999999999112 ) ;
#29625 = B_SPLINE_CURVE_WITH_KNOTS ( 'NONE', 3,
 ( #20423, #35695, #51017, #25744, #20754, #36695, #57654, #11109, #61626, #796 ),
 .UNSPECIFIED., .F., .F.,
 ( 4, 2, 2, 2, 4 ),
 ( 0.005947140490722368188, 0.007059672066379172467, 0.008172203642035975879, 0.009284735217692779291, 0.01039726679334958444 ),
 .UNSPECIFIED. ) ;
#29626 = ADVANCED_FACE ( 'NONE', ( #56686 ), #52453, .F. ) ;
#29627 = ORIENTED_EDGE ( 'NONE', *, *, #24929, .F. ) ;
#29628 = CARTESIAN_POINT ( 'NONE',  ( 37.25000000000000711, -20.00000000000000000, -1.499999999999998002 ) ) ;
#29629 = ORIENTED_EDGE ( 'NONE', *, *, #57360, .T. ) ;
#29630 = CARTESIAN_POINT ( 'NONE',  ( 0.2646305136544065406, -2.256625640822397472, 12.03696649559613796 ) ) ;
#29631 = FACE_OUTER_BOUND ( 'NONE', #38884, .T. ) ;
#29632 = CARTESIAN_POINT ( 'NONE',  ( 36.00000000000000711, -3.805206332242390133, 12.16893194857553340 ) ) ;
#29633 = B_SPLINE_CURVE_WITH_KNOTS ( 'NONE', 3,
 ( #23556, #33191, #6952, #48832, #48504, #37529, #42835, #53152, #2645, #43829, #28213, #12563, #17906, #28525, #18242, #1958 ),
 .UNSPECIFIED., .F., .F.,
 ( 4, 3, 3, 3, 3, 4 ),
 ( 0.000000000000000000, 0.0002176109881720254336, 0.0004352086762394624013, 0.0006528017811446896763, 0.0007615147961451724937, 0.0009453342004947376054 ),
 .UNSPECIFIED. ) ;
#29634 = CARTESIAN_POINT ( 'NONE',  ( 2.251139882114756130, -1.203816215708022552, -7.542197031255136963 ) ) ;
#29635 = ORIENTED_EDGE ( 'NONE', *, *, #22426, .F. ) ;
#29636 = EDGE_CURVE ( 'NONE', #6845, #34249, #26397, .T. ) ;
#29637 = ORIENTED_EDGE ( 'NONE', *, *, #22969, .T. ) ;
#29638 = ORIENTED_EDGE ( 'NONE', *, *, #29507, .T. ) ;
#29639 = CARTESIAN_POINT ( 'NONE',  ( -27.32343372485684796, 3.007804754713644613, 0.1402256980610539494 ) ) ;
#29640 = B_SPLINE_CURVE_WITH_KNOTS ( 'NONE', 3,
 ( #6513, #38657, #17138, #3435, #64245, #18720, #37412, #54289, #26789, #47088, #1544, #12144, #32417 ),
 .UNSPECIFIED., .F., .F.,
 ( 4, 3, 3, 3, 4 ),
 ( 2.737610485525898696E-18, 6.607593386745463275E-05, 0.0001321518677373517020, 0.0001982171734706200737, 0.0002642860854759484460 ),
 .UNSPECIFIED. ) ;
#29642 = CARTESIAN_POINT ( 'NONE',  ( -27.58653843872338385, 9.954257377628556114, -6.707763964583499217 ) ) ;
#29641 = VECTOR ( 'NONE', #57206, 1000.000000000000000 ) ;
#29643 = ORIENTED_EDGE ( 'NONE', *, *, #8356, .T. ) ;
#29644 = CYLINDRICAL_SURFACE ( 'NONE', #14484, 5.000000000000000888 ) ;
#29645 = CARTESIAN_POINT ( 'NONE',  ( 0.2739690278137243973, -9.264642836915884416, 8.012873994335658168 ) ) ;
#29646 = DIRECTION ( 'NONE',  ( 0.000000000000000000, 0.000000000000000000, 1.000000000000000000 ) ) ;
#29647 = ORIENTED_EDGE ( 'NONE', *, *, #21015, .F. ) ;
#29648 = DIRECTION ( 'NONE',  ( 0.000000000000000000, -0.5243256840888443904, -0.8515178078024941977 ) ) ;
#29649 = VECTOR ( 'NONE', #52617, 1000.000000000000114 ) ;
#29650 = CARTESIAN_POINT ( 'NONE',  ( -9.369086346427730305, -29.24458096581343725, -11.21746676167145473 ) ) ;
#29651 = CARTESIAN_POINT ( 'NONE',  ( 37.00000000000000711, -11.73808581813437613, 0.4353888892049613824 ) ) ;
#29653 = ORIENTED_EDGE ( 'NONE', *, *, #56450, .F. ) ;
#29652 = DIRECTION ( 'NONE',  ( 0.000000000000000000, 0.01356324068817998940, -0.9999080150203990547 ) ) ;
#29654 = DIRECTION ( 'NONE',  ( -1.000000000000000000, -1.836970198721029688E-16, 0.000000000000000000 ) ) ;
#29655 = EDGE_LOOP ( 'NONE', ( #58997, #7180, #50833, #60163 ) ) ;
#29656 = CARTESIAN_POINT ( 'NONE',  ( -29.60271627082686052, -3.677907232733526488, -11.42254165076253258 ) ) ;
#29657 = ORIENTED_EDGE ( 'NONE', *, *, #51435, .T. ) ;
#29658 = CARTESIAN_POINT ( 'NONE',  ( -37.00000000000000711, 0.000000000000000000, 0.000000000000000000 ) ) ;
#29659 = CARTESIAN_POINT ( 'NONE',  ( 11.36196501432236872, -11.93139467803644393, -1.301023099206525035 ) ) ;
#29660 = AXIS2_PLACEMENT_3D ( 'NONE', #2927, #37157, #47488 ) ;
#29661 = DIRECTION ( 'NONE',  ( 0.000000000000000000, 0.01356324068817991828, -0.9999080150203990547 ) ) ;
#29662 = CARTESIAN_POINT ( 'NONE',  ( 1.014383007554954474, -6.628652139012841005, -10.59286224865788206 ) ) ;
#29663 = DIRECTION ( 'NONE',  ( 0.000000000000000000, 0.01356324068817992175, -0.9999080150203990547 ) ) ;
#29664 = CARTESIAN_POINT ( 'NONE',  ( 0.000000000000000000, 0.000000000000000000, -12.15774668701806149 ) ) ;
#29665 = CARTESIAN_POINT ( 'NONE',  ( 0.3675815128205912052, 11.62724744438071056, -3.951233083390353062 ) ) ;
#29667 = ORIENTED_EDGE ( 'NONE', *, *, #37664, .T. ) ;
#29666 = CARTESIAN_POINT ( 'NONE',  ( 11.32271610705270426, 13.43847017729220106, -1.294440836893753444 ) ) ;
#29668 = AXIS2_PLACEMENT_3D ( 'NONE', #56823, #26528, #1282 ) ;
#29669 = ORIENTED_EDGE ( 'NONE', *, *, #15882, .F. ) ;
#29670 = CARTESIAN_POINT ( 'NONE',  ( 12.99163133893966915, -13.09490509379091527, -3.288953137075154132 ) ) ;
#29671 = ORIENTED_EDGE ( 'NONE', *, *, #31825, .T. ) ;
#29672 = B_SPLINE_CURVE_WITH_KNOTS ( 'NONE', 3,
 ( #54658, #44625, #64918, #60935, #19397, #10371, #39323, #15372, #39662, #50638, #14054, #3798, #75, #30007, #59962, #14383, #4433, #44313, #15034 ),
 .UNSPECIFIED., .F., .F.,
 ( 4, 3, 3, 3, 3, 3, 4 ),
 ( 1.182973382901717356E-17, 4.457896483014837149E-05, 6.639290541542138609E-05, 8.820687556478841213E-05, 0.0001100173248778912589, 0.0001545671401658127800, 0.0001830328308068567065 ),
 .UNSPECIFIED. ) ;
#29673 = VERTEX_POINT ( 'NONE', #57322 ) ;
#29674 = LINE ( 'NONE', #61261, #15784 ) ;
#29675 = CARTESIAN_POINT ( 'NONE',  ( -37.00000000000000711, -6.307491713049102167, 9.908974237959624176 ) ) ;
#29676 = AXIS2_PLACEMENT_3D ( 'NONE', #36870, #31864, #57167 ) ;
#29677 = CARTESIAN_POINT ( 'NONE',  ( 35.00000000000000000, 11.74614673114903773, 0.01609748574448878478 ) ) ;
#29678 = FACE_OUTER_BOUND ( 'NONE', #59155, .T. ) ;
#29679 = CARTESIAN_POINT ( 'NONE',  ( 17.27839441901508621, 25.00000000000000000, 5.771933972472480967 ) ) ;
#29680 = EDGE_CURVE ( 'NONE', #29997, #44077, #24269, .T. ) ;
#29681 = CARTESIAN_POINT ( 'NONE',  ( 2.266490820341528600, 7.230273269341637388, 2.476945027125681431 ) ) ;
#29682 = DIRECTION ( 'NONE',  ( 1.000000000000000000, 0.000000000000000000, -0.000000000000000000 ) ) ;
#29683 = SHAPE_REPRESENTATION ( 'Inner cradle housing', ( #24966 ), #5855 ) ;
#29684 = ORIENTED_EDGE ( 'NONE', *, *, #53017, .T. ) ;
#29685 = DIRECTION ( 'NONE',  ( -1.000000000000000000, 0.000000000000000000, -0.000000000000000000 ) ) ;
#29686 = DIRECTION ( 'NONE',  ( -1.000000000000000000, -0.000000000000000000, 0.000000000000000000 ) ) ;
#29687 = CARTESIAN_POINT ( 'NONE',  ( 0.2653519991613814688, -7.854838327448906199, -9.395283368383257283 ) ) ;
#29688 = ORIENTED_EDGE ( 'NONE', *, *, #48885, .F. ) ;
#29689 = AXIS2_PLACEMENT_3D ( 'NONE', #59093, #23847, #13197 ) ;
#29690 = EDGE_CURVE ( 'NONE', #47363, #39116, #2351, .T. ) ;
#29691 = CIRCLE ( 'NONE', #47799, 5.000000000000000888 ) ;
#29692 =( BOUNDED_CURVE ( )  B_SPLINE_CURVE ( 3, ( #14701, #54963, #5422, #35657 ),
 .UNSPECIFIED., .F., .F. ) 
 B_SPLINE_CURVE_WITH_KNOTS ( ( 4, 4 ),
 ( 4.298859771126309681, 4.334476141310460662 ),
 .UNSPECIFIED. ) 
 CURVE ( )  GEOMETRIC_REPRESENTATION_ITEM ( )  RATIONAL_B_SPLINE_CURVE ( ( 1.000000000000000000, 0.9998942923082225764, 0.9998942923082225764, 1.000000000000000000 ) ) 
 REPRESENTATION_ITEM ( '' )  );
#29693 = CIRCLE ( 'NONE', #19085, 5.000000000000000888 ) ;
#29694 = CARTESIAN_POINT ( 'NONE',  ( -37.00000000000000711, -5.300372733891723698, 11.59605747147784882 ) ) ;
#29695 = EDGE_CURVE ( 'NONE', #20972, #26426, #41180, .T. ) ;
#29696 = CARTESIAN_POINT ( 'NONE',  ( -22.30625920655495165, 2.110841417170918000, 3.150098859949304941 ) ) ;
#29697 = CARTESIAN_POINT ( 'NONE',  ( -49.84017496522046997, -0.03257330535494378648, -2.852477068595663301 ) ) ;
#29698 = EDGE_CURVE ( 'NONE', #40241, #6864, #44417, .T. ) ;
#29699 = VERTEX_POINT ( 'NONE', #64268 ) ;
#29700 = CARTESIAN_POINT ( 'NONE',  ( 2.276198483117261251, 6.697332984100312636, -3.688810392808482330 ) ) ;
#29701 = CARTESIAN_POINT ( 'NONE',  ( 17.05023968204110929, -34.50000000000000000, 4.356789313881321846 ) ) ;
#29702 = CARTESIAN_POINT ( 'NONE',  ( 3.732195538077428321, 4.611300756578111226, 11.08753034506807822 ) ) ;
#29703 = AXIS2_PLACEMENT_3D ( 'NONE', #64554, #59592, #27120 ) ;
#29704 = EDGE_CURVE ( 'NONE', #26398, #41890, #4110, .T. ) ;
#29705 = DIRECTION ( 'NONE',  ( 0.000000000000000000, -0.01356324068817992175, 0.9999080150203990547 ) ) ;
#29706 = DIRECTION ( 'NONE',  ( 1.000000000000000000, 0.000000000000000000, 0.000000000000000000 ) ) ;
#29707 = AXIS2_PLACEMENT_3D ( 'NONE', #61959, #12620, #32568 ) ;
#29708 = ORIENTED_EDGE ( 'NONE', *, *, #17706, .F. ) ;
#29709 = CARTESIAN_POINT ( 'NONE',  ( 2.259025283528087957, 0.1366755880739711493, 7.639069972920475848 ) ) ;
#29710 = EDGE_CURVE ( 'NONE', #47218, #25348, #58264, .T. ) ;
#29711 = CARTESIAN_POINT ( 'NONE',  ( 0.3401186441510257730, -12.12646044229290254, 1.878666403202292834 ) ) ;
#29712 = CARTESIAN_POINT ( 'NONE',  ( -22.31328051695926007, 3.633840107626944871, -1.076152733467184985 ) ) ;
#29713 = VERTEX_POINT ( 'NONE', #63939 ) ;
#29714 = CARTESIAN_POINT ( 'NONE',  ( 35.00000000000000000, 12.17626345777663488, -0.4993900848167889817 ) ) ;
#29715 = LINE ( 'NONE', #24753, #56368 ) ;
#29716 = EDGE_LOOP ( 'NONE', ( #20921, #55058, #16137, #9338, #55520, #47233 ) ) ;
#29717 = AXIS2_PLACEMENT_3D ( 'NONE', #12253, #32843, #7599 ) ;
#29718 = VERTEX_POINT ( 'NONE', #48665 ) ;
#29719 = ORIENTED_EDGE ( 'NONE', *, *, #35267, .T. ) ;
#29720 = ORIENTED_EDGE ( 'NONE', *, *, #24289, .F. ) ;
#29721 = EDGE_CURVE ( 'NONE', #52971, #30121, #10346, .T. ) ;
#29722 = DIRECTION ( 'NONE',  ( -1.000000000000000000, 0.000000000000000000, 0.000000000000000000 ) ) ;
#29723 = LINE ( 'NONE', #55991, #42068 ) ;
#29724 = DIRECTION ( 'NONE',  ( 1.000000000000000000, 0.000000000000000000, 0.000000000000000000 ) ) ;
#29725 = DIRECTION ( 'NONE',  ( 0.000000000000000000, -0.01356324068817999114, 0.9999080150203989437 ) ) ;
#29727 = EDGE_CURVE ( 'NONE', #30290, #37470, #11544, .T. ) ;
#29726 = CARTESIAN_POINT ( 'NONE',  ( -17.34314652423584491, -28.58740822003687754, 8.955725788651514918 ) ) ;
#29728 = CARTESIAN_POINT ( 'NONE',  ( 5.520433897694421610, 0.01278034823632016002, -0.007971295965052641735 ) ) ;
#29730 = EDGE_LOOP ( 'NONE', ( #27375, #45954, #11038, #9698 ) ) ;
#29729 = CARTESIAN_POINT ( 'NONE',  ( 0.5572780756279074321, 7.697784780878702549, 9.649189244958369827 ) ) ;
#29731 = DIRECTION ( 'NONE',  ( 1.000000000000000000, -0.000000000000000000, 0.000000000000000000 ) ) ;
#29732 = EDGE_LOOP ( 'NONE', ( #1400, #23969, #15512, #62099 ) ) ;
#29733 = DIRECTION ( 'NONE',  ( 0.000000000000000000, 0.000000000000000000, 1.000000000000000000 ) ) ;
#29734 = ORIENTED_EDGE ( 'NONE', *, *, #13744, .F. ) ;
#29735 = ORIENTED_EDGE ( 'NONE', *, *, #61158, .T. ) ;
#29736 = CARTESIAN_POINT ( 'NONE',  ( 0.000000000000000000, -29.00000000000000000, 0.000000000000000000 ) ) ;
#29737 = CARTESIAN_POINT ( 'NONE',  ( 4.958255736529285862, -30.98164499407798189, 14.76282592124280058 ) ) ;
#29738 = CARTESIAN_POINT ( 'NONE',  ( -22.23402523511428086, 1.734723475976807094E-15, -8.673617379884035472E-15 ) ) ;
#29739 = AXIS2_PLACEMENT_3D ( 'NONE', #63171, #27586, #63480 ) ;
#29740 = CIRCLE ( 'NONE', #13825, 12.18650000000000055 ) ;
#29741 = FACE_OUTER_BOUND ( 'NONE', #51304, .T. ) ;
#29742 = DIRECTION ( 'NONE',  ( 1.000000000000000000, 0.000000000000000000, -0.000000000000000000 ) ) ;
#29743 = DIRECTION ( 'NONE',  ( 0.000000000000000000, -0.01356324068817998940, 0.9999080150203990547 ) ) ;
#29744 = ORIENTED_EDGE ( 'NONE', *, *, #50810, .T. ) ;
#29745 = VERTEX_POINT ( 'NONE', #43002 ) ;
#29746 = LINE ( 'NONE', #40379, #10395 ) ;
#29747 = ORIENTED_EDGE ( 'NONE', *, *, #56208, .T. ) ;
#29748 = VERTEX_POINT ( 'NONE', #2462 ) ;
#29749 = CARTESIAN_POINT ( 'NONE',  ( 2.288423627607478306, -7.504187945869063014, 1.486973602181125287 ) ) ;
#29750 = CARTESIAN_POINT ( 'NONE',  ( 3.780834652287974773, 8.352030633203080257, 10.60629927458383115 ) ) ;
#29751 = CARTESIAN_POINT ( 'NONE',  ( 16.78263030916553333, 10.48479066935627202, 5.836879698929882565 ) ) ;
#29752 = CARTESIAN_POINT ( 'NONE',  ( 2.242819959140645913, 7.634209046698939183, 0.1024002568249643141 ) ) ;
#29753 = EDGE_CURVE ( 'NONE', #53931, #9134, #40203, .T. ) ;
#29754 = CARTESIAN_POINT ( 'NONE',  ( 37.00000000000000711, -1.463443770872862482, -12.09831040184923978 ) ) ;
#29755 = DIRECTION ( 'NONE',  ( 1.000000000000000000, -0.000000000000000000, -0.000000000000000000 ) ) ;
#29756 = VECTOR ( 'NONE', #10500, 1000.000000000000114 ) ;
#29757 = ORIENTED_EDGE ( 'NONE', *, *, #54655, .F. ) ;
#29758 = EDGE_LOOP ( 'NONE', ( #39794, #52008, #15824, #44699, #54803, #57576 ) ) ;
#29759 = DIRECTION ( 'NONE',  ( 0.000000000000000000, 0.000000000000000000, 1.000000000000000000 ) ) ;
#29760 = DIRECTION ( 'NONE',  ( -1.000000000000000000, 0.000000000000000000, 0.000000000000000000 ) ) ;
#29761 = EDGE_CURVE ( 'NONE', #65109, #54100, #48728, .T. ) ;
#29762 = AXIS2_PLACEMENT_3D ( 'NONE', #38090, #53069, #7506 ) ;
#29763 = DIRECTION ( 'NONE',  ( 0.000000000000000000, 0.000000000000000000, -1.000000000000000000 ) ) ;
#29764 = CARTESIAN_POINT ( 'NONE',  ( 37.00000000000000711, 4.732539170486261604, -11.23004253107766282 ) ) ;
#29765 = EDGE_CURVE ( 'NONE', #63874, #50124, #62367, .T. ) ;
#29766 = CARTESIAN_POINT ( 'NONE',  ( 0.9232058338315048962, 11.58467545991553926, 4.617996777200612080 ) ) ;
#29767 = AXIS2_PLACEMENT_3D ( 'NONE', #34796, #15193, #65074 ) ;
#29768 = CARTESIAN_POINT ( 'NONE',  ( -4.975205859172452172, -1.416020129149132778, -11.91616074890918675 ) ) ;
#29769 = DIRECTION ( 'NONE',  ( 1.000000000000000000, 0.000000000000000000, 0.000000000000000000 ) ) ;
#29770 = CARTESIAN_POINT ( 'NONE',  ( 28.12931769988050590, 12.24233004620663579, 5.700308019928762349 ) ) ;
#29771 = EDGE_CURVE ( 'NONE', #43286, #52549, #50861, .T. ) ;
#29772 = VERTEX_POINT ( 'NONE', #59289 ) ;
#29773 = CARTESIAN_POINT ( 'NONE',  ( 2.781367136451494471, -6.179587792204012331, -4.783057651000591548 ) ) ;
#29774 = LINE ( 'NONE', #24815, #13043 ) ;
#29775 = FACE_OUTER_BOUND ( 'NONE', #28491, .T. ) ;
#29776 = AXIS2_PLACEMENT_3D ( 'NONE', #622, #20884, #41152 ) ;
#29777 = MECHANICAL_DESIGN_GEOMETRIC_PRESENTATION_REPRESENTATION (  '', ( #18093 ), #14920 ) ;
#29778 = AXIS2_PLACEMENT_3D ( 'NONE', #63824, #53874, #8311 ) ;
#29779 = CARTESIAN_POINT ( 'NONE',  ( -10.63305928498245301, -33.14245637257819510, -11.52579945307858011 ) ) ;
#29780 = CARTESIAN_POINT ( 'NONE',  ( 2.298277635560276089, -5.967558917212167025, 4.791911337974153362 ) ) ;
#29781 = EDGE_LOOP ( 'NONE', ( #1292, #39919, #46221, #10551 ) ) ;
#29782 = CARTESIAN_POINT ( 'NONE',  ( 5.514624014163232779, 0.001921576324372091180, -0.003668383633201698427 ) ) ;
#29783 = CARTESIAN_POINT ( 'NONE',  ( 2.440552418640468346, 6.568204543009822594, 4.020120046181057560 ) ) ;
#29784 = EDGE_CURVE ( 'NONE', #64240, #1294, #50723, .T. ) ;
#29785 = CARTESIAN_POINT ( 'NONE',  ( -5.484316184572717745, -28.21670571277537221, -11.61674069750055160 ) ) ;
#29786 = ORIENTED_EDGE ( 'NONE', *, *, #18915, .T. ) ;
#29787 = CARTESIAN_POINT ( 'NONE',  ( 1.549075743844149367, -6.912427991522798187, 10.62322497417012634 ) ) ;
#29789 = FACE_OUTER_BOUND ( 'NONE', #57831, .T. ) ;
#29788 = B_SPLINE_CURVE_WITH_KNOTS ( 'NONE', 3,
 ( #42762, #53753, #23152, #43415, #47771, #48116, #43094, #7519, #64040, #28459, #37790, #33122, #63694, #12837, #48761, #38101, #18524, #27471, #2223 ),
 .UNSPECIFIED., .F., .F.,
 ( 4, 3, 3, 3, 3, 3, 4 ),
 ( 3.157244383155854313E-18, 2.836829842860746890E-05, 4.224792512343399911E-05, 5.612066614708121319E-05, 6.998859278151859525E-05, 9.832141287888682374E-05, 0.0001178161482480174707 ),
 .UNSPECIFIED. ) ;
#29790 = DIRECTION ( 'NONE',  ( 0.3865475372811020272, -0.8730852074079779035, 0.2971585806051764145 ) ) ;
#29791 = EDGE_CURVE ( 'NONE', #41767, #31515, #44304, .T. ) ;
#29792 = CYLINDRICAL_SURFACE ( 'NONE', #19052, 3.594603870727467676 ) ;
#29793 = DIRECTION ( 'NONE',  ( 0.000000000000000000, 0.7621620551276376831, -0.6473862847818260269 ) ) ;
#29794 = EDGE_CURVE ( 'NONE', #20687, #23822, #43536, .T. ) ;
#29795 = AXIS2_PLACEMENT_3D ( 'NONE', #59610, #9062, #13392 ) ;
#29796 = AXIS2_PLACEMENT_3D ( 'NONE', #57599, #47608, #53599 ) ;
#29797 = CYLINDRICAL_SURFACE ( 'NONE', #33986, 6.936499999999988120 ) ;
#29798 = EDGE_CURVE ( 'NONE', #28152, #46658, #20054, .T. ) ;
#29799 = VERTEX_POINT ( 'NONE', #29996 ) ;
#29801 = EDGE_CURVE ( 'NONE', #38611, #62115, #32407, .T. ) ;
#29800 = VECTOR ( 'NONE', #42719, 1000.000000000000000 ) ;
#29802 = CYLINDRICAL_SURFACE ( 'NONE', #56733, 5.000000000000000888 ) ;
#29803 = CONICAL_SURFACE ( 'NONE', #44657, 7.938172270156617749, 1.280189991382167047 ) ;
#29804 = CARTESIAN_POINT ( 'NONE',  ( -2.822269947909832766, -4.599275498345574142, 11.08601571419041676 ) ) ;
#29805 = CYLINDRICAL_SURFACE ( 'NONE', #36460, 7.499999999999988454 ) ;
#29806 = CARTESIAN_POINT ( 'NONE',  ( 10.48620311856346454, 8.250315036047107142, -10.68561190601526789 ) ) ;
#29807 = DIRECTION ( 'NONE',  ( 0.000000000000000000, 0.000000000000000000, 1.000000000000000000 ) ) ;
#29808 = CIRCLE ( 'NONE', #7669, 5.000000000000001776 ) ;
#29809 = ADVANCED_FACE ( 'NONE', ( #30638 ), #19386, .T. ) ;
#29810 = CARTESIAN_POINT ( 'NONE',  ( -37.00000000000000711, 5.921969905510501064, -10.14408668126206869 ) ) ;
#29811 = CARTESIAN_POINT ( 'NONE',  ( 35.00000000000000000, 1.456211999474505969, 11.65554240571055011 ) ) ;
#29812 = ORIENTED_EDGE ( 'NONE', *, *, #39993, .T. ) ;
#29813 = VERTEX_POINT ( 'NONE', #50948 ) ;
#29814 = LINE ( 'NONE', #30474, #3462 ) ;
#29815 = CONICAL_SURFACE ( 'NONE', #50011, 7.938172270156617749, 1.280189991382167047 ) ;
#29816 = ORIENTED_EDGE ( 'NONE', *, *, #35415, .T. ) ;
#29817 = CARTESIAN_POINT ( 'NONE',  ( 0.2911222467163511740, 11.44063169461055374, 4.392242282524896346 ) ) ;
#29818 = DIRECTION ( 'NONE',  ( 0.000000000000000000, 0.01356324068817998940, -0.9999080150203990547 ) ) ;
#29819 = ORIENTED_EDGE ( 'NONE', *, *, #42398, .T. ) ;
#29821 = DIRECTION ( 'NONE',  ( 0.000000000000000000, 0.000000000000000000, -1.000000000000000000 ) ) ;
#29820 = AXIS2_PLACEMENT_3D ( 'NONE', #30000, #50312, #26323 ) ;
#29822 = CARTESIAN_POINT ( 'NONE',  ( -27.25047371082987269, -12.34411773464382200, 5.468532507261036457 ) ) ;
#29823 = DIRECTION ( 'NONE',  ( 1.000000000000000000, -0.000000000000000000, 0.000000000000000000 ) ) ;
#29824 = ORIENTED_EDGE ( 'NONE', *, *, #9083, .F. ) ;
#29825 = ORIENTED_EDGE ( 'NONE', *, *, #34661, .T. ) ;
#29826 = CARTESIAN_POINT ( 'NONE',  ( 3.100650473569752208, 0.4517506188709136117, -7.907988569972083326 ) ) ;
#29827 = VERTEX_POINT ( 'NONE', #34645 ) ;
#29828 = ORIENTED_EDGE ( 'NONE', *, *, #10334, .F. ) ;
#29829 = DIRECTION ( 'NONE',  ( -1.000000000000000000, 0.000000000000000000, 0.000000000000000000 ) ) ;
#29830 = CARTESIAN_POINT ( 'NONE',  ( -27.10719052120871098, 1.044362304621487825, -2.116547233941206585 ) ) ;
#29831 = CIRCLE ( 'NONE', #30878, 6.936499999999988120 ) ;
#29832 = ADVANCED_FACE ( 'NONE', ( #35303 ), #50308, .T. ) ;
#29833 = CIRCLE ( 'NONE', #23493, 12.18649999999999878 ) ;
#29834 = CARTESIAN_POINT ( 'NONE',  ( 2.770579946183326925, -4.165025702425888099, 6.607710183380618219 ) ) ;
#29835 = CARTESIAN_POINT ( 'NONE',  ( 35.00000000000000000, -2.346765782874354667, 11.95840593935203522 ) ) ;
#29836 = VECTOR ( 'NONE', #60398, 1000.000000000000000 ) ;
#29837 = DIRECTION ( 'NONE',  ( 1.000000000000000000, -0.000000000000000000, -0.000000000000000000 ) ) ;
#29838 = ORIENTED_EDGE ( 'NONE', *, *, #22089, .T. ) ;
#29839 = CARTESIAN_POINT ( 'NONE',  ( 2.284126774967663032, -1.483972655035265653, 7.503320429541877168 ) ) ;
#29840 = AXIS2_PLACEMENT_3D ( 'NONE', #8115, #28708, #33699 ) ;
#29841 = DIRECTION ( 'NONE',  ( 0.000000000000000000, -0.01356324068817991828, 0.9999080150203990547 ) ) ;
#29842 = CARTESIAN_POINT ( 'NONE',  ( 36.00000000000000711, -12.74068829017554094, -0.4871980014161073624 ) ) ;
#29843 = CARTESIAN_POINT ( 'NONE',  ( 2.241506898688418570, 5.873558213059478561, 4.877157973186999840 ) ) ;
#29844 = CARTESIAN_POINT ( 'NONE',  ( 2.000000000000001776, -5.860254403322002759, -3.474373880649873403 ) ) ;
#29845 = CARTESIAN_POINT ( 'NONE',  ( -27.10719052120871098, 1.622102031466687189, -1.714424047991080613 ) ) ;
#29846 = CYLINDRICAL_SURFACE ( 'NONE', #18162, 4.945031439545089391 ) ;
#29847 = CARTESIAN_POINT ( 'NONE',  ( 0.000000000000000000, 0.2704997240206042930, -6.931223712253475000 ) ) ;
#29848 = EDGE_CURVE ( 'NONE', #14064, #55770, #25669, .T. ) ;
#29849 = DIRECTION ( 'NONE',  ( 1.000000000000000000, 0.000000000000000000, 0.000000000000000000 ) ) ;
#29850 = AXIS2_PLACEMENT_3D ( 'NONE', #18736, #64570, #38990 ) ;
#29851 = AXIS2_PLACEMENT_3D ( 'NONE', #1100, #37657, #51976 ) ;
#29852 = ORIENTED_EDGE ( 'NONE', *, *, #46864, .T. ) ;
#29853 = CARTESIAN_POINT ( 'NONE',  ( -16.48910027788405586, 8.233971230660170448, -8.729683764212291308 ) ) ;
#29854 = AXIS2_PLACEMENT_3D ( 'NONE', #12356, #32623, #52934 ) ;
#29855 = AXIS2_PLACEMENT_3D ( 'NONE', #37022, #37356, #57667 ) ;
#29856 = ORIENTED_EDGE ( 'NONE', *, *, #28570, .T. ) ;
#29857 = CARTESIAN_POINT ( 'NONE',  ( -3.215522858303206721, -10.71731889880403976, 5.411963614777410392 ) ) ;
#29858 = CARTESIAN_POINT ( 'NONE',  ( -22.27706485742869091, -3.662257305743835012, 0.3729136217356029959 ) ) ;
#29859 = LINE ( 'NONE', #55472, #26093 ) ;
#29860 = CIRCLE ( 'NONE', #10734, 6.936499999999989008 ) ;
#29861 = CARTESIAN_POINT ( 'NONE',  ( -35.00000000000000000, -9.677500615117949678, 6.657191900728284928 ) ) ;
#29862 = EDGE_CURVE ( 'NONE', #5232, #50756, #19904, .T. ) ;
#29863 = ORIENTED_EDGE ( 'NONE', *, *, #4611, .T. ) ;
#29864 = CARTESIAN_POINT ( 'NONE',  ( -11.40165637462999904, -7.731494526685026791, -11.07003512086042463 ) ) ;
#29866 = VECTOR ( 'NONE', #27158, 1000.000000000000000 ) ;
#29865 = CARTESIAN_POINT ( 'NONE',  ( 2.256373768223412846, -3.703993494727557234, 6.681391662621571470 ) ) ;
#29867 = CARTESIAN_POINT ( 'NONE',  ( 12.03384061974589514, 0.5718066298479855813, 11.98657780702208342 ) ) ;
#29868 = CARTESIAN_POINT ( 'NONE',  ( 1.547277799337862803, 2.861188171558548543, 12.34637640861301300 ) ) ;
#29869 = EDGE_CURVE ( 'NONE', #18739, #5409, #64166, .T. ) ;
#29870 = VECTOR ( 'NONE', #25938, 999.9999999999997726 ) ;
#29871 = CYLINDRICAL_SURFACE ( 'NONE', #60547, 2.899999999999994582 ) ;
#29872 = ORIENTED_EDGE ( 'NONE', *, *, #37043, .F. ) ;
#29873 = CARTESIAN_POINT ( 'NONE',  ( -10.48620311856347875, -9.720786832536937538, 7.036071585506805448 ) ) ;
#29874 = VECTOR ( 'NONE', #33990, 1000.000000000000000 ) ;
#29875 = ORIENTED_EDGE ( 'NONE', *, *, #46482, .T. ) ;
#29876 = CIRCLE ( 'NONE', #63868, 5.000000000000000888 ) ;
#29877 = CARTESIAN_POINT ( 'NONE',  ( 0.2958664285830431839, -0.2205161970873538990, -12.25438626999990355 ) ) ;
#29878 = CARTESIAN_POINT ( 'NONE',  ( 2.000000000000001776, 0.000000000000000000, 0.000000000000000000 ) ) ;
#29879 = CARTESIAN_POINT ( 'NONE',  ( -2.952869152607111136, -7.581333670610126418, 11.17020052527586138 ) ) ;
#29880 = FACE_OUTER_BOUND ( 'NONE', #37291, .T. ) ;
#29881 = EDGE_CURVE ( 'NONE', #22893, #47422, #60255, .T. ) ;
#29882 = CIRCLE ( 'NONE', #45801, 12.74999999999999822 ) ;
#29883 = AXIS2_PLACEMENT_3D ( 'NONE', #62466, #47215, #17603 ) ;
#29884 = VECTOR ( 'NONE', #24007, 1000.000000000000000 ) ;
#29885 = ORIENTED_EDGE ( 'NONE', *, *, #17879, .T. ) ;
#29886 = VERTEX_POINT ( 'NONE', #15362 ) ;
#29887 = DIRECTION ( 'NONE',  ( 0.000000000000000000, -0.2149704402110114709, -0.9766205557100894330 ) ) ;
#29888 = EDGE_CURVE ( 'NONE', #36819, #24391, #28543, .T. ) ;
#29889 = EDGE_LOOP ( 'NONE', ( #13220, #8668, #58970, #21252 ) ) ;
#29890 = CARTESIAN_POINT ( 'NONE',  ( 2.305787727787083519, -6.545285700970500109, -3.971363876084033961 ) ) ;
#29892 = CARTESIAN_POINT ( 'NONE',  ( 6.361445718264521432, -4.355102044641763648, -11.18181944858513077 ) ) ;
#29891 =( BOUNDED_SURFACE ( )  B_SPLINE_SURFACE ( 3, 2, ( 
 ( #31833, #23185, #57135 ),
 ( #11561, #1923, #37152 ),
 ( #47483, #12529, #37493 ),
 ( #52148, #6597, #57462 ),
 ( #11885, #38135, #32162 ),
 ( #12219, #53118, #52486 ),
 ( #32809, #32486, #27848 ),
 ( #6920, #22193, #42451 ),
 ( #2611, #52792, #7221 ),
 ( #2259, #22538, #42802 ),
 ( #63092, #43125, #63403 ),
 ( #58444, #12875, #33154 ),
 ( #8220, #19518, #34125 ),
 ( #54099, #28826, #3902 ),
 ( #9186, #39783, #59745 ),
 ( #29464, #54768, #38809 ),
 ( #64075, #65041, #23860 ),
 ( #39119, #63727, #49463 ),
 ( #55071, #29785, #8537 ),
 ( #59108, #49766, #64704 ),
 ( #58793, #23520, #18855 ),
 ( #18207, #49135, #13211 ),
 ( #13517, #43448, #19173 ),
 ( #33496, #9500, #38475 ),
 ( #4557, #3594, #28490 ),
 ( #44120, #60072, #39445 ),
 ( #14491, #24482, #4212 ),
 ( #43795, #59410, #33799 ),
 ( #50101, #53786, #48797 ),
 ( #3248, #18557, #44760 ),
 ( #64387, #13833, #54443 ),
 ( #8875, #44422, #29167 ),
 ( #24159, #34766, #14175 ),
 ( #34465, #26135, #856 ),
 ( #46412, #45415, #9843 ),
 ( #45107, #55743, #60385 ),
 ( #40423, #24826, #46102 ),
 ( #14809, #56744, #65369 ),
 ( #51743, #30453, #55404 ),
 ( #50750, #21126, #548 ),
 ( #41400, #5878, #10831 ),
 ( #19834, #20488, #40093 ),
 ( #35094, #30136, #50435 ),
 ( #4880, #40773, #60724 ),
 ( #25807, #25146, #45751 ),
 ( #10173, #20812, #35443 ),
 ( #65682, #31115, #5199 ),
 ( #56048, #25467, #41080 ),
 ( #61358, #20152, #15157 ),
 ( #215, #10490, #5542 ) ),
 .UNSPECIFIED., .F., .F., .F. ) 
 B_SPLINE_SURFACE_WITH_KNOTS ( ( 4, 2, 2, 2, 2, 2, 2, 2, 2, 2, 2, 2, 2, 2, 2, 2, 2, 2, 2, 2, 2, 2, 2, 2, 4 ),
 ( 3, 3 ),
 ( 0.06047842900482980344, 0.06367705432712369995, 0.06527636698827063433, 0.06687567964941758258, 0.06847499231056453084, 0.07007430497171146522, 0.07327293029400536173, 0.07647155561629924436, 0.07807086827744619262, 0.07967018093859312700, 0.08286880626088702351, 0.08446811892203395788, 0.08606743158318090614, 0.08926605690547478877, 0.09086536956662173703, 0.09246468222776868529, 0.09566330755006256792, 0.09726262021120951617, 0.09886193287235645055, 0.1020605581946503471, 0.1052591835169442297, 0.1068584961780911780, 0.1084578088392381123, 0.1100571215003850606, 0.1116564341615320088 ),
 ( 0.000000000000000000, 1.000000000000000000 ),
 .UNSPECIFIED. ) 
 GEOMETRIC_REPRESENTATION_ITEM ( )  RATIONAL_B_SPLINE_SURFACE ( (
 ( 1.000000000000000000, 0.4999999999999997224, 1.000000000000000000),
 ( 1.000000000000000000, 0.5048840838053595403, 1.000000000000000000),
 ( 1.000000000000000000, 0.5132072642500212778, 1.000000000000000000),
 ( 1.000000000000000000, 0.5290214861663710133, 1.000000000000000000),
 ( 1.000000000000000000, 0.5348648783786191796, 1.000000000000000000),
 ( 1.000000000000000000, 0.5473516051742142174, 1.000000000000000000),
 ( 1.000000000000000000, 0.5539126387906654347, 1.000000000000000000),
 ( 1.000000000000000000, 0.5674101295481297491, 1.000000000000000000),
 ( 1.000000000000000000, 0.5743474342084209372, 1.000000000000000000),
 ( 1.000000000000000000, 0.5883951384281623787, 1.000000000000000000),
 ( 1.000000000000000000, 0.5955302209472954633, 1.000000000000000000),
 ( 1.000000000000000000, 0.6167715304224314909, 1.000000000000000000),
 ( 1.000000000000000000, 0.6305661306848800995, 1.000000000000000000),
 ( 1.000000000000000000, 0.6565125894471021128, 1.000000000000000000),
 ( 1.000000000000000000, 0.6686743926052455267, 1.000000000000000000),
 ( 1.000000000000000000, 0.6851014456086111926, 1.000000000000000000),
 ( 1.000000000000000000, 0.6902475665164108376, 1.000000000000000000),
 ( 1.000000000000000000, 0.6997062435423183624, 1.000000000000000000),
 ( 1.000000000000000000, 0.7040363771866963161, 1.000000000000000000),
 ( 1.000000000000000000, 0.7157418617803246175, 1.000000000000000000),
 ( 1.000000000000000000, 0.7218341033858746147, 1.000000000000000000),
 ( 1.000000000000000000, 0.7280280015706425134, 1.000000000000000000),
 ( 1.000000000000000000, 0.7296036051598833172, 1.000000000000000000),
 ( 1.000000000000000000, 0.7316818214130011988, 1.000000000000000000),
 ( 1.000000000000000000, 0.7321927565543977501, 1.000000000000000000),
 ( 1.000000000000000000, 0.7321641879724063440, 1.000000000000000000),
 ( 1.000000000000000000, 0.7300624469251318915, 1.000000000000000000),
 ( 1.000000000000000000, 0.7238943330024291134, 1.000000000000000000),
 ( 1.000000000000000000, 0.7213359435419269827, 1.000000000000000000),
 ( 1.000000000000000000, 0.7152343487864535332, 1.000000000000000000),
 ( 1.000000000000000000, 0.7117056589943943079, 1.000000000000000000),
 ( 1.000000000000000000, 0.6999072021060611659, 1.000000000000000000),
 ( 1.000000000000000000, 0.6903911339383190793, 1.000000000000000000),
 ( 1.000000000000000000, 0.6741089150890113846, 1.000000000000000000),
 ( 1.000000000000000000, 0.6683461163769177649, 1.000000000000000000),
 ( 1.000000000000000000, 0.6562237482356456653, 1.000000000000000000),
 ( 1.000000000000000000, 0.6498375142660577364, 1.000000000000000000),
 ( 1.000000000000000000, 0.6302143011362419944, 1.000000000000000000),
 ( 1.000000000000000000, 0.6164540672887564021, 1.000000000000000000),
 ( 1.000000000000000000, 0.5885848209491307825, 1.000000000000000000),
 ( 1.000000000000000000, 0.5744580946949390254, 1.000000000000000000),
 ( 1.000000000000000000, 0.5540565490002423710, 1.000000000000000000),
 ( 1.000000000000000000, 0.5474350731751366217, 1.000000000000000000),
 ( 1.000000000000000000, 0.5350293539660311293, 1.000000000000000000),
 ( 1.000000000000000000, 0.5292092555093077522, 1.000000000000000000),
 ( 1.000000000000000000, 0.5186171472262492976, 1.000000000000000000),
 ( 1.000000000000000000, 0.5138445523878416576, 1.000000000000000000),
 ( 1.000000000000000000, 0.5056909436241932010, 1.000000000000000000),
 ( 1.000000000000000000, 0.5023956439952826925, 1.000000000000000000),
 ( 1.000000000000000000, 0.4999999999999995004, 1.000000000000000000) ) ) 
 REPRESENTATION_ITEM ( '' )  SURFACE ( )  );
#29893 = CARTESIAN_POINT ( 'NONE',  ( -22.27719412087655471, -3.421752300520421120, -1.358750377066208825 ) ) ;
#29894 = DIRECTION ( 'NONE',  ( 0.000000000000000000, 0.01356324068817992175, -0.9999080150203990547 ) ) ;
#29895 = CARTESIAN_POINT ( 'NONE',  ( 2.491965175174665426, 6.575382551509702189, -4.041154086925421218 ) ) ;
#29896 = EDGE_CURVE ( 'NONE', #1348, #62894, #8228, .T. ) ;
#29897 = DIRECTION ( 'NONE',  ( 0.000000000000000000, -0.5767582926625032247, -0.8169148498130232028 ) ) ;
#29898 = CARTESIAN_POINT ( 'NONE',  ( -4.989057617119011745, -0.9162120371760335003, 25.00000000000000000 ) ) ;
#29899 = ORIENTED_EDGE ( 'NONE', *, *, #49428, .T. ) ;
#29901 = VERTEX_POINT ( 'NONE', #26988 ) ;
#29900 = CARTESIAN_POINT ( 'NONE',  ( 0.3106921474978485143, -12.03191800497307007, -2.360654586927916743 ) ) ;
#29902 = ORIENTED_EDGE ( 'NONE', *, *, #30978, .F. ) ;
#29903 = DIRECTION ( 'NONE',  ( -1.000000000000000000, -0.000000000000000000, 0.000000000000000000 ) ) ;
#29904 = AXIS2_PLACEMENT_3D ( 'NONE', #21158, #21507, #15511 ) ;
#29905 = AXIS2_PLACEMENT_3D ( 'NONE', #31208, #56826, #5959 ) ;
#29906 = CARTESIAN_POINT ( 'NONE',  ( 2.034671305879535375, 10.44529075078724922, -5.218565780489550221 ) ) ;
#29908 = ADVANCED_FACE ( 'NONE', ( #36631 ), #46603, .T. ) ;
#29907 = ORIENTED_EDGE ( 'NONE', *, *, #12297, .T. ) ;
#29909 = AXIS2_PLACEMENT_3D ( 'NONE', #6830, #21800, #46719 ) ;
#29910 = CARTESIAN_POINT ( 'NONE',  ( -21.17861794710831091, 25.00000000000000000, -3.604945070120774808 ) ) ;
#29911 = ORIENTED_EDGE ( 'NONE', *, *, #65740, .T. ) ;
#29912 = CARTESIAN_POINT ( 'NONE',  ( 2.903928887688958849, 8.712847781147546655, 0.9983813550129092551 ) ) ;
#29913 = CARTESIAN_POINT ( 'NONE',  ( 4.044423495238602229, -10.40360026321140907, -8.606342947645041264 ) ) ;
#29914 = DIRECTION ( 'NONE',  ( 0.000000000000000000, 0.01356324068817991828, -0.9999080150203990547 ) ) ;
#29915 = CARTESIAN_POINT ( 'NONE',  ( 6.987255982139510380, -8.045048366716516242, 8.915354129207686995 ) ) ;
#29916 = ORIENTED_EDGE ( 'NONE', *, *, #59472, .F. ) ;
#29917 = CIRCLE ( 'NONE', #13959, 12.18650000000000055 ) ;
#29918 = ORIENTED_EDGE ( 'NONE', *, *, #3796, .T. ) ;
#29919 = CARTESIAN_POINT ( 'NONE',  ( 2.639814597422734721, -6.851176153958504322, 3.659458430304324494 ) ) ;
#29920 = VERTEX_POINT ( 'NONE', #56246 ) ;
#29921 = CARTESIAN_POINT ( 'NONE',  ( 10.48620311856346454, 8.250315036047107142, 25.00000000000000000 ) ) ;
#29922 = EDGE_LOOP ( 'NONE', ( #53729, #51578, #11300, #49337 ) ) ;
#29923 = AXIS2_PLACEMENT_3D ( 'NONE', #38360, #33040, #32384 ) ;
#29924 = VERTEX_POINT ( 'NONE', #62533 ) ;
#29925 = VERTEX_POINT ( 'NONE', #56935 ) ;
#29926 = CYLINDRICAL_SURFACE ( 'NONE', #41494, 6.936499999999988120 ) ;
#29927 = CARTESIAN_POINT ( 'NONE',  ( 3.967932057708484894, -25.89885127696171097, 15.40358068932206237 ) ) ;
#29928 = DIRECTION ( 'NONE',  ( -1.000000000000000000, 0.000000000000000000, 0.000000000000000000 ) ) ;
#29929 = DIRECTION ( 'NONE',  ( 0.000000000000000000, 0.9651210252299785575, 0.2618041379715665973 ) ) ;
#29930 = ORIENTED_EDGE ( 'NONE', *, *, #5380, .T. ) ;
#29931 = DIRECTION ( 'NONE',  ( 1.000000000000000000, 0.000000000000000000, 0.000000000000000000 ) ) ;
#29932 = AXIS2_PLACEMENT_3D ( 'NONE', #56877, #51232, #46881 ) ;
#29933 = EDGE_CURVE ( 'NONE', #22075, #12068, #57246, .T. ) ;
#29934 = ORIENTED_EDGE ( 'NONE', *, *, #57601, .T. ) ;
#29935 = LINE ( 'NONE', #5011, #44424 ) ;
#29936 = CARTESIAN_POINT ( 'NONE',  ( 2.000000000000001776, -1.145812388885072863, -6.715725538143620277 ) ) ;
#29937 = EDGE_LOOP ( 'NONE', ( #62686, #58836, #30958, #28414 ) ) ;
#29938 = CARTESIAN_POINT ( 'NONE',  ( 2.941278708680199916, 5.721889327162151595, 2.226055275041809889 ) ) ;
#29939 = CARTESIAN_POINT ( 'NONE',  ( 2.247112776671464029, -6.670755883245737650, -3.716786765232512835 ) ) ;
#29940 = EDGE_CURVE ( 'NONE', #49481, #18779, #16672, .T. ) ;
#29941 = AXIS2_PLACEMENT_3D ( 'NONE', #40560, #55865, #20929 ) ;
#29942 = AXIS2_PLACEMENT_3D ( 'NONE', #16715, #36990, #57294 ) ;
#29943 = VERTEX_POINT ( 'NONE', #5741 ) ;
#29944 = CARTESIAN_POINT ( 'NONE',  ( 0.3675815128205912052, -10.50067073900647330, -6.367184624550275451 ) ) ;
#29945 = ORIENTED_EDGE ( 'NONE', *, *, #43117, .F. ) ;
#29946 = CARTESIAN_POINT ( 'NONE',  ( 0.2958664285830431839, 10.72286791615088752, 5.936220506376270301 ) ) ;
#29947 = DIRECTION ( 'NONE',  ( 0.000000000000000000, -0.01356324068817998940, 0.9999080150203989437 ) ) ;
#29948 = CYLINDRICAL_SURFACE ( 'NONE', #4839, 12.75000000000000178 ) ;
#29949 = LINE ( 'NONE', #5351, #22413 ) ;
#29950 = ADVANCED_FACE ( 'NONE', ( #51291 ), #47593, .T. ) ;
#29951 = EDGE_CURVE ( 'NONE', #51562, #56931, #65539, .T. ) ;
#29952 = ORIENTED_EDGE ( 'NONE', *, *, #49376, .T. ) ;
#29953 = DIRECTION ( 'NONE',  ( 1.000000000000000000, 0.000000000000000000, 0.000000000000000000 ) ) ;
#29954 = CARTESIAN_POINT ( 'NONE',  ( 1.459561108994217316, 5.767168887068948813, -11.25243317554941136 ) ) ;
#29955 = CARTESIAN_POINT ( 'NONE',  ( 35.00000000000000000, 4.705694406421931860E-17, -3.469127814946512892E-15 ) ) ;
#29956 = CARTESIAN_POINT ( 'NONE',  ( -30.16311648624135344, -2.210271246884226937, 13.32375839521249361 ) ) ;
#29957 = AXIS2_PLACEMENT_3D ( 'NONE', #12899, #7588, #22896 ) ;
#29958 = EDGE_CURVE ( 'NONE', #8982, #17169, #732, .T. ) ;
#29959 = VECTOR ( 'NONE', #45588, 1000.000000000000000 ) ;
#29960 = AXIS2_PLACEMENT_3D ( 'NONE', #51974, #31991, #6751 ) ;
#29961 = CARTESIAN_POINT ( 'NONE',  ( -18.85528480568559928, -29.92804508438502253, -6.903306693652388581 ) ) ;
#29962 = VECTOR ( 'NONE', #31622, 1000.000000000000000 ) ;
#29963 = CARTESIAN_POINT ( 'NONE',  ( -35.04660725145885891, -0.01223081933017596858, 0.001288602543471934793 ) ) ;
#29964 = CARTESIAN_POINT ( 'NONE',  ( 2.247112776671464918, -5.923998863713016760, -4.818685025480720974 ) ) ;
#29965 = CARTESIAN_POINT ( 'NONE',  ( 37.00000000000000711, -8.352657516904727686, -8.258652103341406203 ) ) ;
#29966 = CYLINDRICAL_SURFACE ( 'NONE', #8867, 5.000000000000000888 ) ;
#29967 = EDGE_CURVE ( 'NONE', #35715, #37190, #31949, .T. ) ;
#29968 = VERTEX_POINT ( 'NONE', #35943 ) ;
#29969 = CARTESIAN_POINT ( 'NONE',  ( 11.39226460963361376, -11.84307025323660234, -1.956600849590324875 ) ) ;
#29970 = VECTOR ( 'NONE', #11531, 1000.000000000000000 ) ;
#29971 = ORIENTED_EDGE ( 'NONE', *, *, #58640, .T. ) ;
#29972 = DIRECTION ( 'NONE',  ( 1.000000000000000000, 0.000000000000000000, -0.000000000000000000 ) ) ;
#29973 = FACE_OUTER_BOUND ( 'NONE', #59452, .T. ) ;
#29974 = CARTESIAN_POINT ( 'NONE',  ( 3.047904605210390638, -7.561255571389383867, 2.299870214474525110 ) ) ;
#29975 = DIRECTION ( 'NONE',  ( 0.000000000000000000, 0.5472293298355273006, -0.8369827122275342868 ) ) ;
#29976 = EDGE_LOOP ( 'NONE', ( #36042, #61507, #16069, #5942 ) ) ;
#29977 = AXIS2_PLACEMENT_3D ( 'NONE', #42909, #57904, #33265 ) ;
#29978 = ORIENTED_EDGE ( 'NONE', *, *, #63955, .T. ) ;
#29979 = ORIENTED_EDGE ( 'NONE', *, *, #61519, .T. ) ;
#29980 = CARTESIAN_POINT ( 'NONE',  ( 29.00864072608240463, -10.24877626319949186, 6.246278040546365595 ) ) ;
#29981 = CIRCLE ( 'NONE', #56540, 12.75000000000000178 ) ;
#29983 = AXIS2_PLACEMENT_3D ( 'NONE', #49935, #4394, #55243 ) ;
#29982 = CARTESIAN_POINT ( 'NONE',  ( 2.717984159219838158, 3.648459810929824521, -6.886544461123881966 ) ) ;
#29984 = ORIENTED_EDGE ( 'NONE', *, *, #44910, .T. ) ;
#29985 = CARTESIAN_POINT ( 'NONE',  ( 37.00000000000000711, -3.805206332242389244, 12.16893194857553340 ) ) ;
#29986 = CARTESIAN_POINT ( 'NONE',  ( 36.00000000000000711, -0.9416912585475287756, -12.71517666308947625 ) ) ;
#29987 = CARTESIAN_POINT ( 'NONE',  ( -37.00000000000000711, -2.627174906296831480, -11.44858830469743083 ) ) ;
#29988 = VERTEX_POINT ( 'NONE', #51617 ) ;
#29989 = DIRECTION ( 'NONE',  ( 0.000000000000000000, 0.000000000000000000, -1.000000000000000000 ) ) ;
#29990 = CARTESIAN_POINT ( 'NONE',  ( -11.13200843151506092, -27.92871652161695550, -13.87829993151233055 ) ) ;
#29991 = CARTESIAN_POINT ( 'NONE',  ( 2.305787727787084407, -6.711944854845797614, -3.682701754025583085 ) ) ;
#29993 = ORIENTED_EDGE ( 'NONE', *, *, #48499, .F. ) ;
#29992 = CARTESIAN_POINT ( 'NONE',  ( 36.00000000000000711, 1.738225594540170782, 12.63095688309027054 ) ) ;
#29994 = DIRECTION ( 'NONE',  ( 1.000000000000000000, -0.000000000000000000, -0.000000000000000000 ) ) ;
#29995 = ORIENTED_EDGE ( 'NONE', *, *, #28382, .F. ) ;
#29996 = CARTESIAN_POINT ( 'NONE',  ( -35.00000000000000000, 12.68495603654571902, 1.286231064351356368 ) ) ;
#29997 = VERTEX_POINT ( 'NONE', #6063 ) ;
#29998 = CARTESIAN_POINT ( 'NONE',  ( -29.68541646480313645, -1.416020129149148543, -11.91616074890925780 ) ) ;
#29999 = CARTESIAN_POINT ( 'NONE',  ( 13.31887391767931206, -10.25789760254341765, -6.242720968652719193 ) ) ;
#30000 = CARTESIAN_POINT ( 'NONE',  ( 35.00000000000000000, 4.705694406421931860E-17, -3.469127814946512892E-15 ) ) ;
#30001 = CARTESIAN_POINT ( 'NONE',  ( -10.00000000000000178, 0.000000000000000000, 0.000000000000000000 ) ) ;
#30002 = CIRCLE ( 'NONE', #34277, 5.000000000000001776 ) ;
#30003 = CARTESIAN_POINT ( 'NONE',  ( -22.27721688985630522, 0.6032462375556890688, 3.631967556481303649 ) ) ;
#30004 = CARTESIAN_POINT ( 'NONE',  ( 0.2767916011545408228, -12.24854187541374095, 0.1897947303542399933 ) ) ;
#30005 = CARTESIAN_POINT ( 'NONE',  ( 5.514970785353741078, -0.001117786416802142449, 0.004588761610584822515 ) ) ;
#30006 = CARTESIAN_POINT ( 'NONE',  ( 37.00000000000000711, -3.033604067594489528, 12.38385022362084698 ) ) ;
#30007 = CARTESIAN_POINT ( 'NONE',  ( 0.2759803524722196366, -4.011137970318874757, -11.57441428600636968 ) ) ;
#30009 = VERTEX_POINT ( 'NONE', #16002 ) ;
#30008 = CARTESIAN_POINT ( 'NONE',  ( 9.906964480792026961, 13.48511810156870006, -0.6357016161040081048 ) ) ;
#30010 = CARTESIAN_POINT ( 'NONE',  ( 3.152665057734040488, 0.000000000000000000, 0.000000000000000000 ) ) ;
#30011 = EDGE_CURVE ( 'NONE', #6270, #49268, #21287, .T. ) ;
#30012 = VECTOR ( 'NONE', #20260, 1000.000000000000000 ) ;
#30013 = ORIENTED_EDGE ( 'NONE', *, *, #13744, .T. ) ;
#30014 = CARTESIAN_POINT ( 'NONE',  ( 12.97755741834660981, -11.38317177042858042, -7.268834546894593629 ) ) ;
#30015 = ORIENTED_EDGE ( 'NONE', *, *, #31015, .F. ) ;
#30016 = CIRCLE ( 'NONE', #9828, 12.75000000000000178 ) ;
#30017 = EDGE_LOOP ( 'NONE', ( #22576, #40460, #21112, #34993 ) ) ;
#30018 = DIRECTION ( 'NONE',  ( 0.000000000000000000, -0.01356324068818000328, 0.9999080150203990547 ) ) ;
#30019 = DIRECTION ( 'NONE',  ( 1.000000000000000000, 0.000000000000000000, 0.000000000000000000 ) ) ;
#30020 = DIRECTION ( 'NONE',  ( 1.000000000000000000, 0.000000000000000000, 0.000000000000000000 ) ) ;
#30021 = DIRECTION ( 'NONE',  ( 0.000000000000000000, 0.01356324068817998940, -0.9999080150203990547 ) ) ;
#30022 = CARTESIAN_POINT ( 'NONE',  ( 37.00000000000000711, -8.389074212634222150, 8.839356091080130540 ) ) ;
#30023 = ADVANCED_FACE ( 'NONE', ( #61554 ), #36289, .T. ) ;
#30024 = CARTESIAN_POINT ( 'NONE',  ( 2.000000000000001776, 5.585096664091999230, -4.113602740025892324 ) ) ;
#30025 = AXIS2_PLACEMENT_3D ( 'NONE', #11111, #46674, #20425 ) ;
#30026 = ORIENTED_EDGE ( 'NONE', *, *, #61923, .T. ) ;
#30027 = CARTESIAN_POINT ( 'NONE',  ( 2.305787727787084407, 0.1666591538752685842, 7.654065630109507801 ) ) ;
#30028 = DIRECTION ( 'NONE',  ( 0.000000000000000000, -0.01356324068817999114, 0.9999080150203989437 ) ) ;
#30029 = CARTESIAN_POINT ( 'NONE',  ( 0.2653519890518152291, -7.871710682401847237, -9.381125756446651920 ) ) ;
#30030 = EDGE_CURVE ( 'NONE', #44248, #30290, #60241, .T. ) ;
#30031 = ORIENTED_EDGE ( 'NONE', *, *, #59381, .T. ) ;
#30032 = CIRCLE ( 'NONE', #10904, 12.75000000000000178 ) ;
#30033 = VECTOR ( 'NONE', #3926, 1000.000000000000000 ) ;
#30034 = CIRCLE ( 'NONE', #21554, 5.000000000000000000 ) ;
#30035 = VECTOR ( 'NONE', #12375, 1000.000000000000000 ) ;
#30036 = CARTESIAN_POINT ( 'NONE',  ( 29.10325845542004686, -3.352553978523171274, 24.67444324980777992 ) ) ;
#30037 = FACE_OUTER_BOUND ( 'NONE', #64999, .T. ) ;
#30038 = DIRECTION ( 'NONE',  ( 0.000000000000000000, 0.9718671068226468757, -0.2355298848897482422 ) ) ;
#30039 = ORIENTED_EDGE ( 'NONE', *, *, #37079, .T. ) ;
#30040 = DIRECTION ( 'NONE',  ( -1.000000000000000000, 0.000000000000000000, -0.000000000000000000 ) ) ;
#30041 = CARTESIAN_POINT ( 'NONE',  ( 15.82795513634610174, -34.24358411257765056, 7.361295665688344592 ) ) ;
#30042 = CARTESIAN_POINT ( 'NONE',  ( 3.924844264204268018, 5.816699323270774435, 10.49842868086190073 ) ) ;
#30043 = AXIS2_PLACEMENT_3D ( 'NONE', #52043, #38959, #13672 ) ;
#30044 = AXIS2_PLACEMENT_3D ( 'NONE', #22129, #36094, #30780 ) ;
#30045 = DIRECTION ( 'NONE',  ( 0.000000000000000000, -0.3554799084909035511, -0.9346839223284514331 ) ) ;
#30046 = CARTESIAN_POINT ( 'NONE',  ( 145.1370849898475797, 3.309064568108273190E-14, 0.000000000000000000 ) ) ;
#30047 = ORIENTED_EDGE ( 'NONE', *, *, #54064, .T. ) ;
#30048 = CARTESIAN_POINT ( 'NONE',  ( 3.347841273039249721, -10.61118957148187825, 5.603807266321171987 ) ) ;
#30049 = DIRECTION ( 'NONE',  ( 1.000000000000000000, 0.000000000000000000, 0.000000000000000000 ) ) ;
#30050 = CIRCLE ( 'NONE', #31103, 12.18649999999999700 ) ;
#30051 = LINE ( 'NONE', #21046, #32889 ) ;
#30052 = VERTEX_POINT ( 'NONE', #52271 ) ;
#30053 = CARTESIAN_POINT ( 'NONE',  ( 21.74230132213768485, 12.54654960210808134, -4.998279610834257092 ) ) ;
#30054 = CARTESIAN_POINT ( 'NONE',  ( 37.00000000000000711, -2.772148766916200380, -11.86701198550355585 ) ) ;
#30055 = EDGE_LOOP ( 'NONE', ( #59689, #37426, #44525, #16450 ) ) ;
#30056 = EDGE_CURVE ( 'NONE', #42706, #39575, #17296, .T. ) ;
#30057 = ORIENTED_EDGE ( 'NONE', *, *, #53131, .T. ) ;
#30058 = ORIENTED_EDGE ( 'NONE', *, *, #64865, .T. ) ;
#30059 = ADVANCED_FACE ( 'NONE', ( #48920 ), #3041, .T. ) ;
#30060 = AXIS2_PLACEMENT_3D ( 'NONE', #55278, #30647, #45624 ) ;
#30061 = ORIENTED_EDGE ( 'NONE', *, *, #1162, .F. ) ;
#30062 = CARTESIAN_POINT ( 'NONE',  ( 2.000000000000001776, 0.000000000000000000, 0.000000000000000000 ) ) ;
#30063 = CARTESIAN_POINT ( 'NONE',  ( -22.66110217412718342, -3.020638270782523449, 3.914841338650325131 ) ) ;
#30064 = CARTESIAN_POINT ( 'NONE',  ( 1.719304012338199517, 0.000000000000000000, 0.000000000000000000 ) ) ;
#30065 = CARTESIAN_POINT ( 'NONE',  ( -35.00000000000000000, -11.50504120060940316, -4.018060380616521599 ) ) ;
#30066 = CARTESIAN_POINT ( 'NONE',  ( -12.75996857643550797, -29.16082758670667019, 4.038023594093941959 ) ) ;
#30067 = CARTESIAN_POINT ( 'NONE',  ( -18.49080574448724690, 11.99999999999999645, 2.510045011421233839E-15 ) ) ;
#30069 = ORIENTED_EDGE ( 'NONE', *, *, #22429, .T. ) ;
#30068 = CARTESIAN_POINT ( 'NONE',  ( -35.00000000000000000, 6.280308599560139093, 9.926225166347048656 ) ) ;
#30070 = DIRECTION ( 'NONE',  ( 0.000000000000000000, 0.7790879021242487212, -0.6269146997508011632 ) ) ;
#30071 = ORIENTED_EDGE ( 'NONE', *, *, #23444, .T. ) ;
#30072 = CARTESIAN_POINT ( 'NONE',  ( 0.2638984909335720941, -11.57533005135176474, -4.001111175853858448 ) ) ;
#30073 = VERTEX_POINT ( 'NONE', #13637 ) ;
#30074 = AXIS2_PLACEMENT_3D ( 'NONE', #42324, #61642, #46687 ) ;
#30075 = ORIENTED_EDGE ( 'NONE', *, *, #21332, .T. ) ;
#30076 = CARTESIAN_POINT ( 'NONE',  ( 0.000000000000000000, -3.937687286050771895, -6.383151168292510391 ) ) ;
#30077 = CARTESIAN_POINT ( 'NONE',  ( 16.79298069408870830, -34.48269025770200358, 5.249417709786182940 ) ) ;
#30078 = PLANE ( 'NONE',  #1435 ) ;
#30079 = AXIS2_PLACEMENT_3D ( 'NONE', #27277, #11334, #51916 ) ;
#30080 = EDGE_CURVE ( 'NONE', #27538, #20683, #10097, .T. ) ;
#30081 = DIRECTION ( 'NONE',  ( 0.000000000000000000, -0.9903235168508566222, -0.1387779952735712363 ) ) ;
#30082 = DIRECTION ( 'NONE',  ( 0.000000000000000000, 0.000000000000000000, 1.000000000000000000 ) ) ;
#30083 = CARTESIAN_POINT ( 'NONE',  ( 2.256373768221667131, 5.936694589809198064, 4.807932997209342751 ) ) ;
#30084 = ORIENTED_EDGE ( 'NONE', *, *, #20555, .F. ) ;
#30085 =( BOUNDED_SURFACE ( )  B_SPLINE_SURFACE ( 3, 1, ( 
 ( #36474, #56786 ),
 ( #15838, #10211 ),
 ( #60764, #46447 ),
 ( #50475, #50786 ) ),
 .UNSPECIFIED., .F., .F., .F. ) 
 B_SPLINE_SURFACE_WITH_KNOTS ( ( 4, 4 ),
 ( 2, 2 ),
 ( 0.000000000000000000, 1.000000000000000000 ),
 ( 0.000000000000000000, 1.000000000000000000 ),
 .UNSPECIFIED. ) 
 GEOMETRIC_REPRESENTATION_ITEM ( )  RATIONAL_B_SPLINE_SURFACE ( (
 ( 1.000000000000000000, 1.000000000000000000),
 ( 0.9942764183789327692, 0.8450855930916585379),
 ( 0.9942764183789327692, 0.8450855930916585379),
 ( 1.000000000000000000, 1.000000000000000000) ) ) 
 REPRESENTATION_ITEM ( '' )  SURFACE ( )  );
#30086 = EDGE_CURVE ( 'NONE', #57900, #9681, #8374, .T. ) ;
#30087 = ORIENTED_EDGE ( 'NONE', *, *, #59482, .F. ) ;
#30088 = ADVANCED_FACE ( 'NONE', ( #28610 ), #3373, .T. ) ;
#30089 = CARTESIAN_POINT ( 'NONE',  ( 0.2648978790185584908, 11.46165506714228322, 4.312320170909275774 ) ) ;
#30090 = ORIENTED_EDGE ( 'NONE', *, *, #12976, .F. ) ;
#30091 = AXIS2_PLACEMENT_3D ( 'NONE', #13662, #60527, #4711 ) ;
#30092 = ADVANCED_FACE ( 'NONE', ( #12996 ), #8667, .T. ) ;
#30093 = VERTEX_POINT ( 'NONE', #63520 ) ;
#30094 = CIRCLE ( 'NONE', #20512, 12.18650000000000055 ) ;
#30095 = CARTESIAN_POINT ( 'NONE',  ( 2.000000000000001776, 6.160607635185406217, 4.277489166005578269 ) ) ;
#30096 = CARTESIAN_POINT ( 'NONE',  ( -27.09048036756592381, -2.303144499688043911, 0.1785511875142930804 ) ) ;
#30097 = LINE ( 'NONE', #31085, #48959 ) ;
#30098 = CARTESIAN_POINT ( 'NONE',  ( 18.09544918135259906, 5.659161111724000826, 10.59477254556587233 ) ) ;
#30099 = CARTESIAN_POINT ( 'NONE',  ( 2.298277635560279197, 7.651596582281724679, 0.1650558796844366904 ) ) ;
#30100 = VECTOR ( 'NONE', #13142, 1000.000000000000000 ) ;
#30101 = DIRECTION ( 'NONE',  ( -1.000000000000000000, 0.000000000000000000, 0.000000000000000000 ) ) ;
#30102 = EDGE_CURVE ( 'NONE', #33400, #16971, #12331, .T. ) ;
#30103 = CARTESIAN_POINT ( 'NONE',  ( 28.15950597331847405, -12.57621330935229231, 4.911510989912037495 ) ) ;
#30104 = EDGE_LOOP ( 'NONE', ( #4978, #37630, #27342, #9205 ) ) ;
#30105 = VECTOR ( 'NONE', #25091, 1000.000000000000000 ) ;
#30106 =( BOUNDED_CURVE ( )  B_SPLINE_CURVE ( 3, ( #32177, #26882, #43139, #42148 ),
 .UNSPECIFIED., .F., .F. ) 
 B_SPLINE_CURVE_WITH_KNOTS ( ( 4, 4 ),
 ( 4.643929506547320507, 4.657923478229592185 ),
 .UNSPECIFIED. ) 
 CURVE ( )  GEOMETRIC_REPRESENTATION_ITEM ( )  RATIONAL_B_SPLINE_CURVE ( ( 1.000000000000000000, 0.9999836807962925178, 0.9999836807962925178, 1.000000000000000000 ) ) 
 REPRESENTATION_ITEM ( '' )  );
#30107 = EDGE_CURVE ( 'NONE', #4916, #57516, #57080, .T. ) ;
#30108 = ORIENTED_EDGE ( 'NONE', *, *, #13676, .F. ) ;
#30109 = AXIS2_PLACEMENT_3D ( 'NONE', #7961, #13264, #2972 ) ;
#30110 = DIRECTION ( 'NONE',  ( 1.000000000000000000, 0.000000000000000000, 0.000000000000000000 ) ) ;
#30111 = CARTESIAN_POINT ( 'NONE',  ( 2.247112776671464918, 7.499199956302008196, -1.440655381229385190 ) ) ;
#30112 = DIRECTION ( 'NONE',  ( -1.000000000000000000, 0.000000000000000000, 0.000000000000000000 ) ) ;
#30113 = MANIFOLD_SOLID_BREP ( 'Cut-Extrude2', #44007 ) ;
#30114 = CARTESIAN_POINT ( 'NONE',  ( 24.82652845881425208, 25.00000000000000000, -8.578654028722157321 ) ) ;
#30115 = AXIS2_PLACEMENT_3D ( 'NONE', #33604, #44226, #18967 ) ;
#30116 = CARTESIAN_POINT ( 'NONE',  ( -35.00000000000000000, 12.71517666308949401, -0.9416912585473022901 ) ) ;
#30117 = EDGE_CURVE ( 'NONE', #46746, #40556, #25214, .T. ) ;
#30118 = CARTESIAN_POINT ( 'NONE',  ( -35.00000000000000000, -6.891188680298757419, -9.512294188640973758 ) ) ;
#30119 = CARTESIAN_POINT ( 'NONE',  ( 2.241352910868910531, 5.794346703933913822, -4.970878533273699773 ) ) ;
#30120 = CARTESIAN_POINT ( 'NONE',  ( -27.08429572838383947, -2.089332284968714593, -0.9410937941434025511 ) ) ;
#30121 = VERTEX_POINT ( 'NONE', #55191 ) ;
#30122 = AXIS2_PLACEMENT_3D ( 'NONE', #38150, #7927, #28198 ) ;
#30123 = CARTESIAN_POINT ( 'NONE',  ( 1.948354844644523132, -4.761851831285707881, -10.97658859990240998 ) ) ;
#30124 = CARTESIAN_POINT ( 'NONE',  ( 0.3665391374699464300, -12.04754782681755998, -2.392238720110583472 ) ) ;
#30125 = CARTESIAN_POINT ( 'NONE',  ( 0.3665391374699465965, 12.27992639892678284, -0.2638605131387583569 ) ) ;
#30126 = B_SPLINE_CURVE_WITH_KNOTS ( 'NONE', 3,
 ( #56492, #15268, #10939, #5979, #50853, #30550, #35206, #5300, #24931, #45864, #11271, #20598, #61799, #19928, #26235, #40193 ),
 .UNSPECIFIED., .F., .F.,
 ( 4, 3, 3, 3, 3, 4 ),
 ( 0.000000000000000000, 0.0002999043160757333833, 0.0005998071753050970975, 0.0008997092107374508744, 0.001204458948195599125, 0.001510329163476425464 ),
 .UNSPECIFIED. ) ;
#30127 = VECTOR ( 'NONE', #39283, 1000.000000000000000 ) ;
#30128 = CARTESIAN_POINT ( 'NONE',  ( -35.00000000000000000, -1.488153103997047033, 11.65150730582934102 ) ) ;
#30129 = CARTESIAN_POINT ( 'NONE',  ( 1.937114397841932290, 12.45230409340481437, 3.111612666690119156 ) ) ;
#30130 = CIRCLE ( 'NONE', #26959, 5.000000000000000888 ) ;
#30131 = ORIENTED_EDGE ( 'NONE', *, *, #61027, .T. ) ;
#30132 = DIRECTION ( 'NONE',  ( 0.000000000000000000, -0.01356324068817998940, 0.9999080150203990547 ) ) ;
#30133 = CARTESIAN_POINT ( 'NONE',  ( 0.3665391374699467075, -12.27992639892678284, -0.2638605131388441216 ) ) ;
#30134 = B_SPLINE_CURVE_WITH_KNOTS ( 'NONE', 3,
 ( #60911, #20009, #51275, #721, #15656, #45597, #11022, #10038, #35932, #61885, #40272, #30319, #36276 ),
 .UNSPECIFIED., .F., .F.,
 ( 4, 3, 3, 3, 4 ),
 ( 2.424349759030287857E-18, 6.990956068646416019E-05, 0.0001398191187764045215, 0.0002097286751720215173, 0.0002792983885906414167 ),
 .UNSPECIFIED. ) ;
#30135 = VECTOR ( 'NONE', #5940, 1000.000000000000000 ) ;
#30136 = CARTESIAN_POINT ( 'NONE',  ( 12.30974346995382973, -29.30943841933768823, -5.552318955346970064 ) ) ;
#30137 = VERTEX_POINT ( 'NONE', #60844 ) ;
#30138 = CARTESIAN_POINT ( 'NONE',  ( -35.00000000000000000, 0.000000000000000000, 0.000000000000000000 ) ) ;
#30139 = CARTESIAN_POINT ( 'NONE',  ( -27.45775109278351067, -10.51123867646838050, -8.471355351200609007 ) ) ;
#30140 = LINE ( 'NONE', #9504, #11067 ) ;
#30141 = AXIS2_PLACEMENT_3D ( 'NONE', #34112, #23508, #60064 ) ;
#30143 = ORIENTED_EDGE ( 'NONE', *, *, #60637, .F. ) ;
#30142 = CARTESIAN_POINT ( 'NONE',  ( 2.000000000000001776, 6.936109781200720192, -2.853135311044974198 ) ) ;
#30144 = CARTESIAN_POINT ( 'NONE',  ( -9.809773280085975600, -12.34599478600513578, -5.464898509519898084 ) ) ;
#30145 = EDGE_CURVE ( 'NONE', #10633, #14359, #15705, .T. ) ;
#30146 = DIRECTION ( 'NONE',  ( 0.000000000000000000, -0.6478160128812002760, 0.7617968321374830598 ) ) ;
#30147 = ORIENTED_EDGE ( 'NONE', *, *, #51569, .T. ) ;
#30148 = CARTESIAN_POINT ( 'NONE',  ( 0.3401186441510221092, 7.690203051556021130, 9.562489599411557961 ) ) ;
#30149 = CARTESIAN_POINT ( 'NONE',  ( -9.246430435658307800, 11.49892766232029295, -7.081925484302661999 ) ) ;
#30150 = DIRECTION ( 'NONE',  ( 0.000000000000000000, -0.01356324068817998940, 0.9999080150203990547 ) ) ;
#30151 = CARTESIAN_POINT ( 'NONE',  ( 0.3675815128205894289, -1.872154644482002528, -12.13672785388552100 ) ) ;
#30152 = CARTESIAN_POINT ( 'NONE',  ( 0.3675815128205912052, -11.44679196252406506, -4.447030445008294919 ) ) ;
#30153 = VECTOR ( 'NONE', #38444, 1000.000000000000000 ) ;
#30154 = FACE_OUTER_BOUND ( 'NONE', #56136, .T. ) ;
#30155 = CARTESIAN_POINT ( 'NONE',  ( 2.269879328255106188, 1.181008584587388999, -7.552124491909401272 ) ) ;
#30156 = ORIENTED_EDGE ( 'NONE', *, *, #12115, .F. ) ;
#30157 = CYLINDRICAL_SURFACE ( 'NONE', #20417, 5.000000000000000888 ) ;
#30158 = VERTEX_POINT ( 'NONE', #15286 ) ;
#30159 = CARTESIAN_POINT ( 'NONE',  ( -25.00000000000000355, -30.00000000000000000, 5.000000000000000888 ) ) ;
#30160 = EDGE_CURVE ( 'NONE', #17913, #60517, #34773, .T. ) ;
#30161 = DIRECTION ( 'NONE',  ( 0.7932577242209934987, -0.6088860180392799970, 0.000000000000000000 ) ) ;
#30162 = ORIENTED_EDGE ( 'NONE', *, *, #19283, .F. ) ;
#30163 = CARTESIAN_POINT ( 'NONE',  ( -27.45775109278350712, -13.35262336282553441, -1.989333891161978674 ) ) ;
#30164 = CARTESIAN_POINT ( 'NONE',  ( 11.94227997924816087, 11.73039363638092247, -2.534770156389862361 ) ) ;
#30165 = EDGE_CURVE ( 'NONE', #28743, #52094, #39237, .T. ) ;
#30166 = CARTESIAN_POINT ( 'NONE',  ( 2.000000000000001776, 4.976357229393855164, 4.652926418895560801 ) ) ;
#30167 = VERTEX_POINT ( 'NONE', #59534 ) ;
#30168 = EDGE_LOOP ( 'NONE', ( #63505, #24368, #55171, #20870 ) ) ;
#30169 = CARTESIAN_POINT ( 'NONE',  ( 35.00000000000000000, 4.705694406421931860E-17, -3.469127814946512892E-15 ) ) ;
#30170 = EDGE_CURVE ( 'NONE', #23325, #9488, #43285, .T. ) ;
#30171 = AXIS2_PLACEMENT_3D ( 'NONE', #55754, #50761, #61704 ) ;
#30172 = VECTOR ( 'NONE', #50313, 1000.000000000000000 ) ;
#30173 = EDGE_LOOP ( 'NONE', ( #9152, #10353, #11097, #15244 ) ) ;
#30174 = CARTESIAN_POINT ( 'NONE',  ( 37.00000000000000711, -2.216820770815006725, 11.53507381115585417 ) ) ;
#30175 = CYLINDRICAL_SURFACE ( 'NONE', #28907, 5.000000000000000888 ) ;
#30176 = CARTESIAN_POINT ( 'NONE',  ( -47.00000000000000711, 0.000000000000000000, 0.000000000000000000 ) ) ;
#30177 = CARTESIAN_POINT ( 'NONE',  ( -29.65104263560079545, -0.5515657081232090420, 11.98927152364481685 ) ) ;
#30178 = CARTESIAN_POINT ( 'NONE',  ( 35.00000000000000000, 4.705694406421931860E-17, -3.469127814946512892E-15 ) ) ;
#30179 = CARTESIAN_POINT ( 'NONE',  ( -14.11589373245165469, 8.250315036047107142, 10.68561190601526611 ) ) ;
#30180 = LINE ( 'NONE', #50483, #29073 ) ;
#30181 = EDGE_LOOP ( 'NONE', ( #12398, #40003, #42680, #4653 ) ) ;
#30182 = CARTESIAN_POINT ( 'NONE',  ( 37.00000000000000711, 11.07407352312218052, 3.916263239775223504 ) ) ;
#30183 = EDGE_CURVE ( 'NONE', #38380, #47639, #40215, .T. ) ;
#30184 = CARTESIAN_POINT ( 'NONE',  ( 2.835339799623988188, 4.197472173747801349, -6.612744557053391148 ) ) ;
#30185 = EDGE_CURVE ( 'NONE', #6763, #62669, #58172, .T. ) ;
#30186 = FACE_OUTER_BOUND ( 'NONE', #31431, .T. ) ;
#30187 = CARTESIAN_POINT ( 'NONE',  ( -21.17861794710831091, 13.00977982294135593, -3.604945070120774808 ) ) ;
#30188 = VECTOR ( 'NONE', #34025, 1000.000000000000114 ) ;
#30189 = DIRECTION ( 'NONE',  ( 0.000000000000000000, -0.01356324068817998940, 0.9999080150203990547 ) ) ;
#30190 = CARTESIAN_POINT ( 'NONE',  ( -35.00000000000000000, 11.72195762423408816, 0.7536123767500589876 ) ) ;
#30191 = CARTESIAN_POINT ( 'NONE',  ( 0.000000000000000000, 0.000000000000000000, 0.000000000000000000 ) ) ;
#30192 = CARTESIAN_POINT ( 'NONE',  ( -35.00000000000000000, 5.130401251914729954, 11.05394794832831451 ) ) ;
#30193 = EDGE_CURVE ( 'NONE', #20774, #26468, #65170, .T. ) ;
#30194 = AXIS2_PLACEMENT_3D ( 'NONE', #52817, #2288, #56496 ) ;
#30195 = B_SPLINE_CURVE_WITH_KNOTS ( 'NONE', 3,
 ( #58805, #53797, #19185, #13223, #33508, #54110, #44771, #64715, #8232, #33810, #4227, #44130, #28502, #24495, #29177, #49472, #3912, #39456, #59759 ),
 .UNSPECIFIED., .F., .F.,
 ( 4, 3, 3, 3, 3, 3, 4 ),
 ( 0.000000000000000000, 2.831840207499378850E-05, 4.217266859840141746E-05, 5.602024318395757232E-05, 6.290810167968961255E-05, 9.120440630944950803E-05, 0.0001153103026479763337 ),
 .UNSPECIFIED. ) ;
#30196 = EDGE_LOOP ( 'NONE', ( #55929, #22803, #30488, #2375 ) ) ;
#30197 = DIRECTION ( 'NONE',  ( 1.000000000000000000, -0.000000000000000000, 0.000000000000000000 ) ) ;
#30198 = EDGE_CURVE ( 'NONE', #18188, #29586, #5107, .T. ) ;
#30199 = ORIENTED_EDGE ( 'NONE', *, *, #14214, .T. ) ;
#30200 = CARTESIAN_POINT ( 'NONE',  ( -2.927828093388545661, -11.04426939139958463, 4.708968905878549549 ) ) ;
#30201 = CARTESIAN_POINT ( 'NONE',  ( 2.249013661412228693, -7.499157010299424719, -1.444210756221623759 ) ) ;
#30202 = VECTOR ( 'NONE', #51923, 1000.000000000000000 ) ;
#30203 = CARTESIAN_POINT ( 'NONE',  ( -17.96022329889432001, 6.012774911231331565, -12.08928202576066369 ) ) ;
#30204 = EDGE_CURVE ( 'NONE', #9138, #35622, #13577, .T. ) ;
#30205 = CARTESIAN_POINT ( 'NONE',  ( 41.00000000000000711, -1.694065894508600678E-18, 0.000000000000000000 ) ) ;
#30206 = CARTESIAN_POINT ( 'NONE',  ( 2.242418902651891255, 2.517330194228720064, -7.207816731001243760 ) ) ;
#30207 = ORIENTED_EDGE ( 'NONE', *, *, #44652, .F. ) ;
#30208 = DIRECTION ( 'NONE',  ( -1.000000000000000000, 0.000000000000000000, 0.000000000000000000 ) ) ;
#30209 = CARTESIAN_POINT ( 'NONE',  ( -36.00000000000000711, 10.84030624090606665, 6.711949091238182064 ) ) ;
#30210 = DIRECTION ( 'NONE',  ( 1.000000000000000000, 0.000000000000000000, -0.000000000000000000 ) ) ;
#30211 = CARTESIAN_POINT ( 'NONE',  ( -27.35552965826137140, -0.2619431035391951434, 3.094132632038943065 ) ) ;
#30212 = B_SPLINE_CURVE_WITH_KNOTS ( 'NONE', 3,
 ( #55566, #48950, #64857, #19671, #14000, #19339, #3408, #64225, #8702, #18699, #39930, #38957, #59248, #39605, #13669, #28985 ),
 .UNSPECIFIED., .F., .F.,
 ( 4, 3, 3, 3, 3, 4 ),
 ( 0.000000000000000000, 0.0003017745587525273612, 0.0006035491769808764510, 0.0009053241094668200428, 0.001207275924539990414, 0.001510325902532977686 ),
 .UNSPECIFIED. ) ;
#30213 = AXIS2_PLACEMENT_3D ( 'NONE', #53180, #28554, #7629 ) ;
#30214 = CARTESIAN_POINT ( 'NONE',  ( 0.3665391374699467075, 12.27992639892678461, 0.2638605131387583569 ) ) ;
#30215 = CARTESIAN_POINT ( 'NONE',  ( 0.000000000000000000, 6.470132594555847660, -2.133363481234036296 ) ) ;
#30216 = ORIENTED_EDGE ( 'NONE', *, *, #1015, .T. ) ;
#30217 = DIRECTION ( 'NONE',  ( -1.000000000000000000, -0.000000000000000000, 0.000000000000000000 ) ) ;
#30218 = ORIENTED_EDGE ( 'NONE', *, *, #62738, .T. ) ;
#30219 = CARTESIAN_POINT ( 'NONE',  ( 0.2651627682582924916, 12.24583720278846677, -0.08809604936510406770 ) ) ;
#30220 = CARTESIAN_POINT ( 'NONE',  ( -16.81801275797650419, -34.49999999999998579, 5.265606433706007117 ) ) ;
#30221 = CIRCLE ( 'NONE', #480, 12.75000000000000178 ) ;
#30222 = DIRECTION ( 'NONE',  ( 0.000000000000000000, 0.8827602140260299990, -0.4698238015817395308 ) ) ;
#30223 = CARTESIAN_POINT ( 'NONE',  ( 37.00000000000000711, 12.74613886779084737, -0.3137578094509725357 ) ) ;
#30224 = EDGE_CURVE ( 'NONE', #48664, #17397, #56057, .T. ) ;
#30225 = ORIENTED_EDGE ( 'NONE', *, *, #31647, .T. ) ;
#30226 = ORIENTED_EDGE ( 'NONE', *, *, #56123, .T. ) ;
#30227 = DIRECTION ( 'NONE',  ( 1.000000000000000000, 0.000000000000000000, 0.000000000000000000 ) ) ;
#30228 = VERTEX_POINT ( 'NONE', #64503 ) ;
#30229 = DIRECTION ( 'NONE',  ( 0.000000000000000000, -0.5243256840888622650, -0.8515178078024832065 ) ) ;
#30231 = VECTOR ( 'NONE', #23839, 1000.000000000000000 ) ;
#30230 = DIRECTION ( 'NONE',  ( 0.000000000000000000, -0.8696919319575239227, -0.4935949184179166394 ) ) ;
#30232 = DIRECTION ( 'NONE',  ( -0.000000000000000000, -1.000000000000000000, -0.000000000000000000 ) ) ;
#30233 = CARTESIAN_POINT ( 'NONE',  ( 35.00000000000000000, -6.950793414699864670, -10.68873102412840304 ) ) ;
#30234 = CYLINDRICAL_SURFACE ( 'NONE', #39620, 12.18649999999999878 ) ;
#30235 = CARTESIAN_POINT ( 'NONE',  ( -17.29244623348158783, 2.525873743887551814, 11.73115347397430597 ) ) ;
#30236 = DIRECTION ( 'NONE',  ( 0.9996161839461982224, 0.02770351589312032917, -0.000000000000000000 ) ) ;
#30237 = VERTEX_POINT ( 'NONE', #4999 ) ;
#30238 = VECTOR ( 'NONE', #32530, 1000.000000000000000 ) ;
#30239 = EDGE_CURVE ( 'NONE', #38324, #39393, #49914, .T. ) ;
#30240 = CARTESIAN_POINT ( 'NONE',  ( 5.514970785353741078, 0.004713149585127261558, 0.0003039746380524470729 ) ) ;
#30241 = VERTEX_POINT ( 'NONE', #54874 ) ;
#30242 = CARTESIAN_POINT ( 'NONE',  ( -35.00000000000000000, -10.91536515067645041, -4.339012074900068683 ) ) ;
#30243 = AXIS2_PLACEMENT_3D ( 'NONE', #34407, #23798, #64330 ) ;
#30244 = CARTESIAN_POINT ( 'NONE',  ( -35.00000000000000000, 0.000000000000000000, 0.000000000000000000 ) ) ;
#30245 = ADVANCED_FACE ( 'NONE', ( #45535 ), #49888, .T. ) ;
#30246 = ORIENTED_EDGE ( 'NONE', *, *, #59107, .F. ) ;
#30247 = FACE_OUTER_BOUND ( 'NONE', #39682, .T. ) ;
#30248 = ORIENTED_EDGE ( 'NONE', *, *, #22215, .T. ) ;
#30249 = LINE ( 'NONE', #60494, #59897 ) ;
#30250 = DIRECTION ( 'NONE',  ( 0.000000000000000000, -0.01356324068817999114, 0.9999080150203989437 ) ) ;
#30251 = CARTESIAN_POINT ( 'NONE',  ( -37.00000000000000711, 5.672855678558835102, -10.28547182238001767 ) ) ;
#30252 = CARTESIAN_POINT ( 'NONE',  ( 4.200159495149293321, -10.86999738484834666, 5.085916799879192318 ) ) ;
#30253 = ORIENTED_EDGE ( 'NONE', *, *, #44004, .T. ) ;
#30254 = VERTEX_POINT ( 'NONE', #14606 ) ;
#30255 = CARTESIAN_POINT ( 'NONE',  ( 2.770579946183328257, -6.910873157406261846, 3.639932028439796241 ) ) ;
#30256 = EDGE_CURVE ( 'NONE', #11727, #61427, #47449, .T. ) ;
#30257 = VERTEX_POINT ( 'NONE', #61172 ) ;
#30258 = CARTESIAN_POINT ( 'NONE',  ( 0.2911222467163572802, 11.58731125337565437, -3.989243506922225624 ) ) ;
#30259 = ORIENTED_EDGE ( 'NONE', *, *, #35072, .F. ) ;
#30260 = ORIENTED_EDGE ( 'NONE', *, *, #17751, .F. ) ;
#30261 = EDGE_LOOP ( 'NONE', ( #18041, #10143, #414, #18805 ) ) ;
#30262 = LINE ( 'NONE', #25261, #4412 ) ;
#30263 = CARTESIAN_POINT ( 'NONE',  ( -16.02919692786943173, -28.24921752684736376, 10.30002093107130179 ) ) ;
#30264 = AXIS2_PLACEMENT_3D ( 'NONE', #32697, #20865, #41133 ) ;
#30265 = CARTESIAN_POINT ( 'NONE',  ( 37.00000000000000711, 4.705694406421931860E-17, -3.469127814946512892E-15 ) ) ;
#30266 = CARTESIAN_POINT ( 'NONE',  ( -35.00000000000000000, 0.000000000000000000, 0.000000000000000000 ) ) ;
#30267 = CARTESIAN_POINT ( 'NONE',  ( 2.000000000000001776, -3.230174184210094168, 5.998318953995296354 ) ) ;
#30268 = ORIENTED_EDGE ( 'NONE', *, *, #17938, .F. ) ;
#30269 = CARTESIAN_POINT ( 'NONE',  ( 2.298277635560095788, -2.461898367585350300, -7.246601281227178504 ) ) ;
#30270 = EDGE_LOOP ( 'NONE', ( #59202, #499 ) ) ;
#30271 = DIRECTION ( 'NONE',  ( 0.000000000000000000, 0.01356324068817998940, -0.9999080150203989437 ) ) ;
#30272 = FACE_OUTER_BOUND ( 'NONE', #47081, .T. ) ;
#30273 = CIRCLE ( 'NONE', #36630, 12.74999999999999822 ) ;
#30274 = VERTEX_POINT ( 'NONE', #63360 ) ;
#30275 = CYLINDRICAL_SURFACE ( 'NONE', #1010, 4.999999999999999112 ) ;
#30276 = CARTESIAN_POINT ( 'NONE',  ( -35.00000000000000000, 0.000000000000000000, 0.000000000000000000 ) ) ;
#30277 = CARTESIAN_POINT ( 'NONE',  ( 35.00000000000000000, 3.287724142101414504, -11.73463472867577373 ) ) ;
#30278 = EDGE_CURVE ( 'NONE', #9709, #1625, #663, .T. ) ;
#30279 = ORIENTED_EDGE ( 'NONE', *, *, #6886, .F. ) ;
#30280 = CARTESIAN_POINT ( 'NONE',  ( 1.372161826076010005, 6.811451307636476216, 10.61825687422740927 ) ) ;
#30281 = EDGE_CURVE ( 'NONE', #38082, #58835, #14894, .T. ) ;
#30282 = AXIS2_PLACEMENT_3D ( 'NONE', #52229, #15323, #35596 ) ;
#30283 = ORIENTED_EDGE ( 'NONE', *, *, #1531, .T. ) ;
#30284 = CARTESIAN_POINT ( 'NONE',  ( 0.000000000000000000, -3.341639490130797530, 6.078525953551414673 ) ) ;
#30285 = CARTESIAN_POINT ( 'NONE',  ( 36.00000000000000711, 10.23119532541072552, -7.608228585767763619 ) ) ;
#30286 = CARTESIAN_POINT ( 'NONE',  ( -14.60253471108646472, -28.81751583403978145, 11.78204505887441655 ) ) ;
#30287 = EDGE_CURVE ( 'NONE', #59819, #59561, #26569, .T. ) ;
#30288 = CARTESIAN_POINT ( 'NONE',  ( 2.524535260912121437, 4.054303386867375458, 6.580044328001015685 ) ) ;
#30289 = DIRECTION ( 'NONE',  ( -1.000000000000000000, 0.000000000000000000, -0.000000000000000000 ) ) ;
#30290 = VERTEX_POINT ( 'NONE', #7863 ) ;
#30291 = CARTESIAN_POINT ( 'NONE',  ( 2.256373768223419063, -4.807932997207736037, 5.936694589811255973 ) ) ;
#30292 = CARTESIAN_POINT ( 'NONE',  ( 0.4613984246114870569, 5.909164750631185292, -10.80075367333616221 ) ) ;
#30293 = CARTESIAN_POINT ( 'NONE',  ( 2.241352910868908754, 3.889181972941541776, -6.569501556381402096 ) ) ;
#30294 = CARTESIAN_POINT ( 'NONE',  ( 2.835339799623979751, 3.628068688271675502, 6.941489812670536885 ) ) ;
#30295 = AXIS2_PLACEMENT_3D ( 'NONE', #46358, #60325, #20096 ) ;
#30296 = CARTESIAN_POINT ( 'NONE',  ( 0.3654063281920768569, -12.13594617907220297, -1.872466061177207708 ) ) ;
#30297 =( BOUNDED_SURFACE ( )  B_SPLINE_SURFACE ( 3, 1, ( 
 ( #65239, #29335 ),
 ( #18730, #41182 ),
 ( #8401, #19707 ),
 ( #54300, #15587 ) ),
 .UNSPECIFIED., .F., .F., .F. ) 
 B_SPLINE_SURFACE_WITH_KNOTS ( ( 4, 4 ),
 ( 2, 2 ),
 ( 0.000000000000000000, 1.000000000000000000 ),
 ( 0.000000000000000000, 1.000000000000000000 ),
 .UNSPECIFIED. ) 
 GEOMETRIC_REPRESENTATION_ITEM ( )  RATIONAL_B_SPLINE_SURFACE ( (
 ( 1.000000000000000000, 1.000000000000000000),
 ( 0.9942764183789327692, 0.8450855930916580938),
 ( 0.9942764183789327692, 0.8450855930916580938),
 ( 1.000000000000000000, 1.000000000000000000) ) ) 
 REPRESENTATION_ITEM ( '' )  SURFACE ( )  );
#30298 = CARTESIAN_POINT ( 'NONE',  ( 2.000000000000001776, 5.860254403322016969, 3.474373880649828550 ) ) ;
#30299 = LINE ( 'NONE', #50595, #12865 ) ;
#30300 = FACE_OUTER_BOUND ( 'NONE', #54390, .T. ) ;
#30301 = CARTESIAN_POINT ( 'NONE',  ( 2.249013661412227805, 0.1200550008340211805, -7.636012530783590435 ) ) ;
#30302 = CIRCLE ( 'NONE', #55801, 12.75000000000000178 ) ;
#30303 = ADVANCED_FACE ( 'NONE', ( #51857 ), #27800, .T. ) ;
#30304 = B_SPLINE_CURVE_WITH_KNOTS ( 'NONE', 3,
 ( #35115, #64404, #24504, #14508, #39137, #34785, #30155, #45436, #9519, #44779, #24846, #50455, #64723, #59430, #19194, #59767, #14196, #34483, #54786 ),
 .UNSPECIFIED., .F., .F.,
 ( 4, 3, 3, 3, 3, 3, 4 ),
 ( 6.952433221959954168E-18, 2.825908398991504083E-05, 4.208813692702534923E-05, 5.591713747220676827E-05, 6.279584083537379164E-05, 9.105792820726774008E-05, 0.0001153131102486950596 ),
 .UNSPECIFIED. ) ;
#30305 = VERTEX_POINT ( 'NONE', #56171 ) ;
#30306 = CARTESIAN_POINT ( 'NONE',  ( -27.08954555554413801, -1.307633183325040749, -1.900922216193322134 ) ) ;
#30307 = B_SPLINE_CURVE_WITH_KNOTS ( 'NONE', 3,
 ( #53168, #7614, #48206, #28226, #32529, #23906, #2658, #53515, #58842, #17919, #22919, #43173, #23232, #38858, #63449, #38179, #62802, #3640, #52839 ),
 .UNSPECIFIED., .F., .F.,
 ( 4, 3, 3, 3, 3, 3, 4 ),
 ( 1.158841720744533638E-17, 4.457896483014629118E-05, 6.639290541541733389E-05, 8.820687556478164942E-05, 0.0001100173248778832900, 0.0001545671401657995527, 0.0001830328308068548092 ),
 .UNSPECIFIED. ) ;
#30308 = EDGE_CURVE ( 'NONE', #60184, #817, #15603, .T. ) ;
#30309 = ORIENTED_EDGE ( 'NONE', *, *, #43234, .F. ) ;
#30310 = DIRECTION ( 'NONE',  ( 0.000000000000000000, -1.000000000000000000, 0.000000000000000000 ) ) ;
#30311 = CARTESIAN_POINT ( 'NONE',  ( -22.27722019094931127, -3.623977093944207084, 0.6491642780571700300 ) ) ;
#30312 = CARTESIAN_POINT ( 'NONE',  ( 1.000000000000000888, 4.604744433234674972, 5.919993978425482695 ) ) ;
#30313 = CARTESIAN_POINT ( 'NONE',  ( 0.2646305136544065406, -0.1321451301298699199, 12.24595685781654453 ) ) ;
#30314 = EDGE_LOOP ( 'NONE', ( #52332, #7154, #46442, #58696 ) ) ;
#30315 = EDGE_CURVE ( 'NONE', #40551, #55012, #63462, .T. ) ;
#30316 = ORIENTED_EDGE ( 'NONE', *, *, #16439, .F. ) ;
#30317 = VERTEX_POINT ( 'NONE', #48102 ) ;
#30318 = CARTESIAN_POINT ( 'NONE',  ( 5.516018279890452902, 0.002104829434641014487, 0.006440244342253419532 ) ) ;
#30319 = CARTESIAN_POINT ( 'NONE',  ( -22.27722019117889829, 0.6723250025933701357, 3.619826115298641511 ) ) ;
#30320 = ORIENTED_EDGE ( 'NONE', *, *, #35237, .F. ) ;
#30321 = DIRECTION ( 'NONE',  ( 1.000000000000000000, 0.000000000000000000, 0.000000000000000000 ) ) ;
#30322 = CYLINDRICAL_SURFACE ( 'NONE', #34670, 5.000000000000000888 ) ;
#30323 = CARTESIAN_POINT ( 'NONE',  ( 2.000000000000001776, 6.539067737394503865, 2.314222412769824544 ) ) ;
#30324 = ORIENTED_EDGE ( 'NONE', *, *, #59320, .T. ) ;
#30325 = VECTOR ( 'NONE', #54174, 1000.000000000000000 ) ;
#30326 = CARTESIAN_POINT ( 'NONE',  ( -22.31213670151049300, 0.2530575063956244097, 3.777944311993711057 ) ) ;
#30327 = CARTESIAN_POINT ( 'NONE',  ( 4.513117160428445906, -30.90576903066049752, -14.85933548762053924 ) ) ;
#30328 = LINE ( 'NONE', #10356, #63177 ) ;
#30330 = VERTEX_POINT ( 'NONE', #41198 ) ;
#30329 = CARTESIAN_POINT ( 'NONE',  ( -27.09125059358712306, 1.662156772100933377, 1.607567221344176067 ) ) ;
#30331 = DIRECTION ( 'NONE',  ( 0.000000000000000000, -1.000000000000000000, 0.000000000000000000 ) ) ;
#30332 = EDGE_CURVE ( 'NONE', #48986, #56955, #35875, .T. ) ;
#30333 = ORIENTED_EDGE ( 'NONE', *, *, #22697, .F. ) ;
#30334 = DIRECTION ( 'NONE',  ( -1.000000000000000000, 0.000000000000000000, -0.000000000000000000 ) ) ;
#30335 = ORIENTED_EDGE ( 'NONE', *, *, #59834, .T. ) ;
#30336 = LINE ( 'NONE', #50628, #59240 ) ;
#30337 = CARTESIAN_POINT ( 'NONE',  ( -35.00000000000000000, 0.000000000000000000, 0.000000000000000000 ) ) ;
#30338 = EDGE_CURVE ( 'NONE', #2871, #30167, #32761, .T. ) ;
#30339 = AXIS2_PLACEMENT_3D ( 'NONE', #58391, #12816, #48428 ) ;
#30340 = CARTESIAN_POINT ( 'NONE',  ( 5.514624014163232779, 0.004104370840204389984, 0.0005510299962881913495 ) ) ;
#30341 = FACE_OUTER_BOUND ( 'NONE', #6114, .T. ) ;
#30342 = DIRECTION ( 'NONE',  ( 0.000000000000000000, -0.9937233664769772323, 0.1118654143051511785 ) ) ;
#30343 = CARTESIAN_POINT ( 'NONE',  ( -35.00000000000000000, -10.28547182238004076, -5.672855678558794246 ) ) ;
#30344 = CARTESIAN_POINT ( 'NONE',  ( 0.2646305136544072623, -4.064188116014475938, -11.55263159009962592 ) ) ;
#30345 = DIRECTION ( 'NONE',  ( -1.000000000000000000, 0.000000000000000000, 0.000000000000000000 ) ) ;
#30346 = CYLINDRICAL_SURFACE ( 'NONE', #30060, 5.000000000000000888 ) ;
#30348 = ORIENTED_EDGE ( 'NONE', *, *, #11193, .F. ) ;
#30347 = CARTESIAN_POINT ( 'NONE',  ( -18.58686583997218733, 4.908862989891756179, -12.57862506157752236 ) ) ;
#30349 = DIRECTION ( 'NONE',  ( 0.000000000000000000, 0.9467777615094583599, 0.3218879778915939571 ) ) ;
#30350 = EDGE_LOOP ( 'NONE', ( #10343, #49561, #10827, #35445 ) ) ;
#30351 = CARTESIAN_POINT ( 'NONE',  ( 11.66906220897710433, -13.41085082018220298, -1.554662609128065975 ) ) ;
#30352 = ORIENTED_EDGE ( 'NONE', *, *, #12684, .F. ) ;
#30353 = ORIENTED_EDGE ( 'NONE', *, *, #41690, .T. ) ;
#30354 = CARTESIAN_POINT ( 'NONE',  ( 0.2717059086739013196, 8.007130974640039867, 9.268607328094562448 ) ) ;
#30355 = DIRECTION ( 'NONE',  ( 0.000000000000000000, 0.000000000000000000, -1.000000000000000000 ) ) ;
#30356 = CARTESIAN_POINT ( 'NONE',  ( -27.09125059358653331, -2.223272438024535003, 0.6356863790372223599 ) ) ;
#30357 = CARTESIAN_POINT ( 'NONE',  ( -14.47334165536100059, 0.000000000000000000, 0.000000000000000000 ) ) ;
#30358 = EDGE_CURVE ( 'NONE', #53925, #14785, #62411, .T. ) ;
#30359 = FACE_OUTER_BOUND ( 'NONE', #11484, .T. ) ;
#30360 = AXIS2_PLACEMENT_3D ( 'NONE', #61760, #5944, #16556 ) ;
#30361 = CARTESIAN_POINT ( 'NONE',  ( 2.000000000000001776, 4.472310526050855550, -6.020667617347345235 ) ) ;
#30362 = EDGE_CURVE ( 'NONE', #11339, #59141, #51814, .T. ) ;
#30363 = EDGE_LOOP ( 'NONE', ( #46501, #30716, #39310, #18416 ) ) ;
#30364 = DIRECTION ( 'NONE',  ( 0.000000000000000000, 0.4935949184179201366, -0.8696919319575218132 ) ) ;
#30365 = DIRECTION ( 'NONE',  ( 0.000000000000000000, -0.01356324068817998073, 0.9999080150203990547 ) ) ;
#30366 = CARTESIAN_POINT ( 'NONE',  ( 0.4626703367443509851, 12.07256244737112816, 2.416235258139790343 ) ) ;
#30367 = ORIENTED_EDGE ( 'NONE', *, *, #9649, .F. ) ;
#30368 = DIRECTION ( 'NONE',  ( 0.000000000000000000, 1.000000000000000000, 0.000000000000000000 ) ) ;
#30369 = ADVANCED_FACE ( 'NONE', ( #26252 ), #46526, .T. ) ;
#30370 = AXIS2_PLACEMENT_3D ( 'NONE', #61905, #1066, #36635 ) ;
#30371 = DIRECTION ( 'NONE',  ( 0.000000000000000000, -0.01356324068818685717, 0.9999080150203989437 ) ) ;
#30372 = CARTESIAN_POINT ( 'NONE',  ( -48.71973356879950501, -0.2586908456633208453, -8.066649094095314609 ) ) ;
#30373 = ORIENTED_EDGE ( 'NONE', *, *, #4807, .F. ) ;
#30374 = CARTESIAN_POINT ( 'NONE',  ( -35.00000000000000000, 0.000000000000000000, 0.000000000000000000 ) ) ;
#30375 = CARTESIAN_POINT ( 'NONE',  ( 16.45009115226408269, -34.41505313721369674, 6.130398315943972776 ) ) ;
#30376 = CARTESIAN_POINT ( 'NONE',  ( 3.940939162714027333, 6.015482101771779888, 10.38582757690980785 ) ) ;
#30377 = CIRCLE ( 'NONE', #59074, 12.18650000000000055 ) ;
#30378 = CARTESIAN_POINT ( 'NONE',  ( 47.00000000000000711, 4.705694406421931860E-17, -3.469127814946512892E-15 ) ) ;
#30379 = CARTESIAN_POINT ( 'NONE',  ( 35.00000000000000000, 8.854740511458958352, 7.717887834988148121 ) ) ;
#30380 = EDGE_CURVE ( 'NONE', #24055, #7923, #54061, .T. ) ;
#30381 = ORIENTED_EDGE ( 'NONE', *, *, #28080, .F. ) ;
#30382 = CARTESIAN_POINT ( 'NONE',  ( 2.305787727787084407, -0.1666591538752151269, -7.654065630109508689 ) ) ;
#30383 = CARTESIAN_POINT ( 'NONE',  ( 2.000000000000001776, 0.000000000000000000, 0.000000000000000000 ) ) ;
#30384 = CARTESIAN_POINT ( 'NONE',  ( 2.000000000000001776, -1.530946385938319443, -7.342084388195388556 ) ) ;
#30385 = ORIENTED_EDGE ( 'NONE', *, *, #18863, .T. ) ;
#30386 = CARTESIAN_POINT ( 'NONE',  ( 10.39737752511405056, 0.7512156450559613896, 13.48016586525701932 ) ) ;
#30387 = DIRECTION ( 'NONE',  ( -1.000000000000000000, -0.000000000000000000, 0.000000000000000000 ) ) ;
#30388 = ORIENTED_EDGE ( 'NONE', *, *, #40007, .F. ) ;
#30389 = EDGE_LOOP ( 'NONE', ( #14557, #36654, #28289, #19800 ) ) ;
#30390 = VERTEX_POINT ( 'NONE', #34426 ) ;
#30391 = ADVANCED_FACE ( 'NONE', ( #48752 ), #3204, .T. ) ;
#30392 = ORIENTED_EDGE ( 'NONE', *, *, #51147, .T. ) ;
#30393 = DIRECTION ( 'NONE',  ( 1.000000000000000000, 0.000000000000000000, -0.000000000000000000 ) ) ;
#30394 = DIRECTION ( 'NONE',  ( 1.000000000000000000, 0.000000000000000000, 0.000000000000000000 ) ) ;
#30395 = DIRECTION ( 'NONE',  ( 0.000000000000000000, 0.01356324068817998940, -0.9999080150203989437 ) ) ;
#30396 = CYLINDRICAL_SURFACE ( 'NONE', #36466, 6.936499999999988120 ) ;
#30397 = CARTESIAN_POINT ( 'NONE',  ( 22.57855258442564761, -4.427776684447072952, -11.15324139578564910 ) ) ;
#30398 = FACE_OUTER_BOUND ( 'NONE', #3768, .T. ) ;
#30399 = CARTESIAN_POINT ( 'NONE',  ( 23.19604530331957903, -4.580399580743265808, -12.70184690977379383 ) ) ;
#30401 = VERTEX_POINT ( 'NONE', #28139 ) ;
#30400 = CYLINDRICAL_SURFACE ( 'NONE', #47, 14.69297241773857188 ) ;
#30402 = CARTESIAN_POINT ( 'NONE',  ( 2.241449424704146764, -2.553400830064028071, 7.194804211893837120 ) ) ;
#30403 = EDGE_CURVE ( 'NONE', #38732, #55770, #4052, .T. ) ;
#30404 = ORIENTED_EDGE ( 'NONE', *, *, #23826, .T. ) ;
#30405 = CARTESIAN_POINT ( 'NONE',  ( 2.000000000000001776, 0.000000000000000000, 0.000000000000000000 ) ) ;
#30406 = VERTEX_POINT ( 'NONE', #54728 ) ;
#30407 = ORIENTED_EDGE ( 'NONE', *, *, #4625, .F. ) ;
#30408 = CARTESIAN_POINT ( 'NONE',  ( 0.3218525148189898544, 9.550803867331183028, -7.695007528464921087 ) ) ;
#30409 = CARTESIAN_POINT ( 'NONE',  ( 9.591596427418885185, -32.12122108032075118, 13.09346764506430283 ) ) ;
#30410 = ADVANCED_FACE ( 'NONE', ( #38769 ), #830, .T. ) ;
#30411 = CARTESIAN_POINT ( 'NONE',  ( -22.30625920655495165, -0.2529928606556531290, -3.783486345733990674 ) ) ;
#30412 = DIRECTION ( 'NONE',  ( -1.000000000000000000, 0.000000000000000000, 0.000000000000000000 ) ) ;
#30413 = AXIS2_PLACEMENT_3D ( 'NONE', #38406, #23446, #2858 ) ;
#30414 = CARTESIAN_POINT ( 'NONE',  ( -19.16415376008873750, 11.99999999999999822, -0.3279367020959012557 ) ) ;
#30415 = DIRECTION ( 'NONE',  ( 0.000000000000000000, -0.9970832820307030664, -0.07632122047557567124 ) ) ;
#30416 = ORIENTED_EDGE ( 'NONE', *, *, #11188, .F. ) ;
#30417 = AXIS2_PLACEMENT_3D ( 'NONE', #20314, #14983, #65214 ) ;
#30418 = ORIENTED_EDGE ( 'NONE', *, *, #35696, .F. ) ;
#30419 = DIRECTION ( 'NONE',  ( 1.000000000000000000, 0.000000000000000000, 0.000000000000000000 ) ) ;
#30420 = VERTEX_POINT ( 'NONE', #19133 ) ;
#30421 = ORIENTED_EDGE ( 'NONE', *, *, #28748, .T. ) ;
#30422 = CARTESIAN_POINT ( 'NONE',  ( 37.00000000000000711, -9.896810808925339487, 7.110831038798382409 ) ) ;
#30423 = CARTESIAN_POINT ( 'NONE',  ( -27.09729107899852352, -2.324833743198345015, 0.1622107421537080929 ) ) ;
#30424 = CARTESIAN_POINT ( 'NONE',  ( 35.00000000000000000, -2.527899948230725613, -12.49688848680883346 ) ) ;
#30425 = CARTESIAN_POINT ( 'NONE',  ( 16.78263030916553333, -10.48479066935623827, 5.836879698929882565 ) ) ;
#30426 = CARTESIAN_POINT ( 'NONE',  ( 2.261269890822072970, 7.639767381742371022, 0.1394916642590125211 ) ) ;
#30427 = ADVANCED_FACE ( 'NONE', ( #63684 ), #29124, .T. ) ;
#30428 = CARTESIAN_POINT ( 'NONE',  ( -8.377090426847601634, -1.945797233010116312, -11.84431829273728098 ) ) ;
#30429 = CARTESIAN_POINT ( 'NONE',  ( 27.08396654187716024, -12.95140485128378138, 3.821959039601221075 ) ) ;
#30430 = VERTEX_POINT ( 'NONE', #54404 ) ;
#30431 = ORIENTED_EDGE ( 'NONE', *, *, #1469, .F. ) ;
#30432 = CYLINDRICAL_SURFACE ( 'NONE', #4163, 12.18650000000000055 ) ;
#30433 =( LENGTH_UNIT ( ) NAMED_UNIT ( * ) SI_UNIT ( .MILLI., .METRE. ) );
#30434 = CARTESIAN_POINT ( 'NONE',  ( 2.941278708680199916, 2.226055275041868509, -5.721889327162129391 ) ) ;
#30435 = ADVANCED_FACE ( 'NONE', ( #14454 ), #40976, .F. ) ;
#30436 = CARTESIAN_POINT ( 'NONE',  ( -27.10719052120871098, -2.355164825213512003, 0.1538293304135223694 ) ) ;
#30437 = LINE ( 'NONE', #56724, #4580 ) ;
#30438 = CARTESIAN_POINT ( 'NONE',  ( 23.11736814598171108, 2.555106763338435893, -13.25897843685541844 ) ) ;
#30439 = FACE_OUTER_BOUND ( 'NONE', #12187, .T. ) ;
#30440 = CARTESIAN_POINT ( 'NONE',  ( -37.00000000000000711, 8.052525312710004712, -8.551552972816995890 ) ) ;
#30441 = EDGE_LOOP ( 'NONE', ( #3761, #36583, #65550, #55854 ) ) ;
#30442 = CARTESIAN_POINT ( 'NONE',  ( 2.835339799623985080, -0.3287452556171230889, 7.825540862019409794 ) ) ;
#30443 = CARTESIAN_POINT ( 'NONE',  ( 0.2638984909335716500, -12.02508546958695490, -2.322601104020790341 ) ) ;
#30444 = CARTESIAN_POINT ( 'NONE',  ( 15.45402751312076362, -34.86645063878552264, 6.224822664677306605 ) ) ;
#30445 = VECTOR ( 'NONE', #62877, 1000.000000000000000 ) ;
#30446 = AXIS2_PLACEMENT_3D ( 'NONE', #52890, #7324, #27610 ) ;
#30447 = CARTESIAN_POINT ( 'NONE',  ( 5.514970785353741078, 0.003415090918276187260, 0.003262412238248241138 ) ) ;
#30448 = CARTESIAN_POINT ( 'NONE',  ( 5.520433897694421610, -0.004666464468078229330, 0.01432141647227116142 ) ) ;
#30449 = EDGE_CURVE ( 'NONE', #64737, #6776, #55029, .T. ) ;
#30450 = ORIENTED_EDGE ( 'NONE', *, *, #10794, .F. ) ;
#30451 = CARTESIAN_POINT ( 'NONE',  ( -17.28371300127619037, -6.351468865812872622, -11.91715882903726076 ) ) ;
#30452 = CARTESIAN_POINT ( 'NONE',  ( 2.994568964204073591, 6.620406464816390724, 4.283796412555422428 ) ) ;
#30453 = CARTESIAN_POINT ( 'NONE',  ( 10.51584247049436449, -29.12274881419611106, -8.353506175201005135 ) ) ;
#30454 = VERTEX_POINT ( 'NONE', #28781 ) ;
#30455 = EDGE_CURVE ( 'NONE', #45140, #786, #42226, .T. ) ;
#30456 = CARTESIAN_POINT ( 'NONE',  ( 1.198791140417959200, -6.720248575442489880, 10.60778679489404652 ) ) ;
#30457 = DIRECTION ( 'NONE',  ( 0.000000000000000000, 0.6269146997507986097, 0.7790879021242506086 ) ) ;
#30458 = CARTESIAN_POINT ( 'NONE',  ( -22.29570301036918423, -1.042190670255880969, -3.588849529203750777 ) ) ;
#30460 = VERTEX_POINT ( 'NONE', #3867 ) ;
#30459 = CYLINDRICAL_SURFACE ( 'NONE', #14790, 12.74999999999999822 ) ;
#30461 = CARTESIAN_POINT ( 'NONE',  ( -27.08702828306175903, 2.226264228964708103, 0.5765135930308941115 ) ) ;
#30462 = EDGE_CURVE ( 'NONE', #5331, #59201, #9150, .T. ) ;
#30463 = CARTESIAN_POINT ( 'NONE',  ( -26.43258404273186812, -3.465947334857392370, -0.2934201954354464514 ) ) ;
#30464 = VERTEX_POINT ( 'NONE', #29430 ) ;
#30465 = CARTESIAN_POINT ( 'NONE',  ( 0.2657645697724695943, 7.755260067564157644, 9.477802844074060928 ) ) ;
#30466 = CARTESIAN_POINT ( 'NONE',  ( 2.305787727787084407, -2.461236246751023593, -7.249469779319933416 ) ) ;
#30468 = CARTESIAN_POINT ( 'NONE',  ( 23.10852454909521470, -3.964659581577253178, -11.32972118890850943 ) ) ;
#30467 =( BOUNDED_SURFACE ( )  B_SPLINE_SURFACE ( 3, 1, ( 
 ( #26020, #25349 ),
 ( #40305, #65570 ),
 ( #61253, #40974 ),
 ( #15037, #78 ) ),
 .UNSPECIFIED., .F., .F., .F. ) 
 B_SPLINE_SURFACE_WITH_KNOTS ( ( 4, 4 ),
 ( 2, 2 ),
 ( 0.000000000000000000, 1.000000000000000000 ),
 ( 0.000000000000000000, 1.000000000000000000 ),
 .UNSPECIFIED. ) 
 GEOMETRIC_REPRESENTATION_ITEM ( )  RATIONAL_B_SPLINE_SURFACE ( (
 ( 1.000000000000000000, 1.000000000000000000),
 ( 0.8716676215708681896, 0.8964445200148167814),
 ( 0.8716676215708681896, 0.8964445200148167814),
 ( 1.000000000000000000, 1.000000000000000000) ) ) 
 REPRESENTATION_ITEM ( '' )  SURFACE ( )  );
#30469 = CARTESIAN_POINT ( 'NONE',  ( 37.00000000000000711, -11.72195762423410414, -0.7536123767498126291 ) ) ;
#30470 = CARTESIAN_POINT ( 'NONE',  ( -35.00000000000000000, 11.47561260193584687, -5.556331110570288168 ) ) ;
#30471 = FACE_OUTER_BOUND ( 'NONE', #664, .T. ) ;
#30472 = CARTESIAN_POINT ( 'NONE',  ( 0.3474126878361853965, 11.44231427242455723, -4.439989671676105587 ) ) ;
#30473 = ORIENTED_EDGE ( 'NONE', *, *, #62763, .T. ) ;
#30474 = CARTESIAN_POINT ( 'NONE',  ( -10.90165637462999726, -7.508992741355383416, 25.00000000000000000 ) ) ;
#30475 = ORIENTED_EDGE ( 'NONE', *, *, #35946, .F. ) ;
#30476 = DIRECTION ( 'NONE',  ( -1.000000000000000000, 0.000000000000000000, 0.000000000000000000 ) ) ;
#30477 = CARTESIAN_POINT ( 'NONE',  ( 2.000000000000001776, 0.3246585432987117992, -6.805031400696120336 ) ) ;
#30478 = ADVANCED_FACE ( 'NONE', ( #44384 ), #43405, .T. ) ;
#30479 = CARTESIAN_POINT ( 'NONE',  ( 0.3665391374699467075, 3.952034409876297172, 11.62960183138728532 ) ) ;
#30480 = ORIENTED_EDGE ( 'NONE', *, *, #17954, .F. ) ;
#30481 = DIRECTION ( 'NONE',  ( -1.000000000000000000, 0.000000000000000000, 0.000000000000000000 ) ) ;
#30482 = CARTESIAN_POINT ( 'NONE',  ( -35.00000000000000000, 8.017674001891920810, -9.913596905230031453 ) ) ;
#30483 = AXIS2_PLACEMENT_3D ( 'NONE', #24370, #30355, #25357 ) ;
#30484 = CARTESIAN_POINT ( 'NONE',  ( -22.27719412087655471, -1.358750377066196835, 3.421752300520410905 ) ) ;
#30485 = ORIENTED_EDGE ( 'NONE', *, *, #41950, .F. ) ;
#30486 = ORIENTED_EDGE ( 'NONE', *, *, #36412, .T. ) ;
#30487 = CARTESIAN_POINT ( 'NONE',  ( 2.000000000000001776, -3.152010634611648321, -6.039758645301327000 ) ) ;
#30488 = ORIENTED_EDGE ( 'NONE', *, *, #1284, .F. ) ;
#30489 = CARTESIAN_POINT ( 'NONE',  ( 0.000000000000000000, 1.956810415765184219, 6.654767106875543625 ) ) ;
#30490 = AXIS2_PLACEMENT_3D ( 'NONE', #4259, #33202, #18601 ) ;
#30491 = DIRECTION ( 'NONE',  ( 1.000000000000000000, 0.000000000000000000, 0.000000000000000000 ) ) ;
#30492 = CARTESIAN_POINT ( 'NONE',  ( 5.515188684475870851, -0.0003622115669627103194, -0.005339000964282158458 ) ) ;
#30493 = FACE_OUTER_BOUND ( 'NONE', #18726, .T. ) ;
#30494 = DIRECTION ( 'NONE',  ( -1.000000000000000000, 0.000000000000000000, 0.000000000000000000 ) ) ;
#30495 = DIRECTION ( 'NONE',  ( 0.4622435816439414147, -0.000000000000000000, 0.8867529933577789070 ) ) ;
#30496 = AXIS2_PLACEMENT_3D ( 'NONE', #46434, #62692, #11194 ) ;
#30497 = LINE ( 'NONE', #5243, #51405 ) ;
#30498 = ORIENTED_EDGE ( 'NONE', *, *, #8853, .F. ) ;
#30499 = DIRECTION ( 'NONE',  ( -1.000000000000000000, 0.000000000000000000, -0.000000000000000000 ) ) ;
#30500 = DIRECTION ( 'NONE',  ( 0.000000000000000000, -0.8696919319575131535, -0.4935949184179356797 ) ) ;
#30501 = CARTESIAN_POINT ( 'NONE',  ( 2.241509619876138171, 5.823675573301077435, 4.936617871859525053 ) ) ;
#30502 = CARTESIAN_POINT ( 'NONE',  ( 12.70623083740922432, 11.80103865657056872, -6.559203751279317096 ) ) ;
#30503 = DIRECTION ( 'NONE',  ( -1.000000000000000000, 0.000000000000000000, 0.000000000000000000 ) ) ;
#30504 = LINE ( 'NONE', #9552, #27675 ) ;
#30505 = CARTESIAN_POINT ( 'NONE',  ( 35.00000000000000000, -6.891188680298889757, -9.512294188640879611 ) ) ;
#30506 = LINE ( 'NONE', #39838, #51238 ) ;
#30507 = EDGE_CURVE ( 'NONE', #50026, #27033, #9302, .T. ) ;
#30508 = ORIENTED_EDGE ( 'NONE', *, *, #16371, .T. ) ;
#30509 = CARTESIAN_POINT ( 'NONE',  ( -37.00000000000000711, -12.63095688309030429, 1.738225594539952068 ) ) ;
#30510 = VERTEX_POINT ( 'NONE', #59067 ) ;
#30511 = CARTESIAN_POINT ( 'NONE',  ( -3.303901569720309350, -7.697936092459741531, 9.214473394900021930 ) ) ;
#30512 = CARTESIAN_POINT ( 'NONE',  ( 0.2651627682582886614, 0.08809604936506143513, 12.24583720278848631 ) ) ;
#30513 = CARTESIAN_POINT ( 'NONE',  ( 5.516018279890452902, -0.006286471671801945743, 0.002527316374434286465 ) ) ;
#30514 = CARTESIAN_POINT ( 'NONE',  ( 2.524535260912230683, -7.646662375930282529, -1.123794384999050378 ) ) ;
#30515 = CARTESIAN_POINT ( 'NONE',  ( 2.269879328256533491, 2.474479066008462347, -7.232310762824027073 ) ) ;
#30516 = ORIENTED_EDGE ( 'NONE', *, *, #32550, .F. ) ;
#30517 = CARTESIAN_POINT ( 'NONE',  ( -19.56743653832046803, -28.99999999999999645, -4.999999999999997335 ) ) ;
#30518 = CARTESIAN_POINT ( 'NONE',  ( -30.18541646480307250, -1.815008380980587699, -11.86874821329540630 ) ) ;
#30519 = CARTESIAN_POINT ( 'NONE',  ( 1.287602823386676532, -12.47973441446164955, 1.639728374786187715 ) ) ;
#30520 = CARTESIAN_POINT ( 'NONE',  ( 2.241352910868909643, -6.569501556381414531, -3.889181972941518683 ) ) ;
#30521 = VECTOR ( 'NONE', #30976, 1000.000000000000114 ) ;
#30522 = EDGE_CURVE ( 'NONE', #56863, #63134, #31610, .T. ) ;
#30523 = CARTESIAN_POINT ( 'NONE',  ( -18.47557885490082796, -4.422014522762156119, 11.15615431079476672 ) ) ;
#30524 = CARTESIAN_POINT ( 'NONE',  ( -35.00000000000000000, 10.49626516989271074, 7.238157050195666464 ) ) ;
#30525 = ORIENTED_EDGE ( 'NONE', *, *, #23684, .T. ) ;
#30526 = EDGE_CURVE ( 'NONE', #27983, #60081, #11449, .T. ) ;
#30527 = CARTESIAN_POINT ( 'NONE',  ( -37.00000000000000711, -9.896810808925444292, 7.110831038798244741 ) ) ;
#30528 = ORIENTED_EDGE ( 'NONE', *, *, #15773, .F. ) ;
#30529 = EDGE_CURVE ( 'NONE', #50166, #9014, #40101, .T. ) ;
#30530 = DIRECTION ( 'NONE',  ( 0.000000000000000000, -0.01356324068817998940, 0.9999080150203990547 ) ) ;
#30531 = CARTESIAN_POINT ( 'NONE',  ( -26.74023318801843274, -3.035730054944082212, 1.425982498898165751 ) ) ;
#30532 = AXIS2_PLACEMENT_3D ( 'NONE', #20459, #40735, #61024 ) ;
#30533 = CARTESIAN_POINT ( 'NONE',  ( -22.27218376572352554, -0.9890213205919480277, -3.547715993389686240 ) ) ;
#30534 = CARTESIAN_POINT ( 'NONE',  ( 0.3278977287071272451, -11.60975784853194348, 3.961557589215566999 ) ) ;
#30535 = ORIENTED_EDGE ( 'NONE', *, *, #25616, .F. ) ;
#30536 = CIRCLE ( 'NONE', #42209, 2.899999999999997247 ) ;
#30538 = VERTEX_POINT ( 'NONE', #30089 ) ;
#30537 = EDGE_CURVE ( 'NONE', #2479, #58998, #29746, .T. ) ;
#30539 = CYLINDRICAL_SURFACE ( 'NONE', #5345, 2.899999999999994582 ) ;
#30540 = ORIENTED_EDGE ( 'NONE', *, *, #65162, .T. ) ;
#30541 = DIRECTION ( 'NONE',  ( 0.000000000000000000, -0.01356324068817998940, 0.9999080150203990547 ) ) ;
#30542 = CARTESIAN_POINT ( 'NONE',  ( 8.621148270653568702, 25.00000000000000000, -5.251012286260225537 ) ) ;
#30543 = CARTESIAN_POINT ( 'NONE',  ( -22.27706485742869091, -3.547445275915918295, -0.9832726768967802178 ) ) ;
#30544 = CARTESIAN_POINT ( 'NONE',  ( 0.9296196016816602459, 9.278306863859487663, 8.327938962579152005 ) ) ;
#30545 = CARTESIAN_POINT ( 'NONE',  ( 2.305787727787083519, 6.545285700970583598, -3.971363876083895850 ) ) ;
#30546 = EDGE_CURVE ( 'NONE', #48610, #18591, #41046, .T. ) ;
#30547 = FACE_OUTER_BOUND ( 'NONE', #14398, .T. ) ;
#30548 = CARTESIAN_POINT ( 'NONE',  ( 1.198791140419050105, -12.54673713002894075, -0.5160125886328322808 ) ) ;
#30549 = ORIENTED_EDGE ( 'NONE', *, *, #35495, .T. ) ;
#30550 = CARTESIAN_POINT ( 'NONE',  ( 1.287602823386676310, -11.16629420487802449, 5.809161206980312464 ) ) ;
#30551 = ORIENTED_EDGE ( 'NONE', *, *, #63178, .T. ) ;
#30552 = CARTESIAN_POINT ( 'NONE',  ( 0.6473888112830232799, -2.472751636945289100, -12.12394591856681103 ) ) ;
#30553 = CARTESIAN_POINT ( 'NONE',  ( -27.09861164373112530, 1.936722219469636963, -1.303360234155686026 ) ) ;
#30554 = ORIENTED_EDGE ( 'NONE', *, *, #25284, .T. ) ;
#30555 = EDGE_CURVE ( 'NONE', #32620, #2528, #45065, .T. ) ;
#30556 = FACE_BOUND ( 'NONE', #38319, .T. ) ;
#30557 = ORIENTED_EDGE ( 'NONE', *, *, #44950, .T. ) ;
#30558 = DIRECTION ( 'NONE',  ( -1.000000000000000000, 0.000000000000000000, 0.000000000000000000 ) ) ;
#30559 = CARTESIAN_POINT ( 'NONE',  ( 6.776769869547749181, -5.711596899239616221, -12.23794304267072874 ) ) ;
#30560 = DIRECTION ( 'NONE',  ( 0.000000000000000000, -0.5987040770935562195, 0.8009703041134252910 ) ) ;
#30561 = CARTESIAN_POINT ( 'NONE',  ( 5.258427716898767201, -10.28439498637095006, 6.186120577954387301 ) ) ;
#30562 = EDGE_LOOP ( 'NONE', ( #5720, #6278, #25586, #17008 ) ) ;
#30564 = EDGE_CURVE ( 'NONE', #39365, #28622, #23665, .T. ) ;
#30563 = ORIENTED_EDGE ( 'NONE', *, *, #5702, .F. ) ;
#30565 = CARTESIAN_POINT ( 'NONE',  ( 2.994568964204205930, -7.020079750321915668, 3.591541975631944883 ) ) ;
#30566 = ORIENTED_EDGE ( 'NONE', *, *, #15979, .T. ) ;
#30567 = DIRECTION ( 'NONE',  ( 1.000000000000000000, 0.000000000000000000, 0.000000000000000000 ) ) ;
#30568 = ORIENTED_EDGE ( 'NONE', *, *, #51138, .T. ) ;
#30569 = ORIENTED_EDGE ( 'NONE', *, *, #46763, .T. ) ;
#30570 = ORIENTED_EDGE ( 'NONE', *, *, #36785, .T. ) ;
#30571 = CARTESIAN_POINT ( 'NONE',  ( 2.000000000000001776, 6.750946897830712778, 1.593658756657066355 ) ) ;
#30572 = CARTESIAN_POINT ( 'NONE',  ( 15.64771680208055393, -28.15000396670248506, 10.66347899870800298 ) ) ;
#30573 = DIRECTION ( 'NONE',  ( 0.000000000000000000, 0.01356324068817998940, -0.9999080150203990547 ) ) ;
#30574 = DIRECTION ( 'NONE',  ( 1.000000000000000000, 0.000000000000000000, -0.000000000000000000 ) ) ;
#30575 = FACE_OUTER_BOUND ( 'NONE', #169, .T. ) ;
#30576 = ORIENTED_EDGE ( 'NONE', *, *, #35237, .T. ) ;
#30577 = CARTESIAN_POINT ( 'NONE',  ( 0.000000000000000000, 0.4129979343797385294, 6.800241778083691457 ) ) ;
#30578 = EDGE_LOOP ( 'NONE', ( #12665, #53886, #25321, #65594 ) ) ;
#30579 = CYLINDRICAL_SURFACE ( 'NONE', #47631, 6.936499999999988120 ) ;
#30580 = CARTESIAN_POINT ( 'NONE',  ( 35.00000000000000000, 4.705694406421931860E-17, -3.469127814946512892E-15 ) ) ;
#30581 = AXIS2_PLACEMENT_3D ( 'NONE', #45311, #25041, #9385 ) ;
#30582 = ORIENTED_EDGE ( 'NONE', *, *, #29378, .F. ) ;
#30583 = LINE ( 'NONE', #50888, #10521 ) ;
#30584 = CARTESIAN_POINT ( 'NONE',  ( 29.10170639864063702, 8.929942550509162302, 8.028710125001698117 ) ) ;
#30585 = DIRECTION ( 'NONE',  ( 0.000000000000000000, 0.000000000000000000, 1.000000000000000000 ) ) ;
#30586 = AXIS2_PLACEMENT_3D ( 'NONE', #35970, #6085, #53176 ) ;
#30587 = EDGE_CURVE ( 'NONE', #42316, #11282, #36930, .T. ) ;
#30588 = EDGE_CURVE ( 'NONE', #63500, #56480, #41365, .T. ) ;
#30589 = ORIENTED_EDGE ( 'NONE', *, *, #35288, .T. ) ;
#30590 = FACE_OUTER_BOUND ( 'NONE', #57972, .T. ) ;
#30591 = VERTEX_POINT ( 'NONE', #36394 ) ;
#30592 = CARTESIAN_POINT ( 'NONE',  ( -39.82259759989633352, -25.85751090193130253, -4.500000000000000000 ) ) ;
#30593 = CARTESIAN_POINT ( 'NONE',  ( -17.14901781563218819, -29.51442629269803675, 9.398967198486925412 ) ) ;
#30594 = CYLINDRICAL_SURFACE ( 'NONE', #62746, 4.999999999999999112 ) ;
#30595 = DIRECTION ( 'NONE',  ( -0.3939253465568943180, -0.1500280335741535909, 0.9068155327749427563 ) ) ;
#30596 = EDGE_LOOP ( 'NONE', ( #52146, #16984, #19927, #5756 ) ) ;
#30597 = EDGE_CURVE ( 'NONE', #65063, #32207, #30731, .T. ) ;
#30598 = LINE ( 'NONE', #697, #2739 ) ;
#30599 = DIRECTION ( 'NONE',  ( 1.000000000000000000, 0.000000000000000000, 0.000000000000000000 ) ) ;
#30600 = DIRECTION ( 'NONE',  ( 0.000000000000000000, 0.01356324068817998940, -0.9999080150203990547 ) ) ;
#30601 = CARTESIAN_POINT ( 'NONE',  ( 22.27688490018784506, -12.54606834907711210, -4.987630095507642913 ) ) ;
#30602 = EDGE_CURVE ( 'NONE', #58290, #26820, #15116, .T. ) ;
#30603 = CARTESIAN_POINT ( 'NONE',  ( 5.536195898058073439, -0.006672323185952951791, -0.005266167600748141754 ) ) ;
#30604 = CARTESIAN_POINT ( 'NONE',  ( 2.241352910868908754, 2.532612177304442991, 7.202080440908749992 ) ) ;
#30605 = EDGE_CURVE ( 'NONE', #21169, #20211, #19801, .T. ) ;
#30606 = CARTESIAN_POINT ( 'NONE',  ( 2.305787727787084407, -5.047606869483094449, 5.756228004061441084 ) ) ;
#30607 = CARTESIAN_POINT ( 'NONE',  ( 0.9232058338315058954, 9.306586124266710058, -8.301689855530073103 ) ) ;
#30608 = CARTESIAN_POINT ( 'NONE',  ( 2.255723233588950993, 0.1321982600348293457, -7.638048593862501789 ) ) ;
#30609 = AXIS2_PLACEMENT_3D ( 'NONE', #901, #6888, #1892 ) ;
#30610 = ORIENTED_EDGE ( 'NONE', *, *, #816, .T. ) ;
#30611 = CIRCLE ( 'NONE', #52941, 7.499999999999988454 ) ;
#30612 = ORIENTED_EDGE ( 'NONE', *, *, #18300, .T. ) ;
#30613 = DIRECTION ( 'NONE',  ( -1.000000000000000000, 0.000000000000000000, 0.000000000000000000 ) ) ;
#30614 = CARTESIAN_POINT ( 'NONE',  ( 48.99862351417106510, -0.2022747408561471338, -1.593306619454940787 ) ) ;
#30615 = CARTESIAN_POINT ( 'NONE',  ( 0.3675815128205894289, -12.13672785388551389, 1.872154644482044938 ) ) ;
#30616 = ADVANCED_FACE ( 'NONE', ( #60344 ), #14769, .T. ) ;
#30617 = CARTESIAN_POINT ( 'NONE',  ( 2.241526690369557429, 3.832206765347585975, 6.602966219605648668 ) ) ;
#30618 = ORIENTED_EDGE ( 'NONE', *, *, #7823, .F. ) ;
#30619 = ADVANCED_FACE ( 'NONE', ( #51043 ), #10140, .T. ) ;
#30620 = ORIENTED_EDGE ( 'NONE', *, *, #54370, .T. ) ;
#30621 = VECTOR ( 'NONE', #59466, 999.9999999999998863 ) ;
#30622 = ORIENTED_EDGE ( 'NONE', *, *, #24013, .T. ) ;
#30623 = CARTESIAN_POINT ( 'NONE',  ( 5.515539859299206427, 0.001241880655086934895, 0.005924322247675113152 ) ) ;
#30624 = EDGE_CURVE ( 'NONE', #7430, #25248, #6207, .T. ) ;
#30625 = CARTESIAN_POINT ( 'NONE',  ( 37.00000000000000711, -1.286231064351218478, 12.68495603654572612 ) ) ;
#30626 = ORIENTED_EDGE ( 'NONE', *, *, #39526, .T. ) ;
#30627 = EDGE_CURVE ( 'NONE', #27370, #1032, #2992, .T. ) ;
#30628 = DIRECTION ( 'NONE',  ( 0.000000000000000000, 0.01356324068817992175, -0.9999080150203990547 ) ) ;
#30629 = CARTESIAN_POINT ( 'NONE',  ( 2.556980015513758087, -2.429125721802469329, 7.348538402679460013 ) ) ;
#30630 = ORIENTED_EDGE ( 'NONE', *, *, #54628, .F. ) ;
#30631 = DIRECTION ( 'NONE',  ( 0.8751623310228197061, 0.000000000000000000, -0.4838294062566934617 ) ) ;
#30632 = CARTESIAN_POINT ( 'NONE',  ( 7.310206959903694290, -27.15910349781274391, -15.27822828334930705 ) ) ;
#30633 = CARTESIAN_POINT ( 'NONE',  ( 35.00000000000000000, 10.30098186818249673, -5.644643009979106729 ) ) ;
#30634 = ORIENTED_EDGE ( 'NONE', *, *, #36881, .F. ) ;
#30635 = EDGE_CURVE ( 'NONE', #40530, #33180, #58525, .T. ) ;
#30636 = DIRECTION ( 'NONE',  ( 0.000000000000000000, 0.01356324068817992175, -0.9999080150203990547 ) ) ;
#30637 = ORIENTED_EDGE ( 'NONE', *, *, #61719, .F. ) ;
#30638 = FACE_OUTER_BOUND ( 'NONE', #59299, .T. ) ;
#30639 = ORIENTED_EDGE ( 'NONE', *, *, #34886, .T. ) ;
#30640 = DIRECTION ( 'NONE',  ( 0.000000000000000000, -0.6051742151937717917, 0.7960930657056387583 ) ) ;
#30641 = DIRECTION ( 'NONE',  ( 0.000000000000000000, 0.000000000000000000, 1.000000000000000000 ) ) ;
#30642 = CARTESIAN_POINT ( 'NONE',  ( -22.46509356695213455, -3.157489876851681032, -2.840174833751851313 ) ) ;
#30644 = DIRECTION ( 'NONE',  ( 0.000000000000000000, -0.01356324068817991828, 0.9999080150203990547 ) ) ;
#30643 = CIRCLE ( 'NONE', #51901, 12.73084802173761787 ) ;
#30645 = CARTESIAN_POINT ( 'NONE',  ( 2.241352910868910531, 5.794346703933913822, -4.970878533273699773 ) ) ;
#30646 = CARTESIAN_POINT ( 'NONE',  ( -27.08423805673873375, 2.229265646063317341, -0.5302040644010300730 ) ) ;
#30647 = DIRECTION ( 'NONE',  ( -1.000000000000000000, 0.000000000000000000, 0.000000000000000000 ) ) ;
#30649 = ORIENTED_EDGE ( 'NONE', *, *, #38897, .T. ) ;
#30648 = CARTESIAN_POINT ( 'NONE',  ( 6.812204945636112896, -4.138731716409435712, 12.84993773446340803 ) ) ;
#30650 = DIRECTION ( 'NONE',  ( 0.9606638835031803270, 0.1629100154396158073, 0.2249116044183853413 ) ) ;
#30651 = ORIENTED_EDGE ( 'NONE', *, *, #58503, .F. ) ;
#30652 = VECTOR ( 'NONE', #28706, 1000.000000000000000 ) ;
#30653 = CARTESIAN_POINT ( 'NONE',  ( 0.3218525148189809726, -4.423735011438902909, 11.43947393562874915 ) ) ;
#30654 = ORIENTED_EDGE ( 'NONE', *, *, #63208, .F. ) ;
#30655 = DIRECTION ( 'NONE',  ( 0.000000000000000000, 0.01356324068818000848, -0.9999080150203990547 ) ) ;
#30656 =( REPRESENTATION_RELATIONSHIP ('NONE','NONE', #63658, #39018 ) REPRESENTATION_RELATIONSHIP_WITH_TRANSFORMATION ( #27788 )SHAPE_REPRESENTATION_RELATIONSHIP( ) );
#30657 = EDGE_LOOP ( 'NONE', ( #49228, #59485 ) ) ;
#30658 = CARTESIAN_POINT ( 'NONE',  ( 0.3474126878361804005, 8.085727498271769065, 9.233692382639393514 ) ) ;
#30659 = LINE ( 'NONE', #50971, #2178 ) ;
#30660 = CARTESIAN_POINT ( 'NONE',  ( -27.08430792439081003, -2.215465963318195008, 0.5856059198894537632 ) ) ;
#30661 = LINE ( 'NONE', #29679, #32701 ) ;
#30662 = CYLINDRICAL_SURFACE ( 'NONE', #32987, 2.899999999999994582 ) ;
#30663 = EDGE_CURVE ( 'NONE', #44780, #65264, #42238, .T. ) ;
#30664 = VERTEX_POINT ( 'NONE', #42664 ) ;
#30665 = CARTESIAN_POINT ( 'NONE',  ( -18.11037611196539387, -4.786480602738535595, -11.00804596661986068 ) ) ;
#30666 = EDGE_CURVE ( 'NONE', #13558, #1201, #44385, .T. ) ;
#30667 = AXIS2_PLACEMENT_3D ( 'NONE', #14407, #34684, #24736 ) ;
#30668 =( BOUNDED_CURVE ( )  B_SPLINE_CURVE ( 3, ( #32357, #2458, #57661, #52669 ),
 .UNSPECIFIED., .F., .F. ) 
 B_SPLINE_CURVE_WITH_KNOTS ( ( 4, 4 ),
 ( 4.675538416354898530, 4.712388980384690562 ),
 .UNSPECIFIED. ) 
 CURVE ( )  GEOMETRIC_REPRESENTATION_ITEM ( )  RATIONAL_B_SPLINE_CURVE ( ( 1.000000000000000000, 0.9998868395290251287, 0.9998868395290251287, 1.000000000000000000 ) ) 
 REPRESENTATION_ITEM ( '' )  );
#30669 = ORIENTED_EDGE ( 'NONE', *, *, #37443, .F. ) ;
#30670 = CARTESIAN_POINT ( 'NONE',  ( 0.000000000000000000, 6.201547234537035713, 2.820401998297911383 ) ) ;
#30671 = CARTESIAN_POINT ( 'NONE',  ( 2.000000000000001776, -6.470132594555779271, -2.133363481234176628 ) ) ;
#30672 = VECTOR ( 'NONE', #64128, 1000.000000000000000 ) ;
#30673 = CARTESIAN_POINT ( 'NONE',  ( 1.000000000000000888, 0.8935325819928834346, 7.446583077151348817 ) ) ;
#30674 = ORIENTED_EDGE ( 'NONE', *, *, #45102, .T. ) ;
#30675 = EDGE_CURVE ( 'NONE', #42736, #57376, #43349, .T. ) ;
#30676 = CARTESIAN_POINT ( 'NONE',  ( 35.00000000000000000, 11.96656215839374759, 4.400442035670817376 ) ) ;
#30677 = CARTESIAN_POINT ( 'NONE',  ( 49.99855491382518125, -0.0002949769214594301510, -1.660073069598956064 ) ) ;
#30678 = CARTESIAN_POINT ( 'NONE',  ( 25.00000000000000355, -28.99999999999999645, 1.530808498934191521E-15 ) ) ;
#30679 = CARTESIAN_POINT ( 'NONE',  ( 0.3278977287071248026, -5.917385921415723615, -10.74546228373873191 ) ) ;
#30681 = ORIENTED_EDGE ( 'NONE', *, *, #50744, .T. ) ;
#30680 = ADVANCED_FACE ( 'NONE', ( #36719 ), #6468, .T. ) ;
#30682 = CARTESIAN_POINT ( 'NONE',  ( 35.00000000000000000, 11.70009620280413110, 1.039216533672774112 ) ) ;
#30683 = CARTESIAN_POINT ( 'NONE',  ( -37.00000000000000711, 2.346765782874606465, -11.95840593935198903 ) ) ;
#30684 = CARTESIAN_POINT ( 'NONE',  ( -27.04788180060269198, -1.844972430941754782, 2.650714769830304185 ) ) ;
#30685 = ADVANCED_FACE ( 'NONE', ( #11760 ), #41213, .T. ) ;
#30686 = AXIS2_PLACEMENT_3D ( 'NONE', #32882, #32241, #32551 ) ;
#30687 = DIRECTION ( 'NONE',  ( 1.000000000000000000, 0.000000000000000000, 0.000000000000000000 ) ) ;
#30688 = DIRECTION ( 'NONE',  ( 1.000000000000000000, 0.000000000000000000, -0.000000000000000000 ) ) ;
#30689 = ORIENTED_EDGE ( 'NONE', *, *, #58148, .T. ) ;
#30690 = CARTESIAN_POINT ( 'NONE',  ( -37.00000000000000711, -11.73555825188280011, 4.983891302653540301 ) ) ;
#30691 = LINE ( 'NONE', #51671, #42743 ) ;
#30692 = CARTESIAN_POINT ( 'NONE',  ( 35.00000000000000000, 11.74614673114903773, 0.01609748574448878478 ) ) ;
#30693 = ORIENTED_EDGE ( 'NONE', *, *, #44218, .T. ) ;
#30694 = CARTESIAN_POINT ( 'NONE',  ( 2.242418902651940105, -6.561482094363274342, 3.903399295463823915 ) ) ;
#30695 = CARTESIAN_POINT ( 'NONE',  ( -27.45775109278351067, -8.499184579339635448, -8.471355351200609007 ) ) ;
#30696 = EDGE_LOOP ( 'NONE', ( #43815, #13638, #32107, #32788 ) ) ;
#30697 = ORIENTED_EDGE ( 'NONE', *, *, #39857, .F. ) ;
#30698 = EDGE_LOOP ( 'NONE', ( #47745, #49554, #53595, #60828 ) ) ;
#30699 = AXIS2_PLACEMENT_3D ( 'NONE', #11445, #37039, #16113 ) ;
#30700 = EDGE_CURVE ( 'NONE', #58005, #24593, #23526, .T. ) ;
#30701 = CIRCLE ( 'NONE', #2057, 5.000000000000000888 ) ;
#30702 = ORIENTED_EDGE ( 'NONE', *, *, #53555, .T. ) ;
#30703 = EDGE_CURVE ( 'NONE', #38516, #18227, #22754, .T. ) ;
#30704 = DIRECTION ( 'NONE',  ( 0.9582930651793754029, 0.2370079598497654427, -0.1596922922278005419 ) ) ;
#30705 = DIRECTION ( 'NONE',  ( -1.000000000000000000, 0.000000000000000000, 0.000000000000000000 ) ) ;
#30706 = AXIS2_PLACEMENT_3D ( 'NONE', #28576, #48879, #45181 ) ;
#30707 = DIRECTION ( 'NONE',  ( -1.000000000000000000, 0.000000000000000000, 0.000000000000000000 ) ) ;
#30708 = CARTESIAN_POINT ( 'NONE',  ( 0.2652384529303124516, 4.126283314267730873, -11.53005674806958503 ) ) ;
#30709 = CARTESIAN_POINT ( 'NONE',  ( 0.3040950598368144520, 3.956873563689532247, 11.60568999039896454 ) ) ;
#30710 = CARTESIAN_POINT ( 'NONE',  ( 0.3675815128205894289, -10.76447900494936327, -5.910255304480558358 ) ) ;
#30711 = CARTESIAN_POINT ( 'NONE',  ( 12.10998784662220729, -10.46621227226782835, -8.526922110106905706 ) ) ;
#30713 = ORIENTED_EDGE ( 'NONE', *, *, #56288, .T. ) ;
#30712 = CARTESIAN_POINT ( 'NONE',  ( 5.516018279890452902, 0.002104829434640673614, -0.006440244342253036158 ) ) ;
#30714 = EDGE_CURVE ( 'NONE', #12400, #2234, #25273, .T. ) ;
#30715 = CARTESIAN_POINT ( 'NONE',  ( 2.305787727787083519, 1.164987321564732392, 7.566723232958076473 ) ) ;
#30716 = ORIENTED_EDGE ( 'NONE', *, *, #170, .F. ) ;
#30717 = CARTESIAN_POINT ( 'NONE',  ( 2.241352910868909643, 7.503490710578251566, -1.407733736974789762 ) ) ;
#30718 = VERTEX_POINT ( 'NONE', #16759 ) ;
#30719 = CIRCLE ( 'NONE', #3139, 16.73205080756888563 ) ;
#30720 = ORIENTED_EDGE ( 'NONE', *, *, #20426, .F. ) ;
#30721 = CARTESIAN_POINT ( 'NONE',  ( -37.00000000000000711, 0.000000000000000000, 0.000000000000000000 ) ) ;
#30722 = CARTESIAN_POINT ( 'NONE',  ( 12.39041149895467875, -29.91764912108355290, 8.475516454291387447 ) ) ;
#30723 = FACE_OUTER_BOUND ( 'NONE', #36201, .T. ) ;
#30724 = CARTESIAN_POINT ( 'NONE',  ( 35.00000000000000000, 4.705694406421931860E-17, -3.469127814946512892E-15 ) ) ;
#30725 = ADVANCED_FACE ( 'NONE', ( #57019 ), #46696, .F. ) ;
#30726 = CARTESIAN_POINT ( 'NONE',  ( 0.6511581176957887962, -2.473966499148019693, 12.12498040206527072 ) ) ;
#30727 = CARTESIAN_POINT ( 'NONE',  ( -27.08429572838383947, 1.859677275556428810, -1.338867938658195200 ) ) ;
#30728 = AXIS2_PLACEMENT_3D ( 'NONE', #24631, #13987, #34594 ) ;
#30729 = ORIENTED_EDGE ( 'NONE', *, *, #22453, .T. ) ;
#30730 = ORIENTED_EDGE ( 'NONE', *, *, #42693, .T. ) ;
#30731 = LINE ( 'NONE', #9802, #27402 ) ;
#30732 = ORIENTED_EDGE ( 'NONE', *, *, #53413, .F. ) ;
#30733 = ORIENTED_EDGE ( 'NONE', *, *, #16731, .T. ) ;
#30734 = LINE ( 'NONE', #60348, #17953 ) ;
#30735 = DIRECTION ( 'NONE',  ( 0.000000000000000000, 0.01356324068817998940, -0.9999080150203990547 ) ) ;
#30736 = CARTESIAN_POINT ( 'NONE',  ( 2.241451721903216399, 1.265761656830201920, 7.528807736569452125 ) ) ;
#30737 = CARTESIAN_POINT ( 'NONE',  ( 0.9232167919969109793, -12.19756235544080170, 2.570564963838106731 ) ) ;
#30738 = DIRECTION ( 'NONE',  ( -1.000000000000000000, 0.000000000000000000, 0.000000000000000000 ) ) ;
#30739 = DIRECTION ( 'NONE',  ( -1.000000000000000000, 0.000000000000000000, 0.000000000000000000 ) ) ;
#30740 = CIRCLE ( 'NONE', #12694, 4.999999999999999112 ) ;
#30741 = EDGE_CURVE ( 'NONE', #19851, #34326, #37367, .T. ) ;
#30742 = ORIENTED_EDGE ( 'NONE', *, *, #7007, .F. ) ;
#30743 = AXIS2_PLACEMENT_3D ( 'NONE', #57941, #12354, #22688 ) ;
#30744 = ORIENTED_EDGE ( 'NONE', *, *, #55133, .T. ) ;
#30745 = CARTESIAN_POINT ( 'NONE',  ( -35.00000000000000000, 9.063649021439076137, -8.146229107149299153 ) ) ;
#30746 = CARTESIAN_POINT ( 'NONE',  ( 2.665405856346787949, 9.505137710817303187, -1.089747929268594095 ) ) ;
#30747 = VECTOR ( 'NONE', #42064, 1000.000000000000000 ) ;
#30748 = CARTESIAN_POINT ( 'NONE',  ( 4.190943541829291519, -10.32976040564048681, 6.108679903397304045 ) ) ;
#30749 = CARTESIAN_POINT ( 'NONE',  ( -35.00000000000000000, -10.42955799785324444, 6.303578524886909840 ) ) ;
#30750 = VECTOR ( 'NONE', #3835, 1000.000000000000000 ) ;
#30751 = CARTESIAN_POINT ( 'NONE',  ( -37.00000000000000711, 0.000000000000000000, 0.000000000000000000 ) ) ;
#30752 = DIRECTION ( 'NONE',  ( 0.000000000000000000, 0.000000000000000000, 1.000000000000000000 ) ) ;
#30753 = CARTESIAN_POINT ( 'NONE',  ( 2.969415267404188707, 6.276215141898544125, 4.760005747566447454 ) ) ;
#30754 = EDGE_CURVE ( 'NONE', #63926, #30777, #37708, .T. ) ;
#30755 = ORIENTED_EDGE ( 'NONE', *, *, #15796, .F. ) ;
#30756 = CARTESIAN_POINT ( 'NONE',  ( 0.2651627923886300531, 10.56116046379974271, 6.199207987242133733 ) ) ;
#30757 = CARTESIAN_POINT ( 'NONE',  ( 3.092491956585992519, 0.9322768171840450924, -7.863103788722456855 ) ) ;
#30758 = CARTESIAN_POINT ( 'NONE',  ( -37.00000000000000711, 0.000000000000000000, 0.000000000000000000 ) ) ;
#30759 = VECTOR ( 'NONE', #62454, 1000.000000000000000 ) ;
#30760 = EDGE_CURVE ( 'NONE', #39372, #47492, #52023, .T. ) ;
#30761 = CARTESIAN_POINT ( 'NONE',  ( 2.000000000000001776, 6.935703035393450122, 0.1051458740707594125 ) ) ;
#30762 = CARTESIAN_POINT ( 'NONE',  ( 37.00000000000000711, 12.73293890771483916, 0.6593684648219071409 ) ) ;
#30763 = ORIENTED_EDGE ( 'NONE', *, *, #15701, .T. ) ;
#30764 = CARTESIAN_POINT ( 'NONE',  ( 2.241528039335008327, -3.803597072146486457, -6.619488482362972270 ) ) ;
#30765 = CARTESIAN_POINT ( 'NONE',  ( 37.00000000000000711, -0.9416912585475287756, -12.71517666308947625 ) ) ;
#30766 = CARTESIAN_POINT ( 'NONE',  ( 2.251139882113959878, 1.203816215709547111, 7.542197031254625372 ) ) ;
#30767 = ORIENTED_EDGE ( 'NONE', *, *, #4760, .T. ) ;
#30768 = CYLINDRICAL_SURFACE ( 'NONE', #53603, 6.936499999999988120 ) ;
#30769 = CARTESIAN_POINT ( 'NONE',  ( 0.000000000000000000, -1.145812388885151023, 6.715725538143585638 ) ) ;
#30770 = CARTESIAN_POINT ( 'NONE',  ( 35.00000000000000000, 4.705694406421931860E-17, -3.469127814946512892E-15 ) ) ;
#30772 = ORIENTED_EDGE ( 'NONE', *, *, #14048, .T. ) ;
#30771 = CARTESIAN_POINT ( 'NONE',  ( 3.047904605210409734, 0.9519317672906866257, 7.845751380824976806 ) ) ;
#30773 = FACE_OUTER_BOUND ( 'NONE', #64887, .T. ) ;
#30774 = EDGE_CURVE ( 'NONE', #1623, #46377, #63609, .T. ) ;
#30775 = AXIS2_PLACEMENT_3D ( 'NONE', #13290, #7649, #27931 ) ;
#30776 = CARTESIAN_POINT ( 'NONE',  ( 2.000000000000001776, -5.457833520448623688, -4.281014542496604847 ) ) ;
#30777 = VERTEX_POINT ( 'NONE', #54662 ) ;
#30778 = DIRECTION ( 'NONE',  ( 1.000000000000000000, 0.000000000000000000, -0.000000000000000000 ) ) ;
#30779 = CARTESIAN_POINT ( 'NONE',  ( -9.276318581089137538, 12.47567835156090865, -5.170372665552285696 ) ) ;
#30780 = DIRECTION ( 'NONE',  ( 0.000000000000000000, -0.01356324068817998940, 0.9999080150203990547 ) ) ;
#30781 = CARTESIAN_POINT ( 'NONE',  ( 0.6511581176971025231, -1.822219471613997221, -12.23990098761649570 ) ) ;
#30782 = LINE ( 'NONE', #9862, #34205 ) ;
#30783 = CARTESIAN_POINT ( 'NONE',  ( 2.241537034860906275, 2.615577641485621996, -7.172440248506130267 ) ) ;
#30784 = FACE_OUTER_BOUND ( 'NONE', #54255, .T. ) ;
#30785 = ORIENTED_EDGE ( 'NONE', *, *, #46551, .F. ) ;
#30786 = CARTESIAN_POINT ( 'NONE',  ( 2.249013661412228249, -5.000301708456363237, 5.772355099776667053 ) ) ;
#30787 = VERTEX_POINT ( 'NONE', #38694 ) ;
#30788 = DIRECTION ( 'NONE',  ( 1.000000000000000000, 0.000000000000000000, 0.000000000000000000 ) ) ;
#30789 = DIRECTION ( 'NONE',  ( -1.000000000000000000, -0.000000000000000000, -0.000000000000000000 ) ) ;
#30790 = CIRCLE ( 'NONE', #64779, 12.18649999999999878 ) ;
#30791 = ADVANCED_FACE ( 'NONE', ( #58322 ), #24366, .F. ) ;
#30792 = CARTESIAN_POINT ( 'NONE',  ( 2.653899356900376816, 1.606012885791718192, 7.604196386057602730 ) ) ;
#30793 = CYLINDRICAL_SURFACE ( 'NONE', #36209, 12.18649999999999878 ) ;
#30795 = ORIENTED_EDGE ( 'NONE', *, *, #28309, .F. ) ;
#30794 = AXIS2_PLACEMENT_3D ( 'NONE', #12542, #33505, #48167 ) ;
#30796 = CARTESIAN_POINT ( 'NONE',  ( 5.514970785353741078, 0.004713149585127535644, -0.0003039746380528477398 ) ) ;
#30797 = CARTESIAN_POINT ( 'NONE',  ( -35.00000000000000000, -9.913596905230058098, -8.017674001891892388 ) ) ;
#30798 = FACE_BOUND ( 'NONE', #64375, .T. ) ;
#30799 = ORIENTED_EDGE ( 'NONE', *, *, #15601, .F. ) ;
#30800 = EDGE_LOOP ( 'NONE', ( #10938, #30895, #35525, #62792 ) ) ;
#30801 = CARTESIAN_POINT ( 'NONE',  ( 2.589278595513308190, 7.587119248534321514, -1.582391164331529598 ) ) ;
#30802 = ORIENTED_EDGE ( 'NONE', *, *, #40593, .T. ) ;
#30803 = AXIS2_PLACEMENT_3D ( 'NONE', #38768, #9719, #43747 ) ;
#30804 = FACE_OUTER_BOUND ( 'NONE', #1687, .T. ) ;
#30805 = DIRECTION ( 'NONE',  ( 0.000000000000000000, 0.000000000000000000, 1.000000000000000000 ) ) ;
#30806 = DIRECTION ( 'NONE',  ( 0.000000000000000000, -0.01356324068817998940, 0.9999080150203990547 ) ) ;
#30807 = CARTESIAN_POINT ( 'NONE',  ( -27.09729107899804745, 1.021938248125928261, -2.094470452260987159 ) ) ;
#30808 = CARTESIAN_POINT ( 'NONE',  ( 35.00000000000000000, 11.59095880812004964, -1.903127969211395598 ) ) ;
#30809 = CARTESIAN_POINT ( 'NONE',  ( -10.00000000000000178, 0.000000000000000000, 0.000000000000000000 ) ) ;
#30810 = CARTESIAN_POINT ( 'NONE',  ( 0.3654063281920720829, 11.62642356802261823, 3.951404032559308277 ) ) ;
#30811 = VECTOR ( 'NONE', #21160, 1000.000000000000000 ) ;
#30812 = EDGE_CURVE ( 'NONE', #3623, #51096, #38030, .T. ) ;
#30813 = ORIENTED_EDGE ( 'NONE', *, *, #14613, .F. ) ;
#30814 = DIRECTION ( 'NONE',  ( 0.000000000000000000, 0.2355298848897516562, 0.9718671068226459875 ) ) ;
#30815 = EDGE_CURVE ( 'NONE', #65337, #1946, #55032, .T. ) ;
#30816 = AXIS2_PLACEMENT_3D ( 'NONE', #59424, #34143, #44440 ) ;
#30817 = CARTESIAN_POINT ( 'NONE',  ( 22.12488133644825439, 11.11891314965964561, -4.528710933524925153 ) ) ;
#30818 = CARTESIAN_POINT ( 'NONE',  ( -35.00000000000000000, -0.4993900848166508144, -12.17626345777664554 ) ) ;
#30819 = CARTESIAN_POINT ( 'NONE',  ( 2.000000000000001776, 0.000000000000000000, 0.000000000000000000 ) ) ;
#30820 = DIRECTION ( 'NONE',  ( 0.9318405276259970060, 0.3628680629012471237, 0.000000000000000000 ) ) ;
#30821 = CARTESIAN_POINT ( 'NONE',  ( 0.2915757698887283533, -10.71881693660618140, -5.940579417090889436 ) ) ;
#30822 = DIRECTION ( 'NONE',  ( 0.000000000000000000, -0.01356324068817998940, 0.9999080150203990547 ) ) ;
#30823 = B_SPLINE_CURVE_WITH_KNOTS ( 'NONE', 3,
 ( #24372, #30660, #39675, #45639, #40654, #59972, #40314, #15044, #55638, #10075, #30356, #89, #35969, #752, #56268, #21013, #26341, #6398, #10712 ),
 .UNSPECIFIED., .F., .F.,
 ( 4, 3, 3, 3, 3, 3, 4 ),
 ( 0.000000000000000000, 2.832085443540696562E-05, 4.217789847394769317E-05, 5.603488375046152285E-05, 6.989180858579407713E-05, 9.821094829918835742E-05, 0.0001178165571465097797 ),
 .UNSPECIFIED. ) ;
#30824 = LINE ( 'NONE', #915, #60570 ) ;
#30825 = CIRCLE ( 'NONE', #39340, 5.000000000000000000 ) ;
#30826 = AXIS2_PLACEMENT_3D ( 'NONE', #33636, #16775, #38626 ) ;
#30828 = VERTEX_POINT ( 'NONE', #13408 ) ;
#30827 = AXIS2_PLACEMENT_3D ( 'NONE', #16688, #25692, #56266 ) ;
#30829 = EDGE_CURVE ( 'NONE', #16276, #18362, #44631, .T. ) ;
#30830 = CIRCLE ( 'NONE', #24475, 2.899999999999994582 ) ;
#30831 = CARTESIAN_POINT ( 'NONE',  ( 8.437200413559441614, 4.476360154859203355, 12.73625532737111143 ) ) ;
#30832 = ORIENTED_EDGE ( 'NONE', *, *, #27600, .F. ) ;
#30833 = CARTESIAN_POINT ( 'NONE',  ( -22.29290468048228036, -3.718584170466873839, 0.2747050847461821599 ) ) ;
#30834 = CARTESIAN_POINT ( 'NONE',  ( 0.2646305136544072623, 0.1321451301299527148, -12.24595685781654453 ) ) ;
#30835 = CARTESIAN_POINT ( 'NONE',  ( 0.2650492594609232255, -12.07870403910582624, 2.017987075343919745 ) ) ;
#30836 = CARTESIAN_POINT ( 'NONE',  ( 1.000000000000000888, -5.217815162096798076, -5.387430271863655307 ) ) ;
#30837 = EDGE_CURVE ( 'NONE', #2509, #4485, #16773, .T. ) ;
#30838 = ORIENTED_EDGE ( 'NONE', *, *, #35678, .F. ) ;
#30839 = FACE_OUTER_BOUND ( 'NONE', #729, .T. ) ;
#30840 = CARTESIAN_POINT ( 'NONE',  ( 2.368238019615081402, 2.455958560214755781, -7.273245349264682247 ) ) ;
#30841 = DIRECTION ( 'NONE',  ( -1.000000000000000000, 0.000000000000000000, 0.000000000000000000 ) ) ;
#30842 = CARTESIAN_POINT ( 'NONE',  ( -22.46225619532221529, 3.746472695305362421, 1.978788174090766017 ) ) ;
#30843 = AXIS2_PLACEMENT_3D ( 'NONE', #10769, #31389, #52005 ) ;
#30844 = AXIS2_PLACEMENT_3D ( 'NONE', #2180, #32733, #1548 ) ;
#30845 = CARTESIAN_POINT ( 'NONE',  ( 5.536195898058073439, 0.008496323383586771791, -0.0002547682446684141071 ) ) ;
#30846 = CIRCLE ( 'NONE', #51055, 2.899999999999994582 ) ;
#30847 = CARTESIAN_POINT ( 'NONE',  ( 2.247112776671468026, 2.720990995225304410, 7.135103076758457341 ) ) ;
#30848 =( BOUNDED_SURFACE ( )  B_SPLINE_SURFACE ( 3, 1, ( 
 ( #58834, #18895 ),
 ( #59451, #13254 ),
 ( #33534, #49175 ),
 ( #8259, #28531 ) ),
 .UNSPECIFIED., .F., .F., .F. ) 
 B_SPLINE_SURFACE_WITH_KNOTS ( ( 4, 4 ),
 ( 2, 2 ),
 ( 0.000000000000000000, 1.000000000000000000 ),
 ( 0.000000000000000000, 1.000000000000000000 ),
 .UNSPECIFIED. ) 
 GEOMETRIC_REPRESENTATION_ITEM ( )  RATIONAL_B_SPLINE_SURFACE ( (
 ( 1.000000000000000000, 1.000000000000000000),
 ( 0.6933888150995267674, 0.9895912004443193632),
 ( 0.6933888150995267674, 0.9895912004443193632),
 ( 1.000000000000000000, 1.000000000000000000) ) ) 
 REPRESENTATION_ITEM ( '' )  SURFACE ( )  );
#30849 = EDGE_LOOP ( 'NONE', ( #12725, #2105, #3675, #39157 ) ) ;
#30850 = AXIS2_PLACEMENT_3D ( 'NONE', #6240, #52118, #36815 ) ;
#30851 = CARTESIAN_POINT ( 'NONE',  ( -35.00000000000000000, -4.237620530777717498, -11.42599468261433771 ) ) ;
#30852 = ORIENTED_EDGE ( 'NONE', *, *, #241, .F. ) ;
#30853 = CARTESIAN_POINT ( 'NONE',  ( 0.2653519890518151181, 12.24619734961135542, -8.824939166405896469E-06 ) ) ;
#30854 = DIRECTION ( 'NONE',  ( -1.000000000000000000, 0.000000000000000000, -0.000000000000000000 ) ) ;
#30855 = AXIS2_PLACEMENT_3D ( 'NONE', #8344, #48927, #13332 ) ;
#30856 = CARTESIAN_POINT ( 'NONE',  ( 5.515188684475870851, 0.005339000964281803707, 0.0003622115669623466238 ) ) ;
#30857 = CARTESIAN_POINT ( 'NONE',  ( 2.305787727787083519, -7.135468203929965725, -2.774453000917220802 ) ) ;
#30858 = ORIENTED_EDGE ( 'NONE', *, *, #9330, .F. ) ;
#30859 = VERTEX_POINT ( 'NONE', #64922 ) ;
#30860 = CARTESIAN_POINT ( 'NONE',  ( -29.95627872347045084, 0.8329649216453900440, 11.97914056345418565 ) ) ;
#30861 = ORIENTED_EDGE ( 'NONE', *, *, #32247, .T. ) ;
#30862 = AXIS2_PLACEMENT_3D ( 'NONE', #54230, #29281, #55195 ) ;
#30863 = CARTESIAN_POINT ( 'NONE',  ( 2.253265082352432724, -6.549959928643412255, -3.929729351083060873 ) ) ;
#30864 = CARTESIAN_POINT ( 'NONE',  ( -8.891032880924175430, -12.93614229090407974, -3.860857758255645589 ) ) ;
#30865 = CARTESIAN_POINT ( 'NONE',  ( -22.27722015946438816, -3.455127654605128829, -1.271715168852078026 ) ) ;
#30866 = FACE_OUTER_BOUND ( 'NONE', #26094, .T. ) ;
#30867 = CARTESIAN_POINT ( 'NONE',  ( 1.194176325881332934, 9.279760592562206867, -8.457794872459018620 ) ) ;
#30868 = CARTESIAN_POINT ( 'NONE',  ( 5.514970785353741078, 0.004532877335078713300, 0.001326349372336309675 ) ) ;
#30869 = CYLINDRICAL_SURFACE ( 'NONE', #38252, 5.000000000000000888 ) ;
#30870 = ORIENTED_EDGE ( 'NONE', *, *, #50707, .T. ) ;
#30871 = CIRCLE ( 'NONE', #43649, 2.899999999999996358 ) ;
#30872 = EDGE_CURVE ( 'NONE', #55446, #14676, #61379, .T. ) ;
#30873 = CARTESIAN_POINT ( 'NONE',  ( -9.218674071044169693, -9.592100768695239310, -7.220698992947784056 ) ) ;
#30874 = ORIENTED_EDGE ( 'NONE', *, *, #27050, .T. ) ;
#30875 = DIRECTION ( 'NONE',  ( 0.000000000000000000, 0.8696919319575165952, 0.4935949184179292404 ) ) ;
#30876 = CARTESIAN_POINT ( 'NONE',  ( 0.3537226245948376091, 10.49813096858609640, 6.362463382302304460 ) ) ;
#30877 = EDGE_CURVE ( 'NONE', #53881, #25961, #64553, .T. ) ;
#30879 = CARTESIAN_POINT ( 'NONE',  ( -27.09729107899804390, 1.932259710106502215, -1.302895495070934162 ) ) ;
#30878 = AXIS2_PLACEMENT_3D ( 'NONE', #29391, #39043, #18468 ) ;
#30880 = AXIS2_PLACEMENT_3D ( 'NONE', #18190, #13194, #27830 ) ;
#30881 = VECTOR ( 'NONE', #32425, 1000.000000000000000 ) ;
#30882 = ORIENTED_EDGE ( 'NONE', *, *, #53754, .T. ) ;
#30883 = CARTESIAN_POINT ( 'NONE',  ( -14.30187556442842478, -30.10361765235437304, 4.782130246577438015 ) ) ;
#30884 = ORIENTED_EDGE ( 'NONE', *, *, #15172, .F. ) ;
#30885 = CARTESIAN_POINT ( 'NONE',  ( 2.406456491627780636, 10.36527681095535769, 1.188938370542462097 ) ) ;
#30886 = DIRECTION ( 'NONE',  ( 0.000000000000000000, -0.3807014730195085739, 0.9246979985058777496 ) ) ;
#30887 = AXIS2_PLACEMENT_3D ( 'NONE', #45716, #50720, #176 ) ;
#30888 = CARTESIAN_POINT ( 'NONE',  ( 2.717984159219746232, 2.930214355830766948, 7.221467817271564726 ) ) ;
#30889 = CARTESIAN_POINT ( 'NONE',  ( -27.10719052120871098, -2.295785794152564563, -0.5475695427849640584 ) ) ;
#30890 = ORIENTED_EDGE ( 'NONE', *, *, #25231, .T. ) ;
#30891 = ORIENTED_EDGE ( 'NONE', *, *, #35188, .T. ) ;
#30892 = DIRECTION ( 'NONE',  ( -1.000000000000000000, 0.000000000000000000, 0.000000000000000000 ) ) ;
#30893 = ORIENTED_EDGE ( 'NONE', *, *, #22901, .F. ) ;
#30894 = DIRECTION ( 'NONE',  ( 1.000000000000000000, 0.000000000000000000, 0.000000000000000000 ) ) ;
#30895 = ORIENTED_EDGE ( 'NONE', *, *, #12968, .T. ) ;
#30896 = EDGE_LOOP ( 'NONE', ( #42462, #29550, #50372, #51262 ) ) ;
#30897 = ORIENTED_EDGE ( 'NONE', *, *, #9816, .F. ) ;
#30898 = DIRECTION ( 'NONE',  ( -1.000000000000000000, 0.000000000000000000, 0.000000000000000000 ) ) ;
#30899 = CARTESIAN_POINT ( 'NONE',  ( 19.56743653832047514, -28.99999999999999645, 4.999999999999997335 ) ) ;
#30900 = EDGE_CURVE ( 'NONE', #26984, #23983, #35888, .T. ) ;
#30901 = DIRECTION ( 'NONE',  ( 0.000000000000000000, 0.000000000000000000, -1.000000000000000000 ) ) ;
#30902 = CARTESIAN_POINT ( 'NONE',  ( -27.35552965826137140, 1.773915698030573473, -2.548625910254528559 ) ) ;
#30903 = LINE ( 'NONE', #60189, #5867 ) ;
#30904 = VERTEX_POINT ( 'NONE', #44009 ) ;
#30905 = AXIS2_PLACEMENT_3D ( 'NONE', #6668, #11959, #36904 ) ;
#30906 = FACE_OUTER_BOUND ( 'NONE', #40889, .T. ) ;
#30907 = CIRCLE ( 'NONE', #16041, 12.18650000000000055 ) ;
#30908 = ADVANCED_FACE ( 'NONE', ( #39328 ), #597, .F. ) ;
#30909 = ORIENTED_EDGE ( 'NONE', *, *, #41807, .F. ) ;
#30910 = LINE ( 'NONE', #6969, #58270 ) ;
#30911 = ADVANCED_FACE ( 'NONE', ( #2813 ), #18428, .T. ) ;
#30912 = DIRECTION ( 'NONE',  ( 0.000000000000000000, 0.9903235168508545128, 0.1387779952735854194 ) ) ;
#30913 = AXIS2_PLACEMENT_3D ( 'NONE', #30242, #44529, #60488 ) ;
#30914 = EDGE_CURVE ( 'NONE', #36353, #15972, #43332, .T. ) ;
#30915 = CARTESIAN_POINT ( 'NONE',  ( 0.3040950598368152291, -8.072385578287409658, -9.229598020917764600 ) ) ;
#30916 = CARTESIAN_POINT ( 'NONE',  ( 1.375507693220546113, 10.03411718356233706, -7.647735792764737361 ) ) ;
#30917 = CARTESIAN_POINT ( 'NONE',  ( -35.00000000000000000, 4.400442035671113139, -11.96656215839364457 ) ) ;
#30918 = CIRCLE ( 'NONE', #2265, 2.899999999999995026 ) ;
#30919 = CARTESIAN_POINT ( 'NONE',  ( 1.109979610372547443, -10.60154531817216572, -6.674783385105683919 ) ) ;
#30920 = ORIENTED_EDGE ( 'NONE', *, *, #37092, .F. ) ;
#30921 = ADVANCED_FACE ( 'NONE', ( #18082 ), #38349, .T. ) ;
#30922 = CARTESIAN_POINT ( 'NONE',  ( 2.000000000000001776, 0.000000000000000000, 0.000000000000000000 ) ) ;
#30923 = AXIS2_PLACEMENT_3D ( 'NONE', #36946, #58229, #53246 ) ;
#30924 = EDGE_LOOP ( 'NONE', ( #48753, #5159, #49898, #31558 ) ) ;
#30925 = EDGE_CURVE ( 'NONE', #41767, #14897, #47776, .T. ) ;
#30926 = CARTESIAN_POINT ( 'NONE',  ( -24.47698661514656848, -11.24106201439485275, 7.478403204343472055 ) ) ;
#30927 = CARTESIAN_POINT ( 'NONE',  ( 18.79103332550324623, -28.91360719445344785, -6.866334764117087985 ) ) ;
#30928 = CARTESIAN_POINT ( 'NONE',  ( 19.24109636373442100, -29.98159021036885008, 5.977446804020324578 ) ) ;
#30930 = VECTOR ( 'NONE', #38394, 1000.000000000000000 ) ;
#30929 = CARTESIAN_POINT ( 'NONE',  ( 2.253265082352139625, -3.707567016434152318, -6.678225412356649571 ) ) ;
#30931 = CARTESIAN_POINT ( 'NONE',  ( 2.241506898688418126, 7.525229609709738199, 1.286963596520017461 ) ) ;
#30932 = ORIENTED_EDGE ( 'NONE', *, *, #55778, .F. ) ;
#30933 = DIRECTION ( 'NONE',  ( 1.000000000000000000, 0.000000000000000000, -0.000000000000000000 ) ) ;
#30934 = CARTESIAN_POINT ( 'NONE',  ( 1.719304012341582588, 5.690355757825640737, -11.38834240361563488 ) ) ;
#30935 = B_SPLINE_CURVE_WITH_KNOTS ( 'NONE', 3,
 ( #35727, #60353, #14778, #50065, #55040, #55714, #50722, #40063, #4179, #65654, #61335, #35405, #35061, #4524, #20782, #5172, #65009, #56021, #15772, #19482, #50407, #36050 ),
 .UNSPECIFIED., .F., .F.,
 ( 4, 3, 3, 3, 3, 3, 3, 4 ),
 ( 0.000000000000000000, 6.990956068646445834E-05, 0.0001398191187764044672, 0.0002097286751720215444, 0.0002796382307041364807, 0.0003495477861619816708, 0.0004194573423310295505, 0.0005586102576333146046 ),
 .UNSPECIFIED. ) ;
#30936 = CARTESIAN_POINT ( 'NONE',  ( 21.44973177390235364, 11.47610357474619747, -3.531383847275154864 ) ) ;
#30937 = CARTESIAN_POINT ( 'NONE',  ( -35.00000000000000000, 11.99999999999998579, 1.469576158976822172E-15 ) ) ;
#30938 = AXIS2_PLACEMENT_3D ( 'NONE', #59838, #60149, #14268 ) ;
#30939 = VECTOR ( 'NONE', #54009, 1000.000000000000000 ) ;
#30940 = AXIS2_PLACEMENT_3D ( 'NONE', #2160, #37400, #52716 ) ;
#30941 = EDGE_CURVE ( 'NONE', #64485, #42804, #1925, .T. ) ;
#30942 = CARTESIAN_POINT ( 'NONE',  ( -35.00000000000000000, -4.732539170486343316, 11.23004253107762906 ) ) ;
#30943 = CARTESIAN_POINT ( 'NONE',  ( -35.04709527796842394, -0.01016988845958625987, -0.007030359780627049027 ) ) ;
#30944 = CARTESIAN_POINT ( 'NONE',  ( 0.2653519789438783527, -2.104833950422661193, 12.06397564829375746 ) ) ;
#30945 = FACE_OUTER_BOUND ( 'NONE', #54579, .T. ) ;
#30946 = DIRECTION ( 'NONE',  ( -1.000000000000000000, 0.000000000000000000, 0.000000000000000000 ) ) ;
#30947 = B_SPLINE_CURVE_WITH_KNOTS ( 'NONE', 3,
 ( #46303, #11048, #40303, #45972, #60595, #742, #41284, #50639, #15035, #25347, #40972, #51628, #46614, #55628, #10372, #1070, #45625, #20362, #40642, #30648 ),
 .UNSPECIFIED., .F., .F.,
 ( 4, 2, 2, 2, 2, 2, 2, 2, 2, 4 ),
 ( 1.939479807224432123E-18, 0.001283480623487103997, 0.001925220935230654044, 0.002566961246974203657, 0.003850441870461304619, 0.005133922493948405580, 0.006417403117435506107, 0.007700883740922607502, 0.008984364364409708897, 0.01026784498789680942 ),
 .UNSPECIFIED. ) ;
#30948 = AXIS2_PLACEMENT_3D ( 'NONE', #41104, #57083, #16181 ) ;
#30949 = CIRCLE ( 'NONE', #4392, 5.000000000000001776 ) ;
#30950 = ORIENTED_EDGE ( 'NONE', *, *, #30741, .T. ) ;
#30951 = ORIENTED_EDGE ( 'NONE', *, *, #11104, .F. ) ;
#30952 = CARTESIAN_POINT ( 'NONE',  ( 25.00000000000000711, -3.797884998337192286, -24.00000000000000000 ) ) ;
#30953 = FACE_OUTER_BOUND ( 'NONE', #15345, .T. ) ;
#30954 = AXIS2_PLACEMENT_3D ( 'NONE', #15435, #35703, #60664 ) ;
#30955 = CARTESIAN_POINT ( 'NONE',  ( 47.00000000000000711, 4.705694406421931860E-17, -3.469127814946512892E-15 ) ) ;
#30956 = VERTEX_POINT ( 'NONE', #34979 ) ;
#30957 = ORIENTED_EDGE ( 'NONE', *, *, #18021, .F. ) ;
#30958 = ORIENTED_EDGE ( 'NONE', *, *, #2018, .F. ) ;
#30959 = CARTESIAN_POINT ( 'NONE',  ( 3.100650473569641186, 3.129198107108005278, -7.276570693048371119 ) ) ;
#30960 = EDGE_CURVE ( 'NONE', #8976, #1587, #49731, .T. ) ;
#30961 = DIRECTION ( 'NONE',  ( 0.000000000000000000, -0.01356324068817998940, 0.9999080150203990547 ) ) ;
#30962 = ORIENTED_EDGE ( 'NONE', *, *, #61930, .T. ) ;
#30963 = CARTESIAN_POINT ( 'NONE',  ( 35.00000000000000000, 9.752226076388984310, 6.547236723513913503 ) ) ;
#30964 = AXIS2_PLACEMENT_3D ( 'NONE', #44161, #14219, #23564 ) ;
#30965 = DIRECTION ( 'NONE',  ( 0.000000000000000000, -0.01356324068817992001, 0.9999080150203990547 ) ) ;
#30966 = ORIENTED_EDGE ( 'NONE', *, *, #60909, .T. ) ;
#30967 = DIRECTION ( 'NONE',  ( 0.3939253465568944290, -0.3052156353794323596, -0.8669868725995567571 ) ) ;
#30968 = EDGE_CURVE ( 'NONE', #44673, #54109, #26360, .T. ) ;
#30969 = CARTESIAN_POINT ( 'NONE',  ( 16.45277491483739496, -34.41570230176855461, -6.124363151458832810 ) ) ;
#30970 = CYLINDRICAL_SURFACE ( 'NONE', #1640, 13.50000000000000178 ) ;
#30971 = ORIENTED_EDGE ( 'NONE', *, *, #55509, .T. ) ;
#30972 = CIRCLE ( 'NONE', #39466, 12.18650000000000233 ) ;
#30974 = AXIS2_PLACEMENT_3D ( 'NONE', #2440, #2090, #53638 ) ;
#30973 = CARTESIAN_POINT ( 'NONE',  ( 0.000000000000000000, 244.9489742783177917, 24.99999999999999289 ) ) ;
#30975 = ORIENTED_EDGE ( 'NONE', *, *, #1205, .F. ) ;
#30976 = DIRECTION ( 'NONE',  ( -0.3939253465568944290, -0.8669868725995537595, -0.3052156353794409638 ) ) ;
#30977 = ORIENTED_EDGE ( 'NONE', *, *, #6981, .T. ) ;
#30978 = EDGE_CURVE ( 'NONE', #13727, #40874, #21034, .T. ) ;
#30979 = ORIENTED_EDGE ( 'NONE', *, *, #39635, .F. ) ;
#30980 = CARTESIAN_POINT ( 'NONE',  ( -35.00000000000000000, 0.000000000000000000, 0.000000000000000000 ) ) ;
#30981 = CARTESIAN_POINT ( 'NONE',  ( -35.00000000000000000, -2.936739658819952581, 11.37311665002362560 ) ) ;
#30982 = FACE_OUTER_BOUND ( 'NONE', #65709, .T. ) ;
#30983 = CARTESIAN_POINT ( 'NONE',  ( -22.31328051695926007, -2.748895659348118858, -2.608921479762132734 ) ) ;
#30984 = CIRCLE ( 'NONE', #35190, 5.000000000000000000 ) ;
#30986 = AXIS2_PLACEMENT_3D ( 'NONE', #19093, #34689, #64958 ) ;
#30985 = DIRECTION ( 'NONE',  ( -1.000000000000000000, 0.000000000000000000, -0.000000000000000000 ) ) ;
#30987 = ADVANCED_FACE ( 'NONE', ( #5089 ), #10705, .T. ) ;
#30988 = CARTESIAN_POINT ( 'NONE',  ( -35.00000000000000000, 11.05394794832836780, -5.130401251914613603 ) ) ;
#30989 = CARTESIAN_POINT ( 'NONE',  ( 35.00000000000000000, -3.827046518385000429, 11.56998259273181162 ) ) ;
#30990 = CARTESIAN_POINT ( 'NONE',  ( 5.515188684475870851, -0.004322737127823994552, -0.003154373509839847670 ) ) ;
#30992 = EDGE_LOOP ( 'NONE', ( #34084, #28635, #20714, #58802 ) ) ;
#30991 = DIRECTION ( 'NONE',  ( 1.000000000000000000, 0.000000000000000000, -0.000000000000000000 ) ) ;
#30993 = DIRECTION ( 'NONE',  ( 0.000000000000000000, -0.8276889981568841259, -0.5611870653623918237 ) ) ;
#30994 = ORIENTED_EDGE ( 'NONE', *, *, #4130, .T. ) ;
#30995 = CARTESIAN_POINT ( 'NONE',  ( 12.29669898719158638, -13.32434165500316148, -2.178069250421873715 ) ) ;
#30996 = EDGE_CURVE ( 'NONE', #16803, #29123, #19401, .T. ) ;
#30997 = FACE_OUTER_BOUND ( 'NONE', #50947, .T. ) ;
#30998 = EDGE_CURVE ( 'NONE', #18081, #65768, #65572, .T. ) ;
#30999 = VERTEX_POINT ( 'NONE', #26023 ) ;
#31000 = DIRECTION ( 'NONE',  ( -1.000000000000000000, 0.000000000000000000, 0.000000000000000000 ) ) ;
#31001 = CARTESIAN_POINT ( 'NONE',  ( 0.2646305136544065406, 10.67138229758229429, 6.008537389229452685 ) ) ;
#31002 = CARTESIAN_POINT ( 'NONE',  ( 37.00000000000000711, 4.705694406421931860E-17, -3.469127814946512892E-15 ) ) ;
#31004 = CIRCLE ( 'NONE', #50143, 5.000000000000000888 ) ;
#31003 = CYLINDRICAL_SURFACE ( 'NONE', #64557, 12.75000000000000178 ) ;
#31005 = AXIS2_PLACEMENT_3D ( 'NONE', #62422, #16236, #17877 ) ;
#31006 = LINE ( 'NONE', #51316, #56357 ) ;
#31007 = VERTEX_POINT ( 'NONE', #81 ) ;
#31008 = DIRECTION ( 'NONE',  ( -1.000000000000000000, -0.000000000000000000, 0.000000000000000000 ) ) ;
#31009 = AXIS2_PLACEMENT_3D ( 'NONE', #34999, #9750, #50351 ) ;
#31010 = ORIENTED_EDGE ( 'NONE', *, *, #50842, .T. ) ;
#31011 = EDGE_CURVE ( 'NONE', #64161, #13910, #8445, .T. ) ;
#31012 = CIRCLE ( 'NONE', #10830, 12.18649999999999878 ) ;
#31013 = DIRECTION ( 'NONE',  ( 0.000000000000000000, 0.01356324068817992001, -0.9999080150203990547 ) ) ;
#31014 = CARTESIAN_POINT ( 'NONE',  ( 0.3665391374699465965, 0.2638605131387155023, 12.27992639892678461 ) ) ;
#31015 = EDGE_CURVE ( 'NONE', #18880, #14095, #50644, .T. ) ;
#31016 = ORIENTED_EDGE ( 'NONE', *, *, #31609, .T. ) ;
#31017 = CARTESIAN_POINT ( 'NONE',  ( 0.2958664285830442386, -4.398464391600247048, -11.43993536884560669 ) ) ;
#31018 = EDGE_CURVE ( 'NONE', #33456, #60735, #39122, .T. ) ;
#31019 = EDGE_CURVE ( 'NONE', #57990, #5000, #48160, .T. ) ;
#31020 = AXIS2_PLACEMENT_3D ( 'NONE', #54734, #48441, #17834 ) ;
#31021 = CARTESIAN_POINT ( 'NONE',  ( -22.66110217412718697, -2.319520136975679492, -4.366928509133845004 ) ) ;
#31022 = CARTESIAN_POINT ( 'NONE',  ( 49.59714883329486668, -0.08190040965285508290, 4.488761805454714704 ) ) ;
#31023 = ADVANCED_FACE ( 'NONE', ( #21345 ), #43098, .F. ) ;
#31024 = DIRECTION ( 'NONE',  ( -1.000000000000000000, 0.000000000000000000, 0.000000000000000000 ) ) ;
#31025 = CARTESIAN_POINT ( 'NONE',  ( 10.48620311856346454, 8.250315036047107142, 10.68561190601526611 ) ) ;
#31026 = CARTESIAN_POINT ( 'NONE',  ( 2.258463476536646919, 6.683417898966930615, -3.701774005560789504 ) ) ;
#31027 = DIRECTION ( 'NONE',  ( 1.000000000000000000, -0.000000000000000000, 0.000000000000000000 ) ) ;
#31028 = CARTESIAN_POINT ( 'NONE',  ( 0.5572780756287527559, -3.933334466452446332, -11.70006938410077346 ) ) ;
#31029 = AXIS2_PLACEMENT_3D ( 'NONE', #24336, #38072, #53391 ) ;
#31030 = AXIS2_PLACEMENT_3D ( 'NONE', #54175, #24231, #58187 ) ;
#31031 = LINE ( 'NONE', #20736, #19329 ) ;
#31032 = DIRECTION ( 'NONE',  ( 0.000000000000000000, -0.7621620551276289124, -0.6473862847818364630 ) ) ;
#31033 = ORIENTED_EDGE ( 'NONE', *, *, #57917, .T. ) ;
#31034 = CARTESIAN_POINT ( 'NONE',  ( 1.000000000000000888, -5.769711778877296027, -4.791703871138604853 ) ) ;
#31035 = FACE_OUTER_BOUND ( 'NONE', #29889, .T. ) ;
#31036 = CARTESIAN_POINT ( 'NONE',  ( -22.27706089016750113, 3.562910635974989582, -0.9256273512588409913 ) ) ;
#31037 = ORIENTED_EDGE ( 'NONE', *, *, #41219, .F. ) ;
#31038 = CARTESIAN_POINT ( 'NONE',  ( -17.29244623348158783, 2.525873743887551814, 11.73115347397430597 ) ) ;
#31039 = DIRECTION ( 'NONE',  ( 0.000000000000000000, 0.6478160128811893959, -0.7617968321374922747 ) ) ;
#31040 = VERTEX_POINT ( 'NONE', #61912 ) ;
#31041 = VERTEX_POINT ( 'NONE', #27635 ) ;
#31042 = VERTEX_POINT ( 'NONE', #12018 ) ;
#31043 = CIRCLE ( 'NONE', #48053, 12.74999999999999822 ) ;
#31044 = AXIS2_PLACEMENT_3D ( 'NONE', #30769, #16155, #25470 ) ;
#31046 = ADVANCED_FACE ( 'NONE', ( #31333 ), #52614, .T. ) ;
#31045 = CARTESIAN_POINT ( 'NONE',  ( 145.1370849898475797, 3.309064568108273190E-14, 0.000000000000000000 ) ) ;
#31047 = ORIENTED_EDGE ( 'NONE', *, *, #23895, .F. ) ;
#31048 = FACE_OUTER_BOUND ( 'NONE', #12745, .T. ) ;
#31049 = CARTESIAN_POINT ( 'NONE',  ( -22.29382655386184453, -3.584644999358097550, 1.036465316386247393 ) ) ;
#31050 = LINE ( 'NONE', #37008, #60910 ) ;
#31051 = CARTESIAN_POINT ( 'NONE',  ( 35.00000000000000000, 8.389074212634284322, -8.839356091080075473 ) ) ;
#31052 = VERTEX_POINT ( 'NONE', #36308 ) ;
#31053 = AXIS2_PLACEMENT_3D ( 'NONE', #11432, #62296, #11748 ) ;
#31054 = CARTESIAN_POINT ( 'NONE',  ( -35.00000000000000000, 0.000000000000000000, 0.000000000000000000 ) ) ;
#31055 = CIRCLE ( 'NONE', #17257, 6.936499999999988120 ) ;
#31056 = CARTESIAN_POINT ( 'NONE',  ( -0.8442279638247468521, -31.04755392045528950, 14.43184553624044852 ) ) ;
#31057 = CARTESIAN_POINT ( 'NONE',  ( 24.65531244048388615, -2.290097230841563913, -13.30568042842709531 ) ) ;
#31059 = VERTEX_POINT ( 'NONE', #61572 ) ;
#31058 = CARTESIAN_POINT ( 'NONE',  ( -35.00000000000000000, 12.17626345777664376, -0.4993900848166082374 ) ) ;
#31060 = FACE_OUTER_BOUND ( 'NONE', #26660, .T. ) ;
#31061 = ORIENTED_EDGE ( 'NONE', *, *, #34472, .T. ) ;
#31062 = DIRECTION ( 'NONE',  ( 0.000000000000000000, -0.01356324068817998940, 0.9999080150203990547 ) ) ;
#31063 = ORIENTED_EDGE ( 'NONE', *, *, #35605, .F. ) ;
#31064 = ADVANCED_FACE ( 'NONE', ( #27001 ), #57929, .T. ) ;
#31065 = EDGE_LOOP ( 'NONE', ( #44046, #61057, #28889, #58149 ) ) ;
#31066 = FACE_OUTER_BOUND ( 'NONE', #58511, .T. ) ;
#31067 = CARTESIAN_POINT ( 'NONE',  ( 14.42557999472123775, -30.05477271089676350, 4.241434648442734989 ) ) ;
#31068 = CARTESIAN_POINT ( 'NONE',  ( 2.262775599886255762, -7.640237753423681610, -0.1412024122916668845 ) ) ;
#31069 = ORIENTED_EDGE ( 'NONE', *, *, #44532, .T. ) ;
#31070 = FACE_OUTER_BOUND ( 'NONE', #2719, .T. ) ;
#31071 = CARTESIAN_POINT ( 'NONE',  ( 2.000000000000001776, 7.484036900328571384, -0.4890722589968761191 ) ) ;
#31072 = CARTESIAN_POINT ( 'NONE',  ( 0.3474126878361803450, -12.03947592323248372, 2.385599230262000159 ) ) ;
#31073 = ORIENTED_EDGE ( 'NONE', *, *, #22076, .T. ) ;
#31074 = AXIS2_PLACEMENT_3D ( 'NONE', #25515, #41451, #60437 ) ;
#31075 =( BOUNDED_CURVE ( )  B_SPLINE_CURVE ( 3, ( #20854, #41445, #37119, #11851 ),
 .UNSPECIFIED., .F., .F. ) 
 B_SPLINE_CURVE_WITH_KNOTS ( ( 4, 4 ),
 ( 4.992524338435286424, 5.029647046869825999 ),
 .UNSPECIFIED. ) 
 CURVE ( )  GEOMETRIC_REPRESENTATION_ITEM ( )  RATIONAL_B_SPLINE_CURVE ( ( 1.000000000000000000, 0.9998851620069661994, 0.9998851620069661994, 1.000000000000000000 ) ) 
 REPRESENTATION_ITEM ( '' )  );
#31076 = ORIENTED_EDGE ( 'NONE', *, *, #17325, .F. ) ;
#31077 = CARTESIAN_POINT ( 'NONE',  ( 0.3053067050349164147, 12.03105545708856283, 2.355726819985464182 ) ) ;
#31078 = VERTEX_POINT ( 'NONE', #51632 ) ;
#31079 = ADVANCED_FACE ( 'NONE', ( #12343 ), #16017, .T. ) ;
#31080 = VECTOR ( 'NONE', #1775, 1000.000000000000000 ) ;
#31081 = ORIENTED_EDGE ( 'NONE', *, *, #1969, .F. ) ;
#31083 = AXIS2_PLACEMENT_3D ( 'NONE', #46513, #60489, #25245 ) ;
#31082 = DIRECTION ( 'NONE',  ( 0.000000000000000000, 0.01356324068817998940, -0.9999080150203989437 ) ) ;
#31084 = CARTESIAN_POINT ( 'NONE',  ( 0.6473888112830256114, -10.54705164520783178, 6.470260187014684305 ) ) ;
#31085 = CARTESIAN_POINT ( 'NONE',  ( 35.00000000000000000, -12.14284015767850455, -1.030638227056526413 ) ) ;
#31086 = CARTESIAN_POINT ( 'NONE',  ( 1.633930747251837845, -12.36466318969074685, 2.909970528251258681 ) ) ;
#31087 = DIRECTION ( 'NONE',  ( 1.000000000000000000, 0.000000000000000000, 0.000000000000000000 ) ) ;
#31088 = AXIS2_PLACEMENT_3D ( 'NONE', #31197, #22185, #6588 ) ;
#31089 = CYLINDRICAL_SURFACE ( 'NONE', #10793, 5.000000000000000888 ) ;
#31090 = CIRCLE ( 'NONE', #62923, 12.75000000000000178 ) ;
#31091 = DIRECTION ( 'NONE',  ( 0.000000000000000000, 0.5767582926624970074, 0.8169148498130275327 ) ) ;
#31092 = EDGE_LOOP ( 'NONE', ( #29952, #37767, #63882, #10335 ) ) ;
#31093 = DIRECTION ( 'NONE',  ( 0.000000000000000000, 0.8827602140260299990, -0.4698238015817395308 ) ) ;
#31094 = CYLINDRICAL_SURFACE ( 'NONE', #54209, 4.999999999999999112 ) ;
#31095 = CARTESIAN_POINT ( 'NONE',  ( -35.04683013664716640, -0.01162359816264506296, 0.004196202180946132648 ) ) ;
#31096 = ADVANCED_FACE ( 'NONE', ( #52287 ), #46619, .T. ) ;
#31097 = AXIS2_PLACEMENT_3D ( 'NONE', #39214, #12971, #13303 ) ;
#31098 = DIRECTION ( 'NONE',  ( 0.000000000000000000, 0.01356324068817992175, -0.9999080150203990547 ) ) ;
#31099 = CARTESIAN_POINT ( 'NONE',  ( -22.49803948133828513, 2.269619744675257067, 3.704553751086659297 ) ) ;
#31100 = EDGE_CURVE ( 'NONE', #39541, #2304, #31638, .T. ) ;
#31101 = CARTESIAN_POINT ( 'NONE',  ( 23.76403068109624073, 1.692630664537227769, -13.39737798747508890 ) ) ;
#31102 = CYLINDRICAL_SURFACE ( 'NONE', #25858, 6.936499999999988120 ) ;
#31103 = AXIS2_PLACEMENT_3D ( 'NONE', #36953, #41946, #21999 ) ;
#31104 = ADVANCED_FACE ( 'NONE', ( #36644 ), #56947, .T. ) ;
#31105 = DIRECTION ( 'NONE',  ( 1.000000000000000000, 0.000000000000000000, -0.000000000000000000 ) ) ;
#31106 = ORIENTED_EDGE ( 'NONE', *, *, #35123, .F. ) ;
#31107 = DIRECTION ( 'NONE',  ( 1.000000000000000000, 0.000000000000000000, -0.000000000000000000 ) ) ;
#31108 = CARTESIAN_POINT ( 'NONE',  ( 5.514970785353741078, 0.003929719953530069060, 0.002619824551223233922 ) ) ;
#31109 = DIRECTION ( 'NONE',  ( 1.000000000000000000, 0.000000000000000000, 0.000000000000000000 ) ) ;
#31110 = CARTESIAN_POINT ( 'NONE',  ( -25.95111430559885690, 10.26727955753690580, 6.212991851984511982 ) ) ;
#31111 = DIRECTION ( 'NONE',  ( 0.000000000000000000, -0.9970832820307047317, -0.07632122047555403577 ) ) ;
#31112 = ORIENTED_EDGE ( 'NONE', *, *, #54678, .F. ) ;
#31113 = CARTESIAN_POINT ( 'NONE',  ( -17.14841977825820507, -7.768776852921657650, -11.04569896549689290 ) ) ;
#31114 = DIRECTION ( 'NONE',  ( 1.000000000000000000, 0.000000000000000000, -0.000000000000000000 ) ) ;
#31115 = CARTESIAN_POINT ( 'NONE',  ( 12.74086035833940045, -29.15670053398524431, -4.066541195106388784 ) ) ;
#31116 = ORIENTED_EDGE ( 'NONE', *, *, #60346, .F. ) ;
#31117 = CYLINDRICAL_SURFACE ( 'NONE', #34443, 12.18650000000000055 ) ;
#31118 = CARTESIAN_POINT ( 'NONE',  ( 2.000000000000001776, -6.777474576704061171, -0.6925993764991672519 ) ) ;
#31119 = DIRECTION ( 'NONE',  ( 1.000000000000000000, -0.000000000000000000, 0.000000000000000000 ) ) ;
#31120 = VECTOR ( 'NONE', #46505, 999.9999999999998863 ) ;
#31121 = AXIS2_PLACEMENT_3D ( 'NONE', #8901, #49486, #24186 ) ;
#31123 = VERTEX_POINT ( 'NONE', #62887 ) ;
#31122 = CARTESIAN_POINT ( 'NONE',  ( 2.770579946183328257, 1.056759439485575491, 7.739026583264747572 ) ) ;
#31124 = CARTESIAN_POINT ( 'NONE',  ( -35.00000000000000000, 0.000000000000000000, 0.000000000000000000 ) ) ;
#31125 = VECTOR ( 'NONE', #54616, 1000.000000000000000 ) ;
#31126 = PRODUCT_DEFINITION ( 'UNKNOWN', '', #18669, #22623 ) ;
#31127 = AXIS2_PLACEMENT_3D ( 'NONE', #62770, #22210, #17238 ) ;
#31128 = EDGE_CURVE ( 'NONE', #26214, #61654, #16684, .T. ) ;
#31129 = FACE_OUTER_BOUND ( 'NONE', #39514, .T. ) ;
#31130 = ORIENTED_EDGE ( 'NONE', *, *, #1728, .F. ) ;
#31131 = DIRECTION ( 'NONE',  ( 0.3939253465568943180, -0.6978179301705759174, -0.5982248387291217995 ) ) ;
#31132 = ADVANCED_FACE ( 'NONE', ( #31964 ), #6727, .T. ) ;
#31133 = DIRECTION ( 'NONE',  ( 1.000000000000000000, 0.000000000000000000, 0.000000000000000000 ) ) ;
#31134 = CARTESIAN_POINT ( 'NONE',  ( 0.2651627923886330507, -7.938954356958149994, 9.324231535593082043 ) ) ;
#31135 = CARTESIAN_POINT ( 'NONE',  ( 8.437200413559441614, 4.476360154859202467, -12.73625532737110966 ) ) ;
#31136 = CARTESIAN_POINT ( 'NONE',  ( -9.351388602708162523, 11.42638970207765681, -3.665735721005252135 ) ) ;
#31137 = AXIS2_PLACEMENT_3D ( 'NONE', #33633, #42595, #12673 ) ;
#31138 = CARTESIAN_POINT ( 'NONE',  ( -18.14978613422465870, 3.488173043128369066, 13.04371742822381819 ) ) ;
#31140 = ORIENTED_EDGE ( 'NONE', *, *, #62016, .F. ) ;
#31139 = CARTESIAN_POINT ( 'NONE',  ( 0.5547464869798244269, 0.3049355384529007784, 12.33891836761636362 ) ) ;
#31141 = ORIENTED_EDGE ( 'NONE', *, *, #1162, .T. ) ;
#31142 = CARTESIAN_POINT ( 'NONE',  ( -35.00000000000000000, -11.70009620280410978, -1.039216533673027243 ) ) ;
#31143 = AXIS2_PLACEMENT_3D ( 'NONE', #62110, #16562, #26856 ) ;
#31144 = ORIENTED_EDGE ( 'NONE', *, *, #40135, .F. ) ;
#31145 = ADVANCED_FACE ( 'NONE', ( #39253 ), #59548, .T. ) ;
#31146 = DIRECTION ( 'NONE',  ( 0.000000000000000000, 0.000000000000000000, 1.000000000000000000 ) ) ;
#31147 = CARTESIAN_POINT ( 'NONE',  ( 35.00000000000000000, 4.725891942574903304, 10.75351884295722193 ) ) ;
#31148 = CIRCLE ( 'NONE', #20517, 4.999999999999998224 ) ;
#31149 = CARTESIAN_POINT ( 'NONE',  ( 0.000000000000000000, 7.484036900328563391, 0.4890722589969403455 ) ) ;
#31150 = CARTESIAN_POINT ( 'NONE',  ( -37.00000000000000711, -9.390600770287932164, -8.624332853796161658 ) ) ;
#31151 = ORIENTED_EDGE ( 'NONE', *, *, #33952, .F. ) ;
#31152 = CYLINDRICAL_SURFACE ( 'NONE', #55281, 14.69297241773857188 ) ;
#31153 = AXIS2_PLACEMENT_3D ( 'NONE', #27054, #1789, #42308 ) ;
#31154 = CARTESIAN_POINT ( 'NONE',  ( -24.32900315761321153, -7.891165000983839661, 9.051290049333715615 ) ) ;
#31155 = CARTESIAN_POINT ( 'NONE',  ( 9.575800908719084958, 25.00000000000000000, -1.072919909436247154 ) ) ;
#31156 = VERTEX_POINT ( 'NONE', #43932 ) ;
#31157 = AXIS2_PLACEMENT_3D ( 'NONE', #51869, #37548, #32532 ) ;
#31158 = ORIENTED_EDGE ( 'NONE', *, *, #51670, .F. ) ;
#31159 = CARTESIAN_POINT ( 'NONE',  ( 28.81710800639762482, -11.52178284190103064, 7.047181458019091238 ) ) ;
#31160 = EDGE_CURVE ( 'NONE', #41185, #16429, #34270, .T. ) ;
#31161 = EDGE_CURVE ( 'NONE', #37463, #55813, #36982, .T. ) ;
#31162 = EDGE_LOOP ( 'NONE', ( #24028, #38108, #53115, #55109 ) ) ;
#31163 = DIRECTION ( 'NONE',  ( 0.000000000000000000, 0.4380125133593973930, -0.8989688749565157844 ) ) ;
#31164 = DIRECTION ( 'NONE',  ( -1.000000000000000000, 0.000000000000000000, 0.000000000000000000 ) ) ;
#31165 = DIRECTION ( 'NONE',  ( -1.000000000000000000, 0.000000000000000000, 0.000000000000000000 ) ) ;
#31166 = EDGE_CURVE ( 'NONE', #1524, #60735, #23318, .T. ) ;
#31167 = CARTESIAN_POINT ( 'NONE',  ( -29.46763719790810754, 0.7246786509642640928, 11.98539570541942112 ) ) ;
#31168 = CARTESIAN_POINT ( 'NONE',  ( 0.000000000000000000, 0.2704997240205054276, 6.931223712253452796 ) ) ;
#31169 = DIRECTION ( 'NONE',  ( 0.000000000000000000, -0.01356324068817998593, 0.9999080150203990547 ) ) ;
#31170 = VECTOR ( 'NONE', #29450, 1000.000000000000000 ) ;
#31171 = CARTESIAN_POINT ( 'NONE',  ( 47.00000000000000711, 4.705694406421931860E-17, -3.469127814946512892E-15 ) ) ;
#31172 = ORIENTED_EDGE ( 'NONE', *, *, #65528, .T. ) ;
#31173 = CARTESIAN_POINT ( 'NONE',  ( 1.104777566491146557, 12.51694124543052133, -0.4777483965054175608 ) ) ;
#31174 = CARTESIAN_POINT ( 'NONE',  ( -4.806344283790351390, -7.508992741355383416, 25.00000000000000000 ) ) ;
#31175 = DIRECTION ( 'NONE',  ( 0.000000000000000000, 0.5767582926624970074, 0.8169148498130275327 ) ) ;
#31176 = AXIS2_PLACEMENT_3D ( 'NONE', #23876, #54461, #23537 ) ;
#31177 = DIRECTION ( 'NONE',  ( -1.000000000000000000, 0.000000000000000000, -0.000000000000000000 ) ) ;
#31178 = CARTESIAN_POINT ( 'NONE',  ( 0.2834382757447998502, -10.71064820518738969, -5.949714385480752377 ) ) ;
#31179 = LINE ( 'NONE', #56444, #44030 ) ;
#31180 = CIRCLE ( 'NONE', #52405, 4.000000000000000000 ) ;
#31181 = CARTESIAN_POINT ( 'NONE',  ( -35.00000000000000000, -3.340853584269456888, -11.26103545359859304 ) ) ;
#31182 = ADVANCED_FACE ( 'NONE', ( #43580 ), #48294, .T. ) ;
#31183 = VERTEX_POINT ( 'NONE', #3055 ) ;
#31184 = AXIS2_PLACEMENT_3D ( 'NONE', #26295, #51259, #21648 ) ;
#31185 = B_SPLINE_CURVE_WITH_KNOTS ( 'NONE', 3,
 ( #50939, #50297, #45286, #5062, #49953, #20336, #19708, #4752, #65544, #19376, #30629, #25326, #5387, #25659, #25013, #19039 ),
 .UNSPECIFIED., .F., .F.,
 ( 4, 3, 3, 3, 3, 4 ),
 ( 2.813154621161213038E-15, 0.0002126834539179820556, 0.0004253519300366505849, 0.0006380165497224521681, 0.0007442707582428671493, 0.0009453531351415104091 ),
 .UNSPECIFIED. ) ;
#31186 = ORIENTED_EDGE ( 'NONE', *, *, #35927, .F. ) ;
#31187 = CARTESIAN_POINT ( 'NONE',  ( 5.516018279890452902, 0.005976902763918716562, 0.003191189039764460479 ) ) ;
#31188 = EDGE_CURVE ( 'NONE', #47952, #57499, #58239, .T. ) ;
#31189 = ORIENTED_EDGE ( 'NONE', *, *, #49275, .F. ) ;
#31190 = FACE_OUTER_BOUND ( 'NONE', #21998, .T. ) ;
#31191 = CARTESIAN_POINT ( 'NONE',  ( -14.40132519092765939, 7.823324605749410132, -11.00218777330444020 ) ) ;
#31192 = CIRCLE ( 'NONE', #54560, 12.74999999999999822 ) ;
#31193 = DIRECTION ( 'NONE',  ( 1.000000000000000000, -0.000000000000000000, -0.000000000000000000 ) ) ;
#31194 = CARTESIAN_POINT ( 'NONE',  ( 2.288423627607358846, 2.464337058688887971, -7.242304196986070863 ) ) ;
#31195 = ORIENTED_EDGE ( 'NONE', *, *, #30829, .F. ) ;
#31196 = PLANE ( 'NONE',  #11244 ) ;
#31197 = CARTESIAN_POINT ( 'NONE',  ( 35.00000000000000000, 6.307491713049029336, -9.908974237959670361 ) ) ;
#31198 = CARTESIAN_POINT ( 'NONE',  ( 0.7446945582518242901, -12.27434006248818577, 1.802628359587700846 ) ) ;
#31199 = CARTESIAN_POINT ( 'NONE',  ( 3.152665057734040488, 0.000000000000000000, 0.000000000000000000 ) ) ;
#31200 = VECTOR ( 'NONE', #53720, 1000.000000000000000 ) ;
#31201 = CARTESIAN_POINT ( 'NONE',  ( -17.15271379239874250, -7.063395208604966058, 9.707307756281583266 ) ) ;
#31202 = CARTESIAN_POINT ( 'NONE',  ( 2.273267844204864385, 2.756477528575298042, 7.130811676080282879 ) ) ;
#31203 = ORIENTED_EDGE ( 'NONE', *, *, #38771, .F. ) ;
#31204 = CIRCLE ( 'NONE', #2561, 4.500000000000000888 ) ;
#31205 = DIRECTION ( 'NONE',  ( -0.000000000000000000, -1.000000000000000000, -0.000000000000000000 ) ) ;
#31206 = ORIENTED_EDGE ( 'NONE', *, *, #19856, .T. ) ;
#31207 = CARTESIAN_POINT ( 'NONE',  ( 35.00000000000000000, 12.74613886779084559, -0.3137578094509725357 ) ) ;
#31208 = CARTESIAN_POINT ( 'NONE',  ( 37.00000000000000711, 4.705694406421931860E-17, -3.469127814946512892E-15 ) ) ;
#31209 = CARTESIAN_POINT ( 'NONE',  ( -7.181456785175555524, -5.890186129966251904, -10.45493698471458188 ) ) ;
#31210 = DIRECTION ( 'NONE',  ( 1.000000000000000000, 0.000000000000000000, 0.000000000000000000 ) ) ;
#31211 = AXIS2_PLACEMENT_3D ( 'NONE', #20914, #4990, #41516 ) ;
#31212 = ORIENTED_EDGE ( 'NONE', *, *, #6692, .F. ) ;
#31213 = VERTEX_POINT ( 'NONE', #63864 ) ;
#31214 = DIRECTION ( 'NONE',  ( 1.000000000000000000, 0.000000000000000000, -0.000000000000000000 ) ) ;
#31215 = ORIENTED_EDGE ( 'NONE', *, *, #35469, .T. ) ;
#31216 = EDGE_CURVE ( 'NONE', #28521, #59877, #17926, .T. ) ;
#31217 = DIRECTION ( 'NONE',  ( -1.000000000000000000, 0.000000000000000000, 0.000000000000000000 ) ) ;
#31218 = CARTESIAN_POINT ( 'NONE',  ( 0.6920704694426910164, 0.4803808886326909056, -13.50000000000000178 ) ) ;
#31219 = CARTESIAN_POINT ( 'NONE',  ( -22.27718150314433387, -3.507884203786629129, -1.117371044661094937 ) ) ;
#31220 = DIRECTION ( 'NONE',  ( 0.000000000000000000, -0.7381862504171878836, 0.6745969609292743474 ) ) ;
#31221 = DIRECTION ( 'NONE',  ( 0.000000000000000000, 0.01356324068817998940, -0.9999080150203989437 ) ) ;
#31222 = CARTESIAN_POINT ( 'NONE',  ( 1.719304012341585253, 11.38834240361577521, -5.690355757825364513 ) ) ;
#31223 = DIRECTION ( 'NONE',  ( 0.000000000000000000, 0.01356324068817998940, -0.9999080150203990547 ) ) ;
#31224 = ORIENTED_EDGE ( 'NONE', *, *, #9097, .T. ) ;
#31225 = CIRCLE ( 'NONE', #1485, 5.000000000000001776 ) ;
#31226 = CARTESIAN_POINT ( 'NONE',  ( 35.00000000000000000, 8.258652103341434625, -8.352657516904704593 ) ) ;
#31227 = ORIENTED_EDGE ( 'NONE', *, *, #39929, .T. ) ;
#31228 = LINE ( 'NONE', #26238, #58900 ) ;
#31229 = AXIS2_PLACEMENT_3D ( 'NONE', #54692, #45024, #19097 ) ;
#31230 = CARTESIAN_POINT ( 'NONE',  ( 17.57949967008812209, 9.831142232691801652, 9.259614918201451772 ) ) ;
#31231 = ADVANCED_FACE ( 'NONE', ( #28964 ), #33625, .T. ) ;
#31232 = ORIENTED_EDGE ( 'NONE', *, *, #28219, .F. ) ;
#31233 = CARTESIAN_POINT ( 'NONE',  ( -22.27719443589224113, 3.601617131804403016, -0.7635131876694990494 ) ) ;
#31234 = ORIENTED_EDGE ( 'NONE', *, *, #11842, .F. ) ;
#31235 = DIRECTION ( 'NONE',  ( 1.000000000000000000, 0.000000000000000000, 0.000000000000000000 ) ) ;
#31236 = VECTOR ( 'NONE', #56742, 1000.000000000000000 ) ;
#31237 = CARTESIAN_POINT ( 'NONE',  ( 0.9232058338315058954, 10.60677148422253424, -6.559496812049550485 ) ) ;
#31238 = CARTESIAN_POINT ( 'NONE',  ( 2.305787727787084407, 3.971363876083963351, 6.545285700970541853 ) ) ;
#31239 = CARTESIAN_POINT ( 'NONE',  ( -48.36589927958296187, -0.3279091627047597268, 5.494672883103054239 ) ) ;
#31240 = VERTEX_POINT ( 'NONE', #38264 ) ;
#31241 = VERTEX_POINT ( 'NONE', #49271 ) ;
#31242 = CARTESIAN_POINT ( 'NONE',  ( -35.00000000000000000, -7.717887834988307105, 8.854740511458828678 ) ) ;
#31243 = VERTEX_POINT ( 'NONE', #18349 ) ;
#31244 = ADVANCED_FACE ( 'NONE', ( #3728 ), #18989, .T. ) ;
#31245 = CARTESIAN_POINT ( 'NONE',  ( -37.00000000000000711, 0.000000000000000000, 0.000000000000000000 ) ) ;
#31246 = ORIENTED_EDGE ( 'NONE', *, *, #34886, .F. ) ;
#31247 = VECTOR ( 'NONE', #7795, 1000.000000000000000 ) ;
#31248 = ORIENTED_EDGE ( 'NONE', *, *, #57082, .F. ) ;
#31249 = ORIENTED_EDGE ( 'NONE', *, *, #45035, .F. ) ;
#31250 = DIRECTION ( 'NONE',  ( -1.000000000000000000, 0.000000000000000000, 0.000000000000000000 ) ) ;
#31251 = CARTESIAN_POINT ( 'NONE',  ( 1.020182472820975184, 11.58401323226438606, 4.691131056021832002 ) ) ;
#31252 = CARTESIAN_POINT ( 'NONE',  ( 2.639814597422739162, -1.095525832903433416, -7.689608172406203757 ) ) ;
#31253 = CARTESIAN_POINT ( 'NONE',  ( 35.00000000000000000, -6.307491713048959170, 9.908974237959705889 ) ) ;
#31254 = DIRECTION ( 'NONE',  ( 0.000000000000000000, -0.01356324068817992001, 0.9999080150203990547 ) ) ;
#31255 = ORIENTED_EDGE ( 'NONE', *, *, #61041, .F. ) ;
#31256 = DIRECTION ( 'NONE',  ( -1.000000000000000000, 0.000000000000000000, 0.000000000000000000 ) ) ;
#31257 = ORIENTED_EDGE ( 'NONE', *, *, #53553, .F. ) ;
#31258 = DIRECTION ( 'NONE',  ( -1.000000000000000000, 0.000000000000000000, 0.000000000000000000 ) ) ;
#31259 = CIRCLE ( 'NONE', #38707, 5.000000000000000888 ) ;
#31260 = CARTESIAN_POINT ( 'NONE',  ( -3.026545681158347101, 9.064712759764015360, 10.02988752212787738 ) ) ;
#31261 = FACE_OUTER_BOUND ( 'NONE', #49640, .T. ) ;
#31262 = CARTESIAN_POINT ( 'NONE',  ( 0.3002738374340832572, -2.350339881555025379, 12.03040002643110640 ) ) ;
#31263 = CARTESIAN_POINT ( 'NONE',  ( 2.350038591457284554, -4.746773736940665955, -9.502240128961169319 ) ) ;
#31264 = CARTESIAN_POINT ( 'NONE',  ( 2.373367633546870525, -7.676289145832773109, -0.1808255748566272858 ) ) ;
#31265 = EDGE_CURVE ( 'NONE', #47037, #57528, #12429, .T. ) ;
#31266 = AXIS2_PLACEMENT_3D ( 'NONE', #46962, #62242, #31972 ) ;
#31267 = VERTEX_POINT ( 'NONE', #64212 ) ;
#31268 = CYLINDRICAL_SURFACE ( 'NONE', #7797, 4.999999999999999112 ) ;
#31269 =( BOUNDED_SURFACE ( )  B_SPLINE_SURFACE ( 3, 1, ( 
 ( #13571, #44479 ),
 ( #49190, #14541 ),
 ( #64439, #39175 ),
 ( #34185, #55124 ) ),
 .UNSPECIFIED., .F., .F., .F. ) 
 B_SPLINE_SURFACE_WITH_KNOTS ( ( 4, 4 ),
 ( 2, 2 ),
 ( 0.000000000000000000, 1.000000000000000000 ),
 ( 0.000000000000000000, 1.000000000000000000 ),
 .UNSPECIFIED. ) 
 GEOMETRIC_REPRESENTATION_ITEM ( )  RATIONAL_B_SPLINE_SURFACE ( (
 ( 1.000000000000000000, 1.000000000000000000),
 ( 0.9932032654565553509, 0.8386279382598736953),
 ( 0.9932032654565553509, 0.8386279382598736953),
 ( 1.000000000000000000, 1.000000000000000000) ) ) 
 REPRESENTATION_ITEM ( '' )  SURFACE ( )  );
#31270 = ORIENTED_EDGE ( 'NONE', *, *, #42702, .T. ) ;
#31271 = LINE ( 'NONE', #27574, #23213 ) ;
#31272 = CARTESIAN_POINT ( 'NONE',  ( 19.56743653832046803, -28.99999999999999645, -5.000000000000000888 ) ) ;
#31273 = CARTESIAN_POINT ( 'NONE',  ( 2.835339799623981971, 6.206025468804425849, -4.778327228934518445 ) ) ;
#31274 = DIRECTION ( 'NONE',  ( 0.000000000000000000, -0.01356324068817998593, 0.9999080150203990547 ) ) ;
#31275 = LINE ( 'NONE', #693, #7342 ) ;
#31276 = ORIENTED_EDGE ( 'NONE', *, *, #24110, .T. ) ;
#31277 = VECTOR ( 'NONE', #44057, 1000.000000000000000 ) ;
#31278 = AXIS2_PLACEMENT_3D ( 'NONE', #30138, #60074, #45753 ) ;
#31279 = FACE_OUTER_BOUND ( 'NONE', #34888, .T. ) ;
#31280 = DIRECTION ( 'NONE',  ( 0.000000000000000000, 0.8835120444460240474, -0.4684084406997882088 ) ) ;
#31281 = CARTESIAN_POINT ( 'NONE',  ( 2.000000000000001776, 3.859771122243123465, -5.613913289150012531 ) ) ;
#31282 = CARTESIAN_POINT ( 'NONE',  ( 0.000000000000000000, 0.000000000000000000, 0.000000000000000000 ) ) ;
#31283 = ADVANCED_FACE ( 'NONE', ( #18684 ), #38942, .T. ) ;
#31284 = CARTESIAN_POINT ( 'NONE',  ( 0.3109076770648991350, 12.25911371383828907, -0.2359198520041591307 ) ) ;
#31285 = LINE ( 'NONE', #41906, #26409 ) ;
#31286 = CARTESIAN_POINT ( 'NONE',  ( 0.3675815128205894289, -5.910255304480370953, -10.76447900494946452 ) ) ;
#31287 = CARTESIAN_POINT ( 'NONE',  ( 16.78263030916553333, -10.48479066935623827, 5.836879698929882565 ) ) ;
#31288 = FACE_OUTER_BOUND ( 'NONE', #6360, .T. ) ;
#31289 = AXIS2_PLACEMENT_3D ( 'NONE', #65385, #48817, #3266 ) ;
#31290 = ORIENTED_EDGE ( 'NONE', *, *, #21302, .F. ) ;
#31292 = ORIENTED_EDGE ( 'NONE', *, *, #12435, .F. ) ;
#31291 = EDGE_CURVE ( 'NONE', #37992, #32577, #24276, .T. ) ;
#31293 = CARTESIAN_POINT ( 'NONE',  ( 0.2653519789438759657, 2.148225749114993199, 12.05632450344283768 ) ) ;
#31294 = LINE ( 'NONE', #56911, #27950 ) ;
#31295 = CARTESIAN_POINT ( 'NONE',  ( -27.27855387000350262, 25.00000000000000000, 5.631341004100471892 ) ) ;
#31296 = CARTESIAN_POINT ( 'NONE',  ( -35.00000000000000000, 0.000000000000000000, 0.000000000000000000 ) ) ;
#31297 = EDGE_CURVE ( 'NONE', #59054, #42105, #40159, .T. ) ;
#31298 = ORIENTED_EDGE ( 'NONE', *, *, #38635, .T. ) ;
#31299 = ORIENTED_EDGE ( 'NONE', *, *, #63400, .T. ) ;
#31300 = ORIENTED_EDGE ( 'NONE', *, *, #40148, .F. ) ;
#31301 = DIRECTION ( 'NONE',  ( 0.000000000000000000, 0.000000000000000000, 1.000000000000000000 ) ) ;
#31302 = AXIS2_PLACEMENT_3D ( 'NONE', #18615, #1985, #64137 ) ;
#31303 = CARTESIAN_POINT ( 'NONE',  ( -22.71097035706202760, 2.118550233809425087, 4.510116093748266053 ) ) ;
#31304 = ADVANCED_FACE ( 'NONE', ( #65185 ), #9309, .T. ) ;
#31305 = ORIENTED_EDGE ( 'NONE', *, *, #61991, .T. ) ;
#31306 = CARTESIAN_POINT ( 'NONE',  ( -18.08686583997218378, 4.948971728452300489, -10.93424994070406697 ) ) ;
#31307 = DIRECTION ( 'NONE',  ( 0.000000000000000000, 0.000000000000000000, 1.000000000000000000 ) ) ;
#31308 = VERTEX_POINT ( 'NONE', #34899 ) ;
#31309 = CARTESIAN_POINT ( 'NONE',  ( -22.28629837673888048, 0.2936941584814525275, 3.697248502489080213 ) ) ;
#31310 = CARTESIAN_POINT ( 'NONE',  ( 19.27363075669124726, -29.98494805059728208, -5.891112176854690574 ) ) ;
#31311 = CARTESIAN_POINT ( 'NONE',  ( 2.251139882114757018, 7.133642337268560674, 2.728563091336710933 ) ) ;
#31312 = EDGE_LOOP ( 'NONE', ( #38464, #4844, #33126, #48165 ) ) ;
#31313 = CARTESIAN_POINT ( 'NONE',  ( 0.3675815128205912052, 12.13672785388552811, -1.872154644481959895 ) ) ;
#31314 = VERTEX_POINT ( 'NONE', #61188 ) ;
#31315 = ADVANCED_FACE ( 'NONE', ( #49902 ), #50241, .T. ) ;
#31316 = STYLED_ITEM ( 'NONE', ( #48496 ), #65033 ) ;
#31317 = DIRECTION ( 'NONE',  ( 0.000000000000000000, 0.9796553971857748788, 0.2006870767258854826 ) ) ;
#31318 = EDGE_LOOP ( 'NONE', ( #47985, #65743, #58077, #1652 ) ) ;
#31319 = DIRECTION ( 'NONE',  ( 0.000000000000000000, 1.000000000000000000, 0.000000000000000000 ) ) ;
#31320 = DIRECTION ( 'NONE',  ( -1.000000000000000000, 0.000000000000000000, 0.000000000000000000 ) ) ;
#31321 = CARTESIAN_POINT ( 'NONE',  ( 0.000000000000000000, -5.860254403322002759, -3.474373880649873403 ) ) ;
#31322 = CARTESIAN_POINT ( 'NONE',  ( 37.00000000000000711, -10.62137734850271364, -5.015831474386272859 ) ) ;
#31323 = CARTESIAN_POINT ( 'NONE',  ( 37.00000000000000711, -10.54834585426224081, -6.102719229070642015 ) ) ;
#31324 = DIRECTION ( 'NONE',  ( -1.000000000000000000, -0.000000000000000000, 0.000000000000000000 ) ) ;
#31325 = LINE ( 'NONE', #10699, #45242 ) ;
#31326 = CARTESIAN_POINT ( 'NONE',  ( 8.437200413559441614, 4.476360154859203355, -11.13383131558893346 ) ) ;
#31328 = ORIENTED_EDGE ( 'NONE', *, *, #30925, .F. ) ;
#31327 = DIRECTION ( 'NONE',  ( 0.000000000000000000, 0.01356324068817998940, -0.9999080150203990547 ) ) ;
#31329 = EDGE_CURVE ( 'NONE', #38122, #44608, #59242, .T. ) ;
#31330 = CARTESIAN_POINT ( 'NONE',  ( -37.00000000000000711, -10.99909370905153772, -5.246972444134135216 ) ) ;
#31331 = CIRCLE ( 'NONE', #15377, 6.936499999999986343 ) ;
#31332 = EDGE_LOOP ( 'NONE', ( #37898, #33938, #6077, #54226 ) ) ;
#31333 = FACE_OUTER_BOUND ( 'NONE', #65495, .T. ) ;
#31334 = CARTESIAN_POINT ( 'NONE',  ( 2.241352910868908754, 7.532448145350508995, 1.243507963608119438 ) ) ;
#31335 = VERTEX_POINT ( 'NONE', #59887 ) ;
#31336 = CYLINDRICAL_SURFACE ( 'NONE', #4185, 4.999999999999999112 ) ;
#31337 = CARTESIAN_POINT ( 'NONE',  ( 1.634816307077841424, 12.16351623921594260, -3.661851000130128320 ) ) ;
#31338 = FACE_OUTER_BOUND ( 'NONE', #46794, .T. ) ;
#31339 = DIRECTION ( 'NONE',  ( -1.000000000000000000, 0.000000000000000000, 0.000000000000000000 ) ) ;
#31340 = DIRECTION ( 'NONE',  ( -1.000000000000000000, 0.000000000000000000, 0.000000000000000000 ) ) ;
#31341 = EDGE_LOOP ( 'NONE', ( #34250, #27484, #4069, #1314 ) ) ;
#31342 = CARTESIAN_POINT ( 'NONE',  ( -18.73298729874495905, -4.205490829016433452, -11.23957459224111588 ) ) ;
#31343 = ORIENTED_EDGE ( 'NONE', *, *, #65175, .F. ) ;
#31344 = DIRECTION ( 'NONE',  ( -1.000000000000000000, 0.000000000000000000, 0.000000000000000000 ) ) ;
#31345 = CARTESIAN_POINT ( 'NONE',  ( -22.31328051695926007, -2.109671368890623455, -3.148362328073181615 ) ) ;
#31346 = CARTESIAN_POINT ( 'NONE',  ( -35.00000000000000000, 2.968224442958403486, 11.81949347079748058 ) ) ;
#31347 = ORIENTED_EDGE ( 'NONE', *, *, #54324, .T. ) ;
#31348 = CARTESIAN_POINT ( 'NONE',  ( -27.10128162969832388, -1.032914450114644334, 2.102429195189571942 ) ) ;
#31349 = EDGE_CURVE ( 'NONE', #46774, #20824, #19960, .T. ) ;
#31350 = AXIS2_PLACEMENT_3D ( 'NONE', #54676, #59650, #59317 ) ;
#31351 = CARTESIAN_POINT ( 'NONE',  ( -22.51237073810381162, -2.395115314842884757, -3.719289647955750233 ) ) ;
#31352 = CARTESIAN_POINT ( 'NONE',  ( 38.20713125073508110, -2.115151932665336076, 21.24219930640694898 ) ) ;
#31353 = DIRECTION ( 'NONE',  ( -1.000000000000000000, 0.000000000000000000, -0.000000000000000000 ) ) ;
#31354 = CARTESIAN_POINT ( 'NONE',  ( 10.16520822268187807, 8.041842148762462728, 10.84657292646973659 ) ) ;
#31355 = CARTESIAN_POINT ( 'NONE',  ( -9.197504613504056792, -11.40546504581821630, -3.730959538268487474 ) ) ;
#31356 = AXIS2_PLACEMENT_3D ( 'NONE', #1223, #31146, #56075 ) ;
#31357 = FACE_OUTER_BOUND ( 'NONE', #33504, .T. ) ;
#31358 = CARTESIAN_POINT ( 'NONE',  ( 2.665405856346786617, -9.549966053095406693, -0.5773576323838727209 ) ) ;
#31359 = EDGE_CURVE ( 'NONE', #40151, #42493, #1981, .T. ) ;
#31360 = ORIENTED_EDGE ( 'NONE', *, *, #39260, .F. ) ;
#31361 = CARTESIAN_POINT ( 'NONE',  ( -14.29135464769095520, 7.782112657557433977, 11.03126115115966499 ) ) ;
#31362 = CARTESIAN_POINT ( 'NONE',  ( 35.00000000000000000, 4.705694406421931860E-17, -3.469127814946512892E-15 ) ) ;
#31363 = ORIENTED_EDGE ( 'NONE', *, *, #11142, .F. ) ;
#31364 = EDGE_CURVE ( 'NONE', #61571, #24621, #29935, .T. ) ;
#31365 = CARTESIAN_POINT ( 'NONE',  ( 0.8375941296786741930, 10.57337970710546493, 6.548446001455325849 ) ) ;
#31366 = DIRECTION ( 'NONE',  ( -0.000000000000000000, -0.000000000000000000, -1.000000000000000000 ) ) ;
#31367 = CARTESIAN_POINT ( 'NONE',  ( -9.067636645460236622, 10.05071032021384703, -9.020536413389423913 ) ) ;
#31368 = ORIENTED_EDGE ( 'NONE', *, *, #6962, .F. ) ;
#31369 = CARTESIAN_POINT ( 'NONE',  ( 37.00000000000000711, -11.67026961469347768, -4.564151185897032725 ) ) ;
#31370 = DIRECTION ( 'NONE',  ( -1.000000000000000000, 0.000000000000000000, 0.000000000000000000 ) ) ;
#31371 = EDGE_CURVE ( 'NONE', #24519, #10393, #57192, .T. ) ;
#31372 = VERTEX_POINT ( 'NONE', #14951 ) ;
#31373 = CARTESIAN_POINT ( 'NONE',  ( 0.2739690278137261736, -5.965352196073669511, 10.69833303470763575 ) ) ;
#31374 = VERTEX_POINT ( 'NONE', #4701 ) ;
#31375 = ORIENTED_EDGE ( 'NONE', *, *, #2929, .T. ) ;
#31376 = VECTOR ( 'NONE', #23967, 1000.000000000000000 ) ;
#31377 = DIRECTION ( 'NONE',  ( 0.000000000000000000, -1.000000000000000000, 0.000000000000000000 ) ) ;
#31378 = EDGE_CURVE ( 'NONE', #15712, #63812, #29579, .T. ) ;
#31379 = EDGE_LOOP ( 'NONE', ( #63994, #20153, #16880, #53585 ) ) ;
#31380 = CARTESIAN_POINT ( 'NONE',  ( -26.91209319802521449, -10.55322015549179682, 5.712709916062060245 ) ) ;
#31381 = CARTESIAN_POINT ( 'NONE',  ( -22.28856623400852044, -3.573466130470485780, 1.018212315222191355 ) ) ;
#31382 = DIRECTION ( 'NONE',  ( -1.000000000000000000, 0.000000000000000000, 0.000000000000000000 ) ) ;
#31383 = DIRECTION ( 'NONE',  ( 0.000000000000000000, -0.8009703041134234036, -0.5987040770935587730 ) ) ;
#31384 = ORIENTED_EDGE ( 'NONE', *, *, #42803, .F. ) ;
#31385 = CARTESIAN_POINT ( 'NONE',  ( -18.58686583997225839, 5.151216734910813777, 10.83812558286603789 ) ) ;
#31386 = EDGE_CURVE ( 'NONE', #39606, #61650, #28492, .T. ) ;
#31387 = CARTESIAN_POINT ( 'NONE',  ( 11.41243050843482187, -29.26822538582518263, 7.243948608349396245 ) ) ;
#31388 = CARTESIAN_POINT ( 'NONE',  ( 37.00000000000000711, -0.2661492558802491804, 12.18359334611896294 ) ) ;
#31390 = VERTEX_POINT ( 'NONE', #45236 ) ;
#31389 = DIRECTION ( 'NONE',  ( 1.000000000000000000, 0.000000000000000000, 0.000000000000000000 ) ) ;
#31391 = CARTESIAN_POINT ( 'NONE',  ( 0.9232058338315048962, -11.84276737136203828, 3.908895078357480291 ) ) ;
#31392 = ORIENTED_EDGE ( 'NONE', *, *, #16498, .T. ) ;
#31393 = CARTESIAN_POINT ( 'NONE',  ( 0.2655924914740778187, 6.084990060696511271, 10.62761259256418889 ) ) ;
#31394 = ORIENTED_EDGE ( 'NONE', *, *, #8513, .T. ) ;
#31395 = VERTEX_POINT ( 'NONE', #65493 ) ;
#31396 = DIRECTION ( 'NONE',  ( 0.000000000000000000, -0.4380125133594037767, 0.8989688749565126757 ) ) ;
#31397 = ADVANCED_FACE ( 'NONE', ( #60519 ), #25271, .T. ) ;
#31398 = DIRECTION ( 'NONE',  ( -1.000000000000000000, 0.000000000000000000, 0.000000000000000000 ) ) ;
#31399 = LINE ( 'NONE', #16096, #9906 ) ;
#31400 = TOROIDAL_SURFACE ( 'NONE', #53681, 20.19615242270663558, 3.000000000000000000 ) ;
#31401 = EDGE_LOOP ( 'NONE', ( #16977, #19488, #5374, #9603 ) ) ;
#31402 = FACE_OUTER_BOUND ( 'NONE', #18935, .T. ) ;
#31403 = CARTESIAN_POINT ( 'NONE',  ( 1.198791140417946988, -2.686891236232506586, 12.26651935498910184 ) ) ;
#31404 = CARTESIAN_POINT ( 'NONE',  ( 0.2717059086739030405, -12.03041489115253349, 2.300075171420195019 ) ) ;
#31406 = ORIENTED_EDGE ( 'NONE', *, *, #54758, .T. ) ;
#31405 = EDGE_CURVE ( 'NONE', #16904, #52157, #55873, .T. ) ;
#31407 = ORIENTED_EDGE ( 'NONE', *, *, #38182, .F. ) ;
#31408 = CARTESIAN_POINT ( 'NONE',  ( 37.00000000000000711, 4.705694406421931860E-17, -3.469127814946512892E-15 ) ) ;
#31409 = VERTEX_POINT ( 'NONE', #15302 ) ;
#31410 = ADVANCED_FACE ( 'NONE', ( #35577 ), #30579, .T. ) ;
#31411 = ORIENTED_EDGE ( 'NONE', *, *, #35521, .T. ) ;
#31412 = DIRECTION ( 'NONE',  ( -0.8514458006899927600, 0.000000000000000000, -0.5244426074294281648 ) ) ;
#31413 = CARTESIAN_POINT ( 'NONE',  ( -25.54417658651491863, -7.498517398407823720, 11.22596262356930197 ) ) ;
#31414 = DIRECTION ( 'NONE',  ( 1.000000000000000000, 0.000000000000000000, 0.000000000000000000 ) ) ;
#31415 = CARTESIAN_POINT ( 'NONE',  ( -22.29978294495153790, 1.052446240539720357, 3.598607126810713375 ) ) ;
#31416 = DIRECTION ( 'NONE',  ( -1.000000000000000000, 0.000000000000000000, 0.000000000000000000 ) ) ;
#31417 = FACE_OUTER_BOUND ( 'NONE', #60815, .T. ) ;
#31418 = PLANE ( 'NONE',  #17436 ) ;
#31419 = CIRCLE ( 'NONE', #2774, 5.000000000000001776 ) ;
#31420 = ORIENTED_EDGE ( 'NONE', *, *, #49969, .T. ) ;
#31421 = CARTESIAN_POINT ( 'NONE',  ( 0.2646305136544065406, 6.237419468587079407, 10.53923716745248917 ) ) ;
#31422 = CARTESIAN_POINT ( 'NONE',  ( 35.00000000000000000, 11.98254675519227952, -2.220215194441947482 ) ) ;
#31423 = CIRCLE ( 'NONE', #17634, 2.899999999999995026 ) ;
#31424 = EDGE_CURVE ( 'NONE', #9122, #16609, #25316, .T. ) ;
#31425 = CARTESIAN_POINT ( 'NONE',  ( 0.2833330754217412428, 4.379886056891059809, -11.44258640049857512 ) ) ;
#31426 = ADVANCED_FACE ( 'NONE', ( #1979 ), #32222, .T. ) ;
#31427 = DIRECTION ( 'NONE',  ( 0.9606638835031803270, -0.2762341707520458711, 0.02862840969242822636 ) ) ;
#31428 = DIRECTION ( 'NONE',  ( 1.000000000000000000, 0.000000000000000000, 0.000000000000000000 ) ) ;
#31429 = CARTESIAN_POINT ( 'NONE',  ( 0.6511581176971786844, 2.473966499148548603, -12.12498040206563665 ) ) ;
#31430 = CARTESIAN_POINT ( 'NONE',  ( 10.39074034058834428, 0.7556363488327733080, -11.97742577131518971 ) ) ;
#31431 = EDGE_LOOP ( 'NONE', ( #52006, #21328, #31689, #42854 ) ) ;
#31432 = CARTESIAN_POINT ( 'NONE',  ( -35.00000000000000000, -9.060822531526103063, 7.474872387600973944 ) ) ;
#31433 = CARTESIAN_POINT ( 'NONE',  ( 0.2653141617320998735, 10.58343467791296533, 6.161204121352730212 ) ) ;
#31434 = DIRECTION ( 'NONE',  ( -1.000000000000000000, 0.000000000000000000, -0.000000000000000000 ) ) ;
#31435 = EDGE_CURVE ( 'NONE', #64587, #40917, #22248, .T. ) ;
#31436 = CARTESIAN_POINT ( 'NONE',  ( 16.10065672031746331, -35.00000000000000711, 4.574893970807607957 ) ) ;
#31437 = EDGE_CURVE ( 'NONE', #50142, #57779, #1668, .T. ) ;
#31438 = CARTESIAN_POINT ( 'NONE',  ( 12.52750123246316249, 0.4973700281276248192, -13.49083477977253764 ) ) ;
#31439 = CARTESIAN_POINT ( 'NONE',  ( -47.00000000000000711, 0.000000000000000000, 0.000000000000000000 ) ) ;
#31440 = VERTEX_POINT ( 'NONE', #46541 ) ;
#31441 = CYLINDRICAL_SURFACE ( 'NONE', #58847, 5.000000000000000888 ) ;
#31442 = FACE_OUTER_BOUND ( 'NONE', #25174, .T. ) ;
#31443 = CARTESIAN_POINT ( 'NONE',  ( 2.261269890822073414, 1.189259211195942800, 7.547924622047982091 ) ) ;
#31444 = ORIENTED_EDGE ( 'NONE', *, *, #9284, .F. ) ;
#31445 = CARTESIAN_POINT ( 'NONE',  ( 3.031336079629544322, 7.038432939676056321, 3.582646412484421727 ) ) ;
#31446 = FACE_OUTER_BOUND ( 'NONE', #25232, .T. ) ;
#31447 = CARTESIAN_POINT ( 'NONE',  ( 5.520433897694421610, 0.003119431460922217261, 0.01473594271720289964 ) ) ;
#31448 = ADVANCED_FACE ( 'NONE', ( #26266 ), #36891, .T. ) ;
#31450 = ORIENTED_EDGE ( 'NONE', *, *, #52496, .T. ) ;
#31449 = CARTESIAN_POINT ( 'NONE',  ( -22.76187086591099984, 0.9059972289356981179, 5.055065309934907880 ) ) ;
#31451 = DIRECTION ( 'NONE',  ( 1.000000000000000000, 0.000000000000000000, 0.000000000000000000 ) ) ;
#31452 = VECTOR ( 'NONE', #50635, 1000.000000000000000 ) ;
#31453 = CARTESIAN_POINT ( 'NONE',  ( -26.74023318801842919, -3.342010596062586547, -0.2829279580742295463 ) ) ;
#31454 = EDGE_LOOP ( 'NONE', ( #36381, #25640, #10971, #62164 ) ) ;
#31455 = CARTESIAN_POINT ( 'NONE',  ( -22.51237073810381517, 3.719289647955755118, -2.395115314842871435 ) ) ;
#31456 = CARTESIAN_POINT ( 'NONE',  ( 35.00000000000000000, -7.817492529713787164, 9.348667969174485393 ) ) ;
#31457 = CARTESIAN_POINT ( 'NONE',  ( 0.2653519890518161728, -7.871697161810750742, 9.381137101569645864 ) ) ;
#31458 = DIRECTION ( 'NONE',  ( -0.6151304903148129277, 0.000000000000000000, -0.7884253166185480888 ) ) ;
#31459 =( BOUNDED_SURFACE ( )  B_SPLINE_SURFACE ( 3, 1, ( 
 ( #26593, #46886 ),
 ( #16629, #36898 ),
 ( #48535, #8283 ),
 ( #6978, #42194 ) ),
 .UNSPECIFIED., .F., .F., .F. ) 
 B_SPLINE_SURFACE_WITH_KNOTS ( ( 4, 4 ),
 ( 2, 2 ),
 ( 0.000000000000000000, 1.000000000000000000 ),
 ( 0.000000000000000000, 1.000000000000000000 ),
 .UNSPECIFIED. ) 
 GEOMETRIC_REPRESENTATION_ITEM ( )  RATIONAL_B_SPLINE_SURFACE ( (
 ( 1.000000000000000000, 1.000000000000000000),
 ( 0.9856612449720755231, 0.9999558406602322425),
 ( 0.9856612449720755231, 0.9999558406602322425),
 ( 1.000000000000000000, 1.000000000000000000) ) ) 
 REPRESENTATION_ITEM ( '' )  SURFACE ( )  );
#31460 = CARTESIAN_POINT ( 'NONE',  ( -27.01437459610461644, -10.69338818478079922, -8.240233560378637634 ) ) ;
#31461 = EDGE_CURVE ( 'NONE', #51508, #6431, #30910, .T. ) ;
#31462 = CARTESIAN_POINT ( 'NONE',  ( 35.00000000000000000, 12.57916205664484188, 2.080187960898425281 ) ) ;
#31464 = ORIENTED_EDGE ( 'NONE', *, *, #53555, .F. ) ;
#31463 = CARTESIAN_POINT ( 'NONE',  ( 0.2834382757448035139, 11.44241760114840467, -4.380429851625208926 ) ) ;
#31465 = EDGE_CURVE ( 'NONE', #28103, #55517, #11548, .T. ) ;
#31466 = ORIENTED_EDGE ( 'NONE', *, *, #23326, .F. ) ;
#31467 = ORIENTED_EDGE ( 'NONE', *, *, #27432, .F. ) ;
#31468 = DIRECTION ( 'NONE',  ( 0.000000000000000000, -0.7107927964194477033, 0.7034014504948232771 ) ) ;
#31469 = DIRECTION ( 'NONE',  ( -1.000000000000000000, 0.000000000000000000, 0.000000000000000000 ) ) ;
#31470 = EDGE_CURVE ( 'NONE', #38028, #22451, #24317, .T. ) ;
#31471 = CARTESIAN_POINT ( 'NONE',  ( 2.430348790457563357, 1.528169972228492712, 7.544199152379105655 ) ) ;
#31472 = EDGE_CURVE ( 'NONE', #3051, #53717, #24172, .T. ) ;
#31473 = CARTESIAN_POINT ( 'NONE',  ( 1.719304012341460908, 3.626341562669523011, -12.20344780066162649 ) ) ;
#31474 = EDGE_LOOP ( 'NONE', ( #32567, #28366, #6608, #8049 ) ) ;
#31475 = DIRECTION ( 'NONE',  ( -1.000000000000000000, -0.000000000000000000, -0.000000000000000000 ) ) ;
#31476 = CARTESIAN_POINT ( 'NONE',  ( -36.00000000000000711, 7.608228585767727203, 10.23119532541075394 ) ) ;
#31477 = CARTESIAN_POINT ( 'NONE',  ( -22.27711351828769892, -1.028167152775512516, 3.534923377568736313 ) ) ;
#31478 = EDGE_LOOP ( 'NONE', ( #51707, #27311, #40127, #59600 ) ) ;
#31479 = ORIENTED_EDGE ( 'NONE', *, *, #25384, .F. ) ;
#31480 = EDGE_CURVE ( 'NONE', #37413, #20683, #5678, .T. ) ;
#31481 = CARTESIAN_POINT ( 'NONE',  ( 28.12675480332037736, -12.24425775564703045, 5.696251083233389245 ) ) ;
#31482 = VERTEX_POINT ( 'NONE', #16290 ) ;
#31483 = CARTESIAN_POINT ( 'NONE',  ( 21.95708534023389191, -11.48706736601068990, -3.476045417500702062 ) ) ;
#31484 = CARTESIAN_POINT ( 'NONE',  ( 0.000000000000000000, 6.606214214351074254, 2.114938770769925647 ) ) ;
#31485 = DIRECTION ( 'NONE',  ( 0.000000000000000000, -0.9987865678893281807, 0.04924826701373505311 ) ) ;
#31486 = DIRECTION ( 'NONE',  ( 0.000000000000000000, -0.9970832820307031774, -0.07632122047557582389 ) ) ;
#31487 = CYLINDRICAL_SURFACE ( 'NONE', #5454, 12.18650000000000055 ) ;
#31488 = LINE ( 'NONE', #51787, #21118 ) ;
#31489 = CARTESIAN_POINT ( 'NONE',  ( 1.719304012339844867, -11.67935079956417610, 5.066286238786176455 ) ) ;
#31490 = ORIENTED_EDGE ( 'NONE', *, *, #51300, .T. ) ;
#31491 = DIRECTION ( 'NONE',  ( 0.000000000000000000, -0.01356324068817991481, 0.9999080150203990547 ) ) ;
#31492 = CARTESIAN_POINT ( 'NONE',  ( 2.770579946183338915, 4.165025702425937837, -6.607710183380588020 ) ) ;
#31493 = DIRECTION ( 'NONE',  ( -1.000000000000000000, 0.000000000000000000, 0.000000000000000000 ) ) ;
#31494 = CARTESIAN_POINT ( 'NONE',  ( 36.00000000000000711, -12.74613886779084382, 0.3137578094510532489 ) ) ;
#31495 = CARTESIAN_POINT ( 'NONE',  ( 3.152665057735194232, -3.161213418914472051, -7.281573230474045921 ) ) ;
#31496 = CARTESIAN_POINT ( 'NONE',  ( -37.00000000000000711, -11.30684963584386260, -4.545979934229533725 ) ) ;
#31497 = ORIENTED_EDGE ( 'NONE', *, *, #62771, .T. ) ;
#31498 = EDGE_CURVE ( 'NONE', #49238, #47989, #43887, .T. ) ;
#31499 = ORIENTED_EDGE ( 'NONE', *, *, #32616, .F. ) ;
#31500 = CARTESIAN_POINT ( 'NONE',  ( 36.00000000000000711, -7.608228585767796481, -10.23119532541070420 ) ) ;
#31501 = VECTOR ( 'NONE', #14109, 1000.000000000000000 ) ;
#31502 = EDGE_CURVE ( 'NONE', #48023, #53160, #48733, .T. ) ;
#31503 = ORIENTED_EDGE ( 'NONE', *, *, #38104, .T. ) ;
#31504 = CARTESIAN_POINT ( 'NONE',  ( 2.000000000000001776, -1.145812388885151023, 6.715725538143585638 ) ) ;
#31505 = DIRECTION ( 'NONE',  ( -1.000000000000000000, 0.000000000000000000, 0.000000000000000000 ) ) ;
#31506 = CARTESIAN_POINT ( 'NONE',  ( 20.00005080000000035, 3.872983346207417021, 1.000000000000000000 ) ) ;
#31507 = DIRECTION ( 'NONE',  ( 0.000000000000000000, 0.2006870767258890631, -0.9796553971857742127 ) ) ;
#31508 = ORIENTED_EDGE ( 'NONE', *, *, #16502, .F. ) ;
#31509 = DIRECTION ( 'NONE',  ( -1.000000000000000000, -0.000000000000000000, -0.000000000000000000 ) ) ;
#31510 = EDGE_CURVE ( 'NONE', #9279, #46246, #11940, .T. ) ;
#31511 = CARTESIAN_POINT ( 'NONE',  ( 1.198791140418998813, -12.44572864632790932, 1.670544840358051841 ) ) ;
#31512 = CARTESIAN_POINT ( 'NONE',  ( -33.80171706282990840, -2.756546641835186051, 23.41361577495085200 ) ) ;
#31513 = CARTESIAN_POINT ( 'NONE',  ( 0.2833330754217385228, 6.300330022379362127, -10.50818856955511471 ) ) ;
#31514 = CARTESIAN_POINT ( 'NONE',  ( 2.280717697723836146, 2.762096098144338985, 7.131299706077038003 ) ) ;
#31515 = VERTEX_POINT ( 'NONE', #47534 ) ;
#31516 = DIRECTION ( 'NONE',  ( 0.000000000000000000, 0.8169148498130255343, -0.5767582926624998940 ) ) ;
#31517 = VERTEX_POINT ( 'NONE', #42509 ) ;
#31518 = CARTESIAN_POINT ( 'NONE',  ( -22.28506771379528573, 3.575989816848481162, -1.050362426369340296 ) ) ;
#31519 = CARTESIAN_POINT ( 'NONE',  ( 2.000000000000001776, -3.152010634611731366, 6.039758645301271933 ) ) ;
#31520 = CARTESIAN_POINT ( 'NONE',  ( 2.655192694323875280, -9.337840456948674372, 2.234846078477743969 ) ) ;
#31521 = ADVANCED_FACE ( 'NONE', ( #16621 ), #52204, .T. ) ;
#31522 = CARTESIAN_POINT ( 'NONE',  ( -35.00000000000000000, 11.35427606708812753, -4.426194442447117794 ) ) ;
#31523 = EDGE_CURVE ( 'NONE', #55926, #8645, #57227, .T. ) ;
#31524 = LINE ( 'NONE', #51176, #63875 ) ;
#31525 = ORIENTED_EDGE ( 'NONE', *, *, #48536, .F. ) ;
#31526 = ORIENTED_EDGE ( 'NONE', *, *, #54926, .F. ) ;
#31527 = CARTESIAN_POINT ( 'NONE',  ( -29.58743033447366244, 2.139843039584942375, 11.81524931570010395 ) ) ;
#31528 = VERTEX_POINT ( 'NONE', #56875 ) ;
#31529 = CARTESIAN_POINT ( 'NONE',  ( 3.381510803510703322, 5.478318359161011841, 10.67863534124962221 ) ) ;
#31530 = CARTESIAN_POINT ( 'NONE',  ( -36.00000000000000711, 11.80185301892987582, -4.824807283153996096 ) ) ;
#31531 = DIRECTION ( 'NONE',  ( 0.000000000000000000, 0.000000000000000000, 1.000000000000000000 ) ) ;
#31532 = CARTESIAN_POINT ( 'NONE',  ( 35.00000000000000000, 10.80631716521673447, 4.603882218679430594 ) ) ;
#31533 = CARTESIAN_POINT ( 'NONE',  ( 1.198791140419928070, -7.669598593074918647, -9.943044756149140184 ) ) ;
#31534 = CARTESIAN_POINT ( 'NONE',  ( 10.66583743953262342, 7.973724152180637681, -8.969682718315050707 ) ) ;
#31535 = CARTESIAN_POINT ( 'NONE',  ( 37.00000000000000711, 10.93004082984027825, 6.564808257521646873 ) ) ;
#31536 = ORIENTED_EDGE ( 'NONE', *, *, #30605, .F. ) ;
#31537 = CARTESIAN_POINT ( 'NONE',  ( -9.326486438888442976, -10.62366522422245296, -5.593402933327412008 ) ) ;
#31538 = ORIENTED_EDGE ( 'NONE', *, *, #63955, .F. ) ;
#31539 = AXIS2_PLACEMENT_3D ( 'NONE', #17992, #52606, #32288 ) ;
#31540 = EDGE_CURVE ( 'NONE', #64820, #17169, #11643, .T. ) ;
#31541 = FACE_OUTER_BOUND ( 'NONE', #22173, .T. ) ;
#31542 = CARTESIAN_POINT ( 'NONE',  ( -35.00000000000000000, -11.73463472867573643, -3.287724142101541958 ) ) ;
#31543 = VERTEX_POINT ( 'NONE', #11301 ) ;
#31544 = AXIS2_PLACEMENT_3D ( 'NONE', #47578, #48907, #43903 ) ;
#31545 = ADVANCED_FACE ( 'NONE', ( #26922, #47222 ), #18263, .T. ) ;
#31546 = CARTESIAN_POINT ( 'NONE',  ( -35.00000000000000000, -12.16632754454237464, 0.7008968033238341944 ) ) ;
#31547 = ORIENTED_EDGE ( 'NONE', *, *, #32575, .T. ) ;
#31548 = CARTESIAN_POINT ( 'NONE',  ( 36.00000000000000711, -11.96656215839371917, -4.400442035670902641 ) ) ;
#31549 = CARTESIAN_POINT ( 'NONE',  ( -15.83540182711246835, -34.24586518154816872, -7.348477566591427923 ) ) ;
#31550 = CARTESIAN_POINT ( 'NONE',  ( 2.653899356900128126, 2.902068786425453073, 7.209790345489556884 ) ) ;
#31551 = ORIENTED_EDGE ( 'NONE', *, *, #25371, .T. ) ;
#31552 = ORIENTED_EDGE ( 'NONE', *, *, #63706, .T. ) ;
#31553 = ADVANCED_FACE ( 'NONE', ( #48522 ), #7314, .T. ) ;
#31554 = CARTESIAN_POINT ( 'NONE',  ( -9.351388602708162523, 11.42638970207765681, -3.665735721005252135 ) ) ;
#31555 = ORIENTED_EDGE ( 'NONE', *, *, #11134, .F. ) ;
#31556 = CARTESIAN_POINT ( 'NONE',  ( 0.2869720083484362805, 11.58405933820307077, -3.994435966589948706 ) ) ;
#31557 = ORIENTED_EDGE ( 'NONE', *, *, #34653, .F. ) ;
#31558 = ORIENTED_EDGE ( 'NONE', *, *, #39165, .F. ) ;
#31559 = EDGE_LOOP ( 'NONE', ( #15082, #50556, #24309, #58877 ) ) ;
#31560 = DIRECTION ( 'NONE',  ( 1.000000000000000000, 0.000000000000000000, -0.000000000000000000 ) ) ;
#31561 = DIRECTION ( 'NONE',  ( -1.000000000000000000, 0.000000000000000000, 0.000000000000000000 ) ) ;
#31562 = CARTESIAN_POINT ( 'NONE',  ( 3.100650473569749987, -0.9283202922944330249, -7.866294126167268530 ) ) ;
#31563 = CARTESIAN_POINT ( 'NONE',  ( -27.15511094194037867, 1.124668417986074864, -2.237231637349071711 ) ) ;
#31564 = CARTESIAN_POINT ( 'NONE',  ( 35.00000000000000000, 1.113475361586666157, 12.70128625845191017 ) ) ;
#31565 = VERTEX_POINT ( 'NONE', #28877 ) ;
#31566 = LINE ( 'NONE', #61830, #37513 ) ;
#31567 = ORIENTED_EDGE ( 'NONE', *, *, #2249, .T. ) ;
#31568 = DIRECTION ( 'NONE',  ( 0.000000000000000000, 0.9847383929261610547, -0.1740410799127650732 ) ) ;
#31569 = CYLINDRICAL_SURFACE ( 'NONE', #40509, 2.899999999999994582 ) ;
#31570 = DIRECTION ( 'NONE',  ( 1.000000000000000000, 0.000000000000000000, -0.000000000000000000 ) ) ;
#31571 = CARTESIAN_POINT ( 'NONE',  ( -37.00000000000000711, -0.06441628369844948354, 12.18632975068353019 ) ) ;
#31572 = CARTESIAN_POINT ( 'NONE',  ( -35.00000000000000000, 1.262958560998759472, 12.12087942037210198 ) ) ;
#31573 = CARTESIAN_POINT ( 'NONE',  ( 0.4626703367449018223, -10.51809671647426292, -6.399577980714925118 ) ) ;
#31574 =( GEOMETRIC_REPRESENTATION_CONTEXT ( 3 ) GLOBAL_UNCERTAINTY_ASSIGNED_CONTEXT ( ( #12377 ) ) GLOBAL_UNIT_ASSIGNED_CONTEXT ( ( #22659, #37934, #28294 ) ) REPRESENTATION_CONTEXT ( 'NONE', 'WORKASPACE' ) );
#31575 = ORIENTED_EDGE ( 'NONE', *, *, #34947, .T. ) ;
#31576 = CARTESIAN_POINT ( 'NONE',  ( -14.47334165536100059, 7.347880794884120722E-16, 6.000000000000000888 ) ) ;
#31577 = EDGE_CURVE ( 'NONE', #1650, #10081, #65684, .T. ) ;
#31578 = ORIENTED_EDGE ( 'NONE', *, *, #38287, .T. ) ;
#31579 = CARTESIAN_POINT ( 'NONE',  ( 5.530133899448235191, 0.01293763278443408986, -0.009387834778845371292 ) ) ;
#31580 = CARTESIAN_POINT ( 'NONE',  ( -1.994964832131320920, -25.76766306558319286, -15.60102351411471666 ) ) ;
#31581 = CARTESIAN_POINT ( 'NONE',  ( 2.573738926104375047, 6.081632213771451134, -4.796056562246111987 ) ) ;
#31582 = DIRECTION ( 'NONE',  ( 0.000000000000000000, -0.01356324068817991828, 0.9999080150203990547 ) ) ;
#31583 = CARTESIAN_POINT ( 'NONE',  ( 12.93723047338301058, 4.476360154859203355, 25.00000000000000000 ) ) ;
#31584 = ORIENTED_EDGE ( 'NONE', *, *, #17864, .T. ) ;
#31585 = CARTESIAN_POINT ( 'NONE',  ( 2.903928887688294491, 3.918141038919765062, -7.845932231841970861 ) ) ;
#31586 = CARTESIAN_POINT ( 'NONE',  ( 0.2657645697724696499, 2.275433120353249627, -12.03308811492266805 ) ) ;
#31587 = CARTESIAN_POINT ( 'NONE',  ( 21.62857653820161019, 11.91062359620538658, -1.517306329825557576 ) ) ;
#31588 = AXIS2_PLACEMENT_3D ( 'NONE', #57098, #32128, #11522 ) ;
#31589 = DIRECTION ( 'NONE',  ( -1.000000000000000000, -0.000000000000000000, -0.000000000000000000 ) ) ;
#31590 = AXIS2_PLACEMENT_3D ( 'NONE', #46760, #62366, #41769 ) ;
#31591 = DIRECTION ( 'NONE',  ( -1.000000000000000000, 0.000000000000000000, 0.000000000000000000 ) ) ;
#31592 = CARTESIAN_POINT ( 'NONE',  ( -22.28506771379528573, 0.2569416992704561253, 3.718191140878643441 ) ) ;
#31594 = ADVANCED_FACE ( 'NONE', ( #37875 ), #42855, .T. ) ;
#31593 = CARTESIAN_POINT ( 'NONE',  ( 0.2652384529303141170, -2.061422456317107077, 12.07141085622971666 ) ) ;
#31595 = CARTESIAN_POINT ( 'NONE',  ( -19.10799584608659885, -11.93643250936202271, -1.402863707794529846 ) ) ;
#31596 = CARTESIAN_POINT ( 'NONE',  ( 0.3665391374699465965, 7.691255657244421506, -9.576575648338943481 ) ) ;
#31597 = B_SPLINE_CURVE_WITH_KNOTS ( 'NONE', 3,
 ( #14170, #9496, #19830, #48791, #13206, #39440, #4553, #29163, #19169, #55065, #49760, #18850, #28484, #33793, #23855, #44116 ),
 .UNSPECIFIED., .F., .F.,
 ( 4, 3, 3, 3, 3, 4 ),
 ( 2.710505431213761567E-19, 0.0003017745587525280659, 0.0006035491769808807878, 0.0009053241094668280659, 0.001207275924540836525, 0.001510325902534664921 ),
 .UNSPECIFIED. ) ;
#31598 = EDGE_CURVE ( 'NONE', #58669, #33072, #38527, .T. ) ;
#31599 = EDGE_LOOP ( 'NONE', ( #38157, #40129, #20485, #11121 ) ) ;
#31600 = ORIENTED_EDGE ( 'NONE', *, *, #42795, .F. ) ;
#31601 = CYLINDRICAL_SURFACE ( 'NONE', #9820, 5.000000000000000888 ) ;
#31602 = CARTESIAN_POINT ( 'NONE',  ( 39.58329824467850244, -1.898237318462468792, -19.07749194152998129 ) ) ;
#31603 = DIRECTION ( 'NONE',  ( 0.000000000000000000, 0.9999080150203989437, 0.01356324068818348313 ) ) ;
#31604 = CYLINDRICAL_SURFACE ( 'NONE', #15887, 12.18650000000000055 ) ;
#31605 = ORIENTED_EDGE ( 'NONE', *, *, #64683, .T. ) ;
#31606 = ORIENTED_EDGE ( 'NONE', *, *, #38374, .T. ) ;
#31607 = ORIENTED_EDGE ( 'NONE', *, *, #2793, .T. ) ;
#31608 = CARTESIAN_POINT ( 'NONE',  ( 27.16179963944285447, -11.36021166003125593, 3.882017433740367895 ) ) ;
#31609 = EDGE_CURVE ( 'NONE', #12385, #48435, #58164, .T. ) ;
#31610 = CIRCLE ( 'NONE', #2984, 12.74999999999999822 ) ;
#31611 = DIRECTION ( 'NONE',  ( -1.000000000000000000, 0.000000000000000000, 0.000000000000000000 ) ) ;
#31612 = ORIENTED_EDGE ( 'NONE', *, *, #24767, .F. ) ;
#31613 = CARTESIAN_POINT ( 'NONE',  ( 35.00000000000000000, 11.70009620280413110, 1.039216533672774112 ) ) ;
#31614 = FACE_OUTER_BOUND ( 'NONE', #43222, .T. ) ;
#31616 = ORIENTED_EDGE ( 'NONE', *, *, #45035, .T. ) ;
#31615 = AXIS2_PLACEMENT_3D ( 'NONE', #57105, #62389, #26833 ) ;
#31617 = CARTESIAN_POINT ( 'NONE',  ( 2.297017764050236277, 4.791851130936026770, -5.967068736727147993 ) ) ;
#31618 = CARTESIAN_POINT ( 'NONE',  ( 14.19127861765052501, -30.11167671974727256, -5.095448428665124041 ) ) ;
#31619 = CARTESIAN_POINT ( 'NONE',  ( 24.65204228265436726, -2.300319471321356612, 11.77898663366571341 ) ) ;
#31620 = ORIENTED_EDGE ( 'NONE', *, *, #49771, .T. ) ;
#31621 = AXIS2_PLACEMENT_3D ( 'NONE', #15763, #5840, #50399 ) ;
#31622 = DIRECTION ( 'NONE',  ( 1.000000000000000000, -0.000000000000000000, -0.000000000000000000 ) ) ;
#31623 = ORIENTED_EDGE ( 'NONE', *, *, #4761, .T. ) ;
#31624 = CARTESIAN_POINT ( 'NONE',  ( 0.7400311444011693496, 7.698344902199217188, -9.726551103566730916 ) ) ;
#31625 = AXIS2_PLACEMENT_3D ( 'NONE', #39677, #9393, #49985 ) ;
#31626 = B_SPLINE_CURVE_WITH_KNOTS ( 'NONE', 3,
 ( #35853, #30876, #48990, #51196, #5648, #49330, #3448, #24340, #59279, #14033, #44293, #23716, #33987, #44606, #54638, #8739, #64564, #19038, #34324 ),
 .UNSPECIFIED., .F., .F.,
 ( 4, 3, 3, 3, 3, 3, 4 ),
 ( 7.903714856861513238E-18, 4.457896483014812754E-05, 6.639290541542165714E-05, 8.820687556479086513E-05, 0.0001100173248778937932, 0.0001545671401658124818, 0.0001830328308068605555 ),
 .UNSPECIFIED. ) ;
#31627 = CARTESIAN_POINT ( 'NONE',  ( 2.241352910868908310, 4.970878533273761946, 5.794346703933863196 ) ) ;
#31628 = CARTESIAN_POINT ( 'NONE',  ( -35.00000000000000000, -10.23119532541078058, 7.608228585767690788 ) ) ;
#31629 = EDGE_CURVE ( 'NONE', #10704, #12415, #32794, .T. ) ;
#31630 = DIRECTION ( 'NONE',  ( -1.000000000000000000, -0.000000000000000000, 0.000000000000000000 ) ) ;
#31631 = CARTESIAN_POINT ( 'NONE',  ( 2.241528039335007882, -6.619488482362960724, 3.803597072146510438 ) ) ;
#31632 = VECTOR ( 'NONE', #49646, 1000.000000000000000 ) ;
#31633 = DIRECTION ( 'NONE',  ( 0.000000000000000000, 0.01356324068817998940, -0.9999080150203990547 ) ) ;
#31634 = CYLINDRICAL_SURFACE ( 'NONE', #63176, 4.999999999999999112 ) ;
#31635 = ORIENTED_EDGE ( 'NONE', *, *, #4956, .F. ) ;
#31636 =( BOUNDED_SURFACE ( )  B_SPLINE_SURFACE ( 3, 1, ( 
 ( #37105, #37442 ),
 ( #12172, #22485 ),
 ( #31782, #11200 ),
 ( #56777, #6218 ) ),
 .UNSPECIFIED., .F., .F., .F. ) 
 B_SPLINE_SURFACE_WITH_KNOTS ( ( 4, 4 ),
 ( 2, 2 ),
 ( 0.000000000000000000, 1.000000000000000000 ),
 ( 0.000000000000000000, 1.000000000000000000 ),
 .UNSPECIFIED. ) 
 GEOMETRIC_REPRESENTATION_ITEM ( )  RATIONAL_B_SPLINE_SURFACE ( (
 ( 1.000000000000000000, 1.000000000000000000),
 ( 0.9942764183789327692, 0.8450855930916585379),
 ( 0.9942764183789327692, 0.8450855930916585379),
 ( 1.000000000000000000, 1.000000000000000000) ) ) 
 REPRESENTATION_ITEM ( '' )  SURFACE ( )  );
#31637 = ORIENTED_EDGE ( 'NONE', *, *, #12712, .T. ) ;
#31638 = LINE ( 'NONE', #16370, #38076 ) ;
#31639 = CARTESIAN_POINT ( 'NONE',  ( 2.373367633546871858, -5.764146204907428128, -5.072743978105297202 ) ) ;
#31640 = ORIENTED_EDGE ( 'NONE', *, *, #64780, .F. ) ;
#31641 = CARTESIAN_POINT ( 'NONE',  ( -18.35103012267012446, 6.403183891280330720, 10.15237553557610717 ) ) ;
#31642 = DIRECTION ( 'NONE',  ( 0.000000000000000000, 0.000000000000000000, -1.000000000000000000 ) ) ;
#31643 = DIRECTION ( 'NONE',  ( 0.000000000000000000, 0.9346839223284553189, -0.3554799084908935036 ) ) ;
#31644 = CARTESIAN_POINT ( 'NONE',  ( -35.00000000000000000, 0.000000000000000000, 0.000000000000000000 ) ) ;
#31645 = EDGE_LOOP ( 'NONE', ( #23330, #4297, #51008, #63302 ) ) ;
#31646 = CARTESIAN_POINT ( 'NONE',  ( 0.9232058338315058954, -7.723624854284779850, 9.791640253608122180 ) ) ;
#31647 = EDGE_CURVE ( 'NONE', #59346, #7701, #23573, .T. ) ;
#31648 = VERTEX_POINT ( 'NONE', #48212 ) ;
#31649 = LINE ( 'NONE', #1429, #39145 ) ;
#31650 = DIRECTION ( 'NONE',  ( 0.000000000000000000, 0.9551603052523489623, -0.2960891610144475994 ) ) ;
#31651 = EDGE_CURVE ( 'NONE', #63267, #32172, #33852, .T. ) ;
#31652 = FACE_OUTER_BOUND ( 'NONE', #19889, .T. ) ;
#31653 = B_SPLINE_CURVE_WITH_KNOTS ( 'NONE', 3,
 ( #1823, #41377, #22088, #32387, #61664, #16118, #17103, #5851, #27398, #15775, #520, #36406, #42344 ),
 .UNSPECIFIED., .F., .F.,
 ( 4, 3, 3, 3, 4 ),
 ( 2.949348774913951345E-18, 6.990956068646394335E-05, 0.0001398191187764043046, 0.0002097286751720211107, 0.0002792983885906313336 ),
 .UNSPECIFIED. ) ;
#31654 = ORIENTED_EDGE ( 'NONE', *, *, #5054, .T. ) ;
#31655 = FACE_OUTER_BOUND ( 'NONE', #52966, .T. ) ;
#31656 = VECTOR ( 'NONE', #20536, 1000.000000000000000 ) ;
#31657 = EDGE_CURVE ( 'NONE', #55363, #3924, #22592, .T. ) ;
#31658 = CIRCLE ( 'NONE', #45475, 5.000000000000001776 ) ;
#31659 = VECTOR ( 'NONE', #15437, 1000.000000000000114 ) ;
#31660 = CARTESIAN_POINT ( 'NONE',  ( -25.00000000000000355, -9.999999999999998224, -4.999999999999999112 ) ) ;
#31661 = DIRECTION ( 'NONE',  ( 1.000000000000000000, -0.000000000000000000, 0.000000000000000000 ) ) ;
#31662 = DIRECTION ( 'NONE',  ( 0.000000000000000000, -0.7196168960969868689, -0.6943713148249562872 ) ) ;
#31664 = AXIS2_PLACEMENT_3D ( 'NONE', #18003, #17687, #8350 ) ;
#31663 = CARTESIAN_POINT ( 'NONE',  ( -27.35552965826137140, 1.320216934008397569, 2.810569013793730697 ) ) ;
#31665 = CYLINDRICAL_SURFACE ( 'NONE', #16097, 12.75000000000000178 ) ;
#31666 = EDGE_CURVE ( 'NONE', #27200, #14515, #27345, .T. ) ;
#31667 = CARTESIAN_POINT ( 'NONE',  ( 1.194176325881332268, 4.773862381874729444, 11.61285876598807754 ) ) ;
#31668 = CARTESIAN_POINT ( 'NONE',  ( -24.42101984568203576, -2.451666775035103552, 3.522366633939663760 ) ) ;
#31669 = AXIS2_PLACEMENT_3D ( 'NONE', #9549, #2978, #28550 ) ;
#31670 = VERTEX_POINT ( 'NONE', #33211 ) ;
#31671 = DIRECTION ( 'NONE',  ( -0.000000000000000000, -0.000000000000000000, -1.000000000000000000 ) ) ;
#31672 = CARTESIAN_POINT ( 'NONE',  ( 0.2648978790185584908, -12.24533305150758089, -0.1321385342563691223 ) ) ;
#31673 = VERTEX_POINT ( 'NONE', #38184 ) ;
#31674 = CARTESIAN_POINT ( 'NONE',  ( 3.152665057736233845, -4.725420687649230622, 6.378477742801980988 ) ) ;
#31675 = CARTESIAN_POINT ( 'NONE',  ( -22.27711653538342773, 3.377206745425005874, 1.465933162149040792 ) ) ;
#31676 = VERTEX_POINT ( 'NONE', #53836 ) ;
#31677 = CARTESIAN_POINT ( 'NONE',  ( 22.57855258442565116, 3.026812727784649493, 25.00000000000000000 ) ) ;
#31678 = EDGE_LOOP ( 'NONE', ( #29532, #54958, #10359, #5235 ) ) ;
#31679 = CARTESIAN_POINT ( 'NONE',  ( 0.3057689695767527027, -5.928746590069652989, 10.73077184758789393 ) ) ;
#31680 = ORIENTED_EDGE ( 'NONE', *, *, #44432, .F. ) ;
#31681 = ORIENTED_EDGE ( 'NONE', *, *, #41184, .F. ) ;
#31682 = DIRECTION ( 'NONE',  ( -1.000000000000000000, 0.000000000000000000, 0.000000000000000000 ) ) ;
#31683 = AXIS2_PLACEMENT_3D ( 'NONE', #29302, #49595, #23012 ) ;
#31684 = VERTEX_POINT ( 'NONE', #7277 ) ;
#31685 = CARTESIAN_POINT ( 'NONE',  ( -25.69578604477335659, -5.442779444386042442, 10.69993300052666640 ) ) ;
#31686 = CARTESIAN_POINT ( 'NONE',  ( -22.28546858134833641, -3.567529619157803644, 1.005093225210829999 ) ) ;
#31687 = DIRECTION ( 'NONE',  ( 0.000000000000000000, 0.01356324068817998940, -0.9999080150203990547 ) ) ;
#31688 = FACE_OUTER_BOUND ( 'NONE', #31312, .T. ) ;
#31689 = ORIENTED_EDGE ( 'NONE', *, *, #44167, .T. ) ;
#31690 = CARTESIAN_POINT ( 'NONE',  ( -37.00000000000000711, 3.473736367725253960, 12.26766708251992988 ) ) ;
#31691 = AXIS2_PLACEMENT_3D ( 'NONE', #32450, #63052, #28144 ) ;
#31692 = CARTESIAN_POINT ( 'NONE',  ( 12.91449914267798960, -27.44768092100439461, 12.53791341943762916 ) ) ;
#31693 = CARTESIAN_POINT ( 'NONE',  ( 2.717984159220113494, -7.788152353089298430, 0.2836133496102792861 ) ) ;
#31695 = ORIENTED_EDGE ( 'NONE', *, *, #35602, .F. ) ;
#31694 = DIRECTION ( 'NONE',  ( -1.000000000000000000, -0.000000000000000000, 0.000000000000000000 ) ) ;
#31696 = CARTESIAN_POINT ( 'NONE',  ( -27.45775109278351067, 8.499184579339635448, -8.471355351200609007 ) ) ;
#31697 = ORIENTED_EDGE ( 'NONE', *, *, #24387, .T. ) ;
#31698 = DIRECTION ( 'NONE',  ( 1.000000000000000000, -0.000000000000000000, 0.000000000000000000 ) ) ;
#31699 = ORIENTED_EDGE ( 'NONE', *, *, #12968, .F. ) ;
#31700 = CYLINDRICAL_SURFACE ( 'NONE', #8202, 5.000000000000000888 ) ;
#31701 = DIRECTION ( 'NONE',  ( -1.000000000000000000, 0.000000000000000000, 0.000000000000000000 ) ) ;
#31702 = AXIS2_PLACEMENT_3D ( 'NONE', #14278, #8973, #22719 ) ;
#31703 = CARTESIAN_POINT ( 'NONE',  ( 2.284126774967659035, -7.647017279602160933, -0.1584898568958676424 ) ) ;
#31704 = EDGE_CURVE ( 'NONE', #14785, #3974, #2974, .T. ) ;
#31705 = ORIENTED_EDGE ( 'NONE', *, *, #10396, .T. ) ;
#31706 = CARTESIAN_POINT ( 'NONE',  ( 1.459561108992593281, 8.601340491610839578, 9.267924853468722191 ) ) ;
#31707 = FACE_OUTER_BOUND ( 'NONE', #48888, .T. ) ;
#31708 = CARTESIAN_POINT ( 'NONE',  ( 0.2801149460245139777, -12.02936836014264621, 2.320387321174126605 ) ) ;
#31709 = EDGE_LOOP ( 'NONE', ( #63849, #13323, #40320, #9317 ) ) ;
#31710 = AXIS2_PLACEMENT_3D ( 'NONE', #2423, #43607, #57628 ) ;
#31711 = AXIS2_PLACEMENT_3D ( 'NONE', #42571, #11037, #62873 ) ;
#31712 = ORIENTED_EDGE ( 'NONE', *, *, #28003, .F. ) ;
#31713 = DIRECTION ( 'NONE',  ( 1.000000000000000000, 0.000000000000000000, -0.000000000000000000 ) ) ;
#31714 = ORIENTED_EDGE ( 'NONE', *, *, #22036, .T. ) ;
#31715 = VECTOR ( 'NONE', #8681, 999.9999999999998863 ) ;
#31716 = VERTEX_POINT ( 'NONE', #48848 ) ;
#31717 = DIRECTION ( 'NONE',  ( 0.000000000000000000, -0.01356324068817998940, 0.9999080150203990547 ) ) ;
#31718 = CARTESIAN_POINT ( 'NONE',  ( -35.00000000000000000, -2.021542716731318912, -12.01765980939844169 ) ) ;
#31719 = CARTESIAN_POINT ( 'NONE',  ( 1.000000000000000888, 5.217815162096836268, 5.387430271863580700 ) ) ;
#31720 = CARTESIAN_POINT ( 'NONE',  ( 1.452237505248555660, 6.833827325205318992, 10.65201107290469906 ) ) ;
#31721 = CYLINDRICAL_SURFACE ( 'NONE', #49683, 2.899999999999994582 ) ;
#31722 = CARTESIAN_POINT ( 'NONE',  ( 35.00000000000000000, 4.946702696913328090, 11.13736569743268845 ) ) ;
#31723 = EDGE_CURVE ( 'NONE', #34331, #33819, #39171, .T. ) ;
#31724 = CARTESIAN_POINT ( 'NONE',  ( 35.00000000000000000, 5.921969905510355403, -10.14408668126215929 ) ) ;
#31725 = EDGE_CURVE ( 'NONE', #38332, #5898, #23911, .T. ) ;
#31726 = ORIENTED_EDGE ( 'NONE', *, *, #52938, .F. ) ;
#31727 = EDGE_CURVE ( 'NONE', #41185, #6776, #16867, .T. ) ;
#31728 = CARTESIAN_POINT ( 'NONE',  ( 0.3665391374699472626, 6.368473106897130087, 10.50279796150439005 ) ) ;
#31729 = CARTESIAN_POINT ( 'NONE',  ( 0.3002738374340850891, 4.403689978763226875, -11.43949898053766390 ) ) ;
#31730 = CIRCLE ( 'NONE', #30686, 12.75000000000000178 ) ;
#31731 = DIRECTION ( 'NONE',  ( -1.000000000000000000, -0.000000000000000000, 0.000000000000000000 ) ) ;
#31732 = EDGE_CURVE ( 'NONE', #41303, #18751, #36084, .T. ) ;
#31733 = AXIS2_PLACEMENT_3D ( 'NONE', #41050, #35401, #35722 ) ;
#31734 = CARTESIAN_POINT ( 'NONE',  ( -25.00000000000000355, -9.999999999999998224, -25.00000000000000000 ) ) ;
#31735 = EDGE_CURVE ( 'NONE', #28121, #35981, #25369, .T. ) ;
#31736 = CARTESIAN_POINT ( 'NONE',  ( 1.499544914656756101, 0.6073691993713128401, -11.98564492472154086 ) ) ;
#31737 = DIRECTION ( 'NONE',  ( 1.000000000000000000, -0.000000000000000000, 0.000000000000000000 ) ) ;
#31738 = EDGE_LOOP ( 'NONE', ( #50770, #34072, #46968, #54048 ) ) ;
#31739 = CARTESIAN_POINT ( 'NONE',  ( -41.00000000000000711, -25.30020925422648048, 3.022492086418944623 ) ) ;
#31740 = DIRECTION ( 'NONE',  ( -1.000000000000000000, 0.000000000000000000, 0.000000000000000000 ) ) ;
#31741 = CARTESIAN_POINT ( 'NONE',  ( -37.00000000000000711, 0.000000000000000000, 0.000000000000000000 ) ) ;
#31742 = CARTESIAN_POINT ( 'NONE',  ( 16.21117406328131949, -35.00000000000000000, 4.142385751841762165 ) ) ;
#31743 = CIRCLE ( 'NONE', #38112, 5.000000000000001776 ) ;
#31744 = AXIS2_PLACEMENT_3D ( 'NONE', #46738, #4886, #5884 ) ;
#31745 = EDGE_CURVE ( 'NONE', #47135, #16200, #2818, .T. ) ;
#31746 = CARTESIAN_POINT ( 'NONE',  ( 8.937200413559443390, 4.476360154859203355, -12.73625532737111143 ) ) ;
#31747 = CARTESIAN_POINT ( 'NONE',  ( 5.520433897694421610, -0.01186170453199831935, 0.009283255140285138346 ) ) ;
#31748 = CIRCLE ( 'NONE', #29668, 7.499999999999988454 ) ;
#31749 = EDGE_LOOP ( 'NONE', ( #31063, #60203, #7360, #33583 ) ) ;
#31750 = CARTESIAN_POINT ( 'NONE',  ( 2.241352910868908754, -3.889181972941404553, -6.569501556381482921 ) ) ;
#31751 = DIRECTION ( 'NONE',  ( -0.000000000000000000, -1.000000000000000000, -0.000000000000000000 ) ) ;
#31753 = EDGE_CURVE ( 'NONE', #46246, #63372, #35823, .T. ) ;
#31752 = LINE ( 'NONE', #52722, #50912 ) ;
#31754 = VERTEX_POINT ( 'NONE', #39499 ) ;
#31755 = FACE_OUTER_BOUND ( 'NONE', #53095, .T. ) ;
#31756 = CARTESIAN_POINT ( 'NONE',  ( -18.08686583997218733, 5.151216734910788908, -10.83812558286602012 ) ) ;
#31757 = DIRECTION ( 'NONE',  ( 0.000000000000000000, -0.01356324068817998940, 0.9999080150203990547 ) ) ;
#31759 = ORIENTED_EDGE ( 'NONE', *, *, #8704, .T. ) ;
#31758 = DIRECTION ( 'NONE',  ( -1.000000000000000000, 0.000000000000000000, 0.000000000000000000 ) ) ;
#31760 = CARTESIAN_POINT ( 'NONE',  ( -27.09342121492585065, 2.251107617621282753, 0.5565043948849990318 ) ) ;
#31761 = CARTESIAN_POINT ( 'NONE',  ( -9.351388602708162523, 12.99278190472488248, -3.665735721005250358 ) ) ;
#31762 = ORIENTED_EDGE ( 'NONE', *, *, #29300, .T. ) ;
#31763 = CARTESIAN_POINT ( 'NONE',  ( 35.00000000000000000, -1.488153103996881610, 11.65150730582935701 ) ) ;
#31764 = DIRECTION ( 'NONE',  ( 1.000000000000000000, 0.000000000000000000, -0.000000000000000000 ) ) ;
#31765 = CARTESIAN_POINT ( 'NONE',  ( 22.57855258442565116, 3.026812727784649493, -11.61199400236326973 ) ) ;
#31766 = CYLINDRICAL_SURFACE ( 'NONE', #41450, 5.000000000000000000 ) ;
#31767 = CARTESIAN_POINT ( 'NONE',  ( 0.2759803524722221346, -11.44482553421628346, -4.367180139677437900 ) ) ;
#31768 = CARTESIAN_POINT ( 'NONE',  ( 0.3278977287071219160, 5.917385921415800887, 10.74546228373869283 ) ) ;
#31770 = ORIENTED_EDGE ( 'NONE', *, *, #16469, .F. ) ;
#31769 = CARTESIAN_POINT ( 'NONE',  ( 0.2646305136544072623, 10.67138229758229606, 6.008537389229454462 ) ) ;
#31771 = ORIENTED_EDGE ( 'NONE', *, *, #60575, .T. ) ;
#31772 = LINE ( 'NONE', #11504, #5583 ) ;
#31773 = ORIENTED_EDGE ( 'NONE', *, *, #33094, .F. ) ;
#31774 = B_SPLINE_CURVE_WITH_KNOTS ( 'NONE', 3,
 ( #2393, #22669, #49499, #65083, #19558, #42935, #33290, #12656, #22309, #17998, #44464, #42580, #53594, #39488, #29504, #39821, #63214, #52610, #17347, #62882 ),
 .UNSPECIFIED., .F., .F.,
 ( 4, 2, 2, 2, 2, 2, 2, 2, 2, 4 ),
 ( 9.341771812940338307E-18, 0.001217729388623014488, 0.001826594082934518155, 0.002435458777246022038, 0.003653188165869029370, 0.004870917554492038871, 0.006088646943115048372, 0.007306376331738057874, 0.008524105720361066507, 0.009741835108984076008 ),
 .UNSPECIFIED. ) ;
#31775 = DIRECTION ( 'NONE',  ( 0.000000000000000000, -0.01356324068817991828, 0.9999080150203990547 ) ) ;
#31776 = LINE ( 'NONE', #41771, #17319 ) ;
#31777 = EDGE_CURVE ( 'NONE', #12414, #11179, #44824, .T. ) ;
#31778 = VECTOR ( 'NONE', #52783, 1000.000000000000000 ) ;
#31779 = CARTESIAN_POINT ( 'NONE',  ( -36.00000000000000711, -7.882940143791846488, 10.02106554660705839 ) ) ;
#31780 = VERTEX_POINT ( 'NONE', #34513 ) ;
#31781 = LINE ( 'NONE', #52090, #30811 ) ;
#31782 = CARTESIAN_POINT ( 'NONE',  ( 5.515188684475870851, -0.004322737127823499288, 0.003154373509839884532 ) ) ;
#31783 = VECTOR ( 'NONE', #87, 1000.000000000000000 ) ;
#31784 = CARTESIAN_POINT ( 'NONE',  ( 37.00000000000000711, 4.705694406421931860E-17, -3.469127814946512892E-15 ) ) ;
#31785 = VERTEX_POINT ( 'NONE', #54813 ) ;
#31786 = ORIENTED_EDGE ( 'NONE', *, *, #9571, .T. ) ;
#31787 = CARTESIAN_POINT ( 'NONE',  ( 2.556980015513709237, 7.578583798307162667, -1.570584617272491768 ) ) ;
#31788 = EDGE_CURVE ( 'NONE', #8949, #13688, #13886, .T. ) ;
#31789 = ORIENTED_EDGE ( 'NONE', *, *, #12297, .F. ) ;
#31790 = CARTESIAN_POINT ( 'NONE',  ( 2.241537034860906275, 1.330359961362386878, -7.517665055735998081 ) ) ;
#31791 = CARTESIAN_POINT ( 'NONE',  ( 2.000000000000001776, -1.754183803416492493, -6.711026108862277795 ) ) ;
#31792 = CARTESIAN_POINT ( 'NONE',  ( 37.00000000000000711, -12.68495603654572612, -1.286231064351273989 ) ) ;
#31794 = AXIS2_PLACEMENT_3D ( 'NONE', #35543, #29256, #14908 ) ;
#31793 = CARTESIAN_POINT ( 'NONE',  ( -27.08456565417846562, 0.9533904527919729865, -2.084650034356376302 ) ) ;
#31795 = CYLINDRICAL_SURFACE ( 'NONE', #41547, 4.999999999999999112 ) ;
#31796 = DIRECTION ( 'NONE',  ( 0.000000000000000000, -0.7196168960969719919, -0.6943713148249714973 ) ) ;
#31797 = EDGE_CURVE ( 'NONE', #12400, #26236, #62514, .T. ) ;
#31798 = DIRECTION ( 'NONE',  ( 1.000000000000000000, -0.000000000000000000, -0.000000000000000000 ) ) ;
#31799 = CIRCLE ( 'NONE', #26496, 12.75000000000000178 ) ;
#31800 = EDGE_LOOP ( 'NONE', ( #30957, #5790, #41742, #39705 ) ) ;
#31801 = CARTESIAN_POINT ( 'NONE',  ( 0.000000000000000000, 1.865193240757095916, 6.552473556515182374 ) ) ;
#31802 = EDGE_LOOP ( 'NONE', ( #60615, #10994, #20588, #24493 ) ) ;
#31803 = DIRECTION ( 'NONE',  ( -1.000000000000000000, -1.836970198721029688E-16, 0.000000000000000000 ) ) ;
#31804 = EDGE_CURVE ( 'NONE', #30254, #8001, #36926, .T. ) ;
#31805 = CARTESIAN_POINT ( 'NONE',  ( -9.221157027727812761, 9.600812269888216122, -7.209108748489196472 ) ) ;
#31806 = DIRECTION ( 'NONE',  ( -1.000000000000000000, 0.000000000000000000, 0.000000000000000000 ) ) ;
#31807 = CARTESIAN_POINT ( 'NONE',  ( -17.87894447371643025, 11.34875452035183052, 3.899500356681838475 ) ) ;
#31808 = CIRCLE ( 'NONE', #3173, 7.499999999999988454 ) ;
#31809 = VERTEX_POINT ( 'NONE', #41794 ) ;
#31810 = ORIENTED_EDGE ( 'NONE', *, *, #63768, .T. ) ;
#31811 = DIRECTION ( 'NONE',  ( 0.000000000000000000, 0.9868265225415254749, 0.1617819965527686754 ) ) ;
#31812 = B_SPLINE_CURVE_WITH_KNOTS ( 'NONE', 3,
 ( #44640, #14396, #34669, #39998, #54967, #65275, #9395, #29681, #55290, #60281, #14705, #50975, #35328, #755, #56270, #51958, #51641, #6401, #45319 ),
 .UNSPECIFIED., .F., .F.,
 ( 4, 3, 3, 3, 3, 3, 4 ),
 ( 7.217888169571747161E-18, 2.825908398991472574E-05, 4.208813692702314017E-05, 5.591713747220622617E-05, 6.279584083537281586E-05, 9.105792820726668299E-05, 0.0001153131102486956423 ),
 .UNSPECIFIED. ) ;
#31813 = ORIENTED_EDGE ( 'NONE', *, *, #21302, .T. ) ;
#31814 = CARTESIAN_POINT ( 'NONE',  ( 0.3665391374699464300, 12.27992639892678284, 0.2638605131387594671 ) ) ;
#31815 = EDGE_CURVE ( 'NONE', #33072, #918, #5201, .T. ) ;
#31816 = CARTESIAN_POINT ( 'NONE',  ( -14.29135464769095520, 7.782112657557433089, -11.03126115115966854 ) ) ;
#31817 = CARTESIAN_POINT ( 'NONE',  ( 2.262775599886276634, 4.802882839669051940, 5.943524836196961481 ) ) ;
#31818 = CARTESIAN_POINT ( 'NONE',  ( -35.00000000000000000, 10.32377448871677039, -6.475373545682193033 ) ) ;
#31819 = ADVANCED_FACE ( 'NONE', ( #32134 ), #10492, .T. ) ;
#31820 = EDGE_LOOP ( 'NONE', ( #63473, #55489, #42125, #41481 ) ) ;
#31821 = CARTESIAN_POINT ( 'NONE',  ( 2.305787727787083519, 2.461236246751071555, 7.249469779319919205 ) ) ;
#31822 = CARTESIAN_POINT ( 'NONE',  ( 2.241506898688419902, -0.03933068055385580131, -7.634383346098562839 ) ) ;
#31823 = CARTESIAN_POINT ( 'NONE',  ( 0.5547464869798254261, -1.842327806480229757, 12.20441397277155815 ) ) ;
#31824 = CARTESIAN_POINT ( 'NONE',  ( -48.39008813825011401, -0.3233266992476376833, 8.863930066451535694 ) ) ;
#31825 = EDGE_CURVE ( 'NONE', #58095, #44356, #41645, .T. ) ;
#31826 = AXIS2_PLACEMENT_3D ( 'NONE', #54159, #31177, #46462 ) ;
#31827 = EDGE_CURVE ( 'NONE', #6027, #28214, #10538, .T. ) ;
#31828 = EDGE_CURVE ( 'NONE', #44540, #60515, #19014, .T. ) ;
#31829 = DIRECTION ( 'NONE',  ( -1.000000000000000000, 0.000000000000000000, 0.000000000000000000 ) ) ;
#31830 = CARTESIAN_POINT ( 'NONE',  ( 37.00000000000000711, 4.705694406421931860E-17, -3.469127814946512892E-15 ) ) ;
#31831 =( BOUNDED_SURFACE ( )  B_SPLINE_SURFACE ( 3, 1, ( 
 ( #35811, #26199 ),
 ( #36145, #51153 ),
 ( #5263, #65745 ),
 ( #41464, #31814 ) ),
 .UNSPECIFIED., .F., .F., .F. ) 
 B_SPLINE_SURFACE_WITH_KNOTS ( ( 4, 4 ),
 ( 2, 2 ),
 ( 0.000000000000000000, 1.000000000000000000 ),
 ( 0.000000000000000000, 1.000000000000000000 ),
 .UNSPECIFIED. ) 
 GEOMETRIC_REPRESENTATION_ITEM ( )  RATIONAL_B_SPLINE_SURFACE ( (
 ( 1.000000000000000000, 1.000000000000000000),
 ( 0.9942764183789327692, 0.8450855930916580938),
 ( 0.9942764183789327692, 0.8450855930916580938),
 ( 1.000000000000000000, 1.000000000000000000) ) ) 
 REPRESENTATION_ITEM ( '' )  SURFACE ( )  );
#31832 = ORIENTED_EDGE ( 'NONE', *, *, #46016, .T. ) ;
#31834 = EDGE_CURVE ( 'NONE', #59342, #30274, #64645, .T. ) ;
#31833 = CARTESIAN_POINT ( 'NONE',  ( -16.21117406328131594, -35.00000000000000000, -4.142385751841761277 ) ) ;
#31835 = ORIENTED_EDGE ( 'NONE', *, *, #20855, .T. ) ;
#31836 = DIRECTION ( 'NONE',  ( 0.000000000000000000, 0.8369827122275325104, 0.5472293298355300761 ) ) ;
#31837 = CYLINDRICAL_SURFACE ( 'NONE', #17195, 12.18650000000000055 ) ;
#31838 = DIRECTION ( 'NONE',  ( 1.000000000000000000, -0.000000000000000000, 0.000000000000000000 ) ) ;
#31840 = CARTESIAN_POINT ( 'NONE',  ( 5.515539859299206427, 0.005924322247674738452, 0.001241880655086611586 ) ) ;
#31839 = B_SPLINE_CURVE_WITH_KNOTS ( 'NONE', 3,
 ( #38202, #54506, #28560, #13904, #24224, #43192, #44490 ),
 .UNSPECIFIED., .F., .F.,
 ( 4, 3, 4 ),
 ( 0.000000000000000000, 0.001700533616330591980, 0.005002426799371264415 ),
 .UNSPECIFIED. ) ;
#31841 = CARTESIAN_POINT ( 'NONE',  ( -10.25468736929027536, -4.747758800244201716, 11.02689688273352075 ) ) ;
#31842 = ORIENTED_EDGE ( 'NONE', *, *, #54721, .T. ) ;
#31843 = ORIENTED_EDGE ( 'NONE', *, *, #42208, .F. ) ;
#31844 = DIRECTION ( 'NONE',  ( 0.000000000000000000, 0.1740410799127612429, 0.9847383929261617208 ) ) ;
#31845 = EDGE_LOOP ( 'NONE', ( #25319, #33820, #59886, #41866 ) ) ;
#31846 = CARTESIAN_POINT ( 'NONE',  ( 3.467905914750478491, 6.588911164890562944, 10.03839023354865034 ) ) ;
#31847 = CARTESIAN_POINT ( 'NONE',  ( 37.00000000000000711, -9.040300684349746874, -7.499679039484027143 ) ) ;
#31848 = FACE_OUTER_BOUND ( 'NONE', #14269, .T. ) ;
#31849 = CYLINDRICAL_SURFACE ( 'NONE', #20543, 1.750000000000000000 ) ;
#31850 = CARTESIAN_POINT ( 'NONE',  ( 2.524535260910446777, 7.725637239509726584, -0.2211075636754606388 ) ) ;
#31851 = CARTESIAN_POINT ( 'NONE',  ( 5.514970785353741078, 0.002619824551223220045, -0.003929719953530077733 ) ) ;
#31852 = CARTESIAN_POINT ( 'NONE',  ( -11.40165637462999904, -7.508992741355383416, 9.360289953322597611 ) ) ;
#31853 = VERTEX_POINT ( 'NONE', #61100 ) ;
#31854 = CARTESIAN_POINT ( 'NONE',  ( 1.104777566491147889, -5.844728374724341258, 11.07886329447274676 ) ) ;
#31855 = CIRCLE ( 'NONE', #25459, 11.99999999999998579 ) ;
#31856 = ORIENTED_EDGE ( 'NONE', *, *, #27331, .T. ) ;
#31857 = FACE_OUTER_BOUND ( 'NONE', #12995, .T. ) ;
#31858 = CARTESIAN_POINT ( 'NONE',  ( 35.00000000000000000, -12.18359334611896294, -0.2661492558802951991 ) ) ;
#31859 = CARTESIAN_POINT ( 'NONE',  ( 0.9232058338315048962, 0.3773051331669723951, -12.46548196349785798 ) ) ;
#31860 = EDGE_CURVE ( 'NONE', #1201, #33280, #44477, .T. ) ;
#31861 = FACE_OUTER_BOUND ( 'NONE', #30314, .T. ) ;
#31862 = VERTEX_POINT ( 'NONE', #35800 ) ;
#31863 = CARTESIAN_POINT ( 'NONE',  ( 36.00000000000000711, -5.300372733891561161, 11.59605747147791810 ) ) ;
#31864 = DIRECTION ( 'NONE',  ( 1.000000000000000000, -0.000000000000000000, 0.000000000000000000 ) ) ;
#31865 = CARTESIAN_POINT ( 'NONE',  ( -35.00000000000000000, 6.917234959366964198, -9.493370459201624811 ) ) ;
#31866 = ORIENTED_EDGE ( 'NONE', *, *, #18832, .F. ) ;
#31867 = VERTEX_POINT ( 'NONE', #62088 ) ;
#31868 = CARTESIAN_POINT ( 'NONE',  ( -35.00000000000000000, -12.18359334611896472, -0.2661492558804631203 ) ) ;
#31869 = ORIENTED_EDGE ( 'NONE', *, *, #32785, .F. ) ;
#31870 = VERTEX_POINT ( 'NONE', #41126 ) ;
#31871 = ADVANCED_FACE ( 'NONE', ( #5593 ), #51791, .T. ) ;
#31872 = VERTEX_POINT ( 'NONE', #25862 ) ;
#31873 = B_SPLINE_CURVE_WITH_KNOTS ( 'NONE', 3,
 ( #29830, #50145, #10530, #4601, #30807, #41119, #15841, #5923, #26178, #24871, #37115, #27469, #52762, #12495, #1240, #41443, #31793, #52103, #32454 ),
 .UNSPECIFIED., .F., .F.,
 ( 4, 3, 3, 3, 3, 3, 4 ),
 ( 3.223564806431921169E-18, 2.836829843012604650E-05, 4.224792512550834891E-05, 5.612066614913120233E-05, 6.998859278354828948E-05, 9.832141288087297370E-05, 0.0001178161482478445269 ),
 .UNSPECIFIED. ) ;
#31874 = ORIENTED_EDGE ( 'NONE', *, *, #5754, .F. ) ;
#31875 = CARTESIAN_POINT ( 'NONE',  ( 0.3610902822527172207, 4.444884365376601032, 11.44530431865294418 ) ) ;
#31876 = CARTESIAN_POINT ( 'NONE',  ( -37.00000000000000711, -11.10408318471063716, 6.265926637539457111 ) ) ;
#31877 = AXIS2_PLACEMENT_3D ( 'NONE', #35523, #55820, #21205 ) ;
#31879 = VECTOR ( 'NONE', #19815, 1000.000000000000000 ) ;
#31878 = CYLINDRICAL_SURFACE ( 'NONE', #5521, 5.000000000000000888 ) ;
#31880 = CARTESIAN_POINT ( 'NONE',  ( -36.00000000000000711, -6.564808257521847601, 10.93004082984016456 ) ) ;
#31881 = LINE ( 'NONE', #26918, #65632 ) ;
#31882 = AXIS2_PLACEMENT_3D ( 'NONE', #23949, #13610, #34551 ) ;
#31883 = ORIENTED_EDGE ( 'NONE', *, *, #7586, .F. ) ;
#31884 = CARTESIAN_POINT ( 'NONE',  ( 0.2648978790185619880, -9.465406350830555482, -7.769924372105300847 ) ) ;
#31885 = ORIENTED_EDGE ( 'NONE', *, *, #22635, .T. ) ;
#31886 = CARTESIAN_POINT ( 'NONE',  ( -10.95212338237647920, -9.902220863987562183, -9.175839033069911110 ) ) ;
#31887 = CARTESIAN_POINT ( 'NONE',  ( 2.899286259009557387, 4.769992516330251675, 6.239228647238516778 ) ) ;
#31888 = DIRECTION ( 'NONE',  ( -1.000000000000000000, 0.000000000000000000, 0.000000000000000000 ) ) ;
#31889 = ADVANCED_FACE ( 'NONE', ( #15848 ), #42104, .T. ) ;
#31890 = CARTESIAN_POINT ( 'NONE',  ( -35.00000000000000000, 9.348667969174405457, 7.817492529713891081 ) ) ;
#31891 = DIRECTION ( 'NONE',  ( 0.000000000000000000, -0.01356324068817991481, 0.9999080150203990547 ) ) ;
#31892 = CARTESIAN_POINT ( 'NONE',  ( -19.47984447937493613, -3.750539801530005768, -11.39883551934754102 ) ) ;
#31893 = AXIS2_PLACEMENT_3D ( 'NONE', #60326, #59049, #59688 ) ;
#31894 = EDGE_LOOP ( 'NONE', ( #16478, #58541, #53773, #11877 ) ) ;
#31895 = DIRECTION ( 'NONE',  ( 1.000000000000000000, 0.000000000000000000, 0.000000000000000000 ) ) ;
#31896 = VECTOR ( 'NONE', #6241, 1000.000000000000000 ) ;
#31897 = ORIENTED_EDGE ( 'NONE', *, *, #15701, .F. ) ;
#31898 = CARTESIAN_POINT ( 'NONE',  ( 29.51976981715666781, -7.690765383426355406, 11.09513982864076276 ) ) ;
#31899 = CARTESIAN_POINT ( 'NONE',  ( -0.9955874700083122697, -25.73414319850213516, -15.65071058219114342 ) ) ;
#31900 = CARTESIAN_POINT ( 'NONE',  ( -47.00000000000000711, 0.000000000000000000, 0.000000000000000000 ) ) ;
#31901 = CARTESIAN_POINT ( 'NONE',  ( 2.000000000000001776, -4.976357229393876480, 4.652926418895529714 ) ) ;
#31902 = CARTESIAN_POINT ( 'NONE',  ( 2.247206125382827935, -6.670391186503669800, 3.717496781928072203 ) ) ;
#31903 = ORIENTED_EDGE ( 'NONE', *, *, #44712, .F. ) ;
#31904 = DIRECTION ( 'NONE',  ( -1.000000000000000000, -0.000000000000000000, 0.000000000000000000 ) ) ;
#31906 = CIRCLE ( 'NONE', #37177, 5.000000000000001776 ) ;
#31905 = CARTESIAN_POINT ( 'NONE',  ( 0.3053067050349139722, 2.355726819985581422, -12.03105545708854685 ) ) ;
#31907 = FACE_OUTER_BOUND ( 'NONE', #5469, .T. ) ;
#31908 = CARTESIAN_POINT ( 'NONE',  ( -3.838337227274802643, 9.927591105267911331, 9.157165592576390623 ) ) ;
#31909 = EDGE_CURVE ( 'NONE', #64690, #22968, #15659, .T. ) ;
#31910 = EDGE_CURVE ( 'NONE', #39733, #37251, #52855, .T. ) ;
#31911 = EDGE_CURVE ( 'NONE', #11560, #64240, #58176, .T. ) ;
#31912 = CIRCLE ( 'NONE', #29767, 12.75000000000000178 ) ;
#31913 = CARTESIAN_POINT ( 'NONE',  ( 1.452237505248552996, -11.24427360515646512, 5.807998527925852805 ) ) ;
#31914 = ORIENTED_EDGE ( 'NONE', *, *, #27322, .T. ) ;
#31916 = EDGE_CURVE ( 'NONE', #63728, #27622, #50763, .T. ) ;
#31915 = CARTESIAN_POINT ( 'NONE',  ( -37.00000000000000711, -2.696588552978969044, -12.46157735505192399 ) ) ;
#31917 = CIRCLE ( 'NONE', #19160, 5.000000000000000000 ) ;
#31918 = CARTESIAN_POINT ( 'NONE',  ( 0.3675815128205894289, 11.62724744438065727, 3.951233083390508050 ) ) ;
#31919 = CIRCLE ( 'NONE', #18129, 5.000000000000000000 ) ;
#31920 = VECTOR ( 'NONE', #33811, 1000.000000000000000 ) ;
#31921 = ORIENTED_EDGE ( 'NONE', *, *, #15645, .F. ) ;
#31922 = ORIENTED_EDGE ( 'NONE', *, *, #33147, .F. ) ;
#31923 = DIRECTION ( 'NONE',  ( 0.000000000000000000, -0.01356324068817991828, 0.9999080150203990547 ) ) ;
#31924 = VECTOR ( 'NONE', #2219, 1000.000000000000000 ) ;
#31925 = DIRECTION ( 'NONE',  ( -0.000000000000000000, -1.000000000000000000, -0.000000000000000000 ) ) ;
#31926 = DIRECTION ( 'NONE',  ( 1.000000000000000000, -0.000000000000000000, 0.000000000000000000 ) ) ;
#31927 = CARTESIAN_POINT ( 'NONE',  ( 37.00000000000000711, -3.916263239775270577, 11.07407352312216453 ) ) ;
#31928 = ORIENTED_EDGE ( 'NONE', *, *, #65095, .F. ) ;
#31929 = ORIENTED_EDGE ( 'NONE', *, *, #756, .F. ) ;
#31930 = ORIENTED_EDGE ( 'NONE', *, *, #5809, .T. ) ;
#31931 = CARTESIAN_POINT ( 'NONE',  ( 26.76925746416558383, -11.45732145772444710, 3.578150596242692050 ) ) ;
#31932 = AXIS2_PLACEMENT_3D ( 'NONE', #40120, #4243, #35472 ) ;
#31933 = VECTOR ( 'NONE', #23319, 1000.000000000000000 ) ;
#31934 = DIRECTION ( 'NONE',  ( -1.000000000000000000, -0.000000000000000000, -0.000000000000000000 ) ) ;
#31935 = VERTEX_POINT ( 'NONE', #17525 ) ;
#31936 = CARTESIAN_POINT ( 'NONE',  ( 1.000000000000000888, -6.160607635185357367, -4.277489166005654653 ) ) ;
#31937 = AXIS2_PLACEMENT_3D ( 'NONE', #50077, #4535, #40401 ) ;
#31938 = AXIS2_PLACEMENT_3D ( 'NONE', #42807, #16237, #26871 ) ;
#31939 = CYLINDRICAL_SURFACE ( 'NONE', #11968, 13.50000000000000178 ) ;
#31940 = EDGE_CURVE ( 'NONE', #26553, #20972, #29496, .T. ) ;
#31941 = ORIENTED_EDGE ( 'NONE', *, *, #13868, .F. ) ;
#31942 = CARTESIAN_POINT ( 'NONE',  ( -27.08417174366084623, -0.3802265912085517341, -2.259388872100088541 ) ) ;
#31943 = CARTESIAN_POINT ( 'NONE',  ( -35.00000000000000000, 0.000000000000000000, 0.000000000000000000 ) ) ;
#31944 = DIRECTION ( 'NONE',  ( 0.000000000000000000, 0.01356324068817992175, -0.9999080150203990547 ) ) ;
#31945 = EDGE_LOOP ( 'NONE', ( #8017, #11056, #34560, #33932 ) ) ;
#31946 = AXIS2_PLACEMENT_3D ( 'NONE', #33093, #32745, #649 ) ;
#31947 = CARTESIAN_POINT ( 'NONE',  ( 37.00000000000000711, 4.705694406421931860E-17, -3.469127814946512892E-15 ) ) ;
#31948 = ORIENTED_EDGE ( 'NONE', *, *, #64334, .T. ) ;
#31949 = LINE ( 'NONE', #26007, #25365 ) ;
#31950 = AXIS2_PLACEMENT_3D ( 'NONE', #32857, #33204, #28872 ) ;
#31951 = ADVANCED_FACE ( 'NONE', ( #1897 ), #32460, .T. ) ;
#31952 = CARTESIAN_POINT ( 'NONE',  ( 2.241449424704146764, 4.954182807723340076, 5.808712090826627872 ) ) ;
#31953 = FACE_OUTER_BOUND ( 'NONE', #59944, .T. ) ;
#31954 = DIRECTION ( 'NONE',  ( -0.000000000000000000, -1.000000000000000000, -0.000000000000000000 ) ) ;
#31955 = CARTESIAN_POINT ( 'NONE',  ( 37.00000000000000711, -7.251710744571640888, -9.240395740215610942 ) ) ;
#31956 = CARTESIAN_POINT ( 'NONE',  ( 36.00000000000000711, 12.74068829017553917, 0.4871980014161889083 ) ) ;
#31957 = CARTESIAN_POINT ( 'NONE',  ( 1.287602823388475759, 6.765713844066192806, -10.61402828236309759 ) ) ;
#31958 = DIRECTION ( 'NONE',  ( 0.3865475372811020272, -0.6938894834606043061, -0.6075346789811185699 ) ) ;
#31959 = VERTEX_POINT ( 'NONE', #48449 ) ;
#31960 = B_SPLINE_CURVE_WITH_KNOTS ( 'NONE', 3,
 ( #39177, #18912, #33861, #3652, #14233, #8595, #8933, #59468, #9237, #59161, #53842, #28883, #29519, #19885, #4270, #55126, #24214, #44481, #29845 ),
 .UNSPECIFIED., .F., .F.,
 ( 4, 3, 3, 3, 3, 3, 4 ),
 ( 0.000000000000000000, 2.832085443685167180E-05, 4.217789847592021607E-05, 5.603488375296165918E-05, 6.989180858882148130E-05, 9.821094830334582552E-05, 0.0001178165571463619216 ),
 .UNSPECIFIED. ) ;
#31961 = LINE ( 'NONE', #41623, #50255 ) ;
#31962 = CIRCLE ( 'NONE', #45785, 5.000000000000000888 ) ;
#31963 = VERTEX_POINT ( 'NONE', #23156 ) ;
#31964 = FACE_OUTER_BOUND ( 'NONE', #2729, .T. ) ;
#31965 = DIRECTION ( 'NONE',  ( 0.000000000000000000, -0.01356324068818000848, 0.9999080150203990547 ) ) ;
#31966 = CIRCLE ( 'NONE', #3337, 12.75000000000000178 ) ;
#31967 = EDGE_CURVE ( 'NONE', #55740, #22166, #834, .T. ) ;
#31968 = ADVANCED_FACE ( 'NONE', ( #8192 ), #7524, .T. ) ;
#31969 = ORIENTED_EDGE ( 'NONE', *, *, #4307, .T. ) ;
#31970 = CARTESIAN_POINT ( 'NONE',  ( 0.2648978790185584908, -7.972372351883092456, 9.295532325666423290 ) ) ;
#31971 = CARTESIAN_POINT ( 'NONE',  ( 5.516018279890452902, 0.0009545156522404378389, -0.006707902355168868236 ) ) ;
#31972 = DIRECTION ( 'NONE',  ( 0.000000000000000000, -0.01356324068817998940, 0.9999080150203990547 ) ) ;
#31973 = EDGE_CURVE ( 'NONE', #3201, #57823, #51817, .T. ) ;
#31974 = ORIENTED_EDGE ( 'NONE', *, *, #52910, .T. ) ;
#31975 = AXIS2_PLACEMENT_3D ( 'NONE', #47330, #22353, #1773 ) ;
#31976 = AXIS2_PLACEMENT_3D ( 'NONE', #11079, #6100, #30371 ) ;
#31977 = EDGE_LOOP ( 'NONE', ( #44213, #6387, #60505, #51385 ) ) ;
#31978 = EDGE_LOOP ( 'NONE', ( #38006, #37702, #57293, #48981 ) ) ;
#31979 = CARTESIAN_POINT ( 'NONE',  ( 8.437200413559441614, 4.476360154859203355, -11.13383131558893346 ) ) ;
#31980 = CYLINDRICAL_SURFACE ( 'NONE', #47317, 6.936499999999988120 ) ;
#31981 = CARTESIAN_POINT ( 'NONE',  ( 2.241352910868908754, 4.843133558968205854, -5.901537464758406237 ) ) ;
#31982 = ORIENTED_EDGE ( 'NONE', *, *, #14802, .T. ) ;
#31983 = DIRECTION ( 'NONE',  ( -1.000000000000000000, 0.000000000000000000, 0.000000000000000000 ) ) ;
#31984 = EDGE_CURVE ( 'NONE', #10128, #16004, #5108, .T. ) ;
#31985 = VECTOR ( 'NONE', #32563, 1000.000000000000000 ) ;
#31986 = AXIS2_PLACEMENT_3D ( 'NONE', #49526, #3964, #24227 ) ;
#31987 = EDGE_CURVE ( 'NONE', #52675, #46377, #47580, .T. ) ;
#31988 = CARTESIAN_POINT ( 'NONE',  ( -35.05175862995318425, -0.01139565579896285874, -0.005323180402361238350 ) ) ;
#31989 = CARTESIAN_POINT ( 'NONE',  ( 1.000000000000000888, 6.664893814313781029, -3.439359016433444438 ) ) ;
#31990 = VECTOR ( 'NONE', #14041, 1000.000000000000000 ) ;
#31991 = DIRECTION ( 'NONE',  ( 1.000000000000000000, 0.000000000000000000, 0.000000000000000000 ) ) ;
#31992 = CARTESIAN_POINT ( 'NONE',  ( 0.2911222467163592231, -5.940753417478847886, -10.71854909364325614 ) ) ;
#31993 = DIRECTION ( 'NONE',  ( 0.000000000000000000, -0.01356324068817998940, 0.9999080150203990547 ) ) ;
#31994 = DIRECTION ( 'NONE',  ( 0.000000000000000000, 0.1118654143051546479, 0.9937233664769768993 ) ) ;
#31995 = CYLINDRICAL_SURFACE ( 'NONE', #64065, 12.18650000000000055 ) ;
#31996 = CIRCLE ( 'NONE', #23525, 23.66025403784440329 ) ;
#31997 = ORIENTED_EDGE ( 'NONE', *, *, #57090, .F. ) ;
#31998 = CYLINDRICAL_SURFACE ( 'NONE', #8694, 4.999999999999999112 ) ;
#31999 = CARTESIAN_POINT ( 'NONE',  ( 0.3278977287071236368, -12.26453627383315848, -0.2481246099269338867 ) ) ;
#32000 = AXIS2_PLACEMENT_3D ( 'NONE', #12920, #22583, #17600 ) ;
#32001 = ORIENTED_EDGE ( 'NONE', *, *, #36041, .T. ) ;
#32002 = DIRECTION ( 'NONE',  ( -1.000000000000000000, 0.000000000000000000, 0.000000000000000000 ) ) ;
#32003 = CARTESIAN_POINT ( 'NONE',  ( -35.00000000000000000, -4.946702696913093611, -11.13736569743279681 ) ) ;
#32004 = ORIENTED_EDGE ( 'NONE', *, *, #18933, .T. ) ;
#32005 = AXIS2_PLACEMENT_3D ( 'NONE', #4, #16293, #56185 ) ;
#32006 = AXIS2_PLACEMENT_3D ( 'NONE', #25732, #56981, #56303 ) ;
#32007 = CARTESIAN_POINT ( 'NONE',  ( 2.247206125383337749, 6.554642244887925351, 3.917979829729163921 ) ) ;
#32008 = ORIENTED_EDGE ( 'NONE', *, *, #56631, .T. ) ;
#32009 = DIRECTION ( 'NONE',  ( -1.000000000000000000, 0.000000000000000000, 0.000000000000000000 ) ) ;
#32010 = EDGE_LOOP ( 'NONE', ( #21087, #36556, #10425, #21872 ) ) ;
#32011 = ORIENTED_EDGE ( 'NONE', *, *, #39260, .T. ) ;
#32012 = CIRCLE ( 'NONE', #54413, 12.75000000000000178 ) ;
#32013 = CARTESIAN_POINT ( 'NONE',  ( 2.280717697723837034, -7.131299706077048661, 2.762096098144314560 ) ) ;
#32014 = AXIS2_PLACEMENT_3D ( 'NONE', #52198, #42501, #32215 ) ;
#32015 = VECTOR ( 'NONE', #13437, 1000.000000000000000 ) ;
#32016 = ORIENTED_EDGE ( 'NONE', *, *, #42888, .F. ) ;
#32017 = DIRECTION ( 'NONE',  ( 1.000000000000000000, 0.000000000000000000, 0.000000000000000000 ) ) ;
#32018 = CARTESIAN_POINT ( 'NONE',  ( 0.8375941296809037429, -11.54987202580284489, -4.612912274496607345 ) ) ;
#32019 = CARTESIAN_POINT ( 'NONE',  ( 2.000000000000001776, 5.585096664091945939, 4.113602740025928739 ) ) ;
#32020 = CARTESIAN_POINT ( 'NONE',  ( 1.633930747253118376, -0.7186603069043160374, -12.68212725188779544 ) ) ;
#32021 = EDGE_CURVE ( 'NONE', #21361, #21283, #48119, .T. ) ;
#32022 = ORIENTED_EDGE ( 'NONE', *, *, #6903, .T. ) ;
#32023 =( BOUNDED_SURFACE ( )  B_SPLINE_SURFACE ( 3, 1, ( 
 ( #27116, #47723 ),
 ( #22446, #11477 ),
 ( #47080, #6187 ),
 ( #37743, #2167 ) ),
 .UNSPECIFIED., .F., .F., .F. ) 
 B_SPLINE_SURFACE_WITH_KNOTS ( ( 4, 4 ),
 ( 2, 2 ),
 ( 0.000000000000000000, 1.000000000000000000 ),
 ( 0.000000000000000000, 1.000000000000000000 ),
 .UNSPECIFIED. ) 
 GEOMETRIC_REPRESENTATION_ITEM ( )  RATIONAL_B_SPLINE_SURFACE ( (
 ( 1.000000000000000000, 1.000000000000000000),
 ( 0.8716676215708681896, 0.8964445200148164483),
 ( 0.8716676215708681896, 0.8964445200148164483),
 ( 1.000000000000000000, 1.000000000000000000) ) ) 
 REPRESENTATION_ITEM ( '' )  SURFACE ( )  );
#32024 = CARTESIAN_POINT ( 'NONE',  ( -4.989057617119011745, -0.9162120371760335003, -11.96497202265568660 ) ) ;
#32025 = CARTESIAN_POINT ( 'NONE',  ( 9.730232070128172595, -26.74067542416307219, 13.98809302346541372 ) ) ;
#32026 = CARTESIAN_POINT ( 'NONE',  ( -22.65999102136915866, -4.797155153747071132, -0.5917351393135312776 ) ) ;
#32028 = VERTEX_POINT ( 'NONE', #63373 ) ;
#32027 = DIRECTION ( 'NONE',  ( 0.000000000000000000, 0.000000000000000000, 1.000000000000000000 ) ) ;
#32029 = CARTESIAN_POINT ( 'NONE',  ( 36.00000000000000711, -12.70128625845191728, 1.113475361586617307 ) ) ;
#32030 = ORIENTED_EDGE ( 'NONE', *, *, #52938, .T. ) ;
#32031 = CARTESIAN_POINT ( 'NONE',  ( 0.2651627923886347715, 9.437479615842747194, -7.803990550466204823 ) ) ;
#32032 = ORIENTED_EDGE ( 'NONE', *, *, #47004, .F. ) ;
#32033 = CARTESIAN_POINT ( 'NONE',  ( 0.000000000000000000, -33.00000000000000000, 0.000000000000000000 ) ) ;
#32034 = VECTOR ( 'NONE', #49541, 1000.000000000000000 ) ;
#32035 = FACE_OUTER_BOUND ( 'NONE', #54943, .T. ) ;
#32036 = CARTESIAN_POINT ( 'NONE',  ( 1.109979610369590253, -4.732439402373736392, 11.59954799439085349 ) ) ;
#32037 = CIRCLE ( 'NONE', #50094, 6.936499999999989008 ) ;
#32038 = ORIENTED_EDGE ( 'NONE', *, *, #5555, .F. ) ;
#32039 = EDGE_CURVE ( 'NONE', #23644, #64143, #35883, .T. ) ;
#32040 = DIRECTION ( 'NONE',  ( 0.000000000000000000, 0.01356324068817998940, -0.9999080150203990547 ) ) ;
#32041 = CARTESIAN_POINT ( 'NONE',  ( -35.04643116707788408, 0.002453861112619928897, 0.01193867652719490802 ) ) ;
#32042 = CARTESIAN_POINT ( 'NONE',  ( -22.28284753389937123, -3.581493264753385475, -0.9231250029035383831 ) ) ;
#32044 = ORIENTED_EDGE ( 'NONE', *, *, #60346, .T. ) ;
#32043 = VECTOR ( 'NONE', #25063, 1000.000000000000000 ) ;
#32045 = ORIENTED_EDGE ( 'NONE', *, *, #65454, .F. ) ;
#32046 = CARTESIAN_POINT ( 'NONE',  ( 0.000000000000000000, -30.00000000000000000, 0.000000000000000000 ) ) ;
#32047 = VERTEX_POINT ( 'NONE', #18176 ) ;
#32048 = EDGE_LOOP ( 'NONE', ( #7157, #6375, #29757, #25153 ) ) ;
#32049 = AXIS2_PLACEMENT_3D ( 'NONE', #33384, #53680, #8119 ) ;
#32050 = CARTESIAN_POINT ( 'NONE',  ( -35.00000000000000000, 0.000000000000000000, 0.000000000000000000 ) ) ;
#32051 = CYLINDRICAL_SURFACE ( 'NONE', #28360, 13.50000000000000178 ) ;
#32052 = CARTESIAN_POINT ( 'NONE',  ( -35.00000000000000000, -9.733281772932219411, 8.235637554476609168 ) ) ;
#32053 = CARTESIAN_POINT ( 'NONE',  ( 2.000000000000001776, 0.000000000000000000, 0.000000000000000000 ) ) ;
#32054 = CARTESIAN_POINT ( 'NONE',  ( 2.000000000000001776, 0.000000000000000000, 0.000000000000000000 ) ) ;
#32055 = CARTESIAN_POINT ( 'NONE',  ( 0.000000000000000000, 1.693411908627302509, -7.306323022404582979 ) ) ;
#32056 = B_SPLINE_CURVE_WITH_KNOTS ( 'NONE', 3,
 ( #20677, #31306, #62524, #51927, #10676, #55919, #52259, #51607, #21317, #5729 ),
 .UNSPECIFIED., .F., .F.,
 ( 4, 2, 2, 2, 4 ),
 ( 0.005844473438883908585, 0.006520250652290781289, 0.007196027865697654860, 0.007871805079104527564, 0.008547582292511400268 ),
 .UNSPECIFIED. ) ;
#32057 = LINE ( 'NONE', #47696, #30188 ) ;
#32058 = AXIS2_PLACEMENT_3D ( 'NONE', #16623, #56186, #14394 ) ;
#32059 = ORIENTED_EDGE ( 'NONE', *, *, #28178, .F. ) ;
#32060 = CARTESIAN_POINT ( 'NONE',  ( -22.29479313954897535, -3.090162644873540643, 2.096782908204888773 ) ) ;
#32061 = AXIS2_PLACEMENT_3D ( 'NONE', #4256, #58235, #2045 ) ;
#32062 = CARTESIAN_POINT ( 'NONE',  ( 0.3401186441510233305, 4.436257390736984441, -11.44115600261386767 ) ) ;
#32063 = CIRCLE ( 'NONE', #38484, 12.18650000000000055 ) ;
#32064 = DIRECTION ( 'NONE',  ( -1.000000000000000000, 0.000000000000000000, 0.000000000000000000 ) ) ;
#32065 = CARTESIAN_POINT ( 'NONE',  ( 0.2653519789438776311, 12.05632450344285544, -2.148225749114869743 ) ) ;
#32066 = DIRECTION ( 'NONE',  ( -0.4298323628305344979, -0.9029087107030918657, 0.000000000000000000 ) ) ;
#32067 = ORIENTED_EDGE ( 'NONE', *, *, #50831, .F. ) ;
#32068 = CARTESIAN_POINT ( 'NONE',  ( -41.00000000000000711, -25.03188948156373783, 4.499999999999997335 ) ) ;
#32069 = EDGE_CURVE ( 'NONE', #31780, #62820, #22165, .T. ) ;
#32070 = DIRECTION ( 'NONE',  ( 1.000000000000000000, -0.000000000000000000, 0.000000000000000000 ) ) ;
#32071 = DIRECTION ( 'NONE',  ( -1.000000000000000000, 0.000000000000000000, 0.000000000000000000 ) ) ;
#32072 = CARTESIAN_POINT ( 'NONE',  ( -25.74864769002726561, -4.845157721295400677, 10.98320407977280055 ) ) ;
#32073 = AXIS2_PLACEMENT_3D ( 'NONE', #55093, #14832, #35117 ) ;
#32074 = EDGE_CURVE ( 'NONE', #8430, #64491, #40106, .T. ) ;
#32075 = CIRCLE ( 'NONE', #261, 5.000000000000000000 ) ;
#32076 = CARTESIAN_POINT ( 'NONE',  ( 9.042385582766643282, 3.534140635374256600, -13.03150467260951295 ) ) ;
#32077 = CARTESIAN_POINT ( 'NONE',  ( -25.68256394590837033, -11.85982374565230124, 6.450774052159548688 ) ) ;
#32078 = EDGE_LOOP ( 'NONE', ( #35663, #55444, #16161, #37 ) ) ;
#32079 = CARTESIAN_POINT ( 'NONE',  ( 37.00000000000000711, -2.968224442958486975, -11.81949347079746282 ) ) ;
#32080 = DIRECTION ( 'NONE',  ( -1.000000000000000000, 0.000000000000000000, 0.000000000000000000 ) ) ;
#32081 = LINE ( 'NONE', #52398, #42688 ) ;
#32082 = AXIS2_PLACEMENT_3D ( 'NONE', #48507, #28529, #7602 ) ;
#32083 = CARTESIAN_POINT ( 'NONE',  ( 2.298277635560280086, 1.166137492762227224, 7.564013289873174450 ) ) ;
#32084 = VERTEX_POINT ( 'NONE', #22506 ) ;
#32085 = CARTESIAN_POINT ( 'NONE',  ( 2.430348790457427910, 6.761480562106370940, 3.678671624790056605 ) ) ;
#32086 = DIRECTION ( 'NONE',  ( -1.000000000000000000, 0.000000000000000000, -0.000000000000000000 ) ) ;
#32088 = ORIENTED_EDGE ( 'NONE', *, *, #29089, .F. ) ;
#32087 = FACE_OUTER_BOUND ( 'NONE', #55441, .T. ) ;
#32089 = DIRECTION ( 'NONE',  ( -1.000000000000000000, 0.000000000000000000, 0.000000000000000000 ) ) ;
#32090 = ADVANCED_FACE ( 'NONE', ( #42766 ), #32775, .T. ) ;
#32091 = DIRECTION ( 'NONE',  ( 0.000000000000000000, 0.3807014730195220631, -0.9246979985058721985 ) ) ;
#32092 = ORIENTED_EDGE ( 'NONE', *, *, #47148, .F. ) ;
#32093 = DIRECTION ( 'NONE',  ( 0.000000000000000000, 0.01356324068818000848, -0.9999080150203990547 ) ) ;
#32094 = CIRCLE ( 'NONE', #55468, 5.000000000000000888 ) ;
#32095 = CARTESIAN_POINT ( 'NONE',  ( -35.00000000000000000, -9.752226076388847531, -6.547236723514122225 ) ) ;
#32096 = CARTESIAN_POINT ( 'NONE',  ( -37.00000000000000711, -11.56998259273174945, -3.827046518385204266 ) ) ;
#32097 = DIRECTION ( 'NONE',  ( 0.7884253166185480888, 0.000000000000000000, -0.6151304903148129277 ) ) ;
#32098 = ADVANCED_FACE ( 'NONE', ( #43099 ), #26382, .T. ) ;
#32099 = DIRECTION ( 'NONE',  ( -1.000000000000000000, -0.000000000000000000, -0.000000000000000000 ) ) ;
#32100 = EDGE_CURVE ( 'NONE', #7784, #63668, #46479, .T. ) ;
#32101 = B_SPLINE_CURVE_WITH_KNOTS ( 'NONE', 3,
 ( #13771, #23116, #59043, #34063, #54379, #19451, #40355, #55006, #10427, #5476, #19778, #65618, #55338 ),
 .UNSPECIFIED., .F., .F.,
 ( 4, 3, 3, 3, 4 ),
 ( 8.673617379884035472E-19, 6.607593386745623195E-05, 0.0001321518677373556051, 0.0001982171734706223505, 0.0002642860854759480666 ),
 .UNSPECIFIED. ) ;
#32102 = CARTESIAN_POINT ( 'NONE',  ( 37.00000000000000711, -9.348667969174460524, -7.817492529713823579 ) ) ;
#32104 = ORIENTED_EDGE ( 'NONE', *, *, #41227, .T. ) ;
#32103 = CARTESIAN_POINT ( 'NONE',  ( 1.459561108992816880, 0.6317018236571978473, 12.62847742794662409 ) ) ;
#32105 = EDGE_CURVE ( 'NONE', #42804, #31183, #11453, .T. ) ;
#32106 = CARTESIAN_POINT ( 'NONE',  ( -22.27721701579900682, 2.409654355488404676, 2.783642043008622391 ) ) ;
#32107 = ORIENTED_EDGE ( 'NONE', *, *, #10910, .T. ) ;
#32108 = DIRECTION ( 'NONE',  ( -1.000000000000000000, -0.000000000000000000, 0.000000000000000000 ) ) ;
#32109 = VERTEX_POINT ( 'NONE', #37002 ) ;
#32110 = AXIS2_PLACEMENT_3D ( 'NONE', #44530, #24262, #64807 ) ;
#32111 = CARTESIAN_POINT ( 'NONE',  ( 0.8320506296491606557, -11.54877388447407860, 4.610676791972301736 ) ) ;
#32113 = CARTESIAN_POINT ( 'NONE',  ( -35.00000000000000000, 5.143145423404449801, -11.66664283989674367 ) ) ;
#32112 = VECTOR ( 'NONE', #37894, 1000.000000000000000 ) ;
#32114 = CIRCLE ( 'NONE', #3493, 5.000000000000000888 ) ;
#32115 = EDGE_CURVE ( 'NONE', #27902, #63537, #6774, .T. ) ;
#32116 = DIRECTION ( 'NONE',  ( 1.000000000000000000, 0.000000000000000000, 0.000000000000000000 ) ) ;
#32117 = ORIENTED_EDGE ( 'NONE', *, *, #46390, .F. ) ;
#32118 = DIRECTION ( 'NONE',  ( 1.000000000000000000, -0.000000000000000000, -0.000000000000000000 ) ) ;
#32120 = ADVANCED_FACE ( 'NONE', ( #7083 ), #46665, .T. ) ;
#32119 = CARTESIAN_POINT ( 'NONE',  ( 0.000000000000000000, -2.473437528934186780, 7.080403010454960899 ) ) ;
#32121 = ORIENTED_EDGE ( 'NONE', *, *, #10407, .F. ) ;
#32122 = ORIENTED_EDGE ( 'NONE', *, *, #35984, .F. ) ;
#32123 = CARTESIAN_POINT ( 'NONE',  ( 2.257661810676417691, -7.224098098130513179, -2.485866587321456933 ) ) ;
#32124 = EDGE_LOOP ( 'NONE', ( #44990, #52365, #12381, #25135 ) ) ;
#32125 = CARTESIAN_POINT ( 'NONE',  ( 35.00000000000000000, 4.705694406421931860E-17, -3.469127814946512892E-15 ) ) ;
#32126 = CARTESIAN_POINT ( 'NONE',  ( -22.31328051695926007, 3.148362328073167404, -2.109671368890616350 ) ) ;
#32127 = CARTESIAN_POINT ( 'NONE',  ( 12.52750123246316072, 0.4973700281276248192, 13.49083477977253764 ) ) ;
#32128 = DIRECTION ( 'NONE',  ( 1.000000000000000000, -0.000000000000000000, 0.000000000000000000 ) ) ;
#32129 = CARTESIAN_POINT ( 'NONE',  ( -25.00000000000000355, -9.999999999999998224, -5.000000000000000888 ) ) ;
#32130 = CARTESIAN_POINT ( 'NONE',  ( 37.00000000000000711, 11.68758509253246558, -1.171570255487653700 ) ) ;
#32131 = EDGE_CURVE ( 'NONE', #52959, #64071, #6161, .T. ) ;
#32132 = CARTESIAN_POINT ( 'NONE',  ( 1.000000000000000888, -5.769711778877330666, 4.791703871138493831 ) ) ;
#32133 = ORIENTED_EDGE ( 'NONE', *, *, #25523, .F. ) ;
#32134 = FACE_OUTER_BOUND ( 'NONE', #18243, .T. ) ;
#32135 = ORIENTED_EDGE ( 'NONE', *, *, #63274, .T. ) ;
#32136 = CIRCLE ( 'NONE', #1415, 5.000000000000000888 ) ;
#32137 = CARTESIAN_POINT ( 'NONE',  ( 35.00000000000000000, -11.68758509253247091, 1.171570255487570655 ) ) ;
#32138 = LINE ( 'NONE', #26837, #23192 ) ;
#32139 = LINE ( 'NONE', #31494, #58396 ) ;
#32140 = DIRECTION ( 'NONE',  ( 0.000000000000000000, -0.9289767198167871998, -0.3701381553399247792 ) ) ;
#32141 = CARTESIAN_POINT ( 'NONE',  ( 5.516018279890452902, 0.004180585980734530596, -0.005331956019561480582 ) ) ;
#32142 = VERTEX_POINT ( 'NONE', #51679 ) ;
#32143 = ORIENTED_EDGE ( 'NONE', *, *, #14242, .T. ) ;
#32144 = DIRECTION ( 'NONE',  ( 0.000000000000000000, 0.01356324068817992695, -0.9999080150203990547 ) ) ;
#32145 = EDGE_LOOP ( 'NONE', ( #18485, #25333 ) ) ;
#32146 = FACE_OUTER_BOUND ( 'NONE', #17251, .T. ) ;
#32147 = FACE_OUTER_BOUND ( 'NONE', #227, .T. ) ;
#32148 = DIRECTION ( 'NONE',  ( 1.000000000000000000, 0.000000000000000000, 0.000000000000000000 ) ) ;
#32149 = CARTESIAN_POINT ( 'NONE',  ( -35.05175862995318425, 0.01216930940959280727, 0.003178856583437375538 ) ) ;
#32150 = ORIENTED_EDGE ( 'NONE', *, *, #32469, .F. ) ;
#32151 = CIRCLE ( 'NONE', #3530, 12.74999999999999822 ) ;
#32152 = CARTESIAN_POINT ( 'NONE',  ( 0.3006302518452025341, 12.10891847026072199, 1.905681544119282034 ) ) ;
#32153 = DIRECTION ( 'NONE',  ( -1.000000000000000000, 0.000000000000000000, 0.000000000000000000 ) ) ;
#32154 = CARTESIAN_POINT ( 'NONE',  ( -29.68541646480307605, -0.9874700634933176735, -13.47073127497727363 ) ) ;
#32155 = CARTESIAN_POINT ( 'NONE',  ( -49.99855491382518835, -0.0002949769214475305985, 1.660073069598965390 ) ) ;
#32156 = CIRCLE ( 'NONE', #31088, 4.999999999999999112 ) ;
#32157 = ADVANCED_FACE ( 'NONE', ( #26072 ), #62594, .T. ) ;
#32158 = CIRCLE ( 'NONE', #25819, 2.899999999999994582 ) ;
#32159 = CARTESIAN_POINT ( 'NONE',  ( 0.3218525148189821383, 6.342972338926943010, -10.49750909897045936 ) ) ;
#32160 = ORIENTED_EDGE ( 'NONE', *, *, #56771, .T. ) ;
#32161 = CIRCLE ( 'NONE', #50284, 12.18650000000000055 ) ;
#32162 = CARTESIAN_POINT ( 'NONE',  ( -17.92531974009704498, -28.72851451116432031, -8.222150688345376324 ) ) ;
#32163 = ORIENTED_EDGE ( 'NONE', *, *, #56789, .F. ) ;
#32164 = CARTESIAN_POINT ( 'NONE',  ( 2.241352910868908754, -6.652881166698485949, -3.744764251557062718 ) ) ;
#32165 = CARTESIAN_POINT ( 'NONE',  ( 2.000000000000001776, -5.396716205731451943, 4.158041573745051345 ) ) ;
#32166 = AXIS2_PLACEMENT_3D ( 'NONE', #60364, #14792, #9822 ) ;
#32167 = CARTESIAN_POINT ( 'NONE',  ( -35.00000000000000000, 0.000000000000000000, 0.000000000000000000 ) ) ;
#32168 = CARTESIAN_POINT ( 'NONE',  ( -3.740102306720532788, 25.00000000000000000, -6.044082642436763742 ) ) ;
#32169 = VECTOR ( 'NONE', #26152, 1000.000000000000000 ) ;
#32170 = EDGE_CURVE ( 'NONE', #49222, #42435, #61300, .T. ) ;
#32171 = ORIENTED_EDGE ( 'NONE', *, *, #37615, .F. ) ;
#32172 = VERTEX_POINT ( 'NONE', #61620 ) ;
#32173 = LINE ( 'NONE', #17565, #27632 ) ;
#32174 = VERTEX_POINT ( 'NONE', #37338 ) ;
#32175 = CARTESIAN_POINT ( 'NONE',  ( 2.091509324218079335, 2.103201000890800199, 11.81927150886677502 ) ) ;
#32176 = CARTESIAN_POINT ( 'NONE',  ( -35.04582288351658548, -0.01249938581188633595, -0.002280196168886043998 ) ) ;
#32177 = CARTESIAN_POINT ( 'NONE',  ( 22.36482863261543486, -13.46837713145126791, -0.9234811557364140944 ) ) ;
#32178 = CYLINDRICAL_SURFACE ( 'NONE', #25812, 2.999999999999995559 ) ;
#32179 = CARTESIAN_POINT ( 'NONE',  ( -35.00000000000000000, 6.917234959366964198, -9.493370459201624811 ) ) ;
#32180 = EDGE_CURVE ( 'NONE', #37744, #55487, #53565, .T. ) ;
#32181 = AXIS2_PLACEMENT_3D ( 'NONE', #32296, #6725, #42253 ) ;
#32182 = CARTESIAN_POINT ( 'NONE',  ( 2.259025283528083072, -1.191911401085066435, 7.546748801935439843 ) ) ;
#32183 = CARTESIAN_POINT ( 'NONE',  ( -10.25071159343468352, -3.780199704946288985, 11.39050396304778268 ) ) ;
#32184 = ORIENTED_EDGE ( 'NONE', *, *, #20418, .T. ) ;
#32185 = EDGE_CURVE ( 'NONE', #53581, #57915, #10757, .T. ) ;
#32186 = ORIENTED_EDGE ( 'NONE', *, *, #40830, .T. ) ;
#32187 = DIRECTION ( 'NONE',  ( 0.000000000000000000, 0.01356324068818000328, -0.9999080150203990547 ) ) ;
#32188 = VERTEX_POINT ( 'NONE', #16422 ) ;
#32189 = FILL_AREA_STYLE_COLOUR ( '', #52602 ) ;
#32190 = DIRECTION ( 'NONE',  ( 0.000000000000000000, 0.000000000000000000, 1.000000000000000000 ) ) ;
#32191 = CARTESIAN_POINT ( 'NONE',  ( 1.452237505248552996, 0.5922625322518776381, -12.64182585313125351 ) ) ;
#32192 = AXIS2_PLACEMENT_3D ( 'NONE', #64372, #15142, #24147 ) ;
#32193 = EDGE_CURVE ( 'NONE', #16970, #25922, #56987, .T. ) ;
#32194 = DIRECTION ( 'NONE',  ( -0.9688695217174486674, 0.000000000000000000, -0.2475719085175094036 ) ) ;
#32195 = ORIENTED_EDGE ( 'NONE', *, *, #7526, .T. ) ;
#32196 = CARTESIAN_POINT ( 'NONE',  ( 35.00000000000000000, 11.74226168163341377, 0.3025107581129941048 ) ) ;
#32197 = CARTESIAN_POINT ( 'NONE',  ( -13.57005631242148347, -30.10739101144412544, -6.607437777791871802 ) ) ;
#32199 = EDGE_CURVE ( 'NONE', #23561, #20597, #12309, .T. ) ;
#32198 = CARTESIAN_POINT ( 'NONE',  ( 2.941278708680199916, -4.615461433467229924, -4.048809123187982806 ) ) ;
#32200 = ORIENTED_EDGE ( 'NONE', *, *, #51659, .F. ) ;
#32201 = ORIENTED_EDGE ( 'NONE', *, *, #12436, .T. ) ;
#32202 = CARTESIAN_POINT ( 'NONE',  ( 3.369063103260706793, 5.393734308210048845, 12.37743201445020347 ) ) ;
#32204 = ORIENTED_EDGE ( 'NONE', *, *, #31011, .T. ) ;
#32203 = EDGE_CURVE ( 'NONE', #15892, #26006, #28673, .T. ) ;
#32205 = ORIENTED_EDGE ( 'NONE', *, *, #11895, .T. ) ;
#32206 = AXIS2_PLACEMENT_3D ( 'NONE', #34480, #44776, #28087 ) ;
#32207 = VERTEX_POINT ( 'NONE', #48985 ) ;
#32209 = EDGE_CURVE ( 'NONE', #32360, #12705, #65418, .T. ) ;
#32208 = ORIENTED_EDGE ( 'NONE', *, *, #44443, .T. ) ;
#32210 = CARTESIAN_POINT ( 'NONE',  ( 2.241536586108914708, -7.171901127201312676, 2.617055111126424638 ) ) ;
#32211 = CARTESIAN_POINT ( 'NONE',  ( 2.242819959140601060, 4.985618132689532800, -5.782321801516662418 ) ) ;
#32212 = CIRCLE ( 'NONE', #40718, 12.18650000000000055 ) ;
#32213 = B_SPLINE_CURVE_WITH_KNOTS ( 'NONE', 3,
 ( #34535, #30518, #15557, #35817, #50822, #24560 ),
 .UNSPECIFIED., .F., .F.,
 ( 4, 2, 4 ),
 ( 0.005435758617312099611, 0.006631938927966533892, 0.007828119238620968173 ),
 .UNSPECIFIED. ) ;
#32214 = VECTOR ( 'NONE', #23203, 1000.000000000000114 ) ;
#32215 = DIRECTION ( 'NONE',  ( 0.000000000000000000, 0.000000000000000000, 1.000000000000000000 ) ) ;
#32216 = CARTESIAN_POINT ( 'NONE',  ( -37.00000000000000711, -8.029056188533626681, -8.573591947375405198 ) ) ;
#32217 = DIRECTION ( 'NONE',  ( 0.7884253166185480888, 0.000000000000000000, -0.6151304903148129277 ) ) ;
#32218 = ORIENTED_EDGE ( 'NONE', *, *, #49724, .F. ) ;
#32219 = EDGE_CURVE ( 'NONE', #815, #26332, #48634, .T. ) ;
#32220 = DIRECTION ( 'NONE',  ( -1.000000000000000000, 0.000000000000000000, 0.000000000000000000 ) ) ;
#32221 = ORIENTED_EDGE ( 'NONE', *, *, #42615, .T. ) ;
#32222 = CYLINDRICAL_SURFACE ( 'NONE', #35924, 5.000000000000000888 ) ;
#32224 = CARTESIAN_POINT ( 'NONE',  ( 3.152665057736135701, -1.848755561854027452, -7.719888720907647439 ) ) ;
#32223 = AXIS2_PLACEMENT_3D ( 'NONE', #58512, #12278, #2676 ) ;
#32225 = EDGE_CURVE ( 'NONE', #22078, #26234, #4460, .T. ) ;
#32226 = CARTESIAN_POINT ( 'NONE',  ( 2.259025283528611538, 3.701170455110545987, -6.683966451873481596 ) ) ;
#32227 = CARTESIAN_POINT ( 'NONE',  ( 0.3341166715381306829, -8.078283863465435033, -9.234320413907880720 ) ) ;
#32228 = AXIS2_PLACEMENT_3D ( 'NONE', #23601, #48870, #64154 ) ;
#32229 = CARTESIAN_POINT ( 'NONE',  ( -37.00000000000000711, 10.91072401419410554, 5.428340790341743549 ) ) ;
#32230 = CYLINDRICAL_SURFACE ( 'NONE', #65234, 5.000000000000000888 ) ;
#32231 = VECTOR ( 'NONE', #61972, 1000.000000000000114 ) ;
#32232 = ORIENTED_EDGE ( 'NONE', *, *, #21823, .F. ) ;
#32233 = CARTESIAN_POINT ( 'NONE',  ( 2.994568964204208594, -7.263701055179705435, -3.069094401380853210 ) ) ;
#32234 = CIRCLE ( 'NONE', #62992, 5.000000000000000888 ) ;
#32235 = VERTEX_POINT ( 'NONE', #17401 ) ;
#32236 = CARTESIAN_POINT ( 'NONE',  ( 5.515188684475870851, -0.002166413411657830065, -0.004893136156457991714 ) ) ;
#32237 = CARTESIAN_POINT ( 'NONE',  ( 0.2869720083484346151, -0.2084396331387487200, 12.25163264065381874 ) ) ;
#32238 = AXIS2_PLACEMENT_3D ( 'NONE', #11613, #37872, #42853 ) ;
#32239 = CARTESIAN_POINT ( 'NONE',  ( 3.152665057734120868, 6.378477742800529704, -4.725420687650643714 ) ) ;
#32240 = CARTESIAN_POINT ( 'NONE',  ( -27.08430792439081003, -0.5856059198894515427, -2.215465963318195897 ) ) ;
#32241 = DIRECTION ( 'NONE',  ( -1.000000000000000000, 0.000000000000000000, -0.000000000000000000 ) ) ;
#32242 = VERTEX_POINT ( 'NONE', #7396 ) ;
#32243 = CARTESIAN_POINT ( 'NONE',  ( 0.000000000000000000, 7.387287142779368487, -1.295372019972108601 ) ) ;
#32244 = CARTESIAN_POINT ( 'NONE',  ( 2.000000000000001776, 5.450255447309745982, 4.087611905901426645 ) ) ;
#32245 = DIRECTION ( 'NONE',  ( -0.000000000000000000, -0.000000000000000000, -1.000000000000000000 ) ) ;
#32246 = CARTESIAN_POINT ( 'NONE',  ( -3.992466187133344668, 11.80999507292766992, 6.552767039380011482 ) ) ;
#32247 = EDGE_CURVE ( 'NONE', #54467, #19899, #16339, .T. ) ;
#32248 = AXIS2_PLACEMENT_3D ( 'NONE', #55183, #25580, #40204 ) ;
#32249 = CARTESIAN_POINT ( 'NONE',  ( 2.000000000000001776, -1.058508696394911963, -6.730038252034928448 ) ) ;
#32250 = VERTEX_POINT ( 'NONE', #63891 ) ;
#32251 = CARTESIAN_POINT ( 'NONE',  ( 5.514970785353741078, 0.004694330894494369230, -0.0005190732562558711188 ) ) ;
#32252 = CARTESIAN_POINT ( 'NONE',  ( 0.2651627682582919920, -2.039709641845663057, 12.07509313786331795 ) ) ;
#32253 = CIRCLE ( 'NONE', #19604, 5.000000000000000000 ) ;
#32254 = ADVANCED_FACE ( 'NONE', ( #43274 ), #47624, .T. ) ;
#32255 = AXIS2_PLACEMENT_3D ( 'NONE', #50953, #45618, #19393 ) ;
#32256 = EDGE_CURVE ( 'NONE', #33557, #49753, #64548, .T. ) ;
#32257 = VERTEX_POINT ( 'NONE', #3075 ) ;
#32258 = ORIENTED_EDGE ( 'NONE', *, *, #25069, .F. ) ;
#32260 = CIRCLE ( 'NONE', #17430, 5.000000000000000000 ) ;
#32259 = CARTESIAN_POINT ( 'NONE',  ( 3.031336079629648683, -6.621879275826741740, 4.304138522350468676 ) ) ;
#32261 = CARTESIAN_POINT ( 'NONE',  ( -27.09030469827880339, -1.657623467483503754, -1.608164674722925458 ) ) ;
#32262 = CARTESIAN_POINT ( 'NONE',  ( 37.00000000000000711, 4.705694406421931860E-17, -3.469127814946512892E-15 ) ) ;
#32263 = CIRCLE ( 'NONE', #25929, 5.000000000000000000 ) ;
#32264 = LINE ( 'NONE', #57562, #26491 ) ;
#32265 = ORIENTED_EDGE ( 'NONE', *, *, #8526, .T. ) ;
#32266 = EDGE_CURVE ( 'NONE', #34799, #30454, #18025, .T. ) ;
#32267 = AXIS2_PLACEMENT_3D ( 'NONE', #11686, #51310, #31965 ) ;
#32268 = VERTEX_POINT ( 'NONE', #18370 ) ;
#32269 = ORIENTED_EDGE ( 'NONE', *, *, #24719, .F. ) ;
#32270 = CARTESIAN_POINT ( 'NONE',  ( 27.85875306725328571, -11.11252398976967903, 4.542717126716967257 ) ) ;
#32271 = AXIS2_PLACEMENT_3D ( 'NONE', #61802, #42158, #32190 ) ;
#32272 = CARTESIAN_POINT ( 'NONE',  ( -27.35552965826137140, 2.548625910254547655, 1.773915698030531951 ) ) ;
#32273 = ORIENTED_EDGE ( 'NONE', *, *, #5034, .F. ) ;
#32274 = DIRECTION ( 'NONE',  ( -1.000000000000000000, 0.000000000000000000, 0.000000000000000000 ) ) ;
#32275 = DIRECTION ( 'NONE',  ( 0.000000000000000000, 0.000000000000000000, 1.000000000000000000 ) ) ;
#32276 = ORIENTED_EDGE ( 'NONE', *, *, #25601, .T. ) ;
#32277 = DIRECTION ( 'NONE',  ( -1.000000000000000000, 0.000000000000000000, 0.000000000000000000 ) ) ;
#32278 = VECTOR ( 'NONE', #29511, 1000.000000000000000 ) ;
#32279 = DIRECTION ( 'NONE',  ( 0.000000000000000000, 0.01356324068817992175, -0.9999080150203990547 ) ) ;
#32280 = CARTESIAN_POINT ( 'NONE',  ( 24.51709394181822432, -2.671539114876285037, 11.70037924786635486 ) ) ;
#32281 = ORIENTED_EDGE ( 'NONE', *, *, #27463, .T. ) ;
#32282 = CARTESIAN_POINT ( 'NONE',  ( 0.2911222467163586680, 12.10399882413662631, -1.916522451062410592 ) ) ;
#32283 = ORIENTED_EDGE ( 'NONE', *, *, #29958, .F. ) ;
#32284 = DIRECTION ( 'NONE',  ( -0.000000000000000000, -0.000000000000000000, -1.000000000000000000 ) ) ;
#32285 = CARTESIAN_POINT ( 'NONE',  ( 2.241509619876139503, 4.877966158328305823, 5.872890204493035782 ) ) ;
#32286 = EDGE_CURVE ( 'NONE', #18418, #50038, #16771, .T. ) ;
#32287 = CARTESIAN_POINT ( 'NONE',  ( -19.69476066079020171, -4.201994156881551312, 11.24025111398909615 ) ) ;
#32288 = DIRECTION ( 'NONE',  ( 0.000000000000000000, 0.01356324068817992175, -0.9999080150203990547 ) ) ;
#32289 = VECTOR ( 'NONE', #13657, 1000.000000000000000 ) ;
#32290 = CYLINDRICAL_SURFACE ( 'NONE', #62208, 12.75000000000000178 ) ;
#32291 = CARTESIAN_POINT ( 'NONE',  ( 35.00000000000000000, 4.705694406421931860E-17, -3.469127814946512892E-15 ) ) ;
#32292 = CARTESIAN_POINT ( 'NONE',  ( 1.634816307077887831, 6.964001572436961496, -10.62369813896834359 ) ) ;
#32293 = CARTESIAN_POINT ( 'NONE',  ( -27.70104025454409680, -11.17792676666258878, -4.374904684088040341 ) ) ;
#32294 = ORIENTED_EDGE ( 'NONE', *, *, #40446, .F. ) ;
#32295 = ADVANCED_FACE ( 'NONE', ( #13033 ), #47316, .T. ) ;
#32296 = CARTESIAN_POINT ( 'NONE',  ( 2.000000000000001776, 0.000000000000000000, 0.000000000000000000 ) ) ;
#32297 = ORIENTED_EDGE ( 'NONE', *, *, #32474, .T. ) ;
#32298 = CARTESIAN_POINT ( 'NONE',  ( 0.2648321136542688414, -4.321267941897585452, 11.45826514585342082 ) ) ;
#32299 = DIRECTION ( 'NONE',  ( 0.000000000000000000, -0.5243256840888443904, -0.8515178078024941977 ) ) ;
#32300 = EDGE_CURVE ( 'NONE', #6547, #19851, #37976, .T. ) ;
#32301 = CIRCLE ( 'NONE', #3678, 5.000000000000000888 ) ;
#32302 = VERTEX_POINT ( 'NONE', #12683 ) ;
#32304 = AXIS2_PLACEMENT_3D ( 'NONE', #64707, #39447, #35446 ) ;
#32303 = CARTESIAN_POINT ( 'NONE',  ( 2.941278708680199916, -6.021511413163968207, 1.198640839021288818 ) ) ;
#32305 = CARTESIAN_POINT ( 'NONE',  ( 0.2647959493198550618, 12.03358727341677614, -2.271080632827937595 ) ) ;
#32306 = CARTESIAN_POINT ( 'NONE',  ( 2.000000000000001776, -6.160607635185357367, -4.277489166005654653 ) ) ;
#32307 = ORIENTED_EDGE ( 'NONE', *, *, #35423, .F. ) ;
#32308 = ORIENTED_EDGE ( 'NONE', *, *, #21039, .T. ) ;
#32309 = LINE ( 'NONE', #52624, #52378 ) ;
#32310 = ORIENTED_EDGE ( 'NONE', *, *, #36737, .T. ) ;
#32311 = CARTESIAN_POINT ( 'NONE',  ( 2.827825597296802496, 3.592949031604531385, -8.278234963587674855 ) ) ;
#32312 = DIRECTION ( 'NONE',  ( 0.000000000000000000, 0.3218879778915972878, -0.9467777615094571386 ) ) ;
#32313 = CARTESIAN_POINT ( 'NONE',  ( -22.27218376572352554, 3.330959526935401538, 1.571356284315131413 ) ) ;
#32314 = DIRECTION ( 'NONE',  ( -1.000000000000000000, 0.000000000000000000, 0.000000000000000000 ) ) ;
#32315 = DIRECTION ( 'NONE',  ( -1.000000000000000000, 0.000000000000000000, 0.000000000000000000 ) ) ;
#32316 = ORIENTED_EDGE ( 'NONE', *, *, #65182, .T. ) ;
#32317 = CARTESIAN_POINT ( 'NONE',  ( 0.2646305136544065406, 12.03696649559614507, 2.256625640822357060 ) ) ;
#32318 = AXIS2_PLACEMENT_3D ( 'NONE', #33817, #39802, #34784 ) ;
#32319 = EDGE_CURVE ( 'NONE', #55560, #24405, #43288, .T. ) ;
#32320 = EDGE_CURVE ( 'NONE', #34385, #12941, #53945, .T. ) ;
#32321 = CARTESIAN_POINT ( 'NONE',  ( 19.42209513767211604, -30.00000000000001066, -5.494601501491743534 ) ) ;
#32322 = CARTESIAN_POINT ( 'NONE',  ( 47.00000000000000711, 4.705694406421931860E-17, -3.469127814946512892E-15 ) ) ;
#32323 = AXIS2_PLACEMENT_3D ( 'NONE', #28350, #63259, #18724 ) ;
#32324 = CARTESIAN_POINT ( 'NONE',  ( 2.177405672432021877, -3.189307221897416333, 10.73538068360473829 ) ) ;
#32325 = CARTESIAN_POINT ( 'NONE',  ( 35.00000000000000000, 4.705694406421931860E-17, -3.469127814946512892E-15 ) ) ;
#32326 = CARTESIAN_POINT ( 'NONE',  ( -37.00000000000000711, 7.146664589318047156, -9.321877890560362090 ) ) ;
#32327 = FACE_OUTER_BOUND ( 'NONE', #9041, .T. ) ;
#32328 = CARTESIAN_POINT ( 'NONE',  ( -22.28694879868232448, -2.661377239830742258, -2.586016167700816659 ) ) ;
#32329 = B_SPLINE_CURVE_WITH_KNOTS ( 'NONE', 3,
 ( #32820, #16893, #26878, #21898, #47493, #37506, #7921, #2621, #42143, #37163, #32495, #57473, #1934, #62762, #17232, #57811, #22884, #43135, #63414 ),
 .UNSPECIFIED., .F., .F.,
 ( 4, 3, 3, 3, 3, 3, 4 ),
 ( 7.962060684260449495E-18, 4.457896483014778873E-05, 6.639290541542104728E-05, 8.820687556478873739E-05, 0.0001100173248778919230, 0.0001545671401658130781, 0.0001830328308068591189 ),
 .UNSPECIFIED. ) ;
#32330 = ADVANCED_FACE ( 'NONE', ( #17705 ), #60294, .T. ) ;
#32331 = CIRCLE ( 'NONE', #45077, 2.899999999999995914 ) ;
#32332 = VERTEX_POINT ( 'NONE', #27021 ) ;
#32333 = DIRECTION ( 'NONE',  ( -1.000000000000000000, 0.000000000000000000, 0.000000000000000000 ) ) ;
#32334 = CARTESIAN_POINT ( 'NONE',  ( 0.3218525148189843588, -12.26259572563018629, -0.2444206315274449481 ) ) ;
#32335 = VERTEX_POINT ( 'NONE', #57621 ) ;
#32336 = CARTESIAN_POINT ( 'NONE',  ( -22.27715239060371744, -3.586346956688103216, 0.8317362037004271125 ) ) ;
#32337 = DIRECTION ( 'NONE',  ( 0.000000000000000000, 0.000000000000000000, 1.000000000000000000 ) ) ;
#32338 = ORIENTED_EDGE ( 'NONE', *, *, #53392, .F. ) ;
#32339 = LINE ( 'NONE', #37331, #17172 ) ;
#32340 = ORIENTED_EDGE ( 'NONE', *, *, #52590, .F. ) ;
#32341 = ADVANCED_FACE ( 'NONE', ( #53618 ), #8059, .T. ) ;
#32342 = CARTESIAN_POINT ( 'NONE',  ( 37.00000000000000711, 0.4871980014161481631, -12.74068829017554272 ) ) ;
#32343 = ORIENTED_EDGE ( 'NONE', *, *, #42275, .T. ) ;
#32344 = ORIENTED_EDGE ( 'NONE', *, *, #50713, .F. ) ;
#32345 = ADVANCED_FACE ( 'NONE', ( #12040 ), #15895, .F. ) ;
#32346 = DIRECTION ( 'NONE',  ( 1.000000000000000000, 0.000000000000000000, -0.000000000000000000 ) ) ;
#32347 = ORIENTED_EDGE ( 'NONE', *, *, #21290, .F. ) ;
#32348 = CARTESIAN_POINT ( 'NONE',  ( -24.84395261982345104, -8.877669242773048808, 8.075961097281444623 ) ) ;
#32349 = FACE_OUTER_BOUND ( 'NONE', #10869, .T. ) ;
#32350 = DIRECTION ( 'NONE',  ( 0.000000000000000000, 0.01356324068817998940, -0.9999080150203990547 ) ) ;
#32351 = DIRECTION ( 'NONE',  ( 1.000000000000000000, 0.000000000000000000, -0.000000000000000000 ) ) ;
#32352 = ORIENTED_EDGE ( 'NONE', *, *, #1465, .T. ) ;
#32353 = CIRCLE ( 'NONE', #3740, 6.936499999999987232 ) ;
#32354 = DIRECTION ( 'NONE',  ( -1.000000000000000000, 0.000000000000000000, 0.000000000000000000 ) ) ;
#32355 = CARTESIAN_POINT ( 'NONE',  ( 3.413903065650966351, -31.27385512440588400, 14.18194743136197289 ) ) ;
#32356 = CARTESIAN_POINT ( 'NONE',  ( 2.556980015514282556, -7.736177238086868968, 0.2307166419797217205 ) ) ;
#32358 = ORIENTED_EDGE ( 'NONE', *, *, #23683, .F. ) ;
#32357 = CARTESIAN_POINT ( 'NONE',  ( 12.52750123246316249, 0.4973700281276248192, -13.49083477977253764 ) ) ;
#32359 = CARTESIAN_POINT ( 'NONE',  ( 29.51976981715666781, 4.571419055710094881, 11.09513982864076276 ) ) ;
#32360 = VERTEX_POINT ( 'NONE', #57946 ) ;
#32361 = CIRCLE ( 'NONE', #52573, 12.73084802173761787 ) ;
#32362 = DIRECTION ( 'NONE',  ( 0.000000000000000000, -0.01356324068817991828, 0.9999080150203990547 ) ) ;
#32363 = ORIENTED_EDGE ( 'NONE', *, *, #26220, .T. ) ;
#32364 = DIRECTION ( 'NONE',  ( -1.000000000000000000, 0.000000000000000000, 0.000000000000000000 ) ) ;
#32365 = DIRECTION ( 'NONE',  ( 1.000000000000000000, 0.000000000000000000, 0.000000000000000000 ) ) ;
#32366 = EDGE_CURVE ( 'NONE', #64587, #12570, #49675, .T. ) ;
#32367 = AXIS2_PLACEMENT_3D ( 'NONE', #63270, #27368, #47663 ) ;
#32368 = CARTESIAN_POINT ( 'NONE',  ( 0.3675815128205894289, -4.447030445008257615, 11.44679196252407927 ) ) ;
#32369 = ORIENTED_EDGE ( 'NONE', *, *, #36334, .F. ) ;
#32370 = DIRECTION ( 'NONE',  ( -1.000000000000000000, 0.000000000000000000, 0.000000000000000000 ) ) ;
#32371 = CARTESIAN_POINT ( 'NONE',  ( -35.04582288351658548, 0.006479247284605894018, 0.01092946910272066426 ) ) ;
#32372 = CARTESIAN_POINT ( 'NONE',  ( 35.00000000000000000, -8.699265615723042799, -8.534258022646065811 ) ) ;
#32373 = ORIENTED_EDGE ( 'NONE', *, *, #14107, .F. ) ;
#32374 = EDGE_CURVE ( 'NONE', #40614, #5549, #28485, .T. ) ;
#32375 = VERTEX_POINT ( 'NONE', #14332 ) ;
#32376 = CARTESIAN_POINT ( 'NONE',  ( 3.152665057734126197, 7.719888720907812640, 1.848755561852068130 ) ) ;
#32377 = ORIENTED_EDGE ( 'NONE', *, *, #19598, .F. ) ;
#32378 = ORIENTED_EDGE ( 'NONE', *, *, #44113, .F. ) ;
#32379 = DIRECTION ( 'NONE',  ( 1.000000000000000000, -0.000000000000000000, -0.000000000000000000 ) ) ;
#32380 = DIRECTION ( 'NONE',  ( 0.000000000000000000, 0.01356324068817998940, -0.9999080150203989437 ) ) ;
#32381 = CARTESIAN_POINT ( 'NONE',  ( 2.941278708680199916, -3.842273877444594365, 4.788765081995617123 ) ) ;
#32382 = CARTESIAN_POINT ( 'NONE',  ( 2.305787727787085295, 7.249469779319941409, -2.461236246750998724 ) ) ;
#32383 = DIRECTION ( 'NONE',  ( 0.000000000000000000, 0.01356324068817998940, -0.9999080150203989437 ) ) ;
#32384 = DIRECTION ( 'NONE',  ( 0.000000000000000000, -0.01356324068817991828, 0.9999080150203990547 ) ) ;
#32385 = CIRCLE ( 'NONE', #5887, 12.18650000000000055 ) ;
#32386 = EDGE_CURVE ( 'NONE', #10275, #22824, #56109, .T. ) ;
#32387 = CARTESIAN_POINT ( 'NONE',  ( -22.27713295444592845, -0.8543895091636509731, -3.580881989303322577 ) ) ;
#32388 = ORIENTED_EDGE ( 'NONE', *, *, #43354, .T. ) ;
#32389 = CARTESIAN_POINT ( 'NONE',  ( 2.000000000000001776, -2.480520636974139936, -6.345145617221269241 ) ) ;
#32390 = CARTESIAN_POINT ( 'NONE',  ( 5.515539859299206427, 0.002251761459665530159, -0.005618668168217195655 ) ) ;
#32391 = CARTESIAN_POINT ( 'NONE',  ( -35.04582288351658548, -0.004274985098089345917, -0.01196488372923832158 ) ) ;
#32392 = DIRECTION ( 'NONE',  ( 0.000000000000000000, 0.01356324068817998940, -0.9999080150203990547 ) ) ;
#32393 = CARTESIAN_POINT ( 'NONE',  ( 37.00000000000000711, -10.80478261802178075, 5.636262487437428526 ) ) ;
#32394 = EDGE_CURVE ( 'NONE', #35774, #37322, #47625, .T. ) ;
#32395 = AXIS2_PLACEMENT_3D ( 'NONE', #53194, #58186, #7641 ) ;
#32396 = DIRECTION ( 'NONE',  ( 0.000000000000000000, 0.07632122047555796318, -0.9970832820307045097 ) ) ;
#32397 = CARTESIAN_POINT ( 'NONE',  ( 9.949876586531372524, 1.099362317746359841, -11.95077892412715492 ) ) ;
#32398 = VERTEX_POINT ( 'NONE', #39608 ) ;
#32399 = CARTESIAN_POINT ( 'NONE',  ( 2.241352910868910531, 5.794346703933913822, -4.970878533273699773 ) ) ;
#32400 = CYLINDRICAL_SURFACE ( 'NONE', #33511, 12.18650000000000055 ) ;
#32401 = CARTESIAN_POINT ( 'NONE',  ( -25.42680463514452427, -1.651747791411766197, -3.516354806213014772 ) ) ;
#32402 = CARTESIAN_POINT ( 'NONE',  ( 6.013273758146171488, -31.75304111243247007, 13.61309608153140793 ) ) ;
#32403 = VECTOR ( 'NONE', #22982, 1000.000000000000000 ) ;
#32404 = EDGE_CURVE ( 'NONE', #2532, #59070, #56582, .T. ) ;
#32405 = DIRECTION ( 'NONE',  ( 0.000000000000000000, 0.01356324068817998940, -0.9999080150203989437 ) ) ;
#32406 = CARTESIAN_POINT ( 'NONE',  ( -27.10719052120871098, 0.5475695427849553987, -2.295785794152566339 ) ) ;
#32407 =( BOUNDED_CURVE ( )  B_SPLINE_CURVE ( 3, ( #417, #54649, #29656, #9066 ),
 .UNSPECIFIED., .F., .F. ) 
 B_SPLINE_CURVE_WITH_KNOTS ( ( 4, 4 ),
 ( 1.252925267387244856, 1.262475676102403632 ),
 .UNSPECIFIED. ) 
 CURVE ( )  GEOMETRIC_REPRESENTATION_ITEM ( )  RATIONAL_B_SPLINE_CURVE ( ( 1.000000000000000000, 0.9999923991555577096, 0.9999923991555577096, 1.000000000000000000 ) ) 
 REPRESENTATION_ITEM ( '' )  );
#32408 = EDGE_LOOP ( 'NONE', ( #32184, #13843, #43647, #1059 ) ) ;
#32409 = DIRECTION ( 'NONE',  ( 0.000000000000000000, -0.07632122047555069122, 0.9970832820307048427 ) ) ;
#32410 = FACE_OUTER_BOUND ( 'NONE', #65555, .T. ) ;
#32411 = CARTESIAN_POINT ( 'NONE',  ( -35.00000000000000000, -4.426194442447158650, -11.35427606708811155 ) ) ;
#32412 = CARTESIAN_POINT ( 'NONE',  ( -22.28506771379528573, 3.718191140878649659, -0.2569416992704126601 ) ) ;
#32413 = ORIENTED_EDGE ( 'NONE', *, *, #6237, .T. ) ;
#32414 = CARTESIAN_POINT ( 'NONE',  ( -35.00000000000000000, 10.54834585426219995, 6.102719229070713070 ) ) ;
#32415 = LINE ( 'NONE', #56388, #59567 ) ;
#32416 = EDGE_CURVE ( 'NONE', #14585, #59854, #16180, .T. ) ;
#32418 = ORIENTED_EDGE ( 'NONE', *, *, #12976, .T. ) ;
#32417 = CARTESIAN_POINT ( 'NONE',  ( 0.2648978790185602672, -12.24533305150758267, 0.1321385342561976484 ) ) ;
#32419 = CARTESIAN_POINT ( 'NONE',  ( -27.05874794189610455, 1.734723475976807094E-15, -8.673617379884035472E-15 ) ) ;
#32420 = ADVANCED_FACE ( 'NONE', ( #19677 ), #53932, .T. ) ;
#32421 = CIRCLE ( 'NONE', #21822, 12.74999999999999822 ) ;
#32422 = DIRECTION ( 'NONE',  ( -1.836970198721029688E-16, 1.000000000000000000, 0.000000000000000000 ) ) ;
#32423 = ORIENTED_EDGE ( 'NONE', *, *, #34940, .T. ) ;
#32424 = CARTESIAN_POINT ( 'NONE',  ( 0.2956976708475445581, -9.528782683728138636, 7.708404409946622238 ) ) ;
#32425 = DIRECTION ( 'NONE',  ( 1.000000000000000000, 0.000000000000000000, 0.000000000000000000 ) ) ;
#32426 = CYLINDRICAL_SURFACE ( 'NONE', #13109, 4.999999999999999112 ) ;
#32427 = CARTESIAN_POINT ( 'NONE',  ( -3.762821804695729799, -12.34140757501883989, 5.486078560323296216 ) ) ;
#32428 = DIRECTION ( 'NONE',  ( 0.000000000000000000, 0.01356324068817998940, -0.9999080150203990547 ) ) ;
#32429 = CARTESIAN_POINT ( 'NONE',  ( -10.48620311856347875, -9.720786832536937538, 9.367833439828908482 ) ) ;
#32430 = EDGE_LOOP ( 'NONE', ( #36717, #27891, #41506, #19441 ) ) ;
#32431 = LINE ( 'NONE', #57742, #52147 ) ;
#32432 = VERTEX_POINT ( 'NONE', #13356 ) ;
#32433 = CARTESIAN_POINT ( 'NONE',  ( -35.04709527796842394, 0.005220632201000108275, 0.01120703303051501232 ) ) ;
#32434 = ORIENTED_EDGE ( 'NONE', *, *, #12383, .T. ) ;
#32435 = APPLICATION_PROTOCOL_DEFINITION ( 'draft international standard', 'automotive_design', 1998, #61259 ) ;
#32436 = CARTESIAN_POINT ( 'NONE',  ( -14.29135464769095520, 7.782112657557433089, 25.00000000000000000 ) ) ;
#32437 = CARTESIAN_POINT ( 'NONE',  ( 24.82652845881425208, 8.390869743685042792, -8.578654028722157321 ) ) ;
#32438 = EDGE_CURVE ( 'NONE', #665, #48033, #57187, .T. ) ;
#32439 = CARTESIAN_POINT ( 'NONE',  ( 36.00000000000000711, -4.824807283154208370, -11.80185301892979410 ) ) ;
#32440 = CARTESIAN_POINT ( 'NONE',  ( -46.85239813472878723, -0.6216812786252554623, 9.954194587011514272 ) ) ;
#32441 = LINE ( 'NONE', #8490, #23510 ) ;
#32442 = ORIENTED_EDGE ( 'NONE', *, *, #16548, .T. ) ;
#32443 = CIRCLE ( 'NONE', #19751, 12.18650000000000055 ) ;
#32444 = DIRECTION ( 'NONE',  ( 0.000000000000000000, -0.3193015301359870550, 0.9476531711828000137 ) ) ;
#32445 = CARTESIAN_POINT ( 'NONE',  ( 1.657328813023050129, 0.7084331564875310239, -13.50016122470280244 ) ) ;
#32446 = VERTEX_POINT ( 'NONE', #54905 ) ;
#32447 = VERTEX_POINT ( 'NONE', #34291 ) ;
#32448 = CARTESIAN_POINT ( 'NONE',  ( 2.000000000000001776, 0.000000000000000000, 0.000000000000000000 ) ) ;
#32449 = VERTEX_POINT ( 'NONE', #54605 ) ;
#32450 = CARTESIAN_POINT ( 'NONE',  ( -47.00000000000000711, 0.000000000000000000, 0.000000000000000000 ) ) ;
#32451 = CARTESIAN_POINT ( 'NONE',  ( -37.00000000000000711, -11.60979404548637639, 3.704519465651264110 ) ) ;
#32452 = CARTESIAN_POINT ( 'NONE',  ( 10.10417271913525106, 1.641784628707440685, 13.40109299532181986 ) ) ;
#32453 = AXIS2_PLACEMENT_3D ( 'NONE', #19727, #30345, #40640 ) ;
#32454 = CARTESIAN_POINT ( 'NONE',  ( -27.08429572838383947, 0.9410937941434112108, -2.089332284968719922 ) ) ;
#32455 = EDGE_CURVE ( 'NONE', #41431, #34740, #36788, .T. ) ;
#32456 = CARTESIAN_POINT ( 'NONE',  ( -37.25000000000000711, -27.41745588273159839, 3.011965929904363293 ) ) ;
#32457 = DIRECTION ( 'NONE',  ( -1.000000000000000000, 0.000000000000000000, 0.000000000000000000 ) ) ;
#32458 = LINE ( 'NONE', #21177, #12112 ) ;
#32459 = ORIENTED_EDGE ( 'NONE', *, *, #55556, .F. ) ;
#32460 = CYLINDRICAL_SURFACE ( 'NONE', #52892, 7.499999999999988454 ) ;
#32461 = ORIENTED_EDGE ( 'NONE', *, *, #33394, .T. ) ;
#32462 = DIRECTION ( 'NONE',  ( -1.000000000000000000, -0.000000000000000000, -0.000000000000000000 ) ) ;
#32463 = LINE ( 'NONE', #36812, #10460 ) ;
#32464 = DIRECTION ( 'NONE',  ( 0.000000000000000000, 0.000000000000000000, -1.000000000000000000 ) ) ;
#32465 = DIRECTION ( 'NONE',  ( 0.000000000000000000, -0.6745969609292555846, -0.7381862504172050921 ) ) ;
#32466 = ORIENTED_EDGE ( 'NONE', *, *, #3500, .T. ) ;
#32467 = ORIENTED_EDGE ( 'NONE', *, *, #55409, .T. ) ;
#32468 = DIRECTION ( 'NONE',  ( 0.000000000000000000, -0.9868265225415276953, 0.1617819965527552140 ) ) ;
#32469 = EDGE_CURVE ( 'NONE', #61052, #60345, #48690, .T. ) ;
#32470 = ORIENTED_EDGE ( 'NONE', *, *, #3739, .T. ) ;
#32471 = DIRECTION ( 'NONE',  ( 0.000000000000000000, 0.000000000000000000, 1.000000000000000000 ) ) ;
#32472 = CARTESIAN_POINT ( 'NONE',  ( -28.41827485489077532, 3.509237424706437292, -11.47541949982828413 ) ) ;
#32473 = CARTESIAN_POINT ( 'NONE',  ( 0.5547464869798250930, -9.648168635481788158, -7.697709668896167479 ) ) ;
#32474 = EDGE_CURVE ( 'NONE', #42325, #60445, #44578, .T. ) ;
#32475 = CARTESIAN_POINT ( 'NONE',  ( 36.00000000000000711, 4.074242145636175039, 12.08151691381185167 ) ) ;
#32476 = ORIENTED_EDGE ( 'NONE', *, *, #11242, .T. ) ;
#32477 = CARTESIAN_POINT ( 'NONE',  ( -35.00000000000000000, -12.46157735505190978, 2.696588552979012121 ) ) ;
#32478 = LINE ( 'NONE', #57126, #15169 ) ;
#32479 = CARTESIAN_POINT ( 'NONE',  ( -22.94572469358971034, 0.4123340087948583199, -4.870584850960111289 ) ) ;
#32480 = FACE_OUTER_BOUND ( 'NONE', #41110, .T. ) ;
#32481 = EDGE_CURVE ( 'NONE', #28364, #8833, #65516, .T. ) ;
#32482 = VECTOR ( 'NONE', #32676, 1000.000000000000000 ) ;
#32483 = CARTESIAN_POINT ( 'NONE',  ( 2.297017764050093280, -0.1647869190091210967, -7.651182381906875385 ) ) ;
#32484 = DIRECTION ( 'NONE',  ( 0.000000000000000000, 0.01356324068817992001, -0.9999080150203990547 ) ) ;
#32485 = ORIENTED_EDGE ( 'NONE', *, *, #3552, .T. ) ;
#32486 = CARTESIAN_POINT ( 'NONE',  ( -12.19463663866909187, -29.31670792731519626, -5.824636309907595511 ) ) ;
#32487 = ORIENTED_EDGE ( 'NONE', *, *, #61329, .T. ) ;
#32488 = DIRECTION ( 'NONE',  ( 1.000000000000000000, -0.000000000000000000, 0.000000000000000000 ) ) ;
#32489 = LINE ( 'NONE', #58796, #33080 ) ;
#32490 = FACE_OUTER_BOUND ( 'NONE', #61798, .T. ) ;
#32491 = CARTESIAN_POINT ( 'NONE',  ( 0.9232058338315048962, 10.98407661738936980, -5.905985151448033932 ) ) ;
#32492 = CARTESIAN_POINT ( 'NONE',  ( 0.2648978790185593790, -11.55204314799266818, 4.063980959785006952 ) ) ;
#32493 = ORIENTED_EDGE ( 'NONE', *, *, #31371, .T. ) ;
#32494 = ORIENTED_EDGE ( 'NONE', *, *, #21642, .F. ) ;
#32496 = ADVANCED_FACE ( 'NONE', ( #24649 ), #58945, .T. ) ;
#32495 = CARTESIAN_POINT ( 'NONE',  ( 0.2911222467163546712, 1.916522451062537380, 12.10399882413661210 ) ) ;
#32497 = ORIENTED_EDGE ( 'NONE', *, *, #31629, .F. ) ;
#32498 = CARTESIAN_POINT ( 'NONE',  ( 3.142368856636166274, 4.338277973535410226, 11.19578891466989212 ) ) ;
#32499 = CARTESIAN_POINT ( 'NONE',  ( 0.2671309869109486645, -9.484919892054763935, -7.747281147400640222 ) ) ;
#32500 = LINE ( 'NONE', #46832, #23543 ) ;
#32501 = DIRECTION ( 'NONE',  ( 1.000000000000000000, 0.000000000000000000, 0.000000000000000000 ) ) ;
#32502 = DIRECTION ( 'NONE',  ( 1.000000000000000000, 0.000000000000000000, -0.000000000000000000 ) ) ;
#32503 = CARTESIAN_POINT ( 'NONE',  ( 2.247206125383339081, 5.774712443418709817, 4.996658593546202454 ) ) ;
#32504 = CARTESIAN_POINT ( 'NONE',  ( 20.00005080000000035, 5.400000000000000355, -1.000000000000000000 ) ) ;
#32505 = ORIENTED_EDGE ( 'NONE', *, *, #49826, .F. ) ;
#32506 = ORIENTED_EDGE ( 'NONE', *, *, #16389, .F. ) ;
#32507 = CARTESIAN_POINT ( 'NONE',  ( 0.6473888112830256114, -5.898884566269086527, 10.87693551365369693 ) ) ;
#32508 = ORIENTED_EDGE ( 'NONE', *, *, #8356, .F. ) ;
#32509 = CARTESIAN_POINT ( 'NONE',  ( 23.57534446543221307, -11.05662876997433486, -7.751112723597799459 ) ) ;
#32510 = CYLINDRICAL_SURFACE ( 'NONE', #36438, 4.285769192180103992 ) ;
#32512 = CARTESIAN_POINT ( 'NONE',  ( -22.31328051695926007, -1.671726071983958839, 3.401210163132545539 ) ) ;
#32511 = B_SPLINE_CURVE_WITH_KNOTS ( 'NONE', 3,
 ( #16546, #37129, #10543, #47141, #1593, #21866, #56102, #31178, #57431, #30821, #5599, #25869, #46156, #603, #20864, #19454, #46037, #44691, #45360, #64981, #35029, #30710 ),
 .UNSPECIFIED., .F., .F.,
 ( 4, 3, 3, 3, 3, 3, 3, 4 ),
 ( 3.157244383156457514E-18, 4.449119708436502735E-05, 6.626296329540230443E-05, 8.803456484962803995E-05, 0.0001098060367612831709, 0.0001315774408628536197, 0.0001760698110411167507, 0.0001829697163287809627 ),
 .UNSPECIFIED. ) ;
#32513 = EDGE_LOOP ( 'NONE', ( #6189, #52962, #41527, #6244 ) ) ;
#32514 = LINE ( 'NONE', #47514, #56670 ) ;
#32515 = DIRECTION ( 'NONE',  ( -1.000000000000000000, 0.000000000000000000, 0.000000000000000000 ) ) ;
#32516 = CARTESIAN_POINT ( 'NONE',  ( 2.276905613634094383, -5.031956778294427224, -5.757134111949650190 ) ) ;
#32517 = ORIENTED_EDGE ( 'NONE', *, *, #54965, .F. ) ;
#32518 = ORIENTED_EDGE ( 'NONE', *, *, #2489, .T. ) ;
#32519 = DIRECTION ( 'NONE',  ( 1.000000000000000000, -0.000000000000000000, 0.000000000000000000 ) ) ;
#32520 = ORIENTED_EDGE ( 'NONE', *, *, #21091, .F. ) ;
#32521 = ORIENTED_EDGE ( 'NONE', *, *, #9571, .F. ) ;
#32522 = CYLINDRICAL_SURFACE ( 'NONE', #58882, 4.000030059823568074 ) ;
#32523 = ORIENTED_EDGE ( 'NONE', *, *, #7728, .T. ) ;
#32524 = ORIENTED_EDGE ( 'NONE', *, *, #62909, .T. ) ;
#32525 = CARTESIAN_POINT ( 'NONE',  ( 0.2717059086739034846, 4.354191483751273850, 11.44824199474644644 ) ) ;
#32526 = CARTESIAN_POINT ( 'NONE',  ( 2.245754705088265801, 4.993005209687336077, -5.777230445738716469 ) ) ;
#32527 = EDGE_CURVE ( 'NONE', #60470, #9709, #27438, .T. ) ;
#32528 = PLANE ( 'NONE',  #53308 ) ;
#32529 = CARTESIAN_POINT ( 'NONE',  ( 0.3218525148189849694, 8.069481661595467870, -9.236582760335897646 ) ) ;
#32530 = DIRECTION ( 'NONE',  ( 1.000000000000000000, 0.000000000000000000, -0.000000000000000000 ) ) ;
#32531 = AXIS2_PLACEMENT_3D ( 'NONE', #17405, #23715, #43982 ) ;
#32532 = DIRECTION ( 'NONE',  ( 0.000000000000000000, -0.01356324068817998940, 0.9999080150203990547 ) ) ;
#32533 = ORIENTED_EDGE ( 'NONE', *, *, #18549, .T. ) ;
#32534 = DIRECTION ( 'NONE',  ( -1.000000000000000000, 0.000000000000000000, 0.000000000000000000 ) ) ;
#32535 = DIRECTION ( 'NONE',  ( 1.000000000000000000, -0.000000000000000000, 0.000000000000000000 ) ) ;
#32536 = CARTESIAN_POINT ( 'NONE',  ( 5.514624014163232779, -0.0008859786816847168602, -0.004045310349816150751 ) ) ;
#32537 = CARTESIAN_POINT ( 'NONE',  ( 0.3278977287071214719, -2.374069413450224708, 12.03512402322222385 ) ) ;
#32538 = FACE_OUTER_BOUND ( 'NONE', #54800, .T. ) ;
#32539 = CARTESIAN_POINT ( 'NONE',  ( 0.2872850955227752023, -11.58431228138436886, -3.994021792079210709 ) ) ;
#32540 = B_SPLINE_CURVE_WITH_KNOTS ( 'NONE', 3,
 ( #59818, #53853, #3323, #64456, #29531, #14556, #24895, #54172, #49835, #39188, #43865, #4284, #28899, #49209, #34834, #3665 ),
 .UNSPECIFIED., .F., .F.,
 ( 4, 3, 3, 3, 3, 4 ),
 ( 2.740913356018627282E-15, 0.0002126834539179616455, 0.0004253519300366086805, 0.0006380165497223901517, 0.0007442707582427936404, 0.0009453531351420096842 ),
 .UNSPECIFIED. ) ;
#32541 = EDGE_CURVE ( 'NONE', #47095, #36349, #46539, .T. ) ;
#32542 = ORIENTED_EDGE ( 'NONE', *, *, #62315, .F. ) ;
#32543 = FACE_OUTER_BOUND ( 'NONE', #11824, .T. ) ;
#32544 = ORIENTED_EDGE ( 'NONE', *, *, #54484, .T. ) ;
#32545 = EDGE_CURVE ( 'NONE', #17057, #36493, #2675, .T. ) ;
#32546 = CARTESIAN_POINT ( 'NONE',  ( 0.000000000000000000, 3.937687286050910895, -6.383151168292444666 ) ) ;
#32547 = CARTESIAN_POINT ( 'NONE',  ( -37.00000000000000711, -3.287724142101498437, 11.73463472867575064 ) ) ;
#32548 = DIRECTION ( 'NONE',  ( -1.000000000000000000, -0.000000000000000000, -0.000000000000000000 ) ) ;
#32549 = CARTESIAN_POINT ( 'NONE',  ( -27.09833916700227263, -0.6583442518269214672, -2.238843247505190259 ) ) ;
#32550 = EDGE_CURVE ( 'NONE', #14116, #15285, #34827, .T. ) ;
#32551 = DIRECTION ( 'NONE',  ( 0.000000000000000000, -0.01356324068817998940, 0.9999080150203990547 ) ) ;
#32552 = ORIENTED_EDGE ( 'NONE', *, *, #55172, .T. ) ;
#32553 = CARTESIAN_POINT ( 'NONE',  ( -19.56743653832047514, -28.99999999999999645, 5.000000000000000888 ) ) ;
#32554 = DIRECTION ( 'NONE',  ( -1.000000000000000000, 0.000000000000000000, 0.000000000000000000 ) ) ;
#32555 = CARTESIAN_POINT ( 'NONE',  ( 0.000000000000000000, -2.315790869867103474, 7.133520354428079635 ) ) ;
#32556 = CARTESIAN_POINT ( 'NONE',  ( -35.00000000000000000, 7.817492529713985228, -9.348667969174325520 ) ) ;
#32557 = EDGE_CURVE ( 'NONE', #18517, #27530, #21085, .T. ) ;
#32558 = DIRECTION ( 'NONE',  ( -1.000000000000000000, 0.000000000000000000, 0.000000000000000000 ) ) ;
#32559 = ORIENTED_EDGE ( 'NONE', *, *, #30030, .F. ) ;
#32560 = EDGE_CURVE ( 'NONE', #7338, #28155, #50908, .T. ) ;
#32561 = PRODUCT_DEFINITION_CONTEXT ( 'detailed design', #17072, 'design' ) ;
#32562 = CARTESIAN_POINT ( 'NONE',  ( 1.948354844646613238, -5.347695345043367965, 10.70340528295498927 ) ) ;
#32563 = DIRECTION ( 'NONE',  ( -0.000000000000000000, -0.000000000000000000, -1.000000000000000000 ) ) ;
#32564 = AXIS2_PLACEMENT_3D ( 'NONE', #16522, #57086, #51462 ) ;
#32565 = B_SPLINE_CURVE_WITH_KNOTS ( 'NONE', 3,
 ( #55756, #10187, #30468, #870, #11182, #564, #61706, #16164, #47425, #20827, #57066, #11494, #61069, #1861, #6201, #21141, #56398, #31765 ),
 .UNSPECIFIED., .F., .F.,
 ( 4, 2, 2, 2, 2, 2, 2, 2, 4 ),
 ( 4.336808689942017736E-18, 0.001081547705042592211, 0.002163095410085180085, 0.003244643115127768176, 0.004326190820170354966, 0.005407738525212942189, 0.006489286230255530280, 0.007570833935298119238, 0.008652381640340704727 ),
 .UNSPECIFIED. ) ;
#32566 = AXIS2_PLACEMENT_3D ( 'NONE', #28598, #32274, #57906 ) ;
#32567 = ORIENTED_EDGE ( 'NONE', *, *, #57357, .T. ) ;
#32569 = ADVANCED_FACE ( 'NONE', ( #20309 ), #25973, .T. ) ;
#32568 = DIRECTION ( 'NONE',  ( 0.000000000000000000, -0.01356324068817992175, 0.9999080150203990547 ) ) ;
#32570 = VERTEX_POINT ( 'NONE', #40929 ) ;
#32571 = CARTESIAN_POINT ( 'NONE',  ( 12.52750123246316249, 0.4973700281276248192, -13.49083477977253764 ) ) ;
#32572 = CARTESIAN_POINT ( 'NONE',  ( 2.373367633546870969, -3.681545031436607385, -6.738274194514252358 ) ) ;
#32573 = FACE_OUTER_BOUND ( 'NONE', #63290, .T. ) ;
#32574 = CARTESIAN_POINT ( 'NONE',  ( -29.43980975494970309, -3.641506875706030488, 12.99959336572439561 ) ) ;
#32575 = EDGE_CURVE ( 'NONE', #41887, #41521, #34435, .T. ) ;
#32576 = FACE_OUTER_BOUND ( 'NONE', #42641, .T. ) ;
#32577 = VERTEX_POINT ( 'NONE', #56556 ) ;
#32578 = EDGE_LOOP ( 'NONE', ( #13623, #3058, #47368, #38055 ) ) ;
#32579 = ORIENTED_EDGE ( 'NONE', *, *, #52349, .T. ) ;
#32580 = CARTESIAN_POINT ( 'NONE',  ( 2.241352910868908754, -4.843133558968167662, 5.901537464758438212 ) ) ;
#32581 = CARTESIAN_POINT ( 'NONE',  ( 0.000000000000000000, -2.469490258309361419, -6.482025155313371201 ) ) ;
#32582 = VERTEX_POINT ( 'NONE', #26289 ) ;
#32583 = DIRECTION ( 'NONE',  ( 0.000000000000000000, 0.000000000000000000, 1.000000000000000000 ) ) ;
#32584 = DIRECTION ( 'NONE',  ( -1.000000000000000000, 0.000000000000000000, 0.000000000000000000 ) ) ;
#32585 = ORIENTED_EDGE ( 'NONE', *, *, #669, .F. ) ;
#32586 =( BOUNDED_SURFACE ( )  B_SPLINE_SURFACE ( 3, 1, ( 
 ( #45411, #36427 ),
 ( #30448, #55738 ),
 ( #61354, #9838 ),
 ( #26444, #30129 ) ),
 .UNSPECIFIED., .F., .F., .F. ) 
 B_SPLINE_SURFACE_WITH_KNOTS ( ( 4, 4 ),
 ( 2, 2 ),
 ( 0.000000000000000000, 1.000000000000000000 ),
 ( 0.000000000000000000, 1.000000000000000000 ),
 .UNSPECIFIED. ) 
 GEOMETRIC_REPRESENTATION_ITEM ( )  RATIONAL_B_SPLINE_SURFACE ( (
 ( 1.000000000000000000, 1.000000000000000000),
 ( 0.6933888150995267674, 0.9895912004443193632),
 ( 0.6933888150995267674, 0.9895912004443193632),
 ( 1.000000000000000000, 1.000000000000000000) ) ) 
 REPRESENTATION_ITEM ( '' )  SURFACE ( )  );
#32587 = DIRECTION ( 'NONE',  ( 1.000000000000000000, 0.000000000000000000, 0.000000000000000000 ) ) ;
#32588 = DIRECTION ( 'NONE',  ( -0.9688695217174486674, 0.000000000000000000, -0.2475719085175094036 ) ) ;
#32589 = CARTESIAN_POINT ( 'NONE',  ( 2.259830038566063681, 7.131511317046705045, 2.742210045660591788 ) ) ;
#32590 = EDGE_CURVE ( 'NONE', #60004, #12123, #54955, .T. ) ;
#32591 = ORIENTED_EDGE ( 'NONE', *, *, #57622, .T. ) ;
#32592 = ORIENTED_EDGE ( 'NONE', *, *, #52298, .F. ) ;
#32593 = DIRECTION ( 'NONE',  ( 0.000000000000000000, -0.01356324068817991828, 0.9999080150203990547 ) ) ;
#32594 = ORIENTED_EDGE ( 'NONE', *, *, #31461, .T. ) ;
#32595 = CARTESIAN_POINT ( 'NONE',  ( 9.960423179593171028, 1.090233323514599340, -13.45698435061968290 ) ) ;
#32596 = ORIENTED_EDGE ( 'NONE', *, *, #59320, .F. ) ;
#32597 = CARTESIAN_POINT ( 'NONE',  ( 0.2651627682582944345, -4.105539787731786738, 11.53745347823613443 ) ) ;
#32598 = CARTESIAN_POINT ( 'NONE',  ( 2.990245332647833099, -2.413832934171117550, -8.130497889782899890 ) ) ;
#32599 = CARTESIAN_POINT ( 'NONE',  ( 35.00000000000000000, -11.53507381115584529, -2.216820770815045805 ) ) ;
#32600 = EDGE_CURVE ( 'NONE', #55701, #14200, #51582, .T. ) ;
#32601 = CARTESIAN_POINT ( 'NONE',  ( -47.00000000000000711, 0.000000000000000000, 0.000000000000000000 ) ) ;
#32602 = CARTESIAN_POINT ( 'NONE',  ( 8.553317268354581060, 3.425949070068618152, 11.50390082272593162 ) ) ;
#32603 = DIRECTION ( 'NONE',  ( 0.000000000000000000, 0.000000000000000000, 1.000000000000000000 ) ) ;
#32604 = DIRECTION ( 'NONE',  ( 0.000000000000000000, -0.2006870767258961963, 0.9796553971857727694 ) ) ;
#32605 = ORIENTED_EDGE ( 'NONE', *, *, #9674, .T. ) ;
#32606 = DIRECTION ( 'NONE',  ( -1.000000000000000000, -1.836970198721029688E-16, -0.000000000000000000 ) ) ;
#32607 = ORIENTED_EDGE ( 'NONE', *, *, #56614, .T. ) ;
#32608 = CARTESIAN_POINT ( 'NONE',  ( 0.2956976708475410054, -4.397965666276502539, 11.44006538352184954 ) ) ;
#32609 = CARTESIAN_POINT ( 'NONE',  ( 2.256373768221665355, 6.681391662619836858, 3.703993494729489910 ) ) ;
#32610 = EDGE_LOOP ( 'NONE', ( #46399, #59557, #53502, #33800 ) ) ;
#32611 = EDGE_CURVE ( 'NONE', #49577, #55976, #6200, .T. ) ;
#32612 = CARTESIAN_POINT ( 'NONE',  ( 2.653899356900242701, 7.388433688587512371, 2.411250235128028940 ) ) ;
#32613 = CARTESIAN_POINT ( 'NONE',  ( 0.3223008802179240240, 12.03398982086836710, -2.370176598416207092 ) ) ;
#32614 = CIRCLE ( 'NONE', #12442, 12.18650000000000055 ) ;
#32615 = ORIENTED_EDGE ( 'NONE', *, *, #26682, .T. ) ;
#32616 = EDGE_CURVE ( 'NONE', #60341, #30241, #35918, .T. ) ;
#32617 = ORIENTED_EDGE ( 'NONE', *, *, #4440, .T. ) ;
#32618 = CIRCLE ( 'NONE', #35796, 12.18650000000000411 ) ;
#32619 = DIRECTION ( 'NONE',  ( 0.000000000000000000, -0.5243256840888443904, -0.8515178078024941977 ) ) ;
#32620 = VERTEX_POINT ( 'NONE', #32556 ) ;
#32621 = CARTESIAN_POINT ( 'NONE',  ( -35.00000000000000000, 0.000000000000000000, 0.000000000000000000 ) ) ;
#32622 = DIRECTION ( 'NONE',  ( -1.000000000000000000, 0.000000000000000000, 0.000000000000000000 ) ) ;
#32623 = DIRECTION ( 'NONE',  ( -1.000000000000000000, 0.000000000000000000, 0.000000000000000000 ) ) ;
#32624 = EDGE_CURVE ( 'NONE', #26538, #44286, #22550, .T. ) ;
#32625 = CARTESIAN_POINT ( 'NONE',  ( -18.51055391882387369, -5.103712865905460916, 10.86121933613184787 ) ) ;
#32626 = ORIENTED_EDGE ( 'NONE', *, *, #61217, .F. ) ;
#32627 = CARTESIAN_POINT ( 'NONE',  ( -35.00000000000000000, 8.766823244862097297, -7.817610399097422835 ) ) ;
#32628 = CARTESIAN_POINT ( 'NONE',  ( 7.964047368509766578, -27.27321649430781392, -15.08844977892397665 ) ) ;
#32629 = CARTESIAN_POINT ( 'NONE',  ( 0.000000000000000000, 0.000000000000000000, 0.000000000000000000 ) ) ;
#32630 = ADVANCED_FACE ( 'NONE', ( #21957 ), #2000, .T. ) ;
#32631 = CYLINDRICAL_SURFACE ( 'NONE', #45805, 5.000000000000000888 ) ;
#32632 = CARTESIAN_POINT ( 'NONE',  ( -27.08426504710140392, -0.6326154899769325102, 2.202478235133275231 ) ) ;
#32633 = EDGE_CURVE ( 'NONE', #19473, #52495, #19995, .T. ) ;
#32634 = CARTESIAN_POINT ( 'NONE',  ( 37.00000000000000711, -12.21925492305364713, -3.640372113593511649 ) ) ;
#32635 = DIRECTION ( 'NONE',  ( -1.000000000000000000, 0.000000000000000000, 0.000000000000000000 ) ) ;
#32636 = CARTESIAN_POINT ( 'NONE',  ( 3.047904605210412399, 5.398304302092612694, -5.772373816836767091 ) ) ;
#32637 = EDGE_CURVE ( 'NONE', #26131, #16803, #25723, .T. ) ;
#32638 = ORIENTED_EDGE ( 'NONE', *, *, #10086, .T. ) ;
#32639 = EDGE_CURVE ( 'NONE', #38939, #38736, #65640, .T. ) ;
#32640 = DIRECTION ( 'NONE',  ( 0.000000000000000000, -0.9105187689795999351, 0.4134677391718417638 ) ) ;
#32641 = CARTESIAN_POINT ( 'NONE',  ( 5.412955401783937859, -9.519507165005897775, 9.576690525650159103 ) ) ;
#32642 = VECTOR ( 'NONE', #52844, 1000.000000000000000 ) ;
#32643 = ORIENTED_EDGE ( 'NONE', *, *, #40381, .T. ) ;
#32644 = CARTESIAN_POINT ( 'NONE',  ( -22.31213670151049300, 3.777944311993714166, -0.2530575063955878279 ) ) ;
#32645 = CARTESIAN_POINT ( 'NONE',  ( -22.71097035706202405, 4.089776368546564456, 2.846599994298306679 ) ) ;
#32646 = ORIENTED_EDGE ( 'NONE', *, *, #264, .T. ) ;
#32647 = EDGE_CURVE ( 'NONE', #45854, #52466, #37627, .T. ) ;
#32648 = CARTESIAN_POINT ( 'NONE',  ( -3.740102306720532788, 25.00000000000000000, -6.044082642436763742 ) ) ;
#32649 = VERTEX_POINT ( 'NONE', #65121 ) ;
#32650 = DIRECTION ( 'NONE',  ( 1.000000000000000000, -0.000000000000000000, 0.000000000000000000 ) ) ;
#32651 = ORIENTED_EDGE ( 'NONE', *, *, #49546, .F. ) ;
#32652 = CIRCLE ( 'NONE', #880, 5.000000000000000000 ) ;
#32653 = ORIENTED_EDGE ( 'NONE', *, *, #50916, .T. ) ;
#32654 = CARTESIAN_POINT ( 'NONE',  ( 2.000000000000001776, 5.585096664091999230, -4.113602740025892324 ) ) ;
#32655 = CIRCLE ( 'NONE', #6170, 5.000000000000000000 ) ;
#32656 = ORIENTED_EDGE ( 'NONE', *, *, #14540, .T. ) ;
#32657 = CYLINDRICAL_SURFACE ( 'NONE', #1575, 12.75000000000000178 ) ;
#32658 = FACE_OUTER_BOUND ( 'NONE', #55691, .T. ) ;
#32659 = FACE_OUTER_BOUND ( 'NONE', #7392, .T. ) ;
#32660 = DIRECTION ( 'NONE',  ( 0.000000000000000000, 0.2960891610144510966, 0.9551603052523479631 ) ) ;
#32661 = VERTEX_POINT ( 'NONE', #49841 ) ;
#32662 = CARTESIAN_POINT ( 'NONE',  ( 37.00000000000000711, -11.32068061209299259, -5.865551165831043079 ) ) ;
#32663 = CARTESIAN_POINT ( 'NONE',  ( 12.69762816655162574, -29.19309327991231839, 4.289906119467950418 ) ) ;
#32664 = CARTESIAN_POINT ( 'NONE',  ( 2.524535260912988743, -7.725637239510562360, 0.2211075636761446472 ) ) ;
#32666 = EDGE_LOOP ( 'NONE', ( #48783, #54561, #63204, #3787 ) ) ;
#32665 = DIRECTION ( 'NONE',  ( -1.000000000000000000, -0.000000000000000000, -0.000000000000000000 ) ) ;
#32667 = CARTESIAN_POINT ( 'NONE',  ( 1.937114397841932290, -12.33981801388260457, 3.531416430611253876 ) ) ;
#32668 = ORIENTED_EDGE ( 'NONE', *, *, #6962, .T. ) ;
#32669 = CARTESIAN_POINT ( 'NONE',  ( 5.514970785353741078, 0.0003039746380524305930, -0.004713149585127262425 ) ) ;
#32670 = ORIENTED_EDGE ( 'NONE', *, *, #25219, .F. ) ;
#32671 = DIRECTION ( 'NONE',  ( -1.000000000000000000, 0.000000000000000000, 0.000000000000000000 ) ) ;
#32672 = CARTESIAN_POINT ( 'NONE',  ( 0.000000000000000000, 4.915517050588478654, -4.717154614762057108 ) ) ;
#32673 = CARTESIAN_POINT ( 'NONE',  ( -35.00000000000000000, -15.00000000000000000, 0.000000000000000000 ) ) ;
#32675 = ADVANCED_FACE ( 'NONE', ( #38555 ), #44500, .T. ) ;
#32674 = ORIENTED_EDGE ( 'NONE', *, *, #39320, .T. ) ;
#32676 = DIRECTION ( 'NONE',  ( -1.000000000000000000, -0.000000000000000000, 0.000000000000000000 ) ) ;
#32677 = DIRECTION ( 'NONE',  ( 1.000000000000000000, 0.000000000000000000, 0.000000000000000000 ) ) ;
#32678 = CARTESIAN_POINT ( 'NONE',  ( 13.33580375564548781, 12.01919014649627293, -6.162572361761344375 ) ) ;
#32679 = EDGE_LOOP ( 'NONE', ( #479, #37264, #44613, #49543 ) ) ;
#32680 = ORIENTED_EDGE ( 'NONE', *, *, #10421, .F. ) ;
#32681 = CARTESIAN_POINT ( 'NONE',  ( 0.2869720083484339490, 12.02930764912520978, 2.332746648244237608 ) ) ;
#32682 = ORIENTED_EDGE ( 'NONE', *, *, #41142, .T. ) ;
#32683 = B_SPLINE_CURVE_WITH_KNOTS ( 'NONE', 3,
 ( #18590, #59139, #62787, #57834, #32516, #9213, #28859, #64736, #33834, #40458, #54135, #59446, #13867, #29498, #29195, #14208, #14520, #49170, #34495 ),
 .UNSPECIFIED., .F., .F.,
 ( 4, 3, 3, 3, 3, 3, 4 ),
 ( 6.209365080825174961E-18, 2.825908398782148371E-05, 4.208813692417141740E-05, 5.591713746859297335E-05, 6.279584083138583855E-05, 9.105792820165378189E-05, 0.0001153131102489443041 ),
 .UNSPECIFIED. ) ;
#32684 = EDGE_LOOP ( 'NONE', ( #62964, #48399, #64178, #47924 ) ) ;
#32685 = EDGE_CURVE ( 'NONE', #50474, #12842, #31658, .T. ) ;
#32686 = CARTESIAN_POINT ( 'NONE',  ( 47.00000000000000711, 4.705694406421931860E-17, -3.469127814946512892E-15 ) ) ;
#32687 = CARTESIAN_POINT ( 'NONE',  ( -22.27706485742869091, 3.358064672837120401, 1.508175983031588840 ) ) ;
#32688 = B_SPLINE_CURVE_WITH_KNOTS ( 'NONE', 3,
 ( #44507, #64787, #39533, #63757, #3929, #64418, #33528, #59444, #7944, #23555, #44456, #58477, #63436, #23890, #58827, #8252, #59138, #53816, #13551 ),
 .UNSPECIFIED., .F., .F.,
 ( 4, 3, 3, 3, 3, 3, 4 ),
 ( 6.209365080825174961E-18, 2.825908398831632713E-05, 4.208813692484372439E-05, 5.591713746944466836E-05, 6.279584083232523197E-05, 9.105792820297400132E-05, 0.0001153131102488854861 ),
 .UNSPECIFIED. ) ;
#32689 = CARTESIAN_POINT ( 'NONE',  ( 2.241451721903215066, -7.153019588493058301, -2.668222118333522186 ) ) ;
#32690 = CYLINDRICAL_SURFACE ( 'NONE', #52260, 12.75000000000000178 ) ;
#32691 = CARTESIAN_POINT ( 'NONE',  ( 37.00000000000000711, 12.09831040184923978, -1.463443770872822736 ) ) ;
#32692 = AXIS2_PLACEMENT_3D ( 'NONE', #5317, #19303, #25591 ) ;
#32693 = DIRECTION ( 'NONE',  ( -1.000000000000000000, -0.000000000000000000, 0.000000000000000000 ) ) ;
#32694 = DIRECTION ( 'NONE',  ( 1.000000000000000000, 0.000000000000000000, 0.000000000000000000 ) ) ;
#32695 = VECTOR ( 'NONE', #41676, 1000.000000000000000 ) ;
#32696 = ORIENTED_EDGE ( 'NONE', *, *, #26179, .T. ) ;
#32697 = CARTESIAN_POINT ( 'NONE',  ( 35.00000000000000000, -11.47758908105696207, -2.497432891016804657 ) ) ;
#32698 = AXIS2_PLACEMENT_3D ( 'NONE', #31408, #52685, #7112 ) ;
#32699 = CARTESIAN_POINT ( 'NONE',  ( -22.29290468048228036, -3.083035815361902188, 2.097193667172386977 ) ) ;
#32700 = ADVANCED_FACE ( 'NONE', ( #39525 ), #44194, .T. ) ;
#32701 = VECTOR ( 'NONE', #39997, 1000.000000000000000 ) ;
#32702 = EDGE_CURVE ( 'NONE', #39567, #55842, #50808, .T. ) ;
#32703 = DIRECTION ( 'NONE',  ( 0.000000000000000000, -0.01356324068817999114, 0.9999080150203989437 ) ) ;
#32704 = LINE ( 'NONE', #58020, #18478 ) ;
#32705 = DIRECTION ( 'NONE',  ( 0.000000000000000000, 0.4198891015602590482, 0.9075754196709595600 ) ) ;
#32706 = CARTESIAN_POINT ( 'NONE',  ( -37.00000000000000711, 12.74068829017554094, 0.4871980014161925165 ) ) ;
#32707 = CARTESIAN_POINT ( 'NONE',  ( 2.241352910868909643, 7.532448145350525870, -1.243507963608017075 ) ) ;
#32708 = B_SPLINE_CURVE_WITH_KNOTS ( 'NONE', 3,
 ( #37276, #52275, #42929, #47927, #7690, #27975, #7028, #63209, #8031, #17991, #12334, #7340, #11675, #28298, #62876, #38253, #6716, #12649, #47285, #32933, #48283, #27625, #22990, #1725 ),
 .UNSPECIFIED., .F., .F.,
 ( 4, 2, 2, 2, 2, 2, 2, 2, 2, 2, 2, 4 ),
 ( 0.02095799966194190206, 0.02357897855711225260, 0.02619995745228260314, 0.02882093634745295369, 0.03013142579503812896, 0.03144191524262329729, 0.03406289413779364783, 0.03668387303296398450, 0.03799436248054915977, 0.03930485192813433504, 0.04061534137571949643, 0.04192583082330467170 ),
 .UNSPECIFIED. ) ;
#32709 = VERTEX_POINT ( 'NONE', #34537 ) ;
#32710 = DIRECTION ( 'NONE',  ( 0.3865475372811021382, 0.8082200352954648226, -0.4442537292684356487 ) ) ;
#32711 = DIRECTION ( 'NONE',  ( -1.000000000000000000, -1.836970198721029688E-16, -0.000000000000000000 ) ) ;
#32712 = CARTESIAN_POINT ( 'NONE',  ( 2.589278595513889059, -1.582391164331770295, -7.587119248534476057 ) ) ;
#32713 = EDGE_CURVE ( 'NONE', #8677, #24896, #12168, .T. ) ;
#32714 = AXIS2_PLACEMENT_3D ( 'NONE', #26502, #5931, #11533 ) ;
#32715 = EDGE_CURVE ( 'NONE', #59063, #9280, #7449, .T. ) ;
#32716 = DIRECTION ( 'NONE',  ( 0.000000000000000000, -0.01356324068817998940, 0.9999080150203990547 ) ) ;
#32717 = CARTESIAN_POINT ( 'NONE',  ( -26.63135098142518942, -12.18341857921932458, 5.815336232052954912 ) ) ;
#32718 = ORIENTED_EDGE ( 'NONE', *, *, #45335, .T. ) ;
#32719 = CIRCLE ( 'NONE', #28471, 4.999999999999999112 ) ;
#32720 = CARTESIAN_POINT ( 'NONE',  ( 19.08051869631892572, -3.535630671987933127, 11.50449325566757075 ) ) ;
#32721 = CARTESIAN_POINT ( 'NONE',  ( 0.000000000000000000, -6.812627895098285258, 2.855765430652664971 ) ) ;
#32722 = DIRECTION ( 'NONE',  ( 0.000000000000000000, 0.9903235168508544017, 0.1387779952735853917 ) ) ;
#32723 = CARTESIAN_POINT ( 'NONE',  ( 0.5547464869798239828, -12.20441397277156170, -1.842327806480273500 ) ) ;
#32724 = VERTEX_POINT ( 'NONE', #36155 ) ;
#32725 = ADVANCED_FACE ( 'NONE', ( #19903 ), #14882, .T. ) ;
#32726 = DIRECTION ( 'NONE',  ( -0.000000000000000000, -0.000000000000000000, 1.000000000000000000 ) ) ;
#32727 = DIRECTION ( 'NONE',  ( 1.000000000000000000, 0.000000000000000000, 0.000000000000000000 ) ) ;
#32728 = ORIENTED_EDGE ( 'NONE', *, *, #11782, .F. ) ;
#32729 = VERTEX_POINT ( 'NONE', #5618 ) ;
#32730 = DIRECTION ( 'NONE',  ( -1.000000000000000000, -0.000000000000000000, 0.000000000000000000 ) ) ;
#32731 = AXIS2_PLACEMENT_3D ( 'NONE', #22588, #42852, #10970 ) ;
#32732 = EDGE_CURVE ( 'NONE', #60151, #46959, #1104, .T. ) ;
#32733 = DIRECTION ( 'NONE',  ( -1.000000000000000000, 0.000000000000000000, 0.000000000000000000 ) ) ;
#32734 = ORIENTED_EDGE ( 'NONE', *, *, #49756, .T. ) ;
#32735 = DIRECTION ( 'NONE',  ( 0.000000000000000000, 0.01356324068817298112, -0.9999080150203990547 ) ) ;
#32736 = FACE_OUTER_BOUND ( 'NONE', #950, .T. ) ;
#32737 = DIRECTION ( 'NONE',  ( 0.000000000000000000, 0.000000000000000000, 1.000000000000000000 ) ) ;
#32738 = AXIS2_PLACEMENT_3D ( 'NONE', #38333, #28052, #29032 ) ;
#32739 = CARTESIAN_POINT ( 'NONE',  ( -10.48620311856347875, -9.720786832536937538, 25.00000000000000000 ) ) ;
#32740 = DIRECTION ( 'NONE',  ( 0.000000000000000000, -0.01356324068817992175, 0.9999080150203990547 ) ) ;
#32741 = FACE_OUTER_BOUND ( 'NONE', #36184, .T. ) ;
#32743 = VERTEX_POINT ( 'NONE', #60800 ) ;
#32742 = CARTESIAN_POINT ( 'NONE',  ( -28.67667724226168602, 1.840944188131424131, 0.4371157725389773208 ) ) ;
#32744 = VECTOR ( 'NONE', #27988, 1000.000000000000000 ) ;
#32745 = DIRECTION ( 'NONE',  ( -1.000000000000000000, 0.000000000000000000, -0.000000000000000000 ) ) ;
#32746 = VERTEX_POINT ( 'NONE', #11239 ) ;
#32747 = CARTESIAN_POINT ( 'NONE',  ( -2.532614230583026593, -5.020478806276874373, 10.89930238848911337 ) ) ;
#32748 = ORIENTED_EDGE ( 'NONE', *, *, #46396, .F. ) ;
#32749 = AXIS2_PLACEMENT_3D ( 'NONE', #44397, #58766, #8509 ) ;
#32750 = VERTEX_POINT ( 'NONE', #4638 ) ;
#32751 = SHAPE_DEFINITION_REPRESENTATION ( #22274, #45039 ) ;
#32752 = CARTESIAN_POINT ( 'NONE',  ( -10.00000000000000178, 0.000000000000000000, 0.000000000000000000 ) ) ;
#32753 = CARTESIAN_POINT ( 'NONE',  ( -13.40508024068858894, -30.08919203116835206, 6.920461462857061541 ) ) ;
#32754 = CARTESIAN_POINT ( 'NONE',  ( 5.530133899448235191, -0.01111090067015115673, -0.01149180883054598014 ) ) ;
#32755 = CARTESIAN_POINT ( 'NONE',  ( -48.84659035979349540, -0.2326159177122989752, -2.738175293146146050 ) ) ;
#32756 = CARTESIAN_POINT ( 'NONE',  ( 35.00000000000000000, -4.426194442447322075, -11.35427606708804937 ) ) ;
#32757 = ORIENTED_EDGE ( 'NONE', *, *, #24265, .F. ) ;
#32758 = EDGE_CURVE ( 'NONE', #7851, #33347, #19371, .T. ) ;
#32759 = CARTESIAN_POINT ( 'NONE',  ( -22.27722019117889474, -0.6494988092404023750, -3.623917154020615428 ) ) ;
#32760 = CARTESIAN_POINT ( 'NONE',  ( -22.71097035706202405, -4.510116093748277599, 2.118550233809401107 ) ) ;
#32762 = EDGE_LOOP ( 'NONE', ( #58305, #18246, #2635, #50442 ) ) ;
#32761 = LINE ( 'NONE', #2559, #17819 ) ;
#32763 = ORIENTED_EDGE ( 'NONE', *, *, #19890, .T. ) ;
#32764 = DIRECTION ( 'NONE',  ( 1.000000000000000000, 0.000000000000000000, 0.000000000000000000 ) ) ;
#32765 = ORIENTED_EDGE ( 'NONE', *, *, #9834, .F. ) ;
#32766 = CARTESIAN_POINT ( 'NONE',  ( -37.00000000000000711, -1.463443770872689953, -12.09831040184925754 ) ) ;
#32767 = CARTESIAN_POINT ( 'NONE',  ( 0.2638984909335716500, 5.950360275955056011, 10.70468911391666644 ) ) ;
#32768 = CARTESIAN_POINT ( 'NONE',  ( 35.00000000000000000, -0.4353888892049205261, -11.73808581813437968 ) ) ;
#32769 = CARTESIAN_POINT ( 'NONE',  ( 17.27839441901508621, -12.20388373500082224, 5.771933972472480967 ) ) ;
#32770 = CARTESIAN_POINT ( 'NONE',  ( 5.530133899448235191, -0.01459891979722814301, -0.006510401266731771081 ) ) ;
#32771 = DIRECTION ( 'NONE',  ( 1.000000000000000000, 0.000000000000000000, 0.000000000000000000 ) ) ;
#32772 = AXIS2_PLACEMENT_3D ( 'NONE', #57614, #36969, #22015 ) ;
#32773 = CARTESIAN_POINT ( 'NONE',  ( 2.290907136833251645, 3.965134647955987024, -6.543263131934253352 ) ) ;
#32774 = ORIENTED_EDGE ( 'NONE', *, *, #9103, .F. ) ;
#32775 = CYLINDRICAL_SURFACE ( 'NONE', #13580, 12.75000000000000178 ) ;
#32776 = VECTOR ( 'NONE', #5844, 1000.000000000000000 ) ;
#32777 = EDGE_LOOP ( 'NONE', ( #63434, #56846, #15118, #40090 ) ) ;
#32778 = CARTESIAN_POINT ( 'NONE',  ( 2.931247277082688285, 4.248542803114433219, -6.618030015945689293 ) ) ;
#32779 = EDGE_CURVE ( 'NONE', #25087, #14103, #25309, .T. ) ;
#32780 = CARTESIAN_POINT ( 'NONE',  ( -7.181456785175555524, -8.540743096806455270, -10.45493698471458188 ) ) ;
#32781 = ADVANCED_FACE ( 'NONE', ( #61432 ), #45175, .T. ) ;
#32782 = CARTESIAN_POINT ( 'NONE',  ( 0.000000000000000000, 0.000000000000000000, 0.000000000000000000 ) ) ;
#32783 = CARTESIAN_POINT ( 'NONE',  ( 3.152665057735396736, -5.761241965768377327, 5.461013642406604696 ) ) ;
#32784 = CIRCLE ( 'NONE', #50909, 5.000000000000000000 ) ;
#32785 = EDGE_CURVE ( 'NONE', #19909, #24505, #20880, .T. ) ;
#32786 = VECTOR ( 'NONE', #13057, 1000.000000000000000 ) ;
#32787 = ORIENTED_EDGE ( 'NONE', *, *, #12029, .T. ) ;
#32788 = ORIENTED_EDGE ( 'NONE', *, *, #32803, .F. ) ;
#32789 = CYLINDRICAL_SURFACE ( 'NONE', #8926, 5.000000000000002665 ) ;
#32790 =( BOUNDED_CURVE ( )  B_SPLINE_CURVE ( 3, ( #46507, #31534, #61796, #36854 ),
 .UNSPECIFIED., .F., .F. ) 
 B_SPLINE_CURVE_WITH_KNOTS ( ( 4, 4 ),
 ( 5.423376644452276629, 5.470465898410777683 ),
 .UNSPECIFIED. ) 
 CURVE ( )  GEOMETRIC_REPRESENTATION_ITEM ( )  RATIONAL_B_SPLINE_CURVE ( ( 1.000000000000000000, 0.9998152253828482827, 0.9998152253828482827, 1.000000000000000000 ) ) 
 REPRESENTATION_ITEM ( '' )  );
#32791 = ORIENTED_EDGE ( 'NONE', *, *, #47064, .F. ) ;
#32792 = FACE_OUTER_BOUND ( 'NONE', #43393, .T. ) ;
#32793 = CARTESIAN_POINT ( 'NONE',  ( -37.00000000000000711, 7.718225330433808651, 9.430788938294078605 ) ) ;
#32794 = CIRCLE ( 'NONE', #56024, 2.999999999999996447 ) ;
#32795 = CARTESIAN_POINT ( 'NONE',  ( -28.67667724226168602, 0.8389685652162113261, -1.695959153103727912 ) ) ;
#32796 = CARTESIAN_POINT ( 'NONE',  ( 2.969415267404944103, -5.354299007565654911, -5.777543886622379610 ) ) ;
#32797 = VERTEX_POINT ( 'NONE', #4951 ) ;
#32798 = CARTESIAN_POINT ( 'NONE',  ( 0.2652384770603674613, -6.065775245581090047, -10.63836422907230350 ) ) ;
#32799 = CARTESIAN_POINT ( 'NONE',  ( -27.04788180060269909, -0.2724356095623292617, 3.218072544330532470 ) ) ;
#32800 = CARTESIAN_POINT ( 'NONE',  ( -24.42101984568203932, 0.3620223918248580697, -4.276292373952003345 ) ) ;
#32801 = AXIS2_PLACEMENT_3D ( 'NONE', #63969, #63624, #12757 ) ;
#32802 = CARTESIAN_POINT ( 'NONE',  ( -50.00070814568297095, 0.0001445496031171917693, -0.7971761463862191421 ) ) ;
#32803 = EDGE_CURVE ( 'NONE', #19720, #64984, #28089, .T. ) ;
#32804 = LINE ( 'NONE', #53113, #24579 ) ;
#32805 = CYLINDRICAL_SURFACE ( 'NONE', #24473, 12.75000000000000178 ) ;
#32806 = ORIENTED_EDGE ( 'NONE', *, *, #46137, .T. ) ;
#32807 = CARTESIAN_POINT ( 'NONE',  ( -22.27384469013076185, -3.564715702084494175, 0.9224151068931482067 ) ) ;
#32808 = CARTESIAN_POINT ( 'NONE',  ( 35.00000000000000000, 5.391785509271111110, 10.43555801961468887 ) ) ;
#32809 = CARTESIAN_POINT ( 'NONE',  ( -14.06029564544070531, -34.40539544390912141, -8.431086515739542264 ) ) ;
#32810 = ORIENTED_EDGE ( 'NONE', *, *, #4708, .T. ) ;
#32811 = CARTESIAN_POINT ( 'NONE',  ( -18.08686583997219799, 4.944984469693710416, -12.56371394453824841 ) ) ;
#32812 = DIRECTION ( 'NONE',  ( 0.000000000000000000, 0.000000000000000000, -1.000000000000000000 ) ) ;
#32813 = CARTESIAN_POINT ( 'NONE',  ( 0.3675815128205894289, -5.910255304480370953, -10.76447900494946452 ) ) ;
#32814 = CARTESIAN_POINT ( 'NONE',  ( -14.11589373245165469, 8.250315036047107142, 25.00000000000000000 ) ) ;
#32815 = DIRECTION ( 'NONE',  ( 0.000000000000000000, 0.000000000000000000, 1.000000000000000000 ) ) ;
#32816 = EDGE_CURVE ( 'NONE', #57499, #29549, #13008, .T. ) ;
#32817 = AXIS2_PLACEMENT_3D ( 'NONE', #39071, #49422, #43740 ) ;
#32818 = ORIENTED_EDGE ( 'NONE', *, *, #23845, .T. ) ;
#32819 = EDGE_LOOP ( 'NONE', ( #60106, #12645, #43236, #51614 ) ) ;
#32820 = CARTESIAN_POINT ( 'NONE',  ( 0.3675815128205894289, 1.872154644482084684, 12.13672785388550679 ) ) ;
#32821 = VERTEX_POINT ( 'NONE', #5952 ) ;
#32822 = CARTESIAN_POINT ( 'NONE',  ( 37.00000000000000711, 1.262958560998929558, 12.12087942037208066 ) ) ;
#32823 = DIRECTION ( 'NONE',  ( 1.000000000000000000, -0.000000000000000000, 0.000000000000000000 ) ) ;
#32824 = CARTESIAN_POINT ( 'NONE',  ( 2.655192694322970670, 9.337840456951635559, -2.234846078478380793 ) ) ;
#32825 = CARTESIAN_POINT ( 'NONE',  ( 1.547277799339728643, 3.695326562728670883, -12.12286970032385014 ) ) ;
#32827 = FACE_OUTER_BOUND ( 'NONE', #53434, .T. ) ;
#32826 = AXIS2_PLACEMENT_3D ( 'NONE', #22596, #33860, #18612 ) ;
#32828 = CARTESIAN_POINT ( 'NONE',  ( 2.268878695254630706, 5.759001817705426518, 5.025754889200215736 ) ) ;
#32829 = CARTESIAN_POINT ( 'NONE',  ( -37.00000000000000711, 5.015831474386455824, -10.62137734850263016 ) ) ;
#32830 = VERTEX_POINT ( 'NONE', #26208 ) ;
#32831 = VERTEX_POINT ( 'NONE', #41472 ) ;
#32832 = DIRECTION ( 'NONE',  ( 0.000000000000000000, 0.8169148498130297531, -0.5767582926624941209 ) ) ;
#32833 = VERTEX_POINT ( 'NONE', #47478 ) ;
#32834 = DIRECTION ( 'NONE',  ( 0.000000000000000000, -0.1387779952735885280, 0.9903235168508540687 ) ) ;
#32835 = CIRCLE ( 'NONE', #16911, 4.999999999999998224 ) ;
#32836 = FACE_OUTER_BOUND ( 'NONE', #41593, .T. ) ;
#32837 = CARTESIAN_POINT ( 'NONE',  ( 0.000000000000000000, 4.976357229393922665, -4.652926418895522609 ) ) ;
#32839 = ORIENTED_EDGE ( 'NONE', *, *, #4596, .T. ) ;
#32838 = CIRCLE ( 'NONE', #25404, 6.936499999999992561 ) ;
#32840 = DIRECTION ( 'NONE',  ( 0.000000000000000000, 0.01356324068817998940, -0.9999080150203990547 ) ) ;
#32841 = ADVANCED_FACE ( 'NONE', ( #46807 ), #1916, .T. ) ;
#32842 = CARTESIAN_POINT ( 'NONE',  ( -12.36714175812404015, -29.91041276695247575, -8.471522614803607354 ) ) ;
#32843 = DIRECTION ( 'NONE',  ( 1.000000000000000000, 0.000000000000000000, 0.000000000000000000 ) ) ;
#32844 = EDGE_LOOP ( 'NONE', ( #24754, #8484, #23183, #49584 ) ) ;
#32845 = VERTEX_POINT ( 'NONE', #12210 ) ;
#32846 = FACE_OUTER_BOUND ( 'NONE', #5501, .T. ) ;
#32847 = EDGE_CURVE ( 'NONE', #19477, #9113, #17867, .T. ) ;
#32848 = ORIENTED_EDGE ( 'NONE', *, *, #35965, .F. ) ;
#32849 = EDGE_LOOP ( 'NONE', ( #41364, #37582, #48367, #20919 ) ) ;
#32850 = FACE_OUTER_BOUND ( 'NONE', #28597, .T. ) ;
#32851 = ORIENTED_EDGE ( 'NONE', *, *, #23742, .T. ) ;
#32852 = B_SPLINE_CURVE_WITH_KNOTS ( 'NONE', 3,
 ( #31821, #18195, #48140, #1913, #17208, #53451, #52785, #58433, #22184, #62407, #37810, #22864, #2911, #16871, #1607, #27497 ),
 .UNSPECIFIED., .F., .F.,
 ( 4, 3, 3, 3, 3, 4 ),
 ( 0.000000000000000000, 0.0002176109881720192808, 0.0004352086762394508004, 0.0006528017811446763406, 0.0007615147961451593749, 0.0009453342004947440022 ),
 .UNSPECIFIED. ) ;
#32853 = EDGE_LOOP ( 'NONE', ( #56156, #10422, #11156, #5833 ) ) ;
#32854 = CARTESIAN_POINT ( 'NONE',  ( -22.27721701579900682, -2.783642043008650813, 2.409654355488387356 ) ) ;
#32855 = CARTESIAN_POINT ( 'NONE',  ( 19.56743653832047158, -33.00000000000000000, -5.000000000000017764 ) ) ;
#32856 = CARTESIAN_POINT ( 'NONE',  ( -21.17861794710831091, -11.44571409049744481, -3.604945070120774808 ) ) ;
#32858 = EDGE_CURVE ( 'NONE', #62960, #14197, #62111, .T. ) ;
#32857 = CARTESIAN_POINT ( 'NONE',  ( 2.000000000000001776, 0.000000000000000000, 0.000000000000000000 ) ) ;
#32859 = CARTESIAN_POINT ( 'NONE',  ( 0.2655924914740778187, -2.083162675473532399, -12.06787830249867355 ) ) ;
#32860 = CARTESIAN_POINT ( 'NONE',  ( 0.2717059086738999318, 11.56868249951481786, 4.023283916512469638 ) ) ;
#32861 = ORIENTED_EDGE ( 'NONE', *, *, #48792, .T. ) ;
#32862 = DIRECTION ( 'NONE',  ( 0.000000000000000000, -0.01356324068817992175, 0.9999080150203990547 ) ) ;
#32863 = CARTESIAN_POINT ( 'NONE',  ( -22.27706485742869091, 2.985151051101503583, -2.154081322712197544 ) ) ;
#32864 = FACE_OUTER_BOUND ( 'NONE', #25754, .T. ) ;
#32865 = ADVANCED_FACE ( 'NONE', ( #32480 ), #63087, .T. ) ;
#32866 = EDGE_CURVE ( 'NONE', #53501, #7090, #42445, .T. ) ;
#32867 = DIRECTION ( 'NONE',  ( -1.000000000000000000, -0.000000000000000000, 0.000000000000000000 ) ) ;
#32868 = CYLINDRICAL_SURFACE ( 'NONE', #65722, 12.74999999999999822 ) ;
#32869 = DIRECTION ( 'NONE',  ( 1.000000000000000000, 0.000000000000000000, 0.000000000000000000 ) ) ;
#32870 = DIRECTION ( 'NONE',  ( 0.000000000000000000, 0.000000000000000000, 1.000000000000000000 ) ) ;
#32871 = CARTESIAN_POINT ( 'NONE',  ( -4.979813338170842485, -1.249770091004171357, 11.93591655830499931 ) ) ;
#32872 = AXIS2_PLACEMENT_3D ( 'NONE', #60793, #61118, #55474 ) ;
#32873 = AXIS2_PLACEMENT_3D ( 'NONE', #7626, #48219, #26927 ) ;
#32874 = VERTEX_POINT ( 'NONE', #52788 ) ;
#32875 = CARTESIAN_POINT ( 'NONE',  ( 2.705197763288545332, -7.218866228162265308, -2.925192046931980094 ) ) ;
#32876 = AXIS2_PLACEMENT_3D ( 'NONE', #13105, #33388, #3147 ) ;
#32877 = ORIENTED_EDGE ( 'NONE', *, *, #45180, .F. ) ;
#32878 = CARTESIAN_POINT ( 'NONE',  ( -11.19266278829386252, -9.205500726053108096, 7.720277079051165892 ) ) ;
#32879 = CARTESIAN_POINT ( 'NONE',  ( 2.242819959140645913, 5.913965034148218614, -4.828731837260174409 ) ) ;
#32880 = CARTESIAN_POINT ( 'NONE',  ( -36.00000000000000711, 11.66664283989680051, 5.143145423404322791 ) ) ;
#32881 = FACE_OUTER_BOUND ( 'NONE', #18882, .T. ) ;
#32882 = CARTESIAN_POINT ( 'NONE',  ( -35.00000000000000000, 0.000000000000000000, 0.000000000000000000 ) ) ;
#32883 = EDGE_LOOP ( 'NONE', ( #63425, #34526, #46938, #49327 ) ) ;
#32884 = CARTESIAN_POINT ( 'NONE',  ( 35.00000000000000000, 12.09831040184923978, -1.463443770872822736 ) ) ;
#32885 = CARTESIAN_POINT ( 'NONE',  ( 35.00000000000000000, -8.839356091080105671, -8.389074212634254124 ) ) ;
#32886 = CARTESIAN_POINT ( 'NONE',  ( 37.00000000000000711, -11.39945968423467448, 5.710938531231826154 ) ) ;
#32887 = CARTESIAN_POINT ( 'NONE',  ( 4.563054428362612214, -30.91385115595551625, -14.84911024295102422 ) ) ;
#32888 = CIRCLE ( 'NONE', #11640, 12.18650000000000233 ) ;
#32889 = VECTOR ( 'NONE', #782, 1000.000000000000114 ) ;
#32890 = CARTESIAN_POINT ( 'NONE',  ( -4.975205859172449507, -1.416020129149132778, -13.42553116244733680 ) ) ;
#32891 = ORIENTED_EDGE ( 'NONE', *, *, #42843, .T. ) ;
#32892 = CARTESIAN_POINT ( 'NONE',  ( 2.903928887687982741, -3.918141038920174513, 7.845932231842924764 ) ) ;
#32893 = CARTESIAN_POINT ( 'NONE',  ( 1.719304012340734378, -8.755325027794794934, -9.242227816401850760 ) ) ;
#32894 = CARTESIAN_POINT ( 'NONE',  ( -0.9215452301657053313, -30.54833844081648309, 15.29585404987972375 ) ) ;
#32895 = EDGE_CURVE ( 'NONE', #35536, #32989, #59313, .T. ) ;
#32896 = CIRCLE ( 'NONE', #29717, 5.000000000000000888 ) ;
#32897 = ADVANCED_FACE ( 'NONE', ( #53110 ), #7547, .T. ) ;
#32898 = ORIENTED_EDGE ( 'NONE', *, *, #62336, .T. ) ;
#32899 = CARTESIAN_POINT ( 'NONE',  ( -8.907762356386051295, 9.802223273060290509, -9.289308028724567734 ) ) ;
#32900 = ORIENTED_EDGE ( 'NONE', *, *, #35659, .T. ) ;
#32901 = CARTESIAN_POINT ( 'NONE',  ( 2.259025283528087957, -6.547290863799063665, 3.937899517809461791 ) ) ;
#32902 = CARTESIAN_POINT ( 'NONE',  ( 36.00000000000000711, 8.496612874013157679, -9.506317355798405089 ) ) ;
#32903 = CARTESIAN_POINT ( 'NONE',  ( 28.15855999187490966, -3.461419147680622199, 23.80441447217193840 ) ) ;
#32904 = CARTESIAN_POINT ( 'NONE',  ( 2.000000000000001776, 6.796153407501448029, 1.388283512725836388 ) ) ;
#32905 = CARTESIAN_POINT ( 'NONE',  ( -22.27786964138239867, -2.131221155130656353, -3.004507515156384034 ) ) ;
#32906 = ORIENTED_EDGE ( 'NONE', *, *, #8083, .T. ) ;
#32907 = VERTEX_POINT ( 'NONE', #63394 ) ;
#32908 = ORIENTED_EDGE ( 'NONE', *, *, #59076, .F. ) ;
#32909 = DIRECTION ( 'NONE',  ( 1.000000000000000000, 0.000000000000000000, -0.000000000000000000 ) ) ;
#32911 = CARTESIAN_POINT ( 'NONE',  ( 5.514624014163232779, -0.0001700579043838964816, -0.004137701579365772077 ) ) ;
#32910 = AXIS2_PLACEMENT_3D ( 'NONE', #7992, #52566, #6995 ) ;
#32912 = ADVANCED_FACE ( 'NONE', ( #38127 ), #41821, .T. ) ;
#32913 = AXIS2_PLACEMENT_3D ( 'NONE', #56101, #5598, #912 ) ;
#32914 = ORIENTED_EDGE ( 'NONE', *, *, #60369, .T. ) ;
#32915 = DIRECTION ( 'NONE',  ( -1.000000000000000000, 0.000000000000000000, 0.000000000000000000 ) ) ;
#32916 = CARTESIAN_POINT ( 'NONE',  ( -22.28023996335807411, -0.3233044107360732999, -3.676538434326164673 ) ) ;
#32917 = ORIENTED_EDGE ( 'NONE', *, *, #615, .F. ) ;
#32918 = CARTESIAN_POINT ( 'NONE',  ( -35.00000000000000000, 11.81949347079751256, -2.968224442958276921 ) ) ;
#32919 = EDGE_CURVE ( 'NONE', #64219, #31959, #33620, .T. ) ;
#32920 = ADVANCED_FACE ( 'NONE', ( #14721 ), #40674, .T. ) ;
#32921 = B_SPLINE_CURVE_WITH_KNOTS ( 'NONE', 3,
 ( #47815, #36530, #52804, #17234, #42146, #32175, #58128, #57813, #2274, #32498, #42467, #62433, #31529, #62128, #11575, #31846, #27518, #52160, #26880, #16895 ),
 .UNSPECIFIED., .F., .F.,
 ( 4, 2, 2, 2, 2, 2, 2, 2, 2, 4 ),
 ( 2.874676074482899647E-18, 0.001273611734732489056, 0.002547223469464975510, 0.003820835204197461313, 0.005094446938929947551, 0.006368058673662434221, 0.007004864541028676256, 0.007641670408394919158, 0.008915282143127404094, 0.01018889387785988643 ),
 .UNSPECIFIED. ) ;
#32922 = CARTESIAN_POINT ( 'NONE',  ( 2.297017764050093280, -2.771707546665545419, -7.133399178907342097 ) ) ;
#32923 = CARTESIAN_POINT ( 'NONE',  ( -35.00000000000000000, 8.954052073409602741, 9.076753354954030684 ) ) ;
#32924 = ORIENTED_EDGE ( 'NONE', *, *, #61286, .T. ) ;
#32925 = ORIENTED_EDGE ( 'NONE', *, *, #55911, .T. ) ;
#32926 = CARTESIAN_POINT ( 'NONE',  ( 2.284126774967659479, 2.466502196988966666, 7.240052432235658308 ) ) ;
#32927 = EDGE_CURVE ( 'NONE', #20597, #23499, #20069, .T. ) ;
#32928 = ORIENTED_EDGE ( 'NONE', *, *, #10300, .F. ) ;
#32929 = CARTESIAN_POINT ( 'NONE',  ( 11.13055501096828692, 0.3454441929252254906, -13.49618539646086113 ) ) ;
#32930 = VERTEX_POINT ( 'NONE', #23175 ) ;
#32931 = CARTESIAN_POINT ( 'NONE',  ( 2.253265082352433613, 3.707567016433813922, 6.678225412356958657 ) ) ;
#32932 = CIRCLE ( 'NONE', #62638, 5.000000000000000888 ) ;
#32933 = CARTESIAN_POINT ( 'NONE',  ( 15.45402751311997847, -34.86645063878531658, -6.224822664678947959 ) ) ;
#32934 = CARTESIAN_POINT ( 'NONE',  ( 35.00000000000000000, 4.074242145636174151, 12.08151691381185167 ) ) ;
#32935 = CARTESIAN_POINT ( 'NONE',  ( -22.27719381268171617, 3.550654232855438242, 0.9730858478813626533 ) ) ;
#32937 = EDGE_CURVE ( 'NONE', #2547, #40853, #38468, .T. ) ;
#32936 = DIRECTION ( 'NONE',  ( -1.000000000000000000, -0.000000000000000000, 0.000000000000000000 ) ) ;
#32938 = CARTESIAN_POINT ( 'NONE',  ( -35.00000000000000000, -0.7008968033237865658, -12.16632754454237819 ) ) ;
#32939 = DIRECTION ( 'NONE',  ( 1.000000000000000000, 0.000000000000000000, 0.000000000000000000 ) ) ;
#32940 = ORIENTED_EDGE ( 'NONE', *, *, #61102, .F. ) ;
#32941 = CIRCLE ( 'NONE', #43528, 12.18649999999999878 ) ;
#32942 = CARTESIAN_POINT ( 'NONE',  ( -1.327480008007509151E-11, -31.03649492335491544, -14.44372008463338908 ) ) ;
#32943 = ORIENTED_EDGE ( 'NONE', *, *, #22188, .F. ) ;
#32944 = DIRECTION ( 'NONE',  ( -1.000000000000000000, 0.000000000000000000, 0.000000000000000000 ) ) ;
#32945 = EDGE_CURVE ( 'NONE', #23983, #2293, #43441, .T. ) ;
#32946 = CARTESIAN_POINT ( 'NONE',  ( 0.000000000000000000, 5.217815162096925086, -5.387430271863535403 ) ) ;
#32947 = VERTEX_POINT ( 'NONE', #9751 ) ;
#32948 = CARTESIAN_POINT ( 'NONE',  ( 25.05309951391468459, 10.77522019223767558, -8.132934882857098202 ) ) ;
#32949 = CARTESIAN_POINT ( 'NONE',  ( 0.2915757698887249671, 6.312478057070456394, 10.50410115670271516 ) ) ;
#32950 = AXIS2_PLACEMENT_3D ( 'NONE', #30166, #10205, #52093 ) ;
#32951 = CARTESIAN_POINT ( 'NONE',  ( 2.653899356899475759, -7.604196386057373580, 1.606012885791342271 ) ) ;
#32952 = ORIENTED_EDGE ( 'NONE', *, *, #13044, .F. ) ;
#32953 = ORIENTED_EDGE ( 'NONE', *, *, #53183, .F. ) ;
#32954 = DIRECTION ( 'NONE',  ( 1.000000000000000000, 0.000000000000000000, 0.000000000000000000 ) ) ;
#32955 = ADVANCED_FACE ( 'NONE', ( #58783 ), #60379, .T. ) ;
#32956 = AXIS2_PLACEMENT_3D ( 'NONE', #53665, #28372, #48670 ) ;
#32957 = ORIENTED_EDGE ( 'NONE', *, *, #54324, .F. ) ;
#32958 = DIRECTION ( 'NONE',  ( 1.000000000000000000, -0.000000000000000000, -0.000000000000000000 ) ) ;
#32959 = DIRECTION ( 'NONE',  ( 0.000000000000000000, -0.5472293298355157543, 0.8369827122275419473 ) ) ;
#32960 = DIRECTION ( 'NONE',  ( -1.000000000000000000, -0.000000000000000000, 0.000000000000000000 ) ) ;
#32961 = FACE_OUTER_BOUND ( 'NONE', #21434, .T. ) ;
#32962 = VERTEX_POINT ( 'NONE', #38801 ) ;
#32963 = DIRECTION ( 'NONE',  ( 0.000000000000000000, -0.01356324068817992175, 0.9999080150203990547 ) ) ;
#32964 = CIRCLE ( 'NONE', #4323, 2.899999999999995026 ) ;
#32965 = MECHANICAL_DESIGN_GEOMETRIC_PRESENTATION_REPRESENTATION (  '', ( #22337 ), #1096 ) ;
#32966 = CIRCLE ( 'NONE', #19167, 6.936499999999989896 ) ;
#32967 = CARTESIAN_POINT ( 'NONE',  ( 35.00000000000000000, -9.390600770288049404, -8.624332853796024878 ) ) ;
#32968 = CARTESIAN_POINT ( 'NONE',  ( -35.00000000000000000, -11.61175578952785159, -1.771820996347277966 ) ) ;
#32969 = CARTESIAN_POINT ( 'NONE',  ( 5.516018279890452902, 0.006286471671801929263, -0.002527316374434327665 ) ) ;
#32970 = DIRECTION ( 'NONE',  ( 0.000000000000000000, -1.000000000000000000, 0.000000000000000000 ) ) ;
#32971 = B_SPLINE_CURVE_WITH_KNOTS ( 'NONE', 3,
 ( #52288, #31639, #41951, #51951, #6079, #56263, #46957, #5758, #16018, #6391, #26662, #40980, #10706, #84, #15686, #1416 ),
 .UNSPECIFIED., .F., .F.,
 ( 4, 3, 3, 3, 3, 4 ),
 ( 4.336808689942017255E-19, 0.0002176109881720263281, 0.0004352086762394657081, 0.0006528017811446956394, 0.0007615147961451794326, 0.0009453342004944464971 ),
 .UNSPECIFIED. ) ;
#32972 = FACE_OUTER_BOUND ( 'NONE', #32578, .T. ) ;
#32973 = CYLINDRICAL_SURFACE ( 'NONE', #345, 2.899999999999994582 ) ;
#32974 = VECTOR ( 'NONE', #15433, 1000.000000000000000 ) ;
#32975 = EDGE_CURVE ( 'NONE', #45713, #64338, #63553, .T. ) ;
#32976 = AXIS2_PLACEMENT_3D ( 'NONE', #14952, #55208, #48934 ) ;
#32977 = EDGE_LOOP ( 'NONE', ( #31508, #52898, #7003, #50030 ) ) ;
#32978 = CARTESIAN_POINT ( 'NONE',  ( -37.00000000000000711, -4.237174932027140350, -12.02534193257725725 ) ) ;
#32979 = AXIS2_PLACEMENT_3D ( 'NONE', #49112, #58423, #7200 ) ;
#32980 = CIRCLE ( 'NONE', #50002, 12.18650000000000055 ) ;
#32981 =( BOUNDED_SURFACE ( )  B_SPLINE_SURFACE ( 3, 2, ( 
 ( #9782, #60324, #40358 ),
 ( #55995, #15742, #4496 ),
 ( #55343, #30066, #35698 ),
 ( #50035, #50696, #24763 ),
 ( #25092, #10767, #10432 ),
 ( #29726, #4825, #34710 ),
 ( #36020, #49707, #20095 ),
 ( #19782, #60659, #56319 ),
 ( #39724, #15097, #45043 ),
 ( #4154, #60016, #35375 ),
 ( #50378, #55683, #491 ),
 ( #5141, #24418, #14435 ),
 ( #45688, #5480, #55009 ),
 ( #65316, #10120, #9440 ),
 ( #40038, #25408, #147 ),
 ( #14752, #20428, #40705 ),
 ( #25748, #60997, #51019 ),
 ( #15431, #41025, #20756 ),
 ( #61308, #21064, #52344 ),
 ( #37687, #37347, #57983 ),
 ( #41345, #52003, #17411 ),
 ( #62285, #6447, #57316 ),
 ( #26726, #16740, #27057 ),
 ( #41686, #22378, #31056 ),
 ( #51688, #47021, #42643 ),
 ( #6130, #51366, #36699 ),
 ( #46675, #21755, #6783 ),
 ( #799, #1476, #61976 ),
 ( #7092, #42005, #32355 ),
 ( #46357, #62949, #16432 ),
 ( #56997, #61629, #47351 ),
 ( #11738, #26391, #1792 ),
 ( #16083, #37013, #26081 ),
 ( #32025, #22057, #42313 ),
 ( #62603, #17065, #57659 ),
 ( #12075, #1130, #21411 ),
 ( #11422, #52667, #5819 ),
 ( #31692, #36372, #27367 ),
 ( #2108, #47662, #56678 ),
 ( #11112, #31387, #59283 ),
 ( #37999, #58302, #8092 ),
 ( #63589, #13390, #13707 ),
 ( #63933, #12722, #28361 ),
 ( #13073, #33674, #27695 ),
 ( #38675, #18064, #53966 ),
 ( #38326, #32663, #18734 ),
 ( #58649, #33006, #53319 ),
 ( #8406, #7763, #28045 ),
 ( #49334, #18410, #48346 ),
 ( #3781, #28682, #48001 ) ),
 .UNSPECIFIED., .F., .F., .F. ) 
 B_SPLINE_SURFACE_WITH_KNOTS ( ( 4, 2, 2, 2, 2, 2, 2, 2, 2, 2, 2, 2, 2, 2, 2, 2, 2, 2, 2, 2, 2, 2, 2, 2, 4 ),
 ( 3, 3 ),
 ( 0.06047842900482980344, 0.06367705432712369995, 0.06527636698827063433, 0.06687567964941758258, 0.06847499231056453084, 0.07007430497171146522, 0.07327293029400536173, 0.07647155561629924436, 0.07807086827744619262, 0.07967018093859312700, 0.08286880626088702351, 0.08446811892203395788, 0.08606743158318090614, 0.08926605690547478877, 0.09086536956662173703, 0.09246468222776868529, 0.09566330755006256792, 0.09726262021120951617, 0.09886193287235645055, 0.1020605581946503471, 0.1052591835169442297, 0.1068584961780911780, 0.1084578088392381123, 0.1100571215003850606, 0.1116564341615320088 ),
 ( 0.000000000000000000, 1.000000000000000000 ),
 .UNSPECIFIED. ) 
 GEOMETRIC_REPRESENTATION_ITEM ( )  RATIONAL_B_SPLINE_SURFACE ( (
 ( 1.000000000000000000, 0.4999999999999997224, 1.000000000000000000),
 ( 1.000000000000000000, 0.5048840838053595403, 1.000000000000000000),
 ( 1.000000000000000000, 0.5132072642500212778, 1.000000000000000000),
 ( 1.000000000000000000, 0.5290214861663710133, 1.000000000000000000),
 ( 1.000000000000000000, 0.5348648783786191796, 1.000000000000000000),
 ( 1.000000000000000000, 0.5473516051742142174, 1.000000000000000000),
 ( 1.000000000000000000, 0.5539126387906654347, 1.000000000000000000),
 ( 1.000000000000000000, 0.5674101295481297491, 1.000000000000000000),
 ( 1.000000000000000000, 0.5743474342084209372, 1.000000000000000000),
 ( 1.000000000000000000, 0.5883951384281623787, 1.000000000000000000),
 ( 1.000000000000000000, 0.5955302209472954633, 1.000000000000000000),
 ( 1.000000000000000000, 0.6167715304224314909, 1.000000000000000000),
 ( 1.000000000000000000, 0.6305661306848800995, 1.000000000000000000),
 ( 1.000000000000000000, 0.6565125894471021128, 1.000000000000000000),
 ( 1.000000000000000000, 0.6686743926052455267, 1.000000000000000000),
 ( 1.000000000000000000, 0.6851014456086111926, 1.000000000000000000),
 ( 1.000000000000000000, 0.6902475665164108376, 1.000000000000000000),
 ( 1.000000000000000000, 0.6997062435423183624, 1.000000000000000000),
 ( 1.000000000000000000, 0.7040363771866963161, 1.000000000000000000),
 ( 1.000000000000000000, 0.7157418617803246175, 1.000000000000000000),
 ( 1.000000000000000000, 0.7218341033858746147, 1.000000000000000000),
 ( 1.000000000000000000, 0.7280280015706425134, 1.000000000000000000),
 ( 1.000000000000000000, 0.7296036051598833172, 1.000000000000000000),
 ( 1.000000000000000000, 0.7316818214130011988, 1.000000000000000000),
 ( 1.000000000000000000, 0.7321927565543977501, 1.000000000000000000),
 ( 1.000000000000000000, 0.7321641879724063440, 1.000000000000000000),
 ( 1.000000000000000000, 0.7300624469251318915, 1.000000000000000000),
 ( 1.000000000000000000, 0.7238943330024291134, 1.000000000000000000),
 ( 1.000000000000000000, 0.7213359435419269827, 1.000000000000000000),
 ( 1.000000000000000000, 0.7152343487864535332, 1.000000000000000000),
 ( 1.000000000000000000, 0.7117056589943943079, 1.000000000000000000),
 ( 1.000000000000000000, 0.6999072021060611659, 1.000000000000000000),
 ( 1.000000000000000000, 0.6903911339383190793, 1.000000000000000000),
 ( 1.000000000000000000, 0.6741089150890113846, 1.000000000000000000),
 ( 1.000000000000000000, 0.6683461163769177649, 1.000000000000000000),
 ( 1.000000000000000000, 0.6562237482356456653, 1.000000000000000000),
 ( 1.000000000000000000, 0.6498375142660577364, 1.000000000000000000),
 ( 1.000000000000000000, 0.6302143011362419944, 1.000000000000000000),
 ( 1.000000000000000000, 0.6164540672887564021, 1.000000000000000000),
 ( 1.000000000000000000, 0.5885848209491307825, 1.000000000000000000),
 ( 1.000000000000000000, 0.5744580946949390254, 1.000000000000000000),
 ( 1.000000000000000000, 0.5540565490002423710, 1.000000000000000000),
 ( 1.000000000000000000, 0.5474350731751366217, 1.000000000000000000),
 ( 1.000000000000000000, 0.5350293539660311293, 1.000000000000000000),
 ( 1.000000000000000000, 0.5292092555093077522, 1.000000000000000000),
 ( 1.000000000000000000, 0.5186171472262492976, 1.000000000000000000),
 ( 1.000000000000000000, 0.5138445523878416576, 1.000000000000000000),
 ( 1.000000000000000000, 0.5056909436241932010, 1.000000000000000000),
 ( 1.000000000000000000, 0.5023956439952826925, 1.000000000000000000),
 ( 1.000000000000000000, 0.4999999999999995004, 1.000000000000000000) ) ) 
 REPRESENTATION_ITEM ( '' )  SURFACE ( )  );
#32982 = ORIENTED_EDGE ( 'NONE', *, *, #5687, .T. ) ;
#32983 = CARTESIAN_POINT ( 'NONE',  ( 0.3341166715381286290, 1.881279064088004827, -12.12403120948087931 ) ) ;
#32984 = CARTESIAN_POINT ( 'NONE',  ( -22.29677679919927868, 3.730758197825081446, -0.2674217835790786979 ) ) ;
#32985 = CARTESIAN_POINT ( 'NONE',  ( 1.948354844645469264, -6.595573209516436997, -9.982942661983956967 ) ) ;
#32986 = ORIENTED_EDGE ( 'NONE', *, *, #32945, .F. ) ;
#32987 = AXIS2_PLACEMENT_3D ( 'NONE', #45986, #31340, #15693 ) ;
#32988 = CYLINDRICAL_SURFACE ( 'NONE', #2335, 12.74999999999999822 ) ;
#32989 = VERTEX_POINT ( 'NONE', #23509 ) ;
#32990 = CIRCLE ( 'NONE', #6486, 4.999999999999998224 ) ;
#32991 = DIRECTION ( 'NONE',  ( 0.000000000000000000, -0.8660254037844380415, -0.5000000000000009992 ) ) ;
#32992 = ORIENTED_EDGE ( 'NONE', *, *, #38692, .F. ) ;
#32993 = VERTEX_POINT ( 'NONE', #43786 ) ;
#32994 = CARTESIAN_POINT ( 'NONE',  ( 29.60171417218365519, -10.89687559552093532, 7.981938771698986912 ) ) ;
#32995 = CARTESIAN_POINT ( 'NONE',  ( 0.3160775863651110185, -12.03278055228169485, -2.365582350580189619 ) ) ;
#32996 = EDGE_CURVE ( 'NONE', #15001, #1502, #59099, .T. ) ;
#32997 = VERTEX_POINT ( 'NONE', #35346 ) ;
#32998 = LINE ( 'NONE', #33349, #27092 ) ;
#32999 = CYLINDRICAL_SURFACE ( 'NONE', #36768, 14.99999999999998757 ) ;
#33000 = DIRECTION ( 'NONE',  ( -1.000000000000000000, 0.000000000000000000, 0.000000000000000000 ) ) ;
#33001 = AXIS2_PLACEMENT_3D ( 'NONE', #34260, #4015, #13970 ) ;
#33002 = CYLINDRICAL_SURFACE ( 'NONE', #18458, 12.74999999999999822 ) ;
#33003 = ORIENTED_EDGE ( 'NONE', *, *, #53986, .F. ) ;
#33004 = FACE_OUTER_BOUND ( 'NONE', #41258, .T. ) ;
#33005 = EDGE_CURVE ( 'NONE', #51673, #18713, #20053, .T. ) ;
#33006 = CARTESIAN_POINT ( 'NONE',  ( 12.74086035833940045, -29.15670053398430994, 4.066541195106272433 ) ) ;
#33007 = DIRECTION ( 'NONE',  ( 1.000000000000000000, 0.000000000000000000, 0.000000000000000000 ) ) ;
#33009 = ORIENTED_EDGE ( 'NONE', *, *, #48177, .T. ) ;
#33008 = CARTESIAN_POINT ( 'NONE',  ( -37.00000000000000711, 9.348667969174405457, 7.817492529713891081 ) ) ;
#33011 = CIRCLE ( 'NONE', #46839, 12.75000000000000178 ) ;
#33010 = CARTESIAN_POINT ( 'NONE',  ( -2.952869152607111136, 25.00000000000000000, 11.17020052527586138 ) ) ;
#33012 = ADVANCED_FACE ( 'NONE', ( #45014 ), #65288, .T. ) ;
#33013 = ORIENTED_EDGE ( 'NONE', *, *, #532, .T. ) ;
#33014 = CARTESIAN_POINT ( 'NONE',  ( 2.000000000000001776, -6.767909380267597363, -0.7805499053121327524 ) ) ;
#33015 = VERTEX_POINT ( 'NONE', #57287 ) ;
#33016 = CARTESIAN_POINT ( 'NONE',  ( 35.00000000000000000, -10.93004082984022851, -6.564808257521735690 ) ) ;
#33017 = CARTESIAN_POINT ( 'NONE',  ( 35.00000000000000000, 11.59095880812004964, -1.903127969211395598 ) ) ;
#33018 = CYLINDRICAL_SURFACE ( 'NONE', #22325, 5.000000000000000888 ) ;
#33019 = CARTESIAN_POINT ( 'NONE',  ( 0.2872850955227732594, -3.994021792079174293, 11.58431228138438307 ) ) ;
#33020 = AXIS2_PLACEMENT_3D ( 'NONE', #39363, #33407, #63640 ) ;
#33021 = AXIS2_PLACEMENT_3D ( 'NONE', #6905, #2242, #22521 ) ;
#33022 = CARTESIAN_POINT ( 'NONE',  ( 0.2648978790185593790, -11.55204314799266818, 4.063980959785006952 ) ) ;
#33023 = CARTESIAN_POINT ( 'NONE',  ( -22.27834755396593991, -2.305389312780946831, -2.876353066242404388 ) ) ;
#33024 = DIRECTION ( 'NONE',  ( 1.000000000000000000, 0.000000000000000000, 0.000000000000000000 ) ) ;
#33025 = ORIENTED_EDGE ( 'NONE', *, *, #27685, .F. ) ;
#33026 = VECTOR ( 'NONE', #61732, 1000.000000000000000 ) ;
#33027 = DIRECTION ( 'NONE',  ( -1.000000000000000000, -0.000000000000000000, -0.000000000000000000 ) ) ;
#33028 = ORIENTED_EDGE ( 'NONE', *, *, #32732, .T. ) ;
#33029 = EDGE_CURVE ( 'NONE', #31267, #56700, #23234, .T. ) ;
#33030 = EDGE_CURVE ( 'NONE', #55094, #57486, #6752, .T. ) ;
#33031 = EDGE_LOOP ( 'NONE', ( #4887, #51642, #59502, #15495 ) ) ;
#33032 = CARTESIAN_POINT ( 'NONE',  ( -36.00000000000000711, -12.70128625845193859, 1.113475361586445000 ) ) ;
#33033 = FACE_OUTER_BOUND ( 'NONE', #52791, .T. ) ;
#33034 = DIRECTION ( 'NONE',  ( 1.000000000000000000, 0.000000000000000000, -0.000000000000000000 ) ) ;
#33035 = CARTESIAN_POINT ( 'NONE',  ( 0.3223008802179194165, -10.49760329338524301, 6.343104382804274799 ) ) ;
#33036 = EDGE_CURVE ( 'NONE', #57471, #39575, #10401, .T. ) ;
#33038 = CIRCLE ( 'NONE', #21367, 5.000000000000000000 ) ;
#33037 = LINE ( 'NONE', #64595, #58227 ) ;
#33039 = AXIS2_PLACEMENT_3D ( 'NONE', #54614, #23026, #9034 ) ;
#33040 = DIRECTION ( 'NONE',  ( -1.000000000000000000, 0.000000000000000000, 0.000000000000000000 ) ) ;
#33041 = CARTESIAN_POINT ( 'NONE',  ( 145.1370849898475797, 3.309064568108273190E-14, 0.000000000000000000 ) ) ;
#33043 = EDGE_CURVE ( 'NONE', #63537, #11428, #41302, .T. ) ;
#33042 = CIRCLE ( 'NONE', #4395, 7.499999999999988454 ) ;
#33044 = ORIENTED_EDGE ( 'NONE', *, *, #21483, .F. ) ;
#33045 = AXIS2_PLACEMENT_3D ( 'NONE', #17811, #23123, #47743 ) ;
#33046 = EDGE_CURVE ( 'NONE', #5538, #59522, #64952, .T. ) ;
#33047 = CARTESIAN_POINT ( 'NONE',  ( 2.000000000000001776, -0.4804830611969332366, -6.919838746524582085 ) ) ;
#33048 = CARTESIAN_POINT ( 'NONE',  ( -17.78890373828789606, -5.238151136051769186, 12.44321837383489893 ) ) ;
#33049 = CIRCLE ( 'NONE', #119, 5.000000000000000888 ) ;
#33050 = DIRECTION ( 'NONE',  ( -1.000000000000000000, 0.000000000000000000, 0.000000000000000000 ) ) ;
#33051 = CARTESIAN_POINT ( 'NONE',  ( 1.000000000000000888, 6.586971819220337032, 3.586335490831404460 ) ) ;
#33052 = CIRCLE ( 'NONE', #2273, 3.000000000000000444 ) ;
#33053 = FACE_OUTER_BOUND ( 'NONE', #25478, .T. ) ;
#33054 = CARTESIAN_POINT ( 'NONE',  ( 2.000000000000001776, 3.979254915827449945, -5.681598592373734213 ) ) ;
#33055 = VECTOR ( 'NONE', #57642, 1000.000000000000000 ) ;
#33056 = ORIENTED_EDGE ( 'NONE', *, *, #19271, .F. ) ;
#33057 = CARTESIAN_POINT ( 'NONE',  ( 47.00000000000000711, 4.705694406421931860E-17, -3.469127814946512892E-15 ) ) ;
#33058 = CARTESIAN_POINT ( 'NONE',  ( 0.2676618633000489855, -1.968216791520412734, -12.08777609394270947 ) ) ;
#33059 = CARTESIAN_POINT ( 'NONE',  ( 5.516018279890452902, -0.002104829434640716982, 0.006440244342253021413 ) ) ;
#33060 = CARTESIAN_POINT ( 'NONE',  ( 4.340384785892905661, -31.41030204081990362, 14.02840248442622695 ) ) ;
#33061 = B_SPLINE_CURVE_WITH_KNOTS ( 'NONE', 3,
 ( #44259, #38955, #13667, #33310, #33951, #23999, #39268, #13998, #64532, #59564 ),
 .UNSPECIFIED., .F., .F.,
 ( 4, 2, 2, 2, 4 ),
 ( 8.673617379884035472E-19, 0.002710955585989774201, 0.003388694482487217101, 0.004066433378984660868, 0.005421911171979544933 ),
 .UNSPECIFIED. ) ;
#33062 = EDGE_CURVE ( 'NONE', #7394, #5728, #15403, .T. ) ;
#33063 = AXIS2_PLACEMENT_3D ( 'NONE', #53018, #2505, #48388 ) ;
#33064 = AXIS2_PLACEMENT_3D ( 'NONE', #41649, #61942, #16400 ) ;
#33065 = DIRECTION ( 'NONE',  ( -1.000000000000000000, 0.000000000000000000, 0.000000000000000000 ) ) ;
#33066 = CARTESIAN_POINT ( 'NONE',  ( -26.47815227414952233, -12.15021249753662325, 5.884769607083862653 ) ) ;
#33067 = VERTEX_POINT ( 'NONE', #15710 ) ;
#33068 = CARTESIAN_POINT ( 'NONE',  ( -35.00000000000000000, -7.238157050195700215, 10.49626516989268588 ) ) ;
#33069 = DIRECTION ( 'NONE',  ( -1.000000000000000000, 0.000000000000000000, 0.000000000000000000 ) ) ;
#33070 = CYLINDRICAL_SURFACE ( 'NONE', #48041, 6.936499999999988120 ) ;
#33071 = CARTESIAN_POINT ( 'NONE',  ( 1.372161826076676139, -12.51237317864394072, -1.607409531431686744 ) ) ;
#33072 = VERTEX_POINT ( 'NONE', #50988 ) ;
#33073 = CARTESIAN_POINT ( 'NONE',  ( 0.3675815128205894289, 2.391755495700603973, 12.04510820461660003 ) ) ;
#33074 = DIRECTION ( 'NONE',  ( -1.000000000000000000, 0.000000000000000000, 0.000000000000000000 ) ) ;
#33075 = ORIENTED_EDGE ( 'NONE', *, *, #61455, .T. ) ;
#33076 = EDGE_CURVE ( 'NONE', #47363, #36221, #26050, .T. ) ;
#33077 = VERTEX_POINT ( 'NONE', #41000 ) ;
#33078 = DIRECTION ( 'NONE',  ( -1.000000000000000000, 0.000000000000000000, -0.000000000000000000 ) ) ;
#33079 = AXIS2_PLACEMENT_3D ( 'NONE', #36462, #11510, #46437 ) ;
#33080 = VECTOR ( 'NONE', #48476, 999.9999999999998863 ) ;
#33081 = EDGE_CURVE ( 'NONE', #44565, #64384, #61281, .T. ) ;
#33082 = ORIENTED_EDGE ( 'NONE', *, *, #32386, .F. ) ;
#33083 = AXIS2_PLACEMENT_3D ( 'NONE', #24465, #9486, #44745 ) ;
#33084 = CARTESIAN_POINT ( 'NONE',  ( 0.3218525148189810836, -9.550803867331117303, 7.695007528464986812 ) ) ;
#33085 = CARTESIAN_POINT ( 'NONE',  ( 0.3665391374699464300, -9.576575648339069602, 7.691255657244259858 ) ) ;
#33086 = CARTESIAN_POINT ( 'NONE',  ( 37.00000000000000711, 4.705694406421931860E-17, -3.469127814946512892E-15 ) ) ;
#33087 = CYLINDRICAL_SURFACE ( 'NONE', #64803, 24.00000000000000000 ) ;
#33088 = CARTESIAN_POINT ( 'NONE',  ( -27.70115331877724785, 11.17762196442450850, -4.375698238583000332 ) ) ;
#33089 = CIRCLE ( 'NONE', #9740, 2.899999999999995914 ) ;
#33090 = CARTESIAN_POINT ( 'NONE',  ( 0.2869720083484369466, 5.945302302873249900, 10.71444492121018754 ) ) ;
#33092 = ORIENTED_EDGE ( 'NONE', *, *, #8229, .T. ) ;
#33091 = DIRECTION ( 'NONE',  ( -1.000000000000000000, -0.000000000000000000, 0.000000000000000000 ) ) ;
#33093 = CARTESIAN_POINT ( 'NONE',  ( -35.00000000000000000, 0.000000000000000000, 0.000000000000000000 ) ) ;
#33094 = EDGE_CURVE ( 'NONE', #39393, #16656, #57093, .T. ) ;
#33095 = ORIENTED_EDGE ( 'NONE', *, *, #46672, .F. ) ;
#33096 = CARTESIAN_POINT ( 'NONE',  ( 0.2653519789438759657, 10.59450269107742137, -6.142177718873826464 ) ) ;
#33097 = AXIS2_PLACEMENT_3D ( 'NONE', #50724, #21100, #15461 ) ;
#33098 = VERTEX_POINT ( 'NONE', #6102 ) ;
#33099 = VERTEX_POINT ( 'NONE', #26359 ) ;
#33100 = CARTESIAN_POINT ( 'NONE',  ( -24.96502833112928244, 11.16032118974457887, 7.597682957678232540 ) ) ;
#33101 = CARTESIAN_POINT ( 'NONE',  ( -12.92674250727408669, -33.23908083898133015, 10.84893670414254530 ) ) ;
#33102 = CARTESIAN_POINT ( 'NONE',  ( 42.50000000000000000, 1.443454975684918283E-16, -1.399999999999999911 ) ) ;
#33103 = CARTESIAN_POINT ( 'NONE',  ( -44.04183182023682974, -1.142706581721706138, 14.69327751537514715 ) ) ;
#33104 = CARTESIAN_POINT ( 'NONE',  ( 35.00000000000000000, -3.827046518385000429, 11.56998259273181162 ) ) ;
#33105 = ORIENTED_EDGE ( 'NONE', *, *, #669, .T. ) ;
#33106 = VECTOR ( 'NONE', #21519, 1000.000000000000000 ) ;
#33107 = CARTESIAN_POINT ( 'NONE',  ( -27.19357181888462094, -10.84410562793472543, 5.138615876886901468 ) ) ;
#33108 = DIRECTION ( 'NONE',  ( -1.000000000000000000, 0.000000000000000000, 0.000000000000000000 ) ) ;
#33110 = ORIENTED_EDGE ( 'NONE', *, *, #11209, .T. ) ;
#33109 = CARTESIAN_POINT ( 'NONE',  ( 0.2759803524722215795, 11.57441428600638744, -4.011137970318830348 ) ) ;
#33111 = VERTEX_POINT ( 'NONE', #31663 ) ;
#33112 = CARTESIAN_POINT ( 'NONE',  ( -37.00000000000000711, -11.16627499335652374, -3.645068577060142978 ) ) ;
#33113 = ORIENTED_EDGE ( 'NONE', *, *, #53913, .F. ) ;
#33114 = CARTESIAN_POINT ( 'NONE',  ( 2.000000000000001776, 0.000000000000000000, 0.000000000000000000 ) ) ;
#33115 = CARTESIAN_POINT ( 'NONE',  ( -36.00000000000000711, 12.42372387097882580, 2.865935305911670561 ) ) ;
#33116 = CARTESIAN_POINT ( 'NONE',  ( -35.00000000000000000, 9.076753354954126607, -8.954052073409506818 ) ) ;
#33117 = ADVANCED_FACE ( 'NONE', ( #56967 ), #11390, .T. ) ;
#33118 = CARTESIAN_POINT ( 'NONE',  ( -22.27706485742869091, 2.985151051101503583, -2.154081322712197544 ) ) ;
#33119 = VECTOR ( 'NONE', #61698, 1000.000000000000000 ) ;
#33120 = AXIS2_PLACEMENT_3D ( 'NONE', #7613, #48205, #2657 ) ;
#33121 = CARTESIAN_POINT ( 'NONE',  ( 1.452237505248555660, 3.767214359061289652, -12.08199618361509131 ) ) ;
#33122 = CARTESIAN_POINT ( 'NONE',  ( -27.08954555554413446, -1.900922216193322800, 1.307633183325030313 ) ) ;
#33123 = AXIS2_PLACEMENT_3D ( 'NONE', #45341, #65602, #20074 ) ;
#33124 = EDGE_CURVE ( 'NONE', #63543, #25796, #21723, .T. ) ;
#33125 = CARTESIAN_POINT ( 'NONE',  ( -7.181456785175555524, -8.540743096806455270, -10.45493698471458188 ) ) ;
#33126 = ORIENTED_EDGE ( 'NONE', *, *, #9794, .T. ) ;
#33127 = DIRECTION ( 'NONE',  ( -1.000000000000000000, 0.000000000000000000, 0.000000000000000000 ) ) ;
#33128 = ORIENTED_EDGE ( 'NONE', *, *, #60637, .T. ) ;
#33129 = EDGE_CURVE ( 'NONE', #61044, #32174, #57221, .T. ) ;
#33130 = CYLINDRICAL_SURFACE ( 'NONE', #23285, 12.18650000000000055 ) ;
#33131 = CARTESIAN_POINT ( 'NONE',  ( 35.00000000000000000, -10.01317267707881165, 6.946017217730044990 ) ) ;
#33132 = CARTESIAN_POINT ( 'NONE',  ( -25.00000000000000355, -28.99999999999999645, 5.000000000000000888 ) ) ;
#33133 = VECTOR ( 'NONE', #44006, 1000.000000000000000 ) ;
#33134 = CIRCLE ( 'NONE', #4447, 6.936499999999989896 ) ;
#33135 = ORIENTED_EDGE ( 'NONE', *, *, #2353, .T. ) ;
#33136 = CARTESIAN_POINT ( 'NONE',  ( 2.241352910868910531, -3.889181972941495147, 6.569501556381427854 ) ) ;
#33137 = ORIENTED_EDGE ( 'NONE', *, *, #18551, .F. ) ;
#33138 = DIRECTION ( 'NONE',  ( 0.000000000000000000, 0.01356324068817992175, -0.9999080150203990547 ) ) ;
#33139 = CARTESIAN_POINT ( 'NONE',  ( 9.388378107225753055, 7.267209807330653248, 9.555403925956888145 ) ) ;
#33140 = CARTESIAN_POINT ( 'NONE',  ( -27.08506889328344158, -2.083363953276504255, -0.9597901767753411750 ) ) ;
#33141 = CARTESIAN_POINT ( 'NONE',  ( 2.245754705088393255, 1.435454129948307456, -7.499730934370265167 ) ) ;
#33142 = VERTEX_POINT ( 'NONE', #7063 ) ;
#33143 = CARTESIAN_POINT ( 'NONE',  ( 0.2648978790185593790, 12.08224454301448958, 1.996248716311670446 ) ) ;
#33144 = CARTESIAN_POINT ( 'NONE',  ( 18.90132044483814155, 7.635003998667697189, 11.15574165374908056 ) ) ;
#33145 = CARTESIAN_POINT ( 'NONE',  ( 2.000000000000001776, 0.000000000000000000, 0.000000000000000000 ) ) ;
#33146 = DIRECTION ( 'NONE',  ( 0.000000000000000000, 0.000000000000000000, 1.000000000000000000 ) ) ;
#33147 = EDGE_CURVE ( 'NONE', #46634, #44827, #12047, .T. ) ;
#33148 = CARTESIAN_POINT ( 'NONE',  ( 2.717984159219453133, -3.648459810929832070, 6.886544461123724759 ) ) ;
#33149 = EDGE_CURVE ( 'NONE', #28911, #47012, #25364, .T. ) ;
#33150 = DIRECTION ( 'NONE',  ( 0.000000000000000000, -0.01356324068817998940, 0.9999080150203990547 ) ) ;
#33151 = ORIENTED_EDGE ( 'NONE', *, *, #3241, .F. ) ;
#33152 = CARTESIAN_POINT ( 'NONE',  ( -35.04582288351658548, 0.01270482153514039536, -0.0001464581945180892981 ) ) ;
#33153 = CARTESIAN_POINT ( 'NONE',  ( 0.2646305136544072623, 1.996350543472996675, 12.08286001766536089 ) ) ;
#33154 = CARTESIAN_POINT ( 'NONE',  ( -13.72965000697191584, -27.65230582893893896, -12.05355732046426809 ) ) ;
#33155 = VERTEX_POINT ( 'NONE', #42279 ) ;
#33156 = CARTESIAN_POINT ( 'NONE',  ( -11.38914276748393739, -7.969851211656610701, -8.976043701440310940 ) ) ;
#33157 = DIRECTION ( 'NONE',  ( -1.000000000000000000, 0.000000000000000000, 0.000000000000000000 ) ) ;
#33158 = CARTESIAN_POINT ( 'NONE',  ( -35.00000000000000000, -1.903127969211109383, -11.59095880812010471 ) ) ;
#33159 = B_SPLINE_CURVE_WITH_KNOTS ( 'NONE', 3,
 ( #58886, #36680, #1112, #32899, #31367, #22628, #51672, #8309, #7309, #6113, #58542, #12967, #26372, #23614, #41665, #37906, #13300, #33584 ),
 .UNSPECIFIED., .F., .F.,
 ( 4, 2, 2, 2, 2, 2, 2, 2, 4 ),
 ( 1.309687503460227108E-17, 0.002358234771816867213, 0.003537352157725295616, 0.004716469543633724885, 0.005895586929542152854, 0.007074704315450581690, 0.007664263008404797843, 0.008253821701359013996, 0.009432939087267441097 ),
 .UNSPECIFIED. ) ;
#33160 = EDGE_CURVE ( 'NONE', #34567, #54444, #13361, .T. ) ;
#33161 = AXIS2_PLACEMENT_3D ( 'NONE', #14193, #13851, #3917 ) ;
#33162 = DIRECTION ( 'NONE',  ( 1.000000000000000000, 0.000000000000000000, 0.000000000000000000 ) ) ;
#33163 = CARTESIAN_POINT ( 'NONE',  ( 0.3006302518452027006, -11.43947177966005135, 4.404090606399839736 ) ) ;
#33164 = AXIS2_PLACEMENT_3D ( 'NONE', #23105, #63644, #59670 ) ;
#33165 = VERTEX_POINT ( 'NONE', #33648 ) ;
#33166 = DIRECTION ( 'NONE',  ( -1.000000000000000000, 0.000000000000000000, 0.000000000000000000 ) ) ;
#33167 = EDGE_LOOP ( 'NONE', ( #36040, #9297, #55651, #30720 ) ) ;
#33168 = CARTESIAN_POINT ( 'NONE',  ( 37.00000000000000711, 12.70128625845192794, -1.113475361586537593 ) ) ;
#33169 = CYLINDRICAL_SURFACE ( 'NONE', #40681, 12.75000000000000178 ) ;
#33170 = CARTESIAN_POINT ( 'NONE',  ( 2.305787727787084407, -4.792270232040933386, 5.970480882365206909 ) ) ;
#33171 = DIRECTION ( 'NONE',  ( 1.000000000000000000, 0.000000000000000000, -0.000000000000000000 ) ) ;
#33172 = DIRECTION ( 'NONE',  ( 1.000000000000000000, 0.000000000000000000, -0.000000000000000000 ) ) ;
#33173 = CARTESIAN_POINT ( 'NONE',  ( 2.242819959140784025, 5.782321801516017601, 4.985618132690376569 ) ) ;
#33174 = CARTESIAN_POINT ( 'NONE',  ( 47.00000000000000711, 4.705694406421931860E-17, -3.469127814946512892E-15 ) ) ;
#33175 = EDGE_LOOP ( 'NONE', ( #56279, #9351, #29015, #24027 ) ) ;
#33176 = ADVANCED_FACE ( 'NONE', ( #63901 ), #28332, .T. ) ;
#33177 = EDGE_CURVE ( 'NONE', #63912, #30828, #65678, .T. ) ;
#33178 = EDGE_LOOP ( 'NONE', ( #37393, #50218, #36723, #52552 ) ) ;
#33179 = FACE_OUTER_BOUND ( 'NONE', #18586, .T. ) ;
#33180 = VERTEX_POINT ( 'NONE', #47630 ) ;
#33181 = AXIS2_PLACEMENT_3D ( 'NONE', #41850, #42825, #12244 ) ;
#33182 = EDGE_CURVE ( 'NONE', #55598, #51352, #973, .T. ) ;
#33183 = CARTESIAN_POINT ( 'NONE',  ( -35.00000000000000000, -9.908974237959601084, -6.307491713049132365 ) ) ;
#33184 = CIRCLE ( 'NONE', #4537, 2.899999999999996803 ) ;
#33185 = DIRECTION ( 'NONE',  ( 0.000000000000000000, -0.5155538571770109657, -0.8568571761675956022 ) ) ;
#33186 = CARTESIAN_POINT ( 'NONE',  ( 2.000000000000001776, 6.201547234537035713, 2.820401998297911383 ) ) ;
#33187 = ORIENTED_EDGE ( 'NONE', *, *, #8169, .F. ) ;
#33188 = CARTESIAN_POINT ( 'NONE',  ( 0.3341166715381294616, 5.914486946114060117, -10.74942732659225975 ) ) ;
#33189 = CIRCLE ( 'NONE', #47018, 5.000000000000000888 ) ;
#33190 = CARTESIAN_POINT ( 'NONE',  ( 2.963017218115622242, 1.744728040077008879, -7.679262289252030804 ) ) ;
#33191 = CARTESIAN_POINT ( 'NONE',  ( 2.373367633546872302, -1.511052049479969295, 7.528269033630150098 ) ) ;
#33192 = VERTEX_POINT ( 'NONE', #22344 ) ;
#33193 = VECTOR ( 'NONE', #65167, 1000.000000000000000 ) ;
#33194 = ORIENTED_EDGE ( 'NONE', *, *, #10893, .T. ) ;
#33195 = DIRECTION ( 'NONE',  ( 1.000000000000000000, 0.000000000000000000, 0.000000000000000000 ) ) ;
#33196 = ORIENTED_EDGE ( 'NONE', *, *, #17954, .T. ) ;
#33197 = CARTESIAN_POINT ( 'NONE',  ( 2.247112776671468470, 3.918650674719098337, 6.554209700763984792 ) ) ;
#33198 = VERTEX_POINT ( 'NONE', #28016 ) ;
#33199 = VERTEX_POINT ( 'NONE', #63242 ) ;
#33200 = CARTESIAN_POINT ( 'NONE',  ( 0.2872850955227733150, 4.386654201695149524, 11.44140577127595115 ) ) ;
#33201 = EDGE_CURVE ( 'NONE', #63114, #43224, #42964, .T. ) ;
#33202 = DIRECTION ( 'NONE',  ( -1.000000000000000000, 0.000000000000000000, 0.000000000000000000 ) ) ;
#33203 = CARTESIAN_POINT ( 'NONE',  ( 37.00000000000000711, 5.927257550915316919, -10.64792938439757641 ) ) ;
#33204 = DIRECTION ( 'NONE',  ( -1.000000000000000000, 0.000000000000000000, 0.000000000000000000 ) ) ;
#33205 = CARTESIAN_POINT ( 'NONE',  ( 3.152665057734126197, 7.719888720907812640, 1.848755561852068130 ) ) ;
#33206 = EDGE_CURVE ( 'NONE', #54252, #57333, #25277, .T. ) ;
#33207 = DIRECTION ( 'NONE',  ( 0.000000000000000000, -1.000000000000000000, 0.000000000000000000 ) ) ;
#33208 = VECTOR ( 'NONE', #21861, 1000.000000000000000 ) ;
#33209 = ORIENTED_EDGE ( 'NONE', *, *, #40319, .T. ) ;
#33210 =( BOUNDED_SURFACE ( )  B_SPLINE_SURFACE ( 3, 1, ( 
 ( #37515, #13230 ),
 ( #43466, #2941 ),
 ( #48490, #33517 ),
 ( #13537, #18225 ) ),
 .UNSPECIFIED., .F., .F., .F. ) 
 B_SPLINE_SURFACE_WITH_KNOTS ( ( 4, 4 ),
 ( 2, 2 ),
 ( 0.000000000000000000, 1.000000000000000000 ),
 ( 0.000000000000000000, 1.000000000000000000 ),
 .UNSPECIFIED. ) 
 GEOMETRIC_REPRESENTATION_ITEM ( )  RATIONAL_B_SPLINE_SURFACE ( (
 ( 1.000000000000000000, 1.000000000000000000),
 ( 0.9942764183789327692, 0.8450855930916580938),
 ( 0.9942764183789327692, 0.8450855930916580938),
 ( 1.000000000000000000, 1.000000000000000000) ) ) 
 REPRESENTATION_ITEM ( '' )  SURFACE ( )  );
#33211 = CARTESIAN_POINT ( 'NONE',  ( -2.532614230583026593, 5.020478806276888584, 10.89930238848911337 ) ) ;
#33212 = CARTESIAN_POINT ( 'NONE',  ( 2.963017218115482354, 4.761166637500529042, 6.272673870919030392 ) ) ;
#33213 = CARTESIAN_POINT ( 'NONE',  ( 2.276905613634085057, 3.688905863353115322, -6.697548486791003342 ) ) ;
#33214 = CARTESIAN_POINT ( 'NONE',  ( -14.47334165536100059, 0.000000000000000000, 1.000000000000000000 ) ) ;
#33216 = CARTESIAN_POINT ( 'NONE',  ( -22.65999102136919063, 2.911035239830941368, -3.858590659383841714 ) ) ;
#33215 = VECTOR ( 'NONE', #3833, 1000.000000000000000 ) ;
#33217 = LINE ( 'NONE', #2669, #52034 ) ;
#33218 = CARTESIAN_POINT ( 'NONE',  ( -27.08419797710328325, 1.413289504316736611, 1.803546201758800427 ) ) ;
#33219 = DIRECTION ( 'NONE',  ( -1.000000000000000000, 0.000000000000000000, 0.000000000000000000 ) ) ;
#33220 = VECTOR ( 'NONE', #46927, 1000.000000000000227 ) ;
#33221 = CARTESIAN_POINT ( 'NONE',  ( 3.152665057736217413, -7.923639299008909731, 0.4801242025612903475 ) ) ;
#33222 = CIRCLE ( 'NONE', #60853, 12.18650000000000233 ) ;
#33223 = AXIS2_PLACEMENT_3D ( 'NONE', #60557, #5372, #45274 ) ;
#33224 = ORIENTED_EDGE ( 'NONE', *, *, #24393, .F. ) ;
#33225 = DIRECTION ( 'NONE',  ( 0.000000000000000000, 0.4380125133593973930, -0.8989688749565157844 ) ) ;
#33226 = ORIENTED_EDGE ( 'NONE', *, *, #28406, .F. ) ;
#33227 = CARTESIAN_POINT ( 'NONE',  ( 35.00000000000000000, 7.376655759824880754, -9.700295462048687867 ) ) ;
#33228 = CARTESIAN_POINT ( 'NONE',  ( 2.241534463349551753, 9.451863027432619807E-16, 7.634462073473348376 ) ) ;
#33229 = DIRECTION ( 'NONE',  ( 0.000000000000000000, 0.01356324068817998940, -0.9999080150203989437 ) ) ;
#33230 = CARTESIAN_POINT ( 'NONE',  ( 0.2652384529303126182, 9.423437232855667034, 7.820949643217174341 ) ) ;
#33231 = CARTESIAN_POINT ( 'NONE',  ( 2.705197763288547996, -4.789125516644078040, -6.142723737672437068 ) ) ;
#33232 = ORIENTED_EDGE ( 'NONE', *, *, #50486, .T. ) ;
#33233 = CIRCLE ( 'NONE', #6712, 12.18650000000000055 ) ;
#33234 = DIRECTION ( 'NONE',  ( -1.000000000000000000, 0.000000000000000000, 0.000000000000000000 ) ) ;
#33235 = CARTESIAN_POINT ( 'NONE',  ( 0.000000000000000000, -2.480520636974233639, 6.345145617221206180 ) ) ;
#33236 = CARTESIAN_POINT ( 'NONE',  ( -18.23022800145057687, -13.26592958674785194, 2.588920604642957368 ) ) ;
#33237 = CARTESIAN_POINT ( 'NONE',  ( 0.2651627682582914369, -2.213224986694501517, -12.04449770099953554 ) ) ;
#33238 = CIRCLE ( 'NONE', #7752, 6.936499999999989896 ) ;
#33239 = EDGE_CURVE ( 'NONE', #12285, #31390, #35975, .T. ) ;
#33240 = CARTESIAN_POINT ( 'NONE',  ( 0.000000000000000000, -30.00000000000000000, 0.000000000000000000 ) ) ;
#33241 = ORIENTED_EDGE ( 'NONE', *, *, #9664, .T. ) ;
#33242 = AXIS2_PLACEMENT_3D ( 'NONE', #51630, #46616, #60938 ) ;
#33243 = CARTESIAN_POINT ( 'NONE',  ( 2.717984159219154261, -0.2836133496099048079, -7.788152353088992896 ) ) ;
#33244 = CARTESIAN_POINT ( 'NONE',  ( -22.27834755396593991, -1.162947663292857037, 3.497967921180562101 ) ) ;
#33245 = CARTESIAN_POINT ( 'NONE',  ( 2.266490820343227242, -3.946561086901428261, -6.544980046121064099 ) ) ;
#33246 = ADVANCED_FACE ( 'NONE', ( #3418 ), #48190, .F. ) ;
#33247 = AXIS2_PLACEMENT_3D ( 'NONE', #64583, #59628, #34655 ) ;
#33248 = EDGE_LOOP ( 'NONE', ( #8012, #42716, #11545, #35752 ) ) ;
#33249 = CARTESIAN_POINT ( 'NONE',  ( 9.779306477119707353, 6.953054007709951634, -9.784907511924334500 ) ) ;
#33250 = ORIENTED_EDGE ( 'NONE', *, *, #64253, .T. ) ;
#33251 = CARTESIAN_POINT ( 'NONE',  ( 2.263328370261315836, 5.019946231381084978, 5.761609105518099128 ) ) ;
#33252 = CARTESIAN_POINT ( 'NONE',  ( 2.705197763288545776, -3.649695155981463657, -6.881024880055383264 ) ) ;
#33253 = CARTESIAN_POINT ( 'NONE',  ( 32.73308617475132820, -2.903166307960730830, 22.77405829473931576 ) ) ;
#33254 = CARTESIAN_POINT ( 'NONE',  ( 5.520433897694421610, 0.007082458259338569526, -0.01329351892498007413 ) ) ;
#33255 = CARTESIAN_POINT ( 'NONE',  ( -27.27855387000350262, 25.00000000000000000, 5.631341004100471892 ) ) ;
#33256 = ORIENTED_EDGE ( 'NONE', *, *, #36005, .F. ) ;
#33257 = EDGE_CURVE ( 'NONE', #6726, #19811, #38068, .T. ) ;
#33258 = CIRCLE ( 'NONE', #24770, 12.18650000000000055 ) ;
#33259 = CIRCLE ( 'NONE', #4618, 12.73084802173761787 ) ;
#33260 = ORIENTED_EDGE ( 'NONE', *, *, #16255, .T. ) ;
#33261 = ORIENTED_EDGE ( 'NONE', *, *, #49184, .F. ) ;
#33262 = CARTESIAN_POINT ( 'NONE',  ( 5.515188684475870851, -0.004893136156457767935, -0.002166413411657401155 ) ) ;
#33263 = EDGE_CURVE ( 'NONE', #6580, #31041, #64153, .T. ) ;
#33264 = AXIS2_PLACEMENT_3D ( 'NONE', #45018, #44664, #8792 ) ;
#33266 = CIRCLE ( 'NONE', #38584, 12.18650000000000055 ) ;
#33265 = DIRECTION ( 'NONE',  ( -1.000000000000000000, 0.000000000000000000, 0.000000000000000000 ) ) ;
#33267 = ORIENTED_EDGE ( 'NONE', *, *, #49265, .F. ) ;
#33268 = DIRECTION ( 'NONE',  ( 0.000000000000000000, 0.000000000000000000, 1.000000000000000000 ) ) ;
#33269 = CARTESIAN_POINT ( 'NONE',  ( 2.259830038565000976, -7.547174990768408698, 1.190932096469625279 ) ) ;
#33270 = ORIENTED_EDGE ( 'NONE', *, *, #61213, .F. ) ;
#33271 = CARTESIAN_POINT ( 'NONE',  ( -23.41523303002442091, 2.683951991546301930, -3.856096202952854046 ) ) ;
#33272 = DIRECTION ( 'NONE',  ( 0.000000000000000000, 0.000000000000000000, 1.000000000000000000 ) ) ;
#33273 = DIRECTION ( 'NONE',  ( -1.000000000000000000, 0.000000000000000000, -0.000000000000000000 ) ) ;
#33274 = ORIENTED_EDGE ( 'NONE', *, *, #56123, .F. ) ;
#33275 = VECTOR ( 'NONE', #65277, 1000.000000000000000 ) ;
#33276 = ORIENTED_EDGE ( 'NONE', *, *, #17950, .T. ) ;
#33277 = DIRECTION ( 'NONE',  ( 0.000000000000000000, -0.3218879778915842427, 0.9467777615094616905 ) ) ;
#33278 = ORIENTED_EDGE ( 'NONE', *, *, #21231, .T. ) ;
#33279 = CARTESIAN_POINT ( 'NONE',  ( -20.79170840334646542, 11.34110549087207076, -3.921648409140116698 ) ) ;
#33280 = VERTEX_POINT ( 'NONE', #24657 ) ;
#33281 = VECTOR ( 'NONE', #56463, 1000.000000000000114 ) ;
#33282 = CARTESIAN_POINT ( 'NONE',  ( 2.990245332647870402, 6.814589384235040015, -5.049055049623153657 ) ) ;
#33283 = CARTESIAN_POINT ( 'NONE',  ( -37.00000000000000711, -10.39746860227885428, -7.379373053628982326 ) ) ;
#33284 = EDGE_CURVE ( 'NONE', #14592, #58711, #42331, .T. ) ;
#33285 = AXIS2_PLACEMENT_3D ( 'NONE', #46425, #52416, #27129 ) ;
#33286 = CARTESIAN_POINT ( 'NONE',  ( -35.04643116707788408, 0.003844232202716499347, -0.01156612771644957571 ) ) ;
#33287 = CARTESIAN_POINT ( 'NONE',  ( -22.28284753389937123, 3.581493264753388139, 0.9231250029034783200 ) ) ;
#33288 = CARTESIAN_POINT ( 'NONE',  ( 1.459561108994998246, 11.65083230253685009, -4.912799202120054609 ) ) ;
#33289 = CARTESIAN_POINT ( 'NONE',  ( 3.152665057734040488, 0.000000000000000000, 0.000000000000000000 ) ) ;
#33290 = CARTESIAN_POINT ( 'NONE',  ( 5.014783254242184185, -9.842758936301256867, -6.866372042166331013 ) ) ;
#33291 = ORIENTED_EDGE ( 'NONE', *, *, #56996, .F. ) ;
#33292 = CYLINDRICAL_SURFACE ( 'NONE', #41779, 12.18649999999999878 ) ;
#33293 = AXIS2_PLACEMENT_3D ( 'NONE', #65315, #29412, #35027 ) ;
#33294 = ORIENTED_EDGE ( 'NONE', *, *, #50102, .F. ) ;
#33295 = CARTESIAN_POINT ( 'NONE',  ( 2.258463476536644698, -2.740340677911279776, 7.131741622455330720 ) ) ;
#33296 = CIRCLE ( 'NONE', #64094, 5.000000000000000888 ) ;
#33297 = CARTESIAN_POINT ( 'NONE',  ( 0.3665391374699465965, -12.04754782681758662, 2.392238720110418715 ) ) ;
#33298 = VERTEX_POINT ( 'NONE', #9668 ) ;
#33299 = CARTESIAN_POINT ( 'NONE',  ( 3.152665057736161902, 7.719888720907650992, -1.848755561854025231 ) ) ;
#33300 = CARTESIAN_POINT ( 'NONE',  ( 0.3006302518452026451, 12.03044280705497648, -2.350739146140467195 ) ) ;
#33301 = CARTESIAN_POINT ( 'NONE',  ( 2.368238019615056533, -7.526794520527601229, 1.509700170844538558 ) ) ;
#33303 = EDGE_CURVE ( 'NONE', #25961, #63874, #8713, .T. ) ;
#33302 = EDGE_LOOP ( 'NONE', ( #13376, #54876, #55551, #55670 ) ) ;
#33304 = CIRCLE ( 'NONE', #10998, 5.000000000000000000 ) ;
#33305 = ORIENTED_EDGE ( 'NONE', *, *, #61526, .F. ) ;
#33306 = DIRECTION ( 'NONE',  ( 0.4826047536471247956, 0.8758382566188793739, -0.000000000000000000 ) ) ;
#33307 = ORIENTED_EDGE ( 'NONE', *, *, #32590, .F. ) ;
#33308 = CARTESIAN_POINT ( 'NONE',  ( 0.000000000000000000, 6.883677378339481123, -0.8544109087185395301 ) ) ;
#33309 = CARTESIAN_POINT ( 'NONE',  ( -3.673220185152842099, -7.076978035560978597, 9.701075964846328503 ) ) ;
#33310 = CARTESIAN_POINT ( 'NONE',  ( -29.90001358305153545, 1.049925265473337754, 13.46092060699443671 ) ) ;
#33311 = CARTESIAN_POINT ( 'NONE',  ( 0.3401186441510238856, -9.233880480307249172, -8.081824149807792068 ) ) ;
#33312 = DIRECTION ( 'NONE',  ( -1.000000000000000000, -0.000000000000000000, 0.000000000000000000 ) ) ;
#33313 = ORIENTED_EDGE ( 'NONE', *, *, #33545, .T. ) ;
#33314 = AXIS2_PLACEMENT_3D ( 'NONE', #54318, #12404, #53666 ) ;
#33315 = CARTESIAN_POINT ( 'NONE',  ( 3.152665057734040488, 0.000000000000000000, 0.000000000000000000 ) ) ;
#33316 = ADVANCED_FACE ( 'NONE', ( #49608 ), #23102, .F. ) ;
#33317 = CARTESIAN_POINT ( 'NONE',  ( 18.81741048081454082, -29.91393404465042138, -6.911695701493956179 ) ) ;
#33318 = AXIS2_PLACEMENT_3D ( 'NONE', #39781, #60070, #30132 ) ;
#33319 = VECTOR ( 'NONE', #62176, 1000.000000000000000 ) ;
#33320 = CARTESIAN_POINT ( 'NONE',  ( 5.516018279890452902, 0.004180585980734981624, 0.005331956019561726046 ) ) ;
#33321 = CARTESIAN_POINT ( 'NONE',  ( 0.3665391374699472626, -1.872534962004881454, 12.13918562134718115 ) ) ;
#33322 = PRODUCT ( 'BR-837', 'BR-837', '', ( #7495 ) ) ;
#33323 = ADVANCED_FACE ( 'NONE', ( #34294 ), #54273, .T. ) ;
#33324 = CARTESIAN_POINT ( 'NONE',  ( 0.2652384770603670727, 7.820955051613327491, 9.423432754625759245 ) ) ;
#33325 = CARTESIAN_POINT ( 'NONE',  ( 7.137737543050354461, -4.955906025390103942, -10.93869909733096613 ) ) ;
#33326 = FACE_OUTER_BOUND ( 'NONE', #55252, .T. ) ;
#33327 = AXIS2_PLACEMENT_3D ( 'NONE', #50427, #13509, #14166 ) ;
#33328 = AXIS2_PLACEMENT_3D ( 'NONE', #27689, #58298, #32350 ) ;
#33329 = ADVANCED_FACE ( 'NONE', ( #4386 ), #38965, .T. ) ;
#33330 = EDGE_LOOP ( 'NONE', ( #17621, #1812, #44713, #46664 ) ) ;
#33331 = CARTESIAN_POINT ( 'NONE',  ( 12.90521571632873865, -10.89702685051559072, -5.029477694709124869 ) ) ;
#33332 = ORIENTED_EDGE ( 'NONE', *, *, #44705, .T. ) ;
#33333 = CARTESIAN_POINT ( 'NONE',  ( 35.00000000000000000, 4.705694406421931860E-17, -3.469127814946512892E-15 ) ) ;
#33334 = DIRECTION ( 'NONE',  ( -1.000000000000000000, -0.000000000000000000, -0.000000000000000000 ) ) ;
#33335 = DIRECTION ( 'NONE',  ( 1.000000000000000000, -0.000000000000000000, 0.000000000000000000 ) ) ;
#33336 = VECTOR ( 'NONE', #64041, 1000.000000000000000 ) ;
#33337 = ORIENTED_EDGE ( 'NONE', *, *, #30056, .F. ) ;
#33338 = CARTESIAN_POINT ( 'NONE',  ( 2.255723233589907117, 6.548644987607097789, 3.933511348458858858 ) ) ;
#33339 = ORIENTED_EDGE ( 'NONE', *, *, #42888, .T. ) ;
#33340 = EDGE_CURVE ( 'NONE', #10069, #6941, #64540, .T. ) ;
#33341 = CARTESIAN_POINT ( 'NONE',  ( -37.25000000000000711, -20.00000000000000000, 2.449293598294706907E-15 ) ) ;
#33342 = ORIENTED_EDGE ( 'NONE', *, *, #6773, .F. ) ;
#33343 = VERTEX_POINT ( 'NONE', #4047 ) ;
#33344 = CARTESIAN_POINT ( 'NONE',  ( -10.90165637462999726, -7.721945941999268648, -9.189455070444248364 ) ) ;
#33345 = CARTESIAN_POINT ( 'NONE',  ( -22.38932658256920405, 0.2254938976656722660, 4.011828264158250335 ) ) ;
#33346 = AXIS2_PLACEMENT_3D ( 'NONE', #16689, #1420, #36961 ) ;
#33347 = VERTEX_POINT ( 'NONE', #45262 ) ;
#33348 = EDGE_CURVE ( 'NONE', #1474, #58929, #50594, .T. ) ;
#33349 = CARTESIAN_POINT ( 'NONE',  ( 35.00000000000000000, 5.246972444134017977, -10.99909370905159101 ) ) ;
#33350 = CARTESIAN_POINT ( 'NONE',  ( 3.990895163589245787, 6.918992358595912329, 11.62617458216422861 ) ) ;
#33351 = DIRECTION ( 'NONE',  ( -0.000000000000000000, -0.000000000000000000, -1.000000000000000000 ) ) ;
#33352 = DIRECTION ( 'NONE',  ( -1.000000000000000000, -0.000000000000000000, 0.000000000000000000 ) ) ;
#33353 = EDGE_LOOP ( 'NONE', ( #28680, #57770, #16956, #8326 ) ) ;
#33354 = CARTESIAN_POINT ( 'NONE',  ( 0.2739690278137230095, -7.732471127692660318, 9.499928778897087867 ) ) ;
#33355 = DIRECTION ( 'NONE',  ( -1.000000000000000000, 0.000000000000000000, 0.000000000000000000 ) ) ;
#33356 = CARTESIAN_POINT ( 'NONE',  ( -35.00000000000000000, 2.905556151562625811, 11.38112321385051651 ) ) ;
#33358 = ORIENTED_EDGE ( 'NONE', *, *, #48799, .F. ) ;
#33357 = CARTESIAN_POINT ( 'NONE',  ( -26.97113089360557225, 10.82592580676787186, 5.176981052598353727 ) ) ;
#33359 = DIRECTION ( 'NONE',  ( 0.000000000000000000, -0.8169148498130339719, 0.5767582926624881257 ) ) ;
#33360 = VERTEX_POINT ( 'NONE', #13680 ) ;
#33361 = CIRCLE ( 'NONE', #30171, 5.000000000000000000 ) ;
#33362 = CARTESIAN_POINT ( 'NONE',  ( -20.56770621847863723, 13.00092155042986519, -3.647989838260398798 ) ) ;
#33363 = CIRCLE ( 'NONE', #28054, 5.000000000000000888 ) ;
#33364 = ORIENTED_EDGE ( 'NONE', *, *, #56850, .T. ) ;
#33365 = FACE_OUTER_BOUND ( 'NONE', #38432, .T. ) ;
#33366 = DIRECTION ( 'NONE',  ( -1.000000000000000000, 0.000000000000000000, 0.000000000000000000 ) ) ;
#33367 = FACE_OUTER_BOUND ( 'NONE', #24348, .T. ) ;
#33368 = DIRECTION ( 'NONE',  ( 0.000000000000000000, 0.9796553971857749898, 0.2006870767258855104 ) ) ;
#33369 = CARTESIAN_POINT ( 'NONE',  ( -5.792881964653834537, -1.480264921545251688, -13.41892255734878958 ) ) ;
#33370 = CARTESIAN_POINT ( 'NONE',  ( -22.29978294495153435, -3.642708310327671395, -0.8878583829805674066 ) ) ;
#33371 = ORIENTED_EDGE ( 'NONE', *, *, #65711, .F. ) ;
#33372 = DIRECTION ( 'NONE',  ( 1.000000000000000000, 0.000000000000000000, 0.000000000000000000 ) ) ;
#33373 = VERTEX_POINT ( 'NONE', #44271 ) ;
#33374 = ORIENTED_EDGE ( 'NONE', *, *, #58350, .T. ) ;
#33375 = AXIS2_PLACEMENT_3D ( 'NONE', #11771, #7122, #6160 ) ;
#33376 = DIRECTION ( 'NONE',  ( -1.000000000000000000, 0.000000000000000000, 0.000000000000000000 ) ) ;
#33377 = CARTESIAN_POINT ( 'NONE',  ( -22.27786964138239867, 3.347945419004161760, 1.536369256421326490 ) ) ;
#33378 = CARTESIAN_POINT ( 'NONE',  ( 5.530133899448235191, -0.01589823604557702441, 0.001661287012793988965 ) ) ;
#33379 = CARTESIAN_POINT ( 'NONE',  ( -22.27945548916780183, 2.122548946923926483, 3.016427163003885248 ) ) ;
#33380 = CARTESIAN_POINT ( 'NONE',  ( 35.00000000000000000, -9.348667969174460524, -7.817492529713823579 ) ) ;
#33382 = AXIS2_PLACEMENT_3D ( 'NONE', #42189, #16943, #2322 ) ;
#33381 = AXIS2_PLACEMENT_3D ( 'NONE', #17780, #42696, #37731 ) ;
#33383 = EDGE_CURVE ( 'NONE', #19254, #21572, #15020, .T. ) ;
#33384 = CARTESIAN_POINT ( 'NONE',  ( 37.00000000000000711, 4.705694406421931860E-17, -3.469127814946512892E-15 ) ) ;
#33385 = CARTESIAN_POINT ( 'NONE',  ( 35.00000000000000000, 5.556331110570566167, 11.47561260193570654 ) ) ;
#33386 = EDGE_LOOP ( 'NONE', ( #11169, #65483, #45521, #56874 ) ) ;
#33387 = VECTOR ( 'NONE', #55023, 1000.000000000000000 ) ;
#33388 = DIRECTION ( 'NONE',  ( -1.000000000000000000, 0.000000000000000000, 0.000000000000000000 ) ) ;
#33389 = CARTESIAN_POINT ( 'NONE',  ( -37.00000000000000711, 0.000000000000000000, 0.000000000000000000 ) ) ;
#33390 = LINE ( 'NONE', #59319, #21131 ) ;
#33391 = CARTESIAN_POINT ( 'NONE',  ( -35.00000000000000000, -9.821084925794513865, -7.215058775251364409 ) ) ;
#33392 = CARTESIAN_POINT ( 'NONE',  ( 47.00000000000000711, 4.705694406421931860E-17, -3.469127814946512892E-15 ) ) ;
#33393 = AXIS2_PLACEMENT_3D ( 'NONE', #4617, #54497, #29521 ) ;
#33394 = EDGE_CURVE ( 'NONE', #58530, #12917, #60257, .T. ) ;
#33395 =( BOUNDED_SURFACE ( )  B_SPLINE_SURFACE ( 3, 1, ( 
 ( #30005, #25033 ),
 ( #4431, #25344 ),
 ( #24701, #39982 ),
 ( #61248, #30344 ) ),
 .UNSPECIFIED., .F., .F., .F. ) 
 B_SPLINE_SURFACE_WITH_KNOTS ( ( 4, 4 ),
 ( 2, 2 ),
 ( 0.000000000000000000, 1.000000000000000000 ),
 ( 0.000000000000000000, 1.000000000000000000 ),
 .UNSPECIFIED. ) 
 GEOMETRIC_REPRESENTATION_ITEM ( )  RATIONAL_B_SPLINE_SURFACE ( (
 ( 1.000000000000000000, 1.000000000000000000),
 ( 0.9856612449720755231, 0.9999558406602322425),
 ( 0.9856612449720755231, 0.9999558406602322425),
 ( 1.000000000000000000, 1.000000000000000000) ) ) 
 REPRESENTATION_ITEM ( '' )  SURFACE ( )  );
#33396 = CARTESIAN_POINT ( 'NONE',  ( -11.06236561744495717, -5.410674147974703807, 12.37007031003713742 ) ) ;
#33397 = EDGE_CURVE ( 'NONE', #62269, #55569, #57215, .T. ) ;
#33398 = CARTESIAN_POINT ( 'NONE',  ( 2.000000000000001776, 2.664846396702580833, -6.404188155572981600 ) ) ;
#33399 = EDGE_CURVE ( 'NONE', #43107, #51107, #31285, .T. ) ;
#33400 = VERTEX_POINT ( 'NONE', #31915 ) ;
#33401 = CARTESIAN_POINT ( 'NONE',  ( -47.00000000000000711, 0.000000000000000000, 0.000000000000000000 ) ) ;
#33402 = AXIS2_PLACEMENT_3D ( 'NONE', #54705, #19110, #53718 ) ;
#33403 = DIRECTION ( 'NONE',  ( 0.000000000000000000, -0.3807014730195286134, 0.9246979985058695339 ) ) ;
#33404 = CARTESIAN_POINT ( 'NONE',  ( 0.000000000000000000, -4.409940824963369366, -5.354199675985328533 ) ) ;
#33405 = ADVANCED_FACE ( 'NONE', ( #25300 ), #25633, .T. ) ;
#33406 = CARTESIAN_POINT ( 'NONE',  ( -28.66013792860432119, -1.289369452666810467, -1.306994062650345567 ) ) ;
#33407 = DIRECTION ( 'NONE',  ( -1.000000000000000000, 0.000000000000000000, 0.000000000000000000 ) ) ;
#33408 = AXIS2_PLACEMENT_3D ( 'NONE', #60706, #16128, #31098 ) ;
#33409 = ORIENTED_EDGE ( 'NONE', *, *, #43132, .F. ) ;
#33410 = CARTESIAN_POINT ( 'NONE',  ( 5.520433897694421610, 0.01505375422439122861, -0.0005131706886598833180 ) ) ;
#33411 = EDGE_CURVE ( 'NONE', #60515, #55740, #36597, .T. ) ;
#33412 = CARTESIAN_POINT ( 'NONE',  ( 2.258463476536300973, -4.806099079317786682, -5.939075453322352871 ) ) ;
#33413 = CARTESIAN_POINT ( 'NONE',  ( -35.04582288351658548, 0.008224400713785747288, -0.009684687560357898087 ) ) ;
#33414 = ORIENTED_EDGE ( 'NONE', *, *, #13930, .F. ) ;
#33415 = DIRECTION ( 'NONE',  ( 1.000000000000000000, 0.000000000000000000, 0.000000000000000000 ) ) ;
#33416 = LINE ( 'NONE', #53381, #30930 ) ;
#33417 = VERTEX_POINT ( 'NONE', #35604 ) ;
#33418 = ORIENTED_EDGE ( 'NONE', *, *, #40123, .T. ) ;
#33419 = CYLINDRICAL_SURFACE ( 'NONE', #35247, 12.18650000000000055 ) ;
#33420 = EDGE_CURVE ( 'NONE', #5624, #53395, #40596, .T. ) ;
#33421 = B_SPLINE_CURVE_WITH_KNOTS ( 'NONE', 3,
 ( #12302, #32572, #52576, #38571, #59195, #42898, #33252, #43543, #44209, #28925, #29252, #8312, #28587, #63183, #53560, #63825 ),
 .UNSPECIFIED., .F., .F.,
 ( 4, 3, 3, 3, 3, 4 ),
 ( 0.000000000000000000, 0.0002176109881720231839, 0.0004352086762394577393, 0.0006528017811446839300, 0.0007615147961451657717, 0.0009453342004947017183 ),
 .UNSPECIFIED. ) ;
#33422 = CIRCLE ( 'NONE', #38740, 12.74999999999999822 ) ;
#33423 = ORIENTED_EDGE ( 'NONE', *, *, #10118, .F. ) ;
#33424 = ADVANCED_FACE ( 'NONE', ( #50915 ), #25234, .F. ) ;
#33425 = CARTESIAN_POINT ( 'NONE',  ( 2.000000000000001776, 5.888698556700773246, 3.665823448873418045 ) ) ;
#33426 = DIRECTION ( 'NONE',  ( 0.000000000000000000, -0.01356324068817991828, 0.9999080150203990547 ) ) ;
#33427 = CARTESIAN_POINT ( 'NONE',  ( 2.241506898688417682, 7.511570207700577484, -1.364429914801440491 ) ) ;
#33428 = CARTESIAN_POINT ( 'NONE',  ( 2.266490820343225909, -7.550546162186916099, -1.183790889241807420 ) ) ;
#33429 = DIRECTION ( 'NONE',  ( -1.000000000000000000, 0.000000000000000000, 0.000000000000000000 ) ) ;
#33430 = EDGE_CURVE ( 'NONE', #1946, #54776, #14708, .T. ) ;
#33431 = DIRECTION ( 'NONE',  ( -1.000000000000000000, 0.000000000000000000, 0.000000000000000000 ) ) ;
#33433 = ORIENTED_EDGE ( 'NONE', *, *, #48878, .T. ) ;
#33432 = CARTESIAN_POINT ( 'NONE',  ( 1.372161826076019109, 0.5897614319402071370, 12.60140585080791631 ) ) ;
#33434 = CARTESIAN_POINT ( 'NONE',  ( -47.00000000000000711, 0.000000000000000000, 0.000000000000000000 ) ) ;
#33435 = VERTEX_POINT ( 'NONE', #45926 ) ;
#33436 = CARTESIAN_POINT ( 'NONE',  ( 35.00000000000000000, -9.700295462048712736, -7.376655759824850556 ) ) ;
#33437 = ORIENTED_EDGE ( 'NONE', *, *, #49628, .F. ) ;
#33438 = B_SPLINE_CURVE_WITH_KNOTS ( 'NONE', 3,
 ( #47036, #56340, #6465, #31404, #10786, #26743, #31708, #61994, #56011, #46055, #5836, #506, #20444, #21772, #25425, #45707, #41702, #31072, #51384, #52018, #1495, #51705 ),
 .UNSPECIFIED., .F., .F.,
 ( 4, 3, 3, 3, 3, 3, 3, 4 ),
 ( 1.311167604876506724E-18, 4.449119708436815798E-05, 6.626296329540360547E-05, 8.803456484962558695E-05, 0.0001098060367612788341, 0.0001315774408628489034, 0.0001760698110411144739, 0.0001829697163287813692 ),
 .UNSPECIFIED. ) ;
#33439 = ORIENTED_EDGE ( 'NONE', *, *, #38652, .T. ) ;
#33440 = CARTESIAN_POINT ( 'NONE',  ( -25.86628395826706850, 8.041618865309581921, 10.84354029019568522 ) ) ;
#33441 = CARTESIAN_POINT ( 'NONE',  ( -0.5153900578009965594, -26.55329395651783031, 16.22445808467987050 ) ) ;
#33442 = CARTESIAN_POINT ( 'NONE',  ( -25.73422511961580028, 12.22591596592855190, 5.729065348228939314 ) ) ;
#33443 = CIRCLE ( 'NONE', #31350, 4.999999999999998224 ) ;
#33444 = DIRECTION ( 'NONE',  ( 0.000000000000000000, 0.000000000000000000, 1.000000000000000000 ) ) ;
#33445 = CARTESIAN_POINT ( 'NONE',  ( -39.62372872010315916, -1.894461972532858196, -19.09391518418255629 ) ) ;
#33446 = DIRECTION ( 'NONE',  ( -0.000000000000000000, -0.000000000000000000, -1.000000000000000000 ) ) ;
#33447 = VERTEX_POINT ( 'NONE', #378 ) ;
#33448 = CARTESIAN_POINT ( 'NONE',  ( -22.27718112499583469, 0.5110808820053616142, 3.645895996548640383 ) ) ;
#33449 = CARTESIAN_POINT ( 'NONE',  ( 0.9232167919969134218, -3.872606616958349957, 11.84868134597555489 ) ) ;
#33450 = CARTESIAN_POINT ( 'NONE',  ( 3.152665057734040488, 0.000000000000000000, 0.000000000000000000 ) ) ;
#33452 = ORIENTED_EDGE ( 'NONE', *, *, #33760, .T. ) ;
#33451 = B_SPLINE_CURVE_WITH_KNOTS ( 'NONE', 3,
 ( #24403, #50363, #29711, #40023, #4810, #8463, #25076, #34049, #59336, #29086, #18782, #19766, #44351, #49393, #14097, #38730, #4137, #45025, #9764 ),
 .UNSPECIFIED., .F., .F.,
 ( 4, 3, 3, 3, 3, 3, 4 ),
 ( 9.120196284301400213E-18, 4.457896483014723308E-05, 6.639290541541900085E-05, 8.820687556478805976E-05, 0.0001100173248778910014, 0.0001545671401658117229, 0.0001830328308068583328 ),
 .UNSPECIFIED. ) ;
#33453 = LINE ( 'NONE', #13173, #42769 ) ;
#33454 = B_SPLINE_CURVE_WITH_KNOTS ( 'NONE', 3,
 ( #29751, #5171, #25120, #515, #14461, #25436, #65653, #30098, #14776, #55713, #15123, #10797, #50406, #35060, #5847, #26107, #10147, #4523, #24793, #15459, #20122, #19806, #60692, #10462, #40062, #51397, #36049, #46069, #60351, #50064, #56349, #30425 ),
 .UNSPECIFIED., .F., .F.,
 ( 4, 2, 2, 2, 2, 2, 2, 2, 2, 2, 2, 2, 2, 2, 2, 4 ),
 ( 1.941418318260282306E-17, 0.003213204025811739785, 0.004819806038717596233, 0.006426408051623453549, 0.008033010064529310865, 0.009639612077435168180, 0.01124621409034102550, 0.01204951509679395329, 0.01285281610324688281, 0.01606602012905859744, 0.01927922415487031207, 0.02008252516132323987, 0.02088582616777616766, 0.02249242818068202671, 0.02409903019358788576, 0.02570563220649374828 ),
 .UNSPECIFIED. ) ;
#33455 =( GEOMETRIC_REPRESENTATION_CONTEXT ( 3 ) GLOBAL_UNCERTAINTY_ASSIGNED_CONTEXT ( ( #42977 ) ) GLOBAL_UNIT_ASSIGNED_CONTEXT ( ( #58470, #53144, #2286 ) ) REPRESENTATION_CONTEXT ( 'NONE', 'WORKASPACE' ) );
#33456 = VERTEX_POINT ( 'NONE', #51905 ) ;
#33457 = DIRECTION ( 'NONE',  ( 0.000000000000000000, 0.01356324068817992175, -0.9999080150203990547 ) ) ;
#33458 = CARTESIAN_POINT ( 'NONE',  ( 3.152665057736074417, -6.622010822085853121, 4.377619405894153992 ) ) ;
#33459 = B_SPLINE_CURVE_WITH_KNOTS ( 'NONE', 3,
 ( #57700, #47396, #11460, #52384, #47707, #53360, #52046, #32065, #58023, #42354, #57037, #47065, #6491 ),
 .UNSPECIFIED., .F., .F.,
 ( 4, 3, 3, 3, 4 ),
 ( 2.602085213965210642E-18, 6.607593386745516130E-05, 0.0001321518677373524609, 0.0001982171734706215916, 0.0002642860854759484460 ),
 .UNSPECIFIED. ) ;
#33460 = CYLINDRICAL_SURFACE ( 'NONE', #12943, 6.095312090839646757 ) ;
#33461 = FACE_OUTER_BOUND ( 'NONE', #31599, .T. ) ;
#33462 = ADVANCED_FACE ( 'NONE', ( #20657 ), #54593, .F. ) ;
#33463 = ADVANCED_FACE ( 'NONE', ( #35911 ), #51256, .T. ) ;
#33464 = DIRECTION ( 'NONE',  ( -0.9582930651793754029, -0.2067888154783181776, -0.1972632429577070579 ) ) ;
#33465 = DIRECTION ( 'NONE',  ( 0.000000000000000000, -0.9718671068226434340, 0.2355298848897617037 ) ) ;
#33466 = CYLINDRICAL_SURFACE ( 'NONE', #38655, 5.000000000000000000 ) ;
#33467 = ORIENTED_EDGE ( 'NONE', *, *, #3021, .F. ) ;
#33468 = CARTESIAN_POINT ( 'NONE',  ( -17.87891481078355227, 12.92455976930240524, 3.899497271525859787 ) ) ;
#33469 = EDGE_LOOP ( 'NONE', ( #27230, #58814, #57740, #996 ) ) ;
#33470 = DIRECTION ( 'NONE',  ( 0.000000000000000000, 0.01356324068817998940, -0.9999080150203990547 ) ) ;
#33471 = CARTESIAN_POINT ( 'NONE',  ( 2.524535260912817769, 4.796565674004647839, -6.060306679219011450 ) ) ;
#33472 = EDGE_CURVE ( 'NONE', #53899, #40556, #46261, .T. ) ;
#33473 = CARTESIAN_POINT ( 'NONE',  ( 0.2653519890518140634, -11.50766430042467370, -4.188437879978375022 ) ) ;
#33474 = CIRCLE ( 'NONE', #541, 5.000000000000000888 ) ;
#33475 = CARTESIAN_POINT ( 'NONE',  ( -35.00000000000000000, -10.75351884295731253, 4.725891942574718563 ) ) ;
#33476 = ADVANCED_FACE ( 'NONE', ( #56901 ), #6346, .T. ) ;
#33477 = CARTESIAN_POINT ( 'NONE',  ( 5.536195898058073439, 0.0002547682446685005180, 0.008496323383586770056 ) ) ;
#33478 = EDGE_LOOP ( 'NONE', ( #11309, #11285, #34851, #52758 ) ) ;
#33479 = DIRECTION ( 'NONE',  ( -1.000000000000000000, 0.000000000000000000, 0.000000000000000000 ) ) ;
#33480 = CARTESIAN_POINT ( 'NONE',  ( 0.3040950598368144520, 11.60568999039900362, -3.956873563689416784 ) ) ;
#33481 = CARTESIAN_POINT ( 'NONE',  ( -37.00000000000000711, 2.905556151562625811, 11.38112321385051651 ) ) ;
#33482 = CARTESIAN_POINT ( 'NONE',  ( 37.00000000000000711, 4.705694406421931860E-17, -3.469127814946512892E-15 ) ) ;
#33483 = ADVANCED_FACE ( 'NONE', ( #47888 ), #38561, .T. ) ;
#33484 = ORIENTED_EDGE ( 'NONE', *, *, #29588, .F. ) ;
#33485 = CARTESIAN_POINT ( 'NONE',  ( 2.305787727787084407, -5.970480882365190034, -4.792270232040956479 ) ) ;
#33486 = CARTESIAN_POINT ( 'NONE',  ( -22.28169757117798966, -2.592369810060387803, 2.633129923220808077 ) ) ;
#33487 = CARTESIAN_POINT ( 'NONE',  ( 0.2652384770603652409, -10.57229757085618260, -6.180206054297716634 ) ) ;
#33488 = CARTESIAN_POINT ( 'NONE',  ( -36.00000000000000711, -7.238157050195700215, 10.49626516989268588 ) ) ;
#33489 = VECTOR ( 'NONE', #28896, 1000.000000000000000 ) ;
#33490 = CARTESIAN_POINT ( 'NONE',  ( -27.08423805673873375, -0.5302040644010280745, -2.229265646063334660 ) ) ;
#33491 = CARTESIAN_POINT ( 'NONE',  ( -27.86440745243244521, -9.318414989681810923, -7.586129753734442538 ) ) ;
#33492 = ORIENTED_EDGE ( 'NONE', *, *, #65528, .F. ) ;
#33493 = CARTESIAN_POINT ( 'NONE',  ( 5.516018279890452902, -0.002527316374434348482, -0.006286471671801920590 ) ) ;
#33494 = CYLINDRICAL_SURFACE ( 'NONE', #3638, 12.18649999999999878 ) ;
#33495 = ADVANCED_FACE ( 'NONE', ( #2348 ), #34163, .F. ) ;
#33496 = CARTESIAN_POINT ( 'NONE',  ( -0.8442279638247468521, -31.04755392045528950, -14.43184553624044852 ) ) ;
#33497 = ORIENTED_EDGE ( 'NONE', *, *, #56558, .F. ) ;
#33498 = CARTESIAN_POINT ( 'NONE',  ( -35.00000000000000000, 6.303578524886947143, 10.42955799785322490 ) ) ;
#33499 = CARTESIAN_POINT ( 'NONE',  ( 35.00000000000000000, -9.752226076388938125, -6.547236723513990775 ) ) ;
#33500 = LINE ( 'NONE', #12879, #51956 ) ;
#33501 = EDGE_CURVE ( 'NONE', #4057, #63452, #53917, .T. ) ;
#33502 = CARTESIAN_POINT ( 'NONE',  ( 1.719304012338199517, 12.70777170743846796, 0.7661785589580254463 ) ) ;
#33503 = EDGE_CURVE ( 'NONE', #16245, #39958, #42887, .T. ) ;
#33504 = EDGE_LOOP ( 'NONE', ( #26373, #24936 ) ) ;
#33505 = DIRECTION ( 'NONE',  ( 0.2475719085175094314, 0.000000000000000000, -0.9688695217174487784 ) ) ;
#33506 = ADVANCED_FACE ( 'NONE', ( #38216 ), #61343, .F. ) ;
#33507 = ORIENTED_EDGE ( 'NONE', *, *, #36841, .T. ) ;
#33508 = CARTESIAN_POINT ( 'NONE',  ( 2.247206125382827491, -7.214589497757600611, 2.502718378778785002 ) ) ;
#33509 = DIRECTION ( 'NONE',  ( 1.000000000000000000, 0.000000000000000000, 0.000000000000000000 ) ) ;
#33511 = AXIS2_PLACEMENT_3D ( 'NONE', #1838, #17459, #41734 ) ;
#33510 = CARTESIAN_POINT ( 'NONE',  ( -47.00000000000000711, 0.000000000000000000, 0.000000000000000000 ) ) ;
#33512 = DIRECTION ( 'NONE',  ( 0.000000000000000000, 0.6876994588534194319, 0.7259954919231345061 ) ) ;
#33513 = CARTESIAN_POINT ( 'NONE',  ( 2.247206125382827935, 7.539576157880618190, -1.211896144126850094 ) ) ;
#33514 = CARTESIAN_POINT ( 'NONE',  ( 25.05309951391468459, 25.00000000000000000, -8.132934882857099979 ) ) ;
#33515 = EDGE_CURVE ( 'NONE', #7543, #22716, #57883, .T. ) ;
#33516 = DIRECTION ( 'NONE',  ( 0.000000000000000000, -0.01356324068817998940, 0.9999080150203990547 ) ) ;
#33517 = CARTESIAN_POINT ( 'NONE',  ( 0.3040950598368144520, 7.687624643091433008, 9.552450779732136965 ) ) ;
#33518 = ORIENTED_EDGE ( 'NONE', *, *, #58672, .T. ) ;
#33519 = ORIENTED_EDGE ( 'NONE', *, *, #50631, .T. ) ;
#33520 = VERTEX_POINT ( 'NONE', #37900 ) ;
#33521 = SURFACE_STYLE_FILL_AREA ( #13237 ) ;
#33523 = DIRECTION ( 'NONE',  ( 0.000000000000000000, 0.01356324068817998940, -0.9999080150203990547 ) ) ;
#33522 = AXIS2_PLACEMENT_3D ( 'NONE', #48913, #58908, #13632 ) ;
#33524 = CARTESIAN_POINT ( 'NONE',  ( 2.941278708680199916, 6.068329152486375833, 0.9331242451665199278 ) ) ;
#33525 = CARTESIAN_POINT ( 'NONE',  ( -22.27945548916780183, -1.551028078364841800, 3.346394890313962200 ) ) ;
#33526 = VERTEX_POINT ( 'NONE', #17307 ) ;
#33527 = CARTESIAN_POINT ( 'NONE',  ( -35.00000000000000000, -3.511814412392038953, -11.66953048682403171 ) ) ;
#33528 = CARTESIAN_POINT ( 'NONE',  ( 2.269879328256727113, 6.544400685875880086, -3.949706986712128387 ) ) ;
#33529 = CARTESIAN_POINT ( 'NONE',  ( -22.28506771379528573, -3.718191140878641221, 0.2569416992704499081 ) ) ;
#33530 = ORIENTED_EDGE ( 'NONE', *, *, #41807, .T. ) ;
#33531 = ORIENTED_EDGE ( 'NONE', *, *, #13436, .T. ) ;
#33532 = CARTESIAN_POINT ( 'NONE',  ( 3.291290029914074378, 8.250315036047103590, 25.00000000000000000 ) ) ;
#33533 = ORIENTED_EDGE ( 'NONE', *, *, #52381, .F. ) ;
#33534 = CARTESIAN_POINT ( 'NONE',  ( 5.530133899448235191, -0.009387834778845766809, 0.01293763278443448191 ) ) ;
#33535 = ORIENTED_EDGE ( 'NONE', *, *, #54192, .F. ) ;
#33536 = EDGE_LOOP ( 'NONE', ( #47618, #29503, #57677, #63329 ) ) ;
#33537 = CARTESIAN_POINT ( 'NONE',  ( -35.00000000000000000, -2.905556151562544986, -11.38112321385053960 ) ) ;
#33538 = DIRECTION ( 'NONE',  ( -1.000000000000000000, 0.000000000000000000, 0.000000000000000000 ) ) ;
#33539 = VECTOR ( 'NONE', #2592, 1000.000000000000000 ) ;
#33540 = EDGE_CURVE ( 'NONE', #34853, #25053, #38832, .T. ) ;
#33541 = CARTESIAN_POINT ( 'NONE',  ( -27.09252613521643482, -2.309775830546446862, 0.1722886739160240377 ) ) ;
#33542 = FACE_OUTER_BOUND ( 'NONE', #7889, .T. ) ;
#33543 = DIRECTION ( 'NONE',  ( 0.000000000000000000, 0.000000000000000000, 1.000000000000000000 ) ) ;
#33544 = DIRECTION ( 'NONE',  ( -1.000000000000000000, -0.000000000000000000, -0.000000000000000000 ) ) ;
#33545 = EDGE_CURVE ( 'NONE', #21600, #51686, #28260, .T. ) ;
#33546 = ORIENTED_EDGE ( 'NONE', *, *, #52155, .F. ) ;
#33547 = DIRECTION ( 'NONE',  ( 0.000000000000000000, -0.5472293298355157543, 0.8369827122275419473 ) ) ;
#33548 = CARTESIAN_POINT ( 'NONE',  ( 2.350038591457884962, 2.471682575235502277, -10.33030559206184051 ) ) ;
#33549 = CARTESIAN_POINT ( 'NONE',  ( 0.2653141516239115316, -0.04404488958242430696, 12.24612533180317797 ) ) ;
#33550 = FACE_OUTER_BOUND ( 'NONE', #8164, .T. ) ;
#33551 = CARTESIAN_POINT ( 'NONE',  ( -18.23163618117759910, 13.26827036841251584, 2.579412572229281775 ) ) ;
#33552 = CARTESIAN_POINT ( 'NONE',  ( -22.35190811654612375, -3.252894036332505401, 2.161847148103702931 ) ) ;
#33553 = CARTESIAN_POINT ( 'NONE',  ( -35.00000000000000000, -7.499679039484122178, 9.040300684349668714 ) ) ;
#33554 = CARTESIAN_POINT ( 'NONE',  ( -22.31328051695926007, -3.633840107626937765, 1.076152733467191869 ) ) ;
#33555 = ADVANCED_FACE ( 'NONE', ( #43208 ), #63484, .T. ) ;
#33556 = LINE ( 'NONE', #3307, #23604 ) ;
#33557 = VERTEX_POINT ( 'NONE', #44849 ) ;
#33558 = LINE ( 'NONE', #52550, #21660 ) ;
#33559 = AXIS2_PLACEMENT_3D ( 'NONE', #25343, #19726, #20033 ) ;
#33560 = AXIS2_PLACEMENT_3D ( 'NONE', #53023, #7455, #27746 ) ;
#33561 = EDGE_LOOP ( 'NONE', ( #48235, #59968, #9370, #12675 ) ) ;
#33562 = DIRECTION ( 'NONE',  ( 1.000000000000000000, 0.000000000000000000, 0.000000000000000000 ) ) ;
#33563 = DIRECTION ( 'NONE',  ( 1.000000000000000000, 0.000000000000000000, -0.000000000000000000 ) ) ;
#33564 = CARTESIAN_POINT ( 'NONE',  ( 12.66212018674185913, -11.71370580328924227, -6.722415854528632551 ) ) ;
#33565 = CARTESIAN_POINT ( 'NONE',  ( -35.04709527796842394, -0.001082316405377065083, 0.01231589140597219578 ) ) ;
#33566 = CARTESIAN_POINT ( 'NONE',  ( 35.00000000000000000, 12.05416472667167760, 1.791059740004291578 ) ) ;
#33567 = EDGE_CURVE ( 'NONE', #56695, #37848, #57272, .T. ) ;
#33568 = EDGE_LOOP ( 'NONE', ( #6361, #10123, #59511, #60271 ) ) ;
#33569 = DIRECTION ( 'NONE',  ( -1.000000000000000000, 0.000000000000000000, 0.000000000000000000 ) ) ;
#33570 = CARTESIAN_POINT ( 'NONE',  ( 2.280717697723835258, -3.687451363405612970, 6.699799459371652333 ) ) ;
#33571 = CARTESIAN_POINT ( 'NONE',  ( 37.00000000000000711, 4.705694406421931860E-17, -3.469127814946512892E-15 ) ) ;
#33572 = DIRECTION ( 'NONE',  ( 0.000000000000000000, -0.2618041379715704275, 0.9651210252299774472 ) ) ;
#33573 = EDGE_CURVE ( 'NONE', #11101, #11073, #37068, .T. ) ;
#33574 = CIRCLE ( 'NONE', #12291, 12.18649999999999878 ) ;
#33575 = B_SPLINE_CURVE_WITH_KNOTS ( 'NONE', 3,
 ( #40652, #51312, #25045, #750, #15042, #65271, #19735, #39994, #60945, #15384, #60277, #47942, #41628, #2054, #42258, #17357 ),
 .UNSPECIFIED., .F., .F.,
 ( 4, 3, 3, 3, 3, 4 ),
 ( 0.000000000000000000, 0.0003017745587525249760, 0.0006035491769808738489, 0.0009053241094668170071, 0.001207275924540017736, 0.001510325902533033848 ),
 .UNSPECIFIED. ) ;
#33576 = CARTESIAN_POINT ( 'NONE',  ( 35.00000000000000000, -7.146664589317845540, 9.321877890560507751 ) ) ;
#33577 = ORIENTED_EDGE ( 'NONE', *, *, #53660, .T. ) ;
#33578 = DIRECTION ( 'NONE',  ( -1.000000000000000000, 0.000000000000000000, 0.000000000000000000 ) ) ;
#33579 = CARTESIAN_POINT ( 'NONE',  ( 2.556980015513105720, 5.777953785406880982, -5.149458076504359383 ) ) ;
#33580 = DIRECTION ( 'NONE',  ( 1.000000000000000000, -0.000000000000000000, 0.000000000000000000 ) ) ;
#33581 = ADVANCED_FACE ( 'NONE', ( #34214 ), #64280, .F. ) ;
#33582 = ORIENTED_EDGE ( 'NONE', *, *, #45922, .F. ) ;
#33583 = ORIENTED_EDGE ( 'NONE', *, *, #31437, .T. ) ;
#33584 = CARTESIAN_POINT ( 'NONE',  ( -9.351388602708162523, 12.99278190472488248, -3.665735721005250358 ) ) ;
#33585 = EDGE_CURVE ( 'NONE', #27364, #45713, #64466, .T. ) ;
#33586 = ORIENTED_EDGE ( 'NONE', *, *, #1062, .F. ) ;
#33587 = CARTESIAN_POINT ( 'NONE',  ( 0.2646305136544065406, 4.312539723326288765, -11.46223899740595620 ) ) ;
#33588 = DIRECTION ( 'NONE',  ( 0.000000000000000000, 0.9105187689795939399, -0.4134677391718545314 ) ) ;
#33589 = CARTESIAN_POINT ( 'NONE',  ( -27.08850691366480490, -1.648570643964191396, -1.609738257842918019 ) ) ;
#33590 = DIRECTION ( 'NONE',  ( 0.000000000000000000, 0.6269146997507987207, 0.7790879021242507196 ) ) ;
#33591 = ADVANCED_FACE ( 'NONE', ( #40173 ), #65128, .T. ) ;
#33592 = CARTESIAN_POINT ( 'NONE',  ( -35.04643116707788408, 0.01135624435143721411, 0.004425962698848331933 ) ) ;
#33593 = ORIENTED_EDGE ( 'NONE', *, *, #10788, .F. ) ;
#33594 = VERTEX_POINT ( 'NONE', #50185 ) ;
#33595 = VERTEX_POINT ( 'NONE', #29873 ) ;
#33596 = CARTESIAN_POINT ( 'NONE',  ( 0.2638984909335720941, 11.43908195192335953, -4.375449752477019949 ) ) ;
#33597 = CARTESIAN_POINT ( 'NONE',  ( -27.05874794189610455, 1.734723475976807094E-15, -8.673617379884035472E-15 ) ) ;
#33599 = EDGE_CURVE ( 'NONE', #49092, #42734, #24364, .T. ) ;
#33598 = ORIENTED_EDGE ( 'NONE', *, *, #19228, .T. ) ;
#33600 = FACE_OUTER_BOUND ( 'NONE', #18481, .T. ) ;
#33601 = CARTESIAN_POINT ( 'NONE',  ( -22.28776923226071460, -0.2883912626656507938, -3.702096209084106082 ) ) ;
#33602 = ORIENTED_EDGE ( 'NONE', *, *, #59371, .F. ) ;
#33603 = CIRCLE ( 'NONE', #47426, 4.500000000000000888 ) ;
#33604 = CARTESIAN_POINT ( 'NONE',  ( -37.00000000000000711, 0.000000000000000000, 0.000000000000000000 ) ) ;
#33605 =( BOUNDED_SURFACE ( )  B_SPLINE_SURFACE ( 3, 1, ( 
 ( #25599, #26575 ),
 ( #346, #46534 ),
 ( #46869, #20624 ),
 ( #5672, #35876 ) ),
 .UNSPECIFIED., .F., .F., .F. ) 
 B_SPLINE_SURFACE_WITH_KNOTS ( ( 4, 4 ),
 ( 2, 2 ),
 ( 0.000000000000000000, 1.000000000000000000 ),
 ( 0.000000000000000000, 1.000000000000000000 ),
 .UNSPECIFIED. ) 
 GEOMETRIC_REPRESENTATION_ITEM ( )  RATIONAL_B_SPLINE_SURFACE ( (
 ( 1.000000000000000000, 1.000000000000000000),
 ( 0.9856612449720755231, 0.9999558406602322425),
 ( 0.9856612449720755231, 0.9999558406602322425),
 ( 1.000000000000000000, 1.000000000000000000) ) ) 
 REPRESENTATION_ITEM ( '' )  SURFACE ( )  );
#33606 = DIRECTION ( 'NONE',  ( 0.000000000000000000, 0.000000000000000000, 1.000000000000000000 ) ) ;
#33607 = FACE_OUTER_BOUND ( 'NONE', #30173, .T. ) ;
#33608 = ORIENTED_EDGE ( 'NONE', *, *, #56435, .F. ) ;
#33609 = ORIENTED_EDGE ( 'NONE', *, *, #11450, .T. ) ;
#33610 = CARTESIAN_POINT ( 'NONE',  ( 2.245754705088395475, 2.506725724682664413, 7.212684575686784783 ) ) ;
#33611 = ORIENTED_EDGE ( 'NONE', *, *, #14771, .F. ) ;
#33612 = DIRECTION ( 'NONE',  ( 0.000000000000000000, 0.01356324068817992175, -0.9999080150203990547 ) ) ;
#33613 = ORIENTED_EDGE ( 'NONE', *, *, #62847, .F. ) ;
#33614 = CARTESIAN_POINT ( 'NONE',  ( 2.255723233588952326, 3.704537245405040924, 6.680843247642330951 ) ) ;
#33615 = CARTESIAN_POINT ( 'NONE',  ( 2.889800649504073782, -6.016320774579801522, -1.129261637821672215 ) ) ;
#33616 = CARTESIAN_POINT ( 'NONE',  ( -17.71439793346020153, -28.67846309484135503, 8.502197385450015688 ) ) ;
#33617 = CARTESIAN_POINT ( 'NONE',  ( -35.00000000000000000, -6.753013023069787124, 10.14433819232432477 ) ) ;
#33618 = CARTESIAN_POINT ( 'NONE',  ( 1.719304012341202004, 11.67935079956989775, -5.066286238790292273 ) ) ;
#33619 = CARTESIAN_POINT ( 'NONE',  ( -22.46225619532222950, -4.233934615764599840, 0.1595555201818281699 ) ) ;
#33621 = VERTEX_POINT ( 'NONE', #8303 ) ;
#33620 = B_SPLINE_CURVE_WITH_KNOTS ( 'NONE', 3,
 ( #27501, #16876, #37147, #36831, #22867, #47161, #31512, #47796, #22532, #57129, #58436, #6261, #52478, #58109, #12521, #51813, #11557, #37486, #17546, #31824, #6591, #26857, #27184, #1610, #27841, #21881, #32155, #32802, #19754, #29697, #50352, #54980, #2914, #10091, #30372, #50006, #9408, #40011, #53455, #28175, #60298, #65593, #50667, #114, #60626, #12864, #64064, #25377, #28480, #63718, #45333, #5111, #45660, #20394 ),
 .UNSPECIFIED., .F., .F.,
 ( 4, 2, 2, 2, 2, 2, 2, 2, 2, 2, 2, 2, 2, 2, 2, 2, 2, 2, 2, 2, 2, 2, 2, 2, 2, 2, 4 ),
 ( 0.000000000000000000, 0.004909564951003677659, 0.007364347426505511718, 0.009819129902007346644, 0.01472869485301101650, 0.01718347732851285489, 0.01963825980401469329, 0.02454782475501837702, 0.02700260723052021195, 0.02945738970602204687, 0.03191217218152388180, 0.03313956341927479926, 0.03436695465702571672, 0.03927651960802939352, 0.04173130208353122844, 0.04295869332128215284, 0.04418608455903307031, 0.04909564951003672628, 0.05155043198553856121, 0.05400521446104038920, 0.05891477941204405211, 0.06382434436304770808, 0.06627912683854954301, 0.06873390931405137794, 0.07364347426505504779, 0.07609825674055689659, 0.07855303921605873152 ),
 .UNSPECIFIED. ) ;
#33622 = DIRECTION ( 'NONE',  ( 0.000000000000000000, -0.01356324068817998940, 0.9999080150203990547 ) ) ;
#33623 = EDGE_CURVE ( 'NONE', #40116, #27547, #16915, .T. ) ;
#33624 = ORIENTED_EDGE ( 'NONE', *, *, #65077, .F. ) ;
#33625 = CYLINDRICAL_SURFACE ( 'NONE', #41252, 12.75000000000000178 ) ;
#33626 = CARTESIAN_POINT ( 'NONE',  ( 35.00000000000000000, 4.705694406421931860E-17, -3.469127814946512892E-15 ) ) ;
#33627 = ORIENTED_EDGE ( 'NONE', *, *, #44835, .F. ) ;
#33628 = CARTESIAN_POINT ( 'NONE',  ( 5.515539859299206427, 0.005991790098944300112, 0.0008592514567753142991 ) ) ;
#33629 = CARTESIAN_POINT ( 'NONE',  ( 0.2717059086739013751, 6.276007891175726883, 10.51822005841996877 ) ) ;
#33630 = CARTESIAN_POINT ( 'NONE',  ( 0.3164563675027689538, -2.365891945210734981, -12.03284811452139991 ) ) ;
#33631 = EDGE_LOOP ( 'NONE', ( #51386, #18979, #22660, #298 ) ) ;
#33632 = ORIENTED_EDGE ( 'NONE', *, *, #61195, .F. ) ;
#33633 = CARTESIAN_POINT ( 'NONE',  ( 2.000000000000001776, 0.000000000000000000, 0.000000000000000000 ) ) ;
#33634 = ORIENTED_EDGE ( 'NONE', *, *, #2264, .T. ) ;
#33635 = CARTESIAN_POINT ( 'NONE',  ( -25.31227681912704597, -12.03780878397515686, 6.112770619466626698 ) ) ;
#33636 = CARTESIAN_POINT ( 'NONE',  ( 35.00000000000000000, -9.040300684349746874, -7.499679039484027143 ) ) ;
#33637 = CARTESIAN_POINT ( 'NONE',  ( 5.514624014163232779, 0.003668383633201691488, 0.001921576324372104407 ) ) ;
#33638 = DIRECTION ( 'NONE',  ( -1.000000000000000000, -0.000000000000000000, 0.000000000000000000 ) ) ;
#33639 = CARTESIAN_POINT ( 'NONE',  ( -18.02751974386707090, -5.811735475709186360, 10.50276896598090204 ) ) ;
#33640 = EDGE_CURVE ( 'NONE', #27713, #6901, #63607, .T. ) ;
#33641 = VERTEX_POINT ( 'NONE', #34843 ) ;
#33642 = CIRCLE ( 'NONE', #15585, 5.000000000000000000 ) ;
#33643 = CARTESIAN_POINT ( 'NONE',  ( 1.719304012338820131, 1.452142814150020556, 12.64775761152757561 ) ) ;
#33644 = EDGE_CURVE ( 'NONE', #1816, #7740, #4195, .T. ) ;
#33645 = CIRCLE ( 'NONE', #31544, 5.000000000000001776 ) ;
#33646 = CARTESIAN_POINT ( 'NONE',  ( -27.16196273015728124, -13.32896842526023029, -2.143521441892683566 ) ) ;
#33647 = CARTESIAN_POINT ( 'NONE',  ( 24.73620011133604280, 10.89680678806336545, -7.971846375286735231 ) ) ;
#33648 = CARTESIAN_POINT ( 'NONE',  ( 25.00000000000000355, -9.999999999999998224, 24.00000000000000000 ) ) ;
#33649 = LINE ( 'NONE', #37970, #8652 ) ;
#33650 = CARTESIAN_POINT ( 'NONE',  ( 5.887754249840907228, -9.753796435503998552, -7.002310812516553185 ) ) ;
#33651 = CARTESIAN_POINT ( 'NONE',  ( -22.27719381268171261, -2.588413841766858958, -2.618044180756137429 ) ) ;
#33652 = EDGE_CURVE ( 'NONE', #2794, #34196, #22225, .T. ) ;
#33653 = ORIENTED_EDGE ( 'NONE', *, *, #38351, .F. ) ;
#33654 = CARTESIAN_POINT ( 'NONE',  ( 12.83456828947878314, -10.33636979156220370, -6.108674021912653629 ) ) ;
#33655 = ORIENTED_EDGE ( 'NONE', *, *, #37057, .F. ) ;
#33656 = CARTESIAN_POINT ( 'NONE',  ( 0.000000000000000000, 2.480520636974191895, 6.345145617221231049 ) ) ;
#33657 = CARTESIAN_POINT ( 'NONE',  ( -22.29290468048228036, 3.718584170466879613, -0.2747050847461790513 ) ) ;
#33658 = LINE ( 'NONE', #8725, #53410 ) ;
#33659 = ORIENTED_EDGE ( 'NONE', *, *, #19617, .F. ) ;
#33660 = CARTESIAN_POINT ( 'NONE',  ( 39.82259759989631931, -25.85751090193130608, -4.500000000000000000 ) ) ;
#33661 = EDGE_LOOP ( 'NONE', ( #65573, #17598, #44139, #38412 ) ) ;
#33662 = ORIENTED_EDGE ( 'NONE', *, *, #64051, .F. ) ;
#33663 = ORIENTED_EDGE ( 'NONE', *, *, #37092, .T. ) ;
#33664 = CARTESIAN_POINT ( 'NONE',  ( 29.51976981715666781, -7.690765383426355406, 11.09513982864076276 ) ) ;
#33665 = EDGE_CURVE ( 'NONE', #16416, #33072, #32838, .T. ) ;
#33666 = CARTESIAN_POINT ( 'NONE',  ( -22.31328051695926007, -3.401210163132568187, -1.671726071983963946 ) ) ;
#33667 = ORIENTED_EDGE ( 'NONE', *, *, #39529, .F. ) ;
#33668 = CARTESIAN_POINT ( 'NONE',  ( 2.931247277082674074, 5.779735553870104958, 5.333206743525262361 ) ) ;
#33669 = CARTESIAN_POINT ( 'NONE',  ( 2.899286259009686173, -3.018334250363132298, 7.250549018622930220 ) ) ;
#33670 = FACE_OUTER_BOUND ( 'NONE', #45503, .T. ) ;
#33671 = CARTESIAN_POINT ( 'NONE',  ( 19.28625800530496903, 1.699513388191793428, 11.87904264843580471 ) ) ;
#33672 = ORIENTED_EDGE ( 'NONE', *, *, #26156, .T. ) ;
#33673 = CARTESIAN_POINT ( 'NONE',  ( -35.00000000000000000, -7.146664589317976102, 9.321877890560418933 ) ) ;
#33674 = CARTESIAN_POINT ( 'NONE',  ( 12.50310467286144167, -29.27802453453052323, 5.021082754746532650 ) ) ;
#33675 = CARTESIAN_POINT ( 'NONE',  ( -29.76537318338591120, -3.714251817591042393, 11.41077529405956170 ) ) ;
#33677 = ORIENTED_EDGE ( 'NONE', *, *, #28085, .F. ) ;
#33676 = DIRECTION ( 'NONE',  ( 1.000000000000000000, -0.000000000000000000, 0.000000000000000000 ) ) ;
#33678 = DIRECTION ( 'NONE',  ( 0.000000000000000000, 0.000000000000000000, 1.000000000000000000 ) ) ;
#33679 = ORIENTED_EDGE ( 'NONE', *, *, #29268, .F. ) ;
#33680 = CARTESIAN_POINT ( 'NONE',  ( -19.19594308705144314, 13.42342342571188674, -1.564108210525256171 ) ) ;
#33681 = ORIENTED_EDGE ( 'NONE', *, *, #25769, .T. ) ;
#33682 = CIRCLE ( 'NONE', #50686, 3.000000000000001332 ) ;
#33683 = DIRECTION ( 'NONE',  ( 1.000000000000000000, 0.000000000000000000, -0.000000000000000000 ) ) ;
#33684 = CYLINDRICAL_SURFACE ( 'NONE', #12869, 4.999999999999999112 ) ;
#33685 = FACE_OUTER_BOUND ( 'NONE', #40862, .T. ) ;
#33686 = CARTESIAN_POINT ( 'NONE',  ( 0.3057689695767522586, -3.975296631252044133, 11.59726335252432783 ) ) ;
#33687 = CARTESIAN_POINT ( 'NONE',  ( 0.2653141334712577071, -11.49252672845885925, 4.229817350136370280 ) ) ;
#33688 = VECTOR ( 'NONE', #33747, 1000.000000000000000 ) ;
#33689 = CARTESIAN_POINT ( 'NONE',  ( -10.90165637463000614, -7.508992741355389633, -11.21895841913464764 ) ) ;
#33690 = LINE ( 'NONE', #9078, #57553 ) ;
#33691 = EDGE_CURVE ( 'NONE', #2755, #36879, #2340, .T. ) ;
#33692 = ORIENTED_EDGE ( 'NONE', *, *, #33821, .F. ) ;
#33693 = DIRECTION ( 'NONE',  ( -1.000000000000000000, 0.000000000000000000, 0.000000000000000000 ) ) ;
#33694 = VERTEX_POINT ( 'NONE', #59832 ) ;
#33695 = ADVANCED_FACE ( 'NONE', ( #18936 ), #39200, .F. ) ;
#33696 = ORIENTED_EDGE ( 'NONE', *, *, #28512, .T. ) ;
#33697 = DIRECTION ( 'NONE',  ( -1.000000000000000000, -0.000000000000000000, 0.000000000000000000 ) ) ;
#33698 = DIRECTION ( 'NONE',  ( -1.000000000000000000, 0.000000000000000000, 0.000000000000000000 ) ) ;
#33699 = DIRECTION ( 'NONE',  ( 0.000000000000000000, 0.01356324068817998940, -0.9999080150203990547 ) ) ;
#33700 = CARTESIAN_POINT ( 'NONE',  ( -22.27719381268171617, 0.9326100520993234611, 3.561499689648252698 ) ) ;
#33701 = CARTESIAN_POINT ( 'NONE',  ( -37.00000000000000711, -4.309077947445573820, -10.92721691015460550 ) ) ;
#33702 = FACE_OUTER_BOUND ( 'NONE', #2493, .T. ) ;
#33703 = EDGE_CURVE ( 'NONE', #31528, #44677, #48777, .T. ) ;
#33704 = CARTESIAN_POINT ( 'NONE',  ( -35.00000000000000000, 0.000000000000000000, 0.000000000000000000 ) ) ;
#33705 = VERTEX_POINT ( 'NONE', #20576 ) ;
#33706 = CARTESIAN_POINT ( 'NONE',  ( 1.719304012340653998, -9.242227816403676854, -8.755325027797448811 ) ) ;
#33707 = CARTESIAN_POINT ( 'NONE',  ( -27.08418322526030764, -1.431535851194450260, -1.789041206975763076 ) ) ;
#33708 = LINE ( 'NONE', #18766, #51969 ) ;
#33709 = ADVANCED_FACE ( 'NONE', ( #46816 ), #2346, .F. ) ;
#33710 = AXIS2_PLACEMENT_3D ( 'NONE', #55616, #5396, #64906 ) ;
#33711 = DIRECTION ( 'NONE',  ( -1.000000000000000000, 0.000000000000000000, 0.000000000000000000 ) ) ;
#33712 = DIRECTION ( 'NONE',  ( -0.3939253465568943180, 0.6978179301705840221, -0.5982248387291124736 ) ) ;
#33713 = CARTESIAN_POINT ( 'NONE',  ( -9.818496758707208727, -3.216705815951581560, 13.11220466491898407 ) ) ;
#33714 = DIRECTION ( 'NONE',  ( 1.000000000000000000, 0.000000000000000000, 0.000000000000000000 ) ) ;
#33715 = ORIENTED_EDGE ( 'NONE', *, *, #63516, .T. ) ;
#33716 = CARTESIAN_POINT ( 'NONE',  ( 5.530133899448235191, 0.01459891979722878833, -0.006510401266731667864 ) ) ;
#33717 = DIRECTION ( 'NONE',  ( -1.000000000000000000, 0.000000000000000000, 0.000000000000000000 ) ) ;
#33718 = CARTESIAN_POINT ( 'NONE',  ( -22.27384469013076185, -0.3730095848193254460, -3.663183248998795882 ) ) ;
#33719 = AXIS2_PLACEMENT_3D ( 'NONE', #13801, #58755, #28147 ) ;
#33720 = CIRCLE ( 'NONE', #17839, 12.75000000000000178 ) ;
#33721 = CARTESIAN_POINT ( 'NONE',  ( -37.00000000000000711, 1.791059740004591561, -12.05416472667163674 ) ) ;
#33722 = CARTESIAN_POINT ( 'NONE',  ( -35.00000000000000000, 0.000000000000000000, 0.000000000000000000 ) ) ;
#33723 = ORIENTED_EDGE ( 'NONE', *, *, #40905, .F. ) ;
#33724 = CARTESIAN_POINT ( 'NONE',  ( -17.71589014024121411, 3.739618266278695646, 12.97327105657033641 ) ) ;
#33725 = DIRECTION ( 'NONE',  ( 0.3865475372811020827, 0.4778122177792094027, -0.7888450329201726063 ) ) ;
#33726 = CARTESIAN_POINT ( 'NONE',  ( 35.00000000000000000, -8.146229107149464355, -9.063649021438928699 ) ) ;
#33727 = VERTEX_POINT ( 'NONE', #35526 ) ;
#33728 = DIRECTION ( 'NONE',  ( 1.000000000000000000, 0.000000000000000000, -0.000000000000000000 ) ) ;
#33729 = CARTESIAN_POINT ( 'NONE',  ( 0.000000000000000000, -2.664846396702537312, 6.404188155572974495 ) ) ;
#33730 = VERTEX_POINT ( 'NONE', #30527 ) ;
#33731 = ORIENTED_EDGE ( 'NONE', *, *, #11895, .F. ) ;
#33732 = CARTESIAN_POINT ( 'NONE',  ( -37.00000000000000711, 8.496612874013289129, -9.506317355798284296 ) ) ;
#33733 = EDGE_CURVE ( 'NONE', #2404, #21209, #51169, .T. ) ;
#33734 = ORIENTED_EDGE ( 'NONE', *, *, #5113, .F. ) ;
#33735 = FACE_OUTER_BOUND ( 'NONE', #55430, .T. ) ;
#33736 = CARTESIAN_POINT ( 'NONE',  ( 5.515188684475870851, 0.0005703990286340047521, -0.005320786921497682072 ) ) ;
#33737 = CARTESIAN_POINT ( 'NONE',  ( -35.00000000000000000, 8.295159312811854591, 8.927548052240926069 ) ) ;
#33738 = DIRECTION ( 'NONE',  ( -1.000000000000000000, 0.000000000000000000, -0.000000000000000000 ) ) ;
#33739 = CARTESIAN_POINT ( 'NONE',  ( -35.00000000000000000, -1.908798535168293897, -12.60630747491665282 ) ) ;
#33741 = ORIENTED_EDGE ( 'NONE', *, *, #35830, .T. ) ;
#33740 = PLANE ( 'NONE',  #31893 ) ;
#33742 = CARTESIAN_POINT ( 'NONE',  ( -47.00000000000000711, 0.000000000000000000, 0.000000000000000000 ) ) ;
#33743 = VERTEX_POINT ( 'NONE', #50832 ) ;
#33744 = DIRECTION ( 'NONE',  ( -1.000000000000000000, 0.000000000000000000, -0.000000000000000000 ) ) ;
#33745 = ORIENTED_EDGE ( 'NONE', *, *, #12443, .T. ) ;
#33746 = EDGE_LOOP ( 'NONE', ( #39530, #34313, #45818, #13309 ) ) ;
#33747 = DIRECTION ( 'NONE',  ( 1.000000000000000000, 0.000000000000000000, -0.000000000000000000 ) ) ;
#33748 = CARTESIAN_POINT ( 'NONE',  ( -7.529925403075611534, -31.54078451673377614, 13.99923386364726063 ) ) ;
#33749 = DIRECTION ( 'NONE',  ( 1.000000000000000000, -0.000000000000000000, 0.000000000000000000 ) ) ;
#33750 = EDGE_CURVE ( 'NONE', #22729, #63981, #21208, .T. ) ;
#33751 = CARTESIAN_POINT ( 'NONE',  ( 23.98519066662860411, -2.642583004929468959, 11.70655643947132241 ) ) ;
#33752 = CARTESIAN_POINT ( 'NONE',  ( 1.452237505248552996, -12.34692280296790479, -2.778494755359182111 ) ) ;
#33753 = DIRECTION ( 'NONE',  ( 0.000000000000000000, -0.9999080150203988326, -0.01356324068819046366 ) ) ;
#33754 = EDGE_LOOP ( 'NONE', ( #2049, #3004, #53744, #36207 ) ) ;
#33755 = CARTESIAN_POINT ( 'NONE',  ( 2.000000000000001776, -2.315790869867103474, 7.133520354428079635 ) ) ;
#33756 = EDGE_CURVE ( 'NONE', #19313, #29924, #55118, .T. ) ;
#33757 = DIRECTION ( 'NONE',  ( 0.000000000000000000, -0.2960891610144577024, -0.9551603052523457427 ) ) ;
#33758 = CARTESIAN_POINT ( 'NONE',  ( 0.000000000000000000, 0.000000000000000000, 0.000000000000000000 ) ) ;
#33759 = LINE ( 'NONE', #12176, #38560 ) ;
#33760 = EDGE_CURVE ( 'NONE', #61436, #10609, #62556, .T. ) ;
#33761 = ORIENTED_EDGE ( 'NONE', *, *, #16204, .F. ) ;
#33762 = CARTESIAN_POINT ( 'NONE',  ( 2.256373768223415066, -7.499124080223147359, 1.457292142211195074 ) ) ;
#33763 = AXIS2_PLACEMENT_3D ( 'NONE', #48028, #12750, #58679 ) ;
#33764 = CARTESIAN_POINT ( 'NONE',  ( 0.3106921474978491804, 0.2354703039889815830, -12.25904950202576771 ) ) ;
#33765 = CARTESIAN_POINT ( 'NONE',  ( -41.00000000000000711, -1.694065894508600678E-18, 0.000000000000000000 ) ) ;
#33766 = CARTESIAN_POINT ( 'NONE',  ( -22.29677679919927868, 3.097220482904032401, -2.096973157017371747 ) ) ;
#33767 = CARTESIAN_POINT ( 'NONE',  ( -36.00000000000000711, 12.02534193257726969, -4.237174932027097718 ) ) ;
#33768 = CARTESIAN_POINT ( 'NONE',  ( 37.00000000000000711, 8.573591947375318156, -8.029056188533719052 ) ) ;
#33769 = EDGE_CURVE ( 'NONE', #57333, #7851, #46712, .T. ) ;
#33770 = CARTESIAN_POINT ( 'NONE',  ( 2.242819959140647690, 3.905785747114015383, -6.560218843829733970 ) ) ;
#33771 = ORIENTED_EDGE ( 'NONE', *, *, #31804, .F. ) ;
#33772 =( BOUNDED_CURVE ( )  B_SPLINE_CURVE ( 3, ( #3211, #54069, #28457, #3556 ),
 .UNSPECIFIED., .F., .F. ) 
 B_SPLINE_CURVE_WITH_KNOTS ( ( 4, 4 ),
 ( 2.519937747667190919, 2.535468512986650769 ),
 .UNSPECIFIED. ) 
 CURVE ( )  GEOMETRIC_REPRESENTATION_ITEM ( )  RATIONAL_B_SPLINE_CURVE ( ( 1.000000000000000000, 0.9999798997117221866, 0.9999798997117221866, 1.000000000000000000 ) ) 
 REPRESENTATION_ITEM ( '' )  );
#33773 = EDGE_CURVE ( 'NONE', #35253, #56493, #49860, .T. ) ;
#33774 = EDGE_LOOP ( 'NONE', ( #48922, #11857, #63441, #26172 ) ) ;
#33775 = CARTESIAN_POINT ( 'NONE',  ( 1.375507693217718153, 3.754650692913772847, 12.04466556545155065 ) ) ;
#33776 = CARTESIAN_POINT ( 'NONE',  ( 2.907497136250996927, 4.769582063554166140, -6.243048412628978916 ) ) ;
#33777 = LINE ( 'NONE', #33132, #48930 ) ;
#33778 = LINE ( 'NONE', #49746, #30231 ) ;
#33779 = CARTESIAN_POINT ( 'NONE',  ( -28.24214478236189052, 12.24469403912116761, -5.693128020442387083 ) ) ;
#33780 = EDGE_CURVE ( 'NONE', #42105, #33067, #23274, .T. ) ;
#33781 = VECTOR ( 'NONE', #40464, 1000.000000000000000 ) ;
#33782 = CARTESIAN_POINT ( 'NONE',  ( 7.045079518374575578, -7.884504117378364541, -10.96637384480524524 ) ) ;
#33783 = CARTESIAN_POINT ( 'NONE',  ( 35.00000000000000000, -2.772148766916200380, -11.86701198550355585 ) ) ;
#33784 = EDGE_CURVE ( 'NONE', #8260, #25967, #10916, .T. ) ;
#33785 = DIRECTION ( 'NONE',  ( -1.000000000000000000, 0.000000000000000000, 0.000000000000000000 ) ) ;
#33786 = CARTESIAN_POINT ( 'NONE',  ( 2.556980015514183524, -5.149458076504853210, -5.777953785406920950 ) ) ;
#33787 = ORIENTED_EDGE ( 'NONE', *, *, #22856, .T. ) ;
#33788 = CARTESIAN_POINT ( 'NONE',  ( 0.2651627923886311078, 12.04449855907068390, 2.213220384814313935 ) ) ;
#33789 = CARTESIAN_POINT ( 'NONE',  ( 35.00000000000000000, -10.07641281632173325, 6.036400161834665212 ) ) ;
#33790 = CYLINDRICAL_SURFACE ( 'NONE', #30141, 12.18650000000000055 ) ;
#33791 = CIRCLE ( 'NONE', #46533, 12.75000000000000178 ) ;
#33792 = CARTESIAN_POINT ( 'NONE',  ( -27.08417473062937120, -0.4370481938669370514, -2.249064769433628097 ) ) ;
#33793 = CARTESIAN_POINT ( 'NONE',  ( 1.547277799339520366, -4.961646058324188147, -11.66196709685601363 ) ) ;
#33794 = AXIS2_PLACEMENT_3D ( 'NONE', #3669, #23602, #4290 ) ;
#33795 = CIRCLE ( 'NONE', #8327, 1.500000000000000222 ) ;
#33796 = EDGE_LOOP ( 'NONE', ( #13965, #60406, #33261, #54713 ) ) ;
#33797 = CARTESIAN_POINT ( 'NONE',  ( 2.257661810676419023, -2.485866587321432952, 7.224098098130517620 ) ) ;
#33798 = CARTESIAN_POINT ( 'NONE',  ( 0.9232058338315048962, -0.3773051331668853536, 12.46548196349785975 ) ) ;
#33799 = CARTESIAN_POINT ( 'NONE',  ( 3.702144525957873356, -25.87585389521097312, -15.43847573974272613 ) ) ;
#33800 = ORIENTED_EDGE ( 'NONE', *, *, #3226, .T. ) ;
#33801 = CARTESIAN_POINT ( 'NONE',  ( 0.2646305136544072623, 12.03696649559614862, 2.256625640822354839 ) ) ;
#33802 = CARTESIAN_POINT ( 'NONE',  ( 2.827825597296802940, 8.776379025186180627, 2.100863646776085503 ) ) ;
#33803 = DIRECTION ( 'NONE',  ( -1.000000000000000000, 0.000000000000000000, 0.000000000000000000 ) ) ;
#33804 = B_SPLINE_CURVE_WITH_KNOTS ( 'NONE', 3,
 ( #35906, #11319, #31587, #41565, #52231, #30936, #51898, #373, #51250, #56205, #46255, #56555, #25972, #699, #47245, #46899, #20954, #11637 ),
 .UNSPECIFIED., .F., .F.,
 ( 4, 2, 2, 2, 2, 2, 2, 2, 4 ),
 ( 1.192622389734054877E-18, 0.001238680244670008462, 0.002477360489340016056, 0.003716040734010024084, 0.004954720978680030377, 0.006193401223350037538, 0.007432081468020046433, 0.008670761712690053594, 0.009909441957360059020 ),
 .UNSPECIFIED. ) ;
#33805 = CARTESIAN_POINT ( 'NONE',  ( 0.3218525148189792517, -8.069481661595405697, 9.236582760335950937 ) ) ;
#33806 = CARTESIAN_POINT ( 'NONE',  ( 0.2648978790185584908, 12.24533305150758089, 0.1321385342562836074 ) ) ;
#33807 = ADVANCED_FACE ( 'NONE', ( #5956 ), #26213, .T. ) ;
#33808 = DIRECTION ( 'NONE',  ( 1.000000000000000000, 0.000000000000000000, -0.000000000000000000 ) ) ;
#33809 = ORIENTED_EDGE ( 'NONE', *, *, #42781, .T. ) ;
#33810 = CARTESIAN_POINT ( 'NONE',  ( 2.258463476536643810, -7.224688073723619652, 2.484972401833223543 ) ) ;
#33811 = DIRECTION ( 'NONE',  ( 1.000000000000000000, 0.000000000000000000, 0.000000000000000000 ) ) ;
#33812 = CARTESIAN_POINT ( 'NONE',  ( 0.3109076770649036314, -9.542672295796769788, -7.699281309344426560 ) ) ;
#33813 = CARTESIAN_POINT ( 'NONE',  ( -27.15525204139122195, 0.5628609503965513738, -2.440367606305306580 ) ) ;
#33814 = EDGE_CURVE ( 'NONE', #21947, #10229, #31748, .T. ) ;
#33815 = CARTESIAN_POINT ( 'NONE',  ( 2.251139882113960322, 7.542197031254634254, -1.203816215709469839 ) ) ;
#33816 = CARTESIAN_POINT ( 'NONE',  ( 2.241352910868910531, -3.889181972941495147, 6.569501556381427854 ) ) ;
#33817 = CARTESIAN_POINT ( 'NONE',  ( 35.00000000000000000, -10.49591321039684289, -5.273331777780305707 ) ) ;
#33818 = CARTESIAN_POINT ( 'NONE',  ( 2.889800649504073782, -1.129261637821651121, 6.016320774579804187 ) ) ;
#33819 = VERTEX_POINT ( 'NONE', #21561 ) ;
#33820 = ORIENTED_EDGE ( 'NONE', *, *, #2025, .T. ) ;
#33821 = EDGE_CURVE ( 'NONE', #45697, #167, #61520, .T. ) ;
#33822 = CARTESIAN_POINT ( 'NONE',  ( -17.65458117747069267, -7.800522896528933714, -9.123980294853460293 ) ) ;
#33823 = ORIENTED_EDGE ( 'NONE', *, *, #53341, .T. ) ;
#33824 =( NAMED_UNIT ( * ) SI_UNIT ( $, .STERADIAN. ) SOLID_ANGLE_UNIT ( ) );
#33825 = CARTESIAN_POINT ( 'NONE',  ( 37.00000000000000711, -11.98254675519226531, 2.220215194442026974 ) ) ;
#33826 = CARTESIAN_POINT ( 'NONE',  ( 3.347841273039249721, -10.61118957148187825, -8.345816669330458737 ) ) ;
#33827 = CIRCLE ( 'NONE', #63539, 12.73084802173761787 ) ;
#33828 = EDGE_CURVE ( 'NONE', #25074, #311, #27191, .T. ) ;
#33829 = LINE ( 'NONE', #17585, #35103 ) ;
#33830 = ORIENTED_EDGE ( 'NONE', *, *, #42431, .T. ) ;
#33831 = CARTESIAN_POINT ( 'NONE',  ( 37.00000000000000711, 8.839356091080166067, 8.389074212634184846 ) ) ;
#33832 = CARTESIAN_POINT ( 'NONE',  ( 1.452237505248555660, -12.08199618361510552, -3.767214359061247464 ) ) ;
#33833 = CIRCLE ( 'NONE', #11529, 12.18649999999999700 ) ;
#33834 = CARTESIAN_POINT ( 'NONE',  ( 2.263328370262063238, -5.019946231381820390, -5.761609105517779383 ) ) ;
#33835 = ORIENTED_EDGE ( 'NONE', *, *, #53294, .T. ) ;
#33836 = ORIENTED_EDGE ( 'NONE', *, *, #11700, .F. ) ;
#33837 = CARTESIAN_POINT ( 'NONE',  ( -35.00000000000000000, -9.896810808925444292, 7.110831038798244741 ) ) ;
#33838 = EDGE_CURVE ( 'NONE', #37783, #14488, #48473, .T. ) ;
#33839 = FACE_OUTER_BOUND ( 'NONE', #46292, .T. ) ;
#33840 = ORIENTED_EDGE ( 'NONE', *, *, #49829, .F. ) ;
#33841 = VERTEX_POINT ( 'NONE', #28184 ) ;
#33842 = DIRECTION ( 'NONE',  ( -1.000000000000000000, 0.000000000000000000, 0.000000000000000000 ) ) ;
#33844 = CIRCLE ( 'NONE', #29567, 2.899999999999994582 ) ;
#33843 = CARTESIAN_POINT ( 'NONE',  ( -27.09833916700337397, -1.609723001518240659, 1.689564470273824837 ) ) ;
#33845 = CARTESIAN_POINT ( 'NONE',  ( 2.889800649504073782, -4.732281052280285394, -3.882893708502096697 ) ) ;
#33846 = CARTESIAN_POINT ( 'NONE',  ( -35.00000000000000000, -1.171570255487366152, -11.68758509253249400 ) ) ;
#33847 = CARTESIAN_POINT ( 'NONE',  ( 1.452237505248555660, -5.807998527925970933, 11.24427360515640295 ) ) ;
#33848 = DIRECTION ( 'NONE',  ( -1.000000000000000000, -1.836970198721029688E-16, 0.000000000000000000 ) ) ;
#33849 = VECTOR ( 'NONE', #21376, 1000.000000000000000 ) ;
#33850 = PRESENTATION_LAYER_ASSIGNMENT (  '', '', ( #22176 ) ) ;
#33851 = ORIENTED_EDGE ( 'NONE', *, *, #5961, .T. ) ;
#33852 = LINE ( 'NONE', #2317, #64515 ) ;
#33853 = EDGE_CURVE ( 'NONE', #55855, #36091, #38163, .T. ) ;
#33854 = CARTESIAN_POINT ( 'NONE',  ( 0.2651627923886306637, 7.938954356958216607, -9.324231535593035858 ) ) ;
#33855 = AXIS2_PLACEMENT_3D ( 'NONE', #30182, #29513, #4265 ) ;
#33856 = PRODUCT ( 'motion translator_ISO - Spur gear 0.25M 58T 20PA 2FW ---S58B6H18L3.0N', 'motion translator_ISO - Spur gear 0.25M 58T 20PA 2FW ---S58B6H18L3.0N', '', ( #37769 ) ) ;
#33857 = CARTESIAN_POINT ( 'NONE',  ( -19.79851336404619744, -13.40886403912690206, -1.595110065591720083 ) ) ;
#33858 = EDGE_CURVE ( 'NONE', #56666, #1032, #57799, .T. ) ;
#33859 = FACE_OUTER_BOUND ( 'NONE', #29512, .T. ) ;
#33860 = DIRECTION ( 'NONE',  ( -1.000000000000000000, 0.000000000000000000, -0.000000000000000000 ) ) ;
#33861 = CARTESIAN_POINT ( 'NONE',  ( -27.08485414902845534, 1.620258667553448051, -1.622802444813711054 ) ) ;
#33862 = CARTESIAN_POINT ( 'NONE',  ( -27.08429572838383947, 1.338867938658203860, 1.859677275556406384 ) ) ;
#33863 = CARTESIAN_POINT ( 'NONE',  ( 0.2767916011545382138, -11.57477803659170768, -4.010899340181539152 ) ) ;
#33864 = AXIS2_PLACEMENT_3D ( 'NONE', #22095, #62015, #1515 ) ;
#33865 = LINE ( 'NONE', #40485, #45908 ) ;
#33866 = ADVANCED_FACE ( 'NONE', ( #37824 ), #61743, .F. ) ;
#33867 = ORIENTED_EDGE ( 'NONE', *, *, #47313, .T. ) ;
#33868 = DIRECTION ( 'NONE',  ( 0.000000000000000000, 0.5243256840888502746, 0.8515178078024904229 ) ) ;
#33869 = ADVANCED_FACE ( 'NONE', ( #48154 ), #29891, .T. ) ;
#33870 = EDGE_CURVE ( 'NONE', #62784, #51848, #19642, .T. ) ;
#33871 = ORIENTED_EDGE ( 'NONE', *, *, #51656, .F. ) ;
#33872 = CARTESIAN_POINT ( 'NONE',  ( -11.35260098629715309, -8.408840821862247239, 8.581102366670037895 ) ) ;
#33873 = CARTESIAN_POINT ( 'NONE',  ( 37.00000000000000711, -12.16632754454236043, 0.7008968033240018380 ) ) ;
#33874 = DIRECTION ( 'NONE',  ( 1.000000000000000000, 0.000000000000000000, 0.000000000000000000 ) ) ;
#33875 = EDGE_CURVE ( 'NONE', #60939, #26603, #31752, .T. ) ;
#33876 = CARTESIAN_POINT ( 'NONE',  ( -22.30625920655495165, -2.750410778797871547, -2.610366806364701642 ) ) ;
#33877 = CARTESIAN_POINT ( 'NONE',  ( 37.00000000000000711, 11.95840593935204765, 2.346765782874299155 ) ) ;
#33878 = ORIENTED_EDGE ( 'NONE', *, *, #59985, .T. ) ;
#33879 = DIRECTION ( 'NONE',  ( 0.000000000000000000, -0.01356324068817991828, 0.9999080150203990547 ) ) ;
#33880 = CARTESIAN_POINT ( 'NONE',  ( 22.68159425457230682, -4.559965384753717821, 12.70733236524612764 ) ) ;
#33881 = CARTESIAN_POINT ( 'NONE',  ( -27.08506889328328171, 2.083363953276920366, 0.9597901767732474054 ) ) ;
#33882 = CARTESIAN_POINT ( 'NONE',  ( -22.30398854582848145, 2.724439933030925687, 2.594196582746961965 ) ) ;
#33883 = AXIS2_PLACEMENT_3D ( 'NONE', #19127, #60030, #14447 ) ;
#33884 = DIRECTION ( 'NONE',  ( 0.000000000000000000, 0.000000000000000000, 1.000000000000000000 ) ) ;
#33885 = ORIENTED_EDGE ( 'NONE', *, *, #170, .T. ) ;
#33886 = AXIS2_PLACEMENT_3D ( 'NONE', #64440, #53526, #39176 ) ;
#33887 = CARTESIAN_POINT ( 'NONE',  ( -18.11253622212529280, 11.56839684805698276, 3.263418409390943076 ) ) ;
#33888 = EDGE_LOOP ( 'NONE', ( #22970, #32505, #8014, #49844 ) ) ;
#33889 = CARTESIAN_POINT ( 'NONE',  ( -35.04582288351658548, 0.006225574250530754340, -0.01107592729723687851 ) ) ;
#33890 = CARTESIAN_POINT ( 'NONE',  ( -9.668839327557112284, -32.14098936784372285, 13.07247934321766181 ) ) ;
#33891 = DIRECTION ( 'NONE',  ( -1.000000000000000000, 0.000000000000000000, 0.000000000000000000 ) ) ;
#33892 = DIRECTION ( 'NONE',  ( 0.000000000000000000, 0.01356324068817998940, -0.9999080150203990547 ) ) ;
#33893 = CIRCLE ( 'NONE', #47714, 2.899999999999994582 ) ;
#33894 = ADVANCED_FACE ( 'NONE', ( #41745 ), #37075, .T. ) ;
#33895 = VERTEX_POINT ( 'NONE', #48064 ) ;
#33896 = ORIENTED_EDGE ( 'NONE', *, *, #34332, .F. ) ;
#33897 = DIRECTION ( 'NONE',  ( 0.000000000000000000, -0.9868265225415276953, 0.1617819965527551584 ) ) ;
#33898 = AXIS2_PLACEMENT_3D ( 'NONE', #65760, #51509, #20886 ) ;
#33899 = DIRECTION ( 'NONE',  ( 1.000000000000000000, -0.000000000000000000, -0.000000000000000000 ) ) ;
#33900 = CARTESIAN_POINT ( 'NONE',  ( 37.00000000000000711, 11.05394794832829497, -5.130401251914769922 ) ) ;
#33901 = CARTESIAN_POINT ( 'NONE',  ( 35.00000000000000000, 11.91791701451269780, 2.544412758415707909 ) ) ;
#33902 = CARTESIAN_POINT ( 'NONE',  ( 1.719304012339819332, -7.581471372739574832, 10.22720798541442555 ) ) ;
#33903 = ORIENTED_EDGE ( 'NONE', *, *, #59206, .F. ) ;
#33904 = EDGE_CURVE ( 'NONE', #21663, #61727, #2061, .T. ) ;
#33905 = ORIENTED_EDGE ( 'NONE', *, *, #21521, .F. ) ;
#33906 = CIRCLE ( 'NONE', #57280, 3.000000000000000444 ) ;
#33907 = ORIENTED_EDGE ( 'NONE', *, *, #535, .T. ) ;
#33908 = FACE_OUTER_BOUND ( 'NONE', #25455, .T. ) ;
#33909 = CARTESIAN_POINT ( 'NONE',  ( -36.00000000000000711, 11.96656215839369253, 4.400442035670988794 ) ) ;
#33910 = ORIENTED_EDGE ( 'NONE', *, *, #29005, .T. ) ;
#33911 = CARTESIAN_POINT ( 'NONE',  ( -35.00000000000000000, 9.908974237959645492, 6.307491713049065751 ) ) ;
#33912 = LINE ( 'NONE', #27288, #49168 ) ;
#33913 = ORIENTED_EDGE ( 'NONE', *, *, #53199, .T. ) ;
#33914 = CARTESIAN_POINT ( 'NONE',  ( 2.373367633546870969, 7.151506276328627898, 2.795365972209097549 ) ) ;
#33915 = CARTESIAN_POINT ( 'NONE',  ( 2.241317068080781905, -2.696905536171245732, -7.142175514530103797 ) ) ;
#33916 = CARTESIAN_POINT ( 'NONE',  ( 1.000000000000000888, -4.604744433234713163, 5.919993978425451608 ) ) ;
#33917 = VERTEX_POINT ( 'NONE', #21474 ) ;
#33918 = VERTEX_POINT ( 'NONE', #52059 ) ;
#33919 = LINE ( 'NONE', #13635, #43779 ) ;
#33920 = EDGE_CURVE ( 'NONE', #58860, #9046, #34923, .T. ) ;
#33921 = ORIENTED_EDGE ( 'NONE', *, *, #51716, .T. ) ;
#33922 = CARTESIAN_POINT ( 'NONE',  ( 35.00000000000000000, -11.47758908105696207, -2.497432891016804657 ) ) ;
#33923 = EDGE_LOOP ( 'NONE', ( #58163, #54456, #25114, #42840 ) ) ;
#33924 = ORIENTED_EDGE ( 'NONE', *, *, #60292, .T. ) ;
#33925 = VERTEX_POINT ( 'NONE', #1194 ) ;
#33926 = CARTESIAN_POINT ( 'NONE',  ( 47.00000000000000711, 4.705694406421931860E-17, -3.469127814946512892E-15 ) ) ;
#33927 = DIRECTION ( 'NONE',  ( 0.000000000000000000, 0.9718671068226467646, -0.2355298848897482977 ) ) ;
#33929 = CARTESIAN_POINT ( 'NONE',  ( 2.941278708680199916, 3.842273877444625896, -4.788765081995591366 ) ) ;
#33928 = CIRCLE ( 'NONE', #42400, 4.999999999999998224 ) ;
#33930 = CARTESIAN_POINT ( 'NONE',  ( -8.891032880924177206, 25.00000000000000000, -3.860857758255646921 ) ) ;
#33931 = DIRECTION ( 'NONE',  ( 0.000000000000000000, 0.9999080150203990547, 0.01356324068817645230 ) ) ;
#33932 = ORIENTED_EDGE ( 'NONE', *, *, #53860, .T. ) ;
#33933 = CARTESIAN_POINT ( 'NONE',  ( -22.30625920655495165, -3.403091720605013748, -1.672644928563079780 ) ) ;
#33934 = ORIENTED_EDGE ( 'NONE', *, *, #63129, .F. ) ;
#33935 = AXIS2_PLACEMENT_3D ( 'NONE', #45990, #56276, #30364 ) ;
#33936 = CARTESIAN_POINT ( 'NONE',  ( -35.00000000000000000, 11.30684963584389280, 4.545979934229452901 ) ) ;
#33937 = CARTESIAN_POINT ( 'NONE',  ( -19.69476066079020171, -4.201994156881551312, -12.82938989607585789 ) ) ;
#33938 = ORIENTED_EDGE ( 'NONE', *, *, #37912, .T. ) ;
#33939 = DIRECTION ( 'NONE',  ( 0.000000000000000000, 0.6051742151937661296, -0.7960930657056429771 ) ) ;
#33940 = CARTESIAN_POINT ( 'NONE',  ( 2.080613030138688480, 5.400000000000000355, 1.000000000000000000 ) ) ;
#33941 = CARTESIAN_POINT ( 'NONE',  ( 2.717984159219104079, -7.620583877640514814, 1.631703089059925338 ) ) ;
#33942 = ADVANCED_FACE ( 'NONE', ( #52399 ), #32023, .F. ) ;
#33943 = EDGE_LOOP ( 'NONE', ( #17264, #9568, #24869, #48655 ) ) ;
#33944 = ORIENTED_EDGE ( 'NONE', *, *, #16611, .T. ) ;
#33945 = CARTESIAN_POINT ( 'NONE',  ( -27.08429572838383947, -2.217805374070538349, 0.5764601019425888984 ) ) ;
#33946 = ADVANCED_FACE ( 'NONE', ( #16489 ), #37069, .F. ) ;
#33947 = CIRCLE ( 'NONE', #11641, 6.936499999999992561 ) ;
#33948 = ORIENTED_EDGE ( 'NONE', *, *, #15529, .F. ) ;
#33949 = DIRECTION ( 'NONE',  ( -1.000000000000000000, 0.000000000000000000, 0.000000000000000000 ) ) ;
#33950 = DIRECTION ( 'NONE',  ( -1.000000000000000000, -0.000000000000000000, 0.000000000000000000 ) ) ;
#33951 = CARTESIAN_POINT ( 'NONE',  ( -29.95040744112532494, 0.8263397880752897384, 13.47653596729246672 ) ) ;
#33952 = EDGE_CURVE ( 'NONE', #14132, #37036, #24441, .T. ) ;
#33953 = CARTESIAN_POINT ( 'NONE',  ( 0.2911222467163562255, -9.248441845564627783, -8.040284153519465349 ) ) ;
#33954 = CYLINDRICAL_SURFACE ( 'NONE', #4182, 12.18649999999999878 ) ;
#33955 = ORIENTED_EDGE ( 'NONE', *, *, #9994, .T. ) ;
#33956 = VECTOR ( 'NONE', #40207, 1000.000000000000000 ) ;
#33957 = CARTESIAN_POINT ( 'NONE',  ( 37.00000000000000711, -11.13736569743270799, 4.946702696913285457 ) ) ;
#33958 = CARTESIAN_POINT ( 'NONE',  ( 35.00000000000000000, -8.699265615723042799, -8.534258022646065811 ) ) ;
#33959 = CARTESIAN_POINT ( 'NONE',  ( -16.81808179455697427, -29.42526233323303941, -9.774508714121761699 ) ) ;
#33960 = CARTESIAN_POINT ( 'NONE',  ( -35.00000000000000000, -4.725891942574680371, -10.75351884295732496 ) ) ;
#33961 = CARTESIAN_POINT ( 'NONE',  ( -22.39032720737627002, 3.916738514147016126, 0.9101257950220676962 ) ) ;
#33962 = CARTESIAN_POINT ( 'NONE',  ( 0.2653141334712595389, 7.905403790036969802, 9.352759824582522086 ) ) ;
#33963 = DIRECTION ( 'NONE',  ( -1.000000000000000000, 0.000000000000000000, 0.000000000000000000 ) ) ;
#33964 = DIRECTION ( 'NONE',  ( -1.000000000000000000, -0.000000000000000000, 0.000000000000000000 ) ) ;
#33965 = AXIS2_PLACEMENT_3D ( 'NONE', #16042, #26690, #52310 ) ;
#33966 = ADVANCED_FACE ( 'NONE', ( #7149 ), #63007, .T. ) ;
#33967 = CIRCLE ( 'NONE', #36089, 2.899999999999995470 ) ;
#33968 = VERTEX_POINT ( 'NONE', #23779 ) ;
#33969 = CARTESIAN_POINT ( 'NONE',  ( -35.00000000000000000, 0.01609748574461371262, -11.74614673114903951 ) ) ;
#33970 = ADVANCED_FACE ( 'NONE', ( #28106 ), #63993, .T. ) ;
#33971 = ORIENTED_EDGE ( 'NONE', *, *, #43413, .F. ) ;
#33973 =( BOUNDED_SURFACE ( )  B_SPLINE_SURFACE ( 3, 1, ( 
 ( #44488, #65108 ),
 ( #19579, #1262 ),
 ( #4938, #21191 ),
 ( #31187, #10549 ) ),
 .UNSPECIFIED., .F., .F., .F. ) 
 B_SPLINE_SURFACE_WITH_KNOTS ( ( 4, 4 ),
 ( 2, 2 ),
 ( 0.000000000000000000, 1.000000000000000000 ),
 ( 0.000000000000000000, 1.000000000000000000 ),
 .UNSPECIFIED. ) 
 GEOMETRIC_REPRESENTATION_ITEM ( )  RATIONAL_B_SPLINE_SURFACE ( (
 ( 1.000000000000000000, 1.000000000000000000),
 ( 0.6933888150995267674, 0.9895912004443193632),
 ( 0.6933888150995267674, 0.9895912004443193632),
 ( 1.000000000000000000, 1.000000000000000000) ) ) 
 REPRESENTATION_ITEM ( '' )  SURFACE ( )  );
#33972 = FACE_OUTER_BOUND ( 'NONE', #4074, .T. ) ;
#33974 = DIRECTION ( 'NONE',  ( -1.000000000000000000, -0.000000000000000000, -0.000000000000000000 ) ) ;
#33975 = CARTESIAN_POINT ( 'NONE',  ( 0.2650492594609231700, 6.027447650185369099, 10.66007682546619506 ) ) ;
#33976 = DIRECTION ( 'NONE',  ( -1.000000000000000000, 0.000000000000000000, 0.000000000000000000 ) ) ;
#33977 = ORIENTED_EDGE ( 'NONE', *, *, #25082, .F. ) ;
#33978 = ADVANCED_FACE ( 'NONE', ( #14421 ), #36697, .F. ) ;
#33979 = VERTEX_POINT ( 'NONE', #2847 ) ;
#33980 = VERTEX_POINT ( 'NONE', #53708 ) ;
#33981 = CARTESIAN_POINT ( 'NONE',  ( 0.3537226245948354442, -7.688925565304952414, -9.569332148897542467 ) ) ;
#33982 = VECTOR ( 'NONE', #11821, 1000.000000000000000 ) ;
#33983 = ORIENTED_EDGE ( 'NONE', *, *, #40505, .F. ) ;
#33984 = CYLINDRICAL_SURFACE ( 'NONE', #16467, 12.75000000000000178 ) ;
#33985 = CARTESIAN_POINT ( 'NONE',  ( 2.573738926104374602, -2.868819712476760042, 7.194322927777948351 ) ) ;
#33986 = AXIS2_PLACEMENT_3D ( 'NONE', #18865, #34137, #39129 ) ;
#33987 = CARTESIAN_POINT ( 'NONE',  ( 0.2833330754217400771, 10.50818856955517866, 6.300330022379253769 ) ) ;
#33988 = CYLINDRICAL_SURFACE ( 'NONE', #51342, 3.309571291727934295 ) ;
#33989 = ORIENTED_EDGE ( 'NONE', *, *, #5245, .F. ) ;
#33990 = DIRECTION ( 'NONE',  ( 1.000000000000000000, 0.000000000000000000, 0.000000000000000000 ) ) ;
#33991 = DIRECTION ( 'NONE',  ( -1.000000000000000000, 0.000000000000000000, 0.000000000000000000 ) ) ;
#33992 = FACE_OUTER_BOUND ( 'NONE', #783, .T. ) ;
#33994 = ORIENTED_EDGE ( 'NONE', *, *, #24953, .T. ) ;
#33993 = CYLINDRICAL_SURFACE ( 'NONE', #16037, 1.399999999999999911 ) ;
#33995 = EDGE_CURVE ( 'NONE', #19006, #48895, #56209, .T. ) ;
#33996 = ADVANCED_FACE ( 'NONE', ( #8142 ), #43476, .T. ) ;
#33997 = VERTEX_POINT ( 'NONE', #29087 ) ;
#33998 = CARTESIAN_POINT ( 'NONE',  ( 0.2717059086739033180, -6.276007891175655828, -10.51822005842000785 ) ) ;
#33999 = AXIS2_PLACEMENT_3D ( 'NONE', #12173, #2558, #18159 ) ;
#34000 = ORIENTED_EDGE ( 'NONE', *, *, #3309, .F. ) ;
#34001 = CARTESIAN_POINT ( 'NONE',  ( 21.62617364511530837, -11.90943727674767416, -1.526638328776592779 ) ) ;
#34002 = DIRECTION ( 'NONE',  ( 0.000000000000000000, 0.000000000000000000, 1.000000000000000000 ) ) ;
#34003 = ADVANCED_FACE ( 'NONE', ( #49057 ), #14099, .T. ) ;
#34004 = CARTESIAN_POINT ( 'NONE',  ( 0.9232058338315048962, -8.301689855530229423, 9.306586124266566173 ) ) ;
#34005 = CARTESIAN_POINT ( 'NONE',  ( -2.952869152607106251, 11.39722960915212724, 3.755417052241485365 ) ) ;
#34006 = FACE_OUTER_BOUND ( 'NONE', #46456, .T. ) ;
#34007 = FACE_OUTER_BOUND ( 'NONE', #48553, .T. ) ;
#34008 = DIRECTION ( 'NONE',  ( 1.000000000000000000, 0.000000000000000000, 0.000000000000000000 ) ) ;
#34009 = AXIS2_PLACEMENT_3D ( 'NONE', #35886, #45551, #30912 ) ;
#34010 = ORIENTED_EDGE ( 'NONE', *, *, #27357, .T. ) ;
#34011 = CARTESIAN_POINT ( 'NONE',  ( 2.000000000000001776, -0.3246585432986597852, 6.805031400696099020 ) ) ;
#34012 = ORIENTED_EDGE ( 'NONE', *, *, #44714, .F. ) ;
#34013 = VERTEX_POINT ( 'NONE', #64626 ) ;
#34014 = DIRECTION ( 'NONE',  ( -1.000000000000000000, 0.000000000000000000, 0.000000000000000000 ) ) ;
#34015 = DIRECTION ( 'NONE',  ( 0.000000000000000000, 0.000000000000000000, 1.000000000000000000 ) ) ;
#34016 = FACE_OUTER_BOUND ( 'NONE', #18576, .T. ) ;
#34017 = CARTESIAN_POINT ( 'NONE',  ( -22.30527770659433173, 2.100259071719474235, 3.125767038151177513 ) ) ;
#34018 = LINE ( 'NONE', #37715, #23147 ) ;
#34019 = EDGE_CURVE ( 'NONE', #12979, #59777, #63305, .T. ) ;
#34020 = CARTESIAN_POINT ( 'NONE',  ( 0.3401186441510234415, 10.75260364139053415, -5.912862694513600026 ) ) ;
#34021 = AXIS2_PLACEMENT_3D ( 'NONE', #13918, #8956, #23606 ) ;
#34022 = CIRCLE ( 'NONE', #30826, 4.999999999999998224 ) ;
#34023 = CIRCLE ( 'NONE', #54210, 12.74999999999999822 ) ;
#34024 = CIRCLE ( 'NONE', #3242, 12.18650000000000055 ) ;
#34025 = DIRECTION ( 'NONE',  ( 0.3865475372811021382, -0.7187975063895761796, 0.5778504531710970671 ) ) ;
#34026 = EDGE_CURVE ( 'NONE', #38075, #20003, #31799, .T. ) ;
#34027 = ORIENTED_EDGE ( 'NONE', *, *, #21713, .F. ) ;
#34028 = CARTESIAN_POINT ( 'NONE',  ( -35.00000000000000000, 3.511814412392118445, 11.66953048682401040 ) ) ;
#34029 = CARTESIAN_POINT ( 'NONE',  ( -35.00000000000000000, 6.475373545682302279, 10.32377448871670467 ) ) ;
#34030 = CARTESIAN_POINT ( 'NONE',  ( -17.14880393894236832, -7.773003649151587702, 11.04270090464071075 ) ) ;
#34031 = ORIENTED_EDGE ( 'NONE', *, *, #59994, .T. ) ;
#34032 = CIRCLE ( 'NONE', #36156, 12.18650000000000233 ) ;
#34033 = CIRCLE ( 'NONE', #6427, 5.000000000000001776 ) ;
#34034 = AXIS2_PLACEMENT_3D ( 'NONE', #42455, #54447, #43799 ) ;
#34035 = CARTESIAN_POINT ( 'NONE',  ( 35.00000000000000000, 11.01837265713072966, -6.415447294506745557 ) ) ;
#34036 = AXIS2_PLACEMENT_3D ( 'NONE', #39178, #32869, #48220 ) ;
#34037 = LINE ( 'NONE', #34683, #39495 ) ;
#34038 = VERTEX_POINT ( 'NONE', #4138 ) ;
#34039 = CARTESIAN_POINT ( 'NONE',  ( 5.536195898058073439, 0.006344799443924024202, -0.005656495196971017721 ) ) ;
#34040 = CARTESIAN_POINT ( 'NONE',  ( 0.3040950598368152291, -11.43390362554256257, 4.428852722102693207 ) ) ;
#34041 = CARTESIAN_POINT ( 'NONE',  ( 37.00000000000000711, 4.705694406421931860E-17, -3.469127814946512892E-15 ) ) ;
#34042 = AXIS2_PLACEMENT_3D ( 'NONE', #30266, #65179, #50562 ) ;
#34043 = CARTESIAN_POINT ( 'NONE',  ( -35.00000000000000000, 0.000000000000000000, 0.000000000000000000 ) ) ;
#34044 = CARTESIAN_POINT ( 'NONE',  ( 3.459614771489464946, -11.09853614738469396, 7.685863346768216253 ) ) ;
#34045 = VECTOR ( 'NONE', #57085, 1000.000000000000000 ) ;
#34046 = EDGE_CURVE ( 'NONE', #52529, #25546, #8464, .T. ) ;
#34047 = ORIENTED_EDGE ( 'NONE', *, *, #32320, .F. ) ;
#34048 = CARTESIAN_POINT ( 'NONE',  ( 3.152665057734040488, 0.000000000000000000, 0.000000000000000000 ) ) ;
#34049 = CARTESIAN_POINT ( 'NONE',  ( 0.3053067050349171918, -12.11120005789972609, 1.901204202464632287 ) ) ;
#34050 = CARTESIAN_POINT ( 'NONE',  ( -22.27384469013076185, -2.985904959940905545, 2.154627400808026838 ) ) ;
#34051 = ORIENTED_EDGE ( 'NONE', *, *, #39285, .F. ) ;
#34052 = CARTESIAN_POINT ( 'NONE',  ( 8.626064170299294176, 3.158121739564950126, 13.12798721807445368 ) ) ;
#34053 = CIRCLE ( 'NONE', #57425, 4.999999999999999112 ) ;
#34054 = CYLINDRICAL_SURFACE ( 'NONE', #40462, 7.499999999999988454 ) ;
#34055 = VERTEX_POINT ( 'NONE', #60000 ) ;
#34056 =( REPRESENTATION_RELATIONSHIP ('NONE','NONE', #63658, #13953 ) REPRESENTATION_RELATIONSHIP_WITH_TRANSFORMATION ( #38420 )SHAPE_REPRESENTATION_RELATIONSHIP( ) );
#34057 = ORIENTED_EDGE ( 'NONE', *, *, #51926, .F. ) ;
#34058 = CARTESIAN_POINT ( 'NONE',  ( 37.00000000000000711, 8.258652103341434625, -8.352657516904704593 ) ) ;
#34059 = VECTOR ( 'NONE', #50674, 1000.000000000000114 ) ;
#34060 = EDGE_CURVE ( 'NONE', #48764, #43267, #24404, .T. ) ;
#34061 = ORIENTED_EDGE ( 'NONE', *, *, #21484, .F. ) ;
#34062 = CARTESIAN_POINT ( 'NONE',  ( 19.13486214123187423, 6.258902428715833466, 11.96274114462061533 ) ) ;
#34063 = CARTESIAN_POINT ( 'NONE',  ( 0.2652384770603681829, 6.180206054297750384, -10.57229757085615596 ) ) ;
#34064 = CARTESIAN_POINT ( 'NONE',  ( 0.2759803524722186374, -6.288205958087853098, 10.51260004517010671 ) ) ;
#34065 = CARTESIAN_POINT ( 'NONE',  ( 2.000000000000001776, 6.250523986464036064, -3.007653927006531447 ) ) ;
#34066 = DIRECTION ( 'NONE',  ( 1.000000000000000000, 0.000000000000000000, -0.000000000000000000 ) ) ;
#34068 = ORIENTED_EDGE ( 'NONE', *, *, #50336, .T. ) ;
#34067 = CARTESIAN_POINT ( 'NONE',  ( 0.7446945582507944472, 7.698291984229363116, 9.728576129009507412 ) ) ;
#34069 = CARTESIAN_POINT ( 'NONE',  ( 35.00000000000000000, 4.705694406421931860E-17, -3.469127814946512892E-15 ) ) ;
#34070 = VERTEX_POINT ( 'NONE', #39047 ) ;
#34071 = DIRECTION ( 'NONE',  ( 0.000000000000000000, 0.01356324068818000848, -0.9999080150203990547 ) ) ;
#34072 = ORIENTED_EDGE ( 'NONE', *, *, #26785, .F. ) ;
#34073 = EDGE_LOOP ( 'NONE', ( #29360, #14843, #22830, #36271 ) ) ;
#34074 = CARTESIAN_POINT ( 'NONE',  ( -14.37447982603986141, 8.347221320025207447, 10.61079098056672620 ) ) ;
#34075 = CARTESIAN_POINT ( 'NONE',  ( -4.505835087371258041, -30.89562805149345337, 14.87534964460356512 ) ) ;
#34076 = CARTESIAN_POINT ( 'NONE',  ( -24.30576933614230484, 10.54161591164828415, 8.435916383667265706 ) ) ;
#34077 = CARTESIAN_POINT ( 'NONE',  ( 0.2646305136544072623, -12.08286001766536799, 1.996350543472957151 ) ) ;
#34078 = DIRECTION ( 'NONE',  ( 1.000000000000000000, -0.000000000000000000, 0.000000000000000000 ) ) ;
#34079 = CARTESIAN_POINT ( 'NONE',  ( 2.276905613632195902, 5.955225895209577125, 4.795880183930062657 ) ) ;
#34080 = EDGE_LOOP ( 'NONE', ( #3922, #49891, #52483, #26735 ) ) ;
#34081 = ORIENTED_EDGE ( 'NONE', *, *, #27794, .F. ) ;
#34082 = AXIS2_PLACEMENT_3D ( 'NONE', #17656, #52886, #47907 ) ;
#34083 = CARTESIAN_POINT ( 'NONE',  ( 37.00000000000000711, 6.891188680298960811, 9.512294188640820991 ) ) ;
#34084 = ORIENTED_EDGE ( 'NONE', *, *, #25139, .T. ) ;
#34085 = VECTOR ( 'NONE', #15527, 1000.000000000000000 ) ;
#34086 = CARTESIAN_POINT ( 'NONE',  ( 35.00000000000000000, 1.791059740004421919, -12.05416472667166339 ) ) ;
#34087 = CARTESIAN_POINT ( 'NONE',  ( 0.3675815128205894289, 0.2638082659430137644, -12.27743992903065973 ) ) ;
#34088 = DIRECTION ( 'NONE',  ( 0.000000000000000000, 0.01356324068817992175, -0.9999080150203990547 ) ) ;
#34089 = DIRECTION ( 'NONE',  ( -1.000000000000000000, 0.000000000000000000, 0.000000000000000000 ) ) ;
#34090 = EDGE_CURVE ( 'NONE', #34196, #56385, #23106, .T. ) ;
#34091 = DIRECTION ( 'NONE',  ( -0.9688695217174487784, 0.000000000000000000, 0.2475719085175093481 ) ) ;
#34092 = DIRECTION ( 'NONE',  ( 1.000000000000000000, 0.000000000000000000, 0.000000000000000000 ) ) ;
#34093 = VECTOR ( 'NONE', #13000, 1000.000000000000000 ) ;
#34094 = ORIENTED_EDGE ( 'NONE', *, *, #34210, .T. ) ;
#34095 = ORIENTED_EDGE ( 'NONE', *, *, #13428, .T. ) ;
#34096 = CARTESIAN_POINT ( 'NONE',  ( 0.7446945582511054207, 3.906659168237073487, 11.77484212699327415 ) ) ;
#34097 = CARTESIAN_POINT ( 'NONE',  ( -35.00000000000000000, 0.000000000000000000, 0.000000000000000000 ) ) ;
#34098 = CARTESIAN_POINT ( 'NONE',  ( 37.00000000000000711, -6.950793414699864670, -10.68873102412840304 ) ) ;
#34099 = EDGE_CURVE ( 'NONE', #19106, #56769, #54365, .T. ) ;
#34100 = AXIS2_PLACEMENT_3D ( 'NONE', #19606, #34848, #9587 ) ;
#34101 = AXIS2_PLACEMENT_3D ( 'NONE', #11388, #17035, #17379 ) ;
#34102 = CARTESIAN_POINT ( 'NONE',  ( 2.990245332647884613, -0.9653152459622390547, -8.426135047918871024 ) ) ;
#34103 = AXIS2_PLACEMENT_3D ( 'NONE', #40416, #60719, #55737 ) ;
#34104 = CARTESIAN_POINT ( 'NONE',  ( -27.87914506689667959, 11.20956315821615412, -7.546760284812030761 ) ) ;
#34105 = CARTESIAN_POINT ( 'NONE',  ( -6.413058664601522629, -1.625581343069429474, -11.88948361578930069 ) ) ;
#34106 = DIRECTION ( 'NONE',  ( 0.000000000000000000, -1.000000000000000000, 0.000000000000000000 ) ) ;
#34107 = CARTESIAN_POINT ( 'NONE',  ( 2.244591118396557228, 1.431619869711851400, 7.500068934084574757 ) ) ;
#34108 = CYLINDRICAL_SURFACE ( 'NONE', #33965, 6.936499999999988120 ) ;
#34109 = ORIENTED_EDGE ( 'NONE', *, *, #43658, .F. ) ;
#34110 = CARTESIAN_POINT ( 'NONE',  ( 3.092491956584956014, -6.343509225034599908, -4.738927301402582337 ) ) ;
#34111 = CARTESIAN_POINT ( 'NONE',  ( -37.00000000000000711, 7.251710744571578715, 9.240395740215660680 ) ) ;
#34112 = CARTESIAN_POINT ( 'NONE',  ( -35.00000000000000000, 0.000000000000000000, 0.000000000000000000 ) ) ;
#34113 = B_SPLINE_CURVE_WITH_KNOTS ( 'NONE', 3,
 ( #59770, #60092, #4239, #34152, #33822, #53807, #14199, #59434, #29487, #44783, #65066, #39140, #24507, #39807, #28204, #8243, #44448, #3617, #64726, #3270 ),
 .UNSPECIFIED., .F., .F.,
 ( 4, 2, 2, 2, 2, 2, 2, 2, 2, 4 ),
 ( 4.906538933386796626E-18, 0.001836704664428997482, 0.002755056996643492646, 0.003673409328857988026, 0.004591761661072483840, 0.005050937827179729361, 0.005510113993286975750, 0.006428466325501474600, 0.006887642491608728795, 0.007346818657715982991 ),
 .UNSPECIFIED. ) ;
#34114 = CIRCLE ( 'NONE', #42605, 16.19615242270663558 ) ;
#34115 = CIRCLE ( 'NONE', #42606, 4.999999999999999112 ) ;
#34116 = EDGE_CURVE ( 'NONE', #62051, #3315, #18120, .T. ) ;
#34117 = AXIS2_PLACEMENT_3D ( 'NONE', #30440, #19498, #55056 ) ;
#34118 = CARTESIAN_POINT ( 'NONE',  ( 37.25000000000000711, -1.694065894508600678E-18, 0.000000000000000000 ) ) ;
#34119 = CARTESIAN_POINT ( 'NONE',  ( 2.253265082352432724, -5.932955906470540164, 4.810902415501113083 ) ) ;
#34120 = EDGE_CURVE ( 'NONE', #11257, #63179, #23329, .T. ) ;
#34121 = ORIENTED_EDGE ( 'NONE', *, *, #2414, .T. ) ;
#34122 = EDGE_CURVE ( 'NONE', #60252, #13554, #55163, .T. ) ;
#34123 = CARTESIAN_POINT ( 'NONE',  ( 2.276905613633648962, -2.469846004795358763, 7.236369456722870908 ) ) ;
#34124 = CARTESIAN_POINT ( 'NONE',  ( 27.62838931380291996, 25.00000000000000000, -3.066727421130092779 ) ) ;
#34125 = CARTESIAN_POINT ( 'NONE',  ( -12.89187373143239945, -27.44222185127960145, -12.55025375818352629 ) ) ;
#34126 = ORIENTED_EDGE ( 'NONE', *, *, #21728, .T. ) ;
#34127 = ADVANCED_FACE ( 'NONE', ( #54994 ), #18839, .F. ) ;
#34128 = CARTESIAN_POINT ( 'NONE',  ( -7.145635969647290864, -1.338498515901911157, -13.43367374991614227 ) ) ;
#34129 = CARTESIAN_POINT ( 'NONE',  ( 35.00000000000000000, 11.38112321385050585, -2.905556151562669331 ) ) ;
#34130 = B_SPLINE_CURVE_WITH_KNOTS ( 'NONE', 3,
 ( #22927, #11943, #18266, #48525, #33213, #52543, #21938, #2977, #27905, #63455, #32226, #11618, #23239, #53524, #6971, #42187, #26925, #7966, #47225 ),
 .UNSPECIFIED., .F., .F.,
 ( 4, 3, 3, 3, 3, 3, 4 ),
 ( 8.251341272764500075E-18, 2.825908398783091627E-05, 4.208813692418309291E-05, 5.591713746860777948E-05, 6.279584083140069212E-05, 9.105792820167411068E-05, 0.0001153131102489391135 ),
 .UNSPECIFIED. ) ;
#34131 = CARTESIAN_POINT ( 'NONE',  ( 18.06755238356944204, -8.467740623938468048, 10.54028520740660646 ) ) ;
#34132 = AXIS2_PLACEMENT_3D ( 'NONE', #10464, #30739, #25780 ) ;
#34133 = CARTESIAN_POINT ( 'NONE',  ( 0.2759803524722221346, -8.018167820447549943, 9.260954523383706061 ) ) ;
#34134 = B_SPLINE_CURVE_WITH_KNOTS ( 'NONE', 3,
 ( #37942, #53251, #7698, #22995, #27982, #24200, #58582, #8036, #38259, #32293, #59786, #48289, #2736, #43250 ),
 .UNSPECIFIED., .F., .F.,
 ( 4, 2, 2, 2, 2, 2, 4 ),
 ( 2.453269466693398698E-18, 0.001754878791416509013, 0.002632318187124761677, 0.003509757582833014124, 0.004387196978541266570, 0.005264636374249519017, 0.007019515165666019574 ),
 .UNSPECIFIED. ) ;
#34135 = DIRECTION ( 'NONE',  ( 1.000000000000000000, 0.000000000000000000, 0.000000000000000000 ) ) ;
#34136 = EDGE_CURVE ( 'NONE', #325, #11644, #46669, .T. ) ;
#34137 = DIRECTION ( 'NONE',  ( -1.000000000000000000, 0.000000000000000000, 0.000000000000000000 ) ) ;
#34138 = EDGE_LOOP ( 'NONE', ( #22164, #45723, #53316, #44632 ) ) ;
#34139 = CARTESIAN_POINT ( 'NONE',  ( -35.00000000000000000, -1.030638227056651424, 12.14284015767849567 ) ) ;
#34140 = CIRCLE ( 'NONE', #47936, 5.000000000000002665 ) ;
#34141 = CARTESIAN_POINT ( 'NONE',  ( 5.514970785353741078, -0.002093325033903841153, 0.004233694591582948079 ) ) ;
#34142 = CARTESIAN_POINT ( 'NONE',  ( -17.54726996257253191, 12.93490414535030020, 3.865003848717349033 ) ) ;
#34143 = DIRECTION ( 'NONE',  ( -1.000000000000000000, 0.000000000000000000, 0.000000000000000000 ) ) ;
#34144 = CARTESIAN_POINT ( 'NONE',  ( 2.298277635560286303, 7.564013289873170898, -1.166137492762147287 ) ) ;
#34145 = DIRECTION ( 'NONE',  ( 1.000000000000000000, 0.000000000000000000, 0.000000000000000000 ) ) ;
#34146 = ADVANCED_FACE ( 'NONE', ( #19767 ), #25077, .F. ) ;
#34147 = CARTESIAN_POINT ( 'NONE',  ( -35.00000000000000000, 0.000000000000000000, 0.000000000000000000 ) ) ;
#34148 = CARTESIAN_POINT ( 'NONE',  ( -35.00000000000000000, 0.000000000000000000, 0.000000000000000000 ) ) ;
#34149 = ORIENTED_EDGE ( 'NONE', *, *, #8619, .F. ) ;
#34150 = CIRCLE ( 'NONE', #57536, 2.899999999999995914 ) ;
#34151 = ORIENTED_EDGE ( 'NONE', *, *, #14740, .T. ) ;
#34152 = CARTESIAN_POINT ( 'NONE',  ( -17.68631299100147203, -8.034711453839296524, -8.918265921354986858 ) ) ;
#34153 = ORIENTED_EDGE ( 'NONE', *, *, #4890, .T. ) ;
#34154 =( LENGTH_UNIT ( ) NAMED_UNIT ( * ) SI_UNIT ( .MILLI., .METRE. ) );
#34156 = DIRECTION ( 'NONE',  ( -1.000000000000000000, 0.000000000000000000, 0.000000000000000000 ) ) ;
#34155 = VECTOR ( 'NONE', #25817, 1000.000000000000000 ) ;
#34157 = CONICAL_SURFACE ( 'NONE', #11849, 12.73084802173761787, 0.3217505529694027477 ) ;
#34158 = AXIS2_PLACEMENT_3D ( 'NONE', #30378, #50997, #15410 ) ;
#34159 = EDGE_CURVE ( 'NONE', #56656, #63445, #30051, .T. ) ;
#34160 = FACE_OUTER_BOUND ( 'NONE', #5543, .T. ) ;
#34161 = VERTEX_POINT ( 'NONE', #50364 ) ;
#34162 = DIRECTION ( 'NONE',  ( -1.000000000000000000, 0.000000000000000000, 0.000000000000000000 ) ) ;
#34163 =( BOUNDED_SURFACE ( )  B_SPLINE_SURFACE ( 3, 1, ( 
 ( #32251, #27588 ),
 ( #48554, #22273 ),
 ( #43532, #2006 ),
 ( #7651, #27934 ) ),
 .UNSPECIFIED., .F., .F., .F. ) 
 B_SPLINE_SURFACE_WITH_KNOTS ( ( 4, 4 ),
 ( 2, 2 ),
 ( 0.000000000000000000, 1.000000000000000000 ),
 ( 0.000000000000000000, 1.000000000000000000 ),
 .UNSPECIFIED. ) 
 GEOMETRIC_REPRESENTATION_ITEM ( )  RATIONAL_B_SPLINE_SURFACE ( (
 ( 1.000000000000000000, 1.000000000000000000),
 ( 0.9856612449720755231, 0.9999558406602322425),
 ( 0.9856612449720755231, 0.9999558406602322425),
 ( 1.000000000000000000, 1.000000000000000000) ) ) 
 REPRESENTATION_ITEM ( '' )  SURFACE ( )  );
#34164 = CARTESIAN_POINT ( 'NONE',  ( 35.00000000000000000, -1.030638227056475120, 12.14284015767850811 ) ) ;
#34165 = CARTESIAN_POINT ( 'NONE',  ( 23.19610847111811935, -4.580350341167983785, 12.70186574010239866 ) ) ;
#34166 = ORIENTED_EDGE ( 'NONE', *, *, #60195, .F. ) ;
#34167 = EDGE_LOOP ( 'NONE', ( #5398, #14739, #53796, #42173 ) ) ;
#34168 = LINE ( 'NONE', #64111, #23677 ) ;
#34169 = CARTESIAN_POINT ( 'NONE',  ( 37.00000000000000711, -9.240395740215580744, 7.251710744571670197 ) ) ;
#34170 = ORIENTED_EDGE ( 'NONE', *, *, #51064, .F. ) ;
#34171 = ORIENTED_EDGE ( 'NONE', *, *, #32575, .F. ) ;
#34172 = CIRCLE ( 'NONE', #10820, 4.999999999999999112 ) ;
#34173 = CARTESIAN_POINT ( 'NONE',  ( 1.000000000000000888, -7.203928197742102135, 2.086484728383119158 ) ) ;
#34174 = DIRECTION ( 'NONE',  ( 0.000000000000000000, -0.9937233664769749009, 0.1118654143051720229 ) ) ;
#34175 = CARTESIAN_POINT ( 'NONE',  ( 0.2915757698887279648, 10.50410115670278444, -6.312478057070352477 ) ) ;
#34176 = CARTESIAN_POINT ( 'NONE',  ( 2.354167843600960097, -6.278647867796540716, 25.00000000000000000 ) ) ;
#34177 = CARTESIAN_POINT ( 'NONE',  ( -35.00000000000000000, 11.53507381115580444, 2.216820770815288721 ) ) ;
#34178 = VECTOR ( 'NONE', #53020, 1000.000000000000000 ) ;
#34179 = CARTESIAN_POINT ( 'NONE',  ( 0.2739690278137220658, 11.57167385487633560, 4.016979056590812114 ) ) ;
#34180 = VERTEX_POINT ( 'NONE', #9422 ) ;
#34181 = DIRECTION ( 'NONE',  ( -1.000000000000000000, 0.000000000000000000, 0.000000000000000000 ) ) ;
#34182 = CARTESIAN_POINT ( 'NONE',  ( 0.2653141617321004841, 7.905395731875621834, -9.352766656399982281 ) ) ;
#34183 = AXIS2_PLACEMENT_3D ( 'NONE', #60923, #60580, #4759 ) ;
#34184 = CARTESIAN_POINT ( 'NONE',  ( 35.00000000000000000, 10.14433819232443490, 6.753013023069603271 ) ) ;
#34185 = CARTESIAN_POINT ( 'NONE',  ( -35.04643116707788408, 0.004425962698851801380, -0.01135624435145456135 ) ) ;
#34186 = CARTESIAN_POINT ( 'NONE',  ( 29.27326790309752980, 9.878007402510375456, 6.829635556393566453 ) ) ;
#34187 = CARTESIAN_POINT ( 'NONE',  ( 0.8375941296813829151, 0.3844307390191658569, -12.43103843094074357 ) ) ;
#34188 = CIRCLE ( 'NONE', #39507, 7.938172270156617749 ) ;
#34189 = DIRECTION ( 'NONE',  ( 0.000000000000000000, 0.01356324068817998940, -0.9999080150203989437 ) ) ;
#34190 = LINE ( 'NONE', #60124, #64205 ) ;
#34191 = CARTESIAN_POINT ( 'NONE',  ( 1.634816307074680841, 5.718391684266664221, 11.34285134320760946 ) ) ;
#34192 = EDGE_CURVE ( 'NONE', #8491, #63532, #4479, .T. ) ;
#34193 = VERTEX_POINT ( 'NONE', #10104 ) ;
#34194 = CARTESIAN_POINT ( 'NONE',  ( -16.35799066125883527, 8.282504492528538265, -8.683502121879305591 ) ) ;
#34195 = VECTOR ( 'NONE', #1507, 1000.000000000000000 ) ;
#34196 = VERTEX_POINT ( 'NONE', #30384 ) ;
#34197 = CARTESIAN_POINT ( 'NONE',  ( 37.00000000000000711, 1.457575200925545822, -12.66641127287626567 ) ) ;
#34198 = CARTESIAN_POINT ( 'NONE',  ( 2.000000000000001776, 6.539067737394540281, -2.314222412769769033 ) ) ;
#34199 = CARTESIAN_POINT ( 'NONE',  ( 0.2638984909335716500, 11.43908195192329735, 4.375449752477170939 ) ) ;
#34200 = CARTESIAN_POINT ( 'NONE',  ( 0.2653519789438766874, 9.395292406847929101, 7.854827495960845063 ) ) ;
#34201 = CARTESIAN_POINT ( 'NONE',  ( 5.515188684475870851, -0.002166413411657383374, 0.004893136156457774874 ) ) ;
#34202 = ORIENTED_EDGE ( 'NONE', *, *, #12007, .F. ) ;
#34203 = DIRECTION ( 'NONE',  ( 0.000000000000000000, 0.8009703041134188517, 0.5987040770935648792 ) ) ;
#34204 = CARTESIAN_POINT ( 'NONE',  ( -35.04643116707788408, -0.01156612771643569793, -0.003844232202723438241 ) ) ;
#34205 = VECTOR ( 'NONE', #55424, 1000.000000000000000 ) ;
#34206 = CARTESIAN_POINT ( 'NONE',  ( -27.08579483061179616, 2.081508743190604083, 0.9690219683526558603 ) ) ;
#34207 = CARTESIAN_POINT ( 'NONE',  ( 16.93394556191327283, -34.50000000000001421, -4.811904876957583177 ) ) ;
#34208 = AXIS2_PLACEMENT_3D ( 'NONE', #23335, #18368, #53930 ) ;
#34209 = VECTOR ( 'NONE', #37882, 1000.000000000000000 ) ;
#34210 = EDGE_CURVE ( 'NONE', #58300, #53581, #16962, .T. ) ;
#34211 = DIRECTION ( 'NONE',  ( -1.000000000000000000, 0.000000000000000000, 0.000000000000000000 ) ) ;
#34212 = EDGE_LOOP ( 'NONE', ( #40068, #26162, #7523, #60535 ) ) ;
#34213 = EDGE_CURVE ( 'NONE', #3030, #21349, #12535, .T. ) ;
#34214 = FACE_OUTER_BOUND ( 'NONE', #23909, .T. ) ;
#34215 = EDGE_LOOP ( 'NONE', ( #22441, #58381, #7562, #25687 ) ) ;
#34216 = EDGE_CURVE ( 'NONE', #34377, #35057, #61569, .T. ) ;
#34217 = CARTESIAN_POINT ( 'NONE',  ( -22.27384469013076185, -0.9835229356382323429, 3.548341908721027060 ) ) ;
#34218 = CARTESIAN_POINT ( 'NONE',  ( -15.84367078531945516, -34.24835312396420051, 7.333865081865427626 ) ) ;
#34219 = CARTESIAN_POINT ( 'NONE',  ( 37.00000000000000711, 4.705694406421931860E-17, -3.469127814946512892E-15 ) ) ;
#34220 = VECTOR ( 'NONE', #22140, 1000.000000000000000 ) ;
#34221 = CARTESIAN_POINT ( 'NONE',  ( -29.43980975494970309, -3.641506875706034041, -12.99959336572439561 ) ) ;
#34222 = AXIS2_PLACEMENT_3D ( 'NONE', #33333, #28026, #3762 ) ;
#34223 = ORIENTED_EDGE ( 'NONE', *, *, #25050, .F. ) ;
#34225 = VERTEX_POINT ( 'NONE', #48562 ) ;
#34224 = EDGE_CURVE ( 'NONE', #36765, #18385, #34695, .T. ) ;
#34226 = DIRECTION ( 'NONE',  ( 0.000000000000000000, 0.3218879778915905709, -0.9467777615094595811 ) ) ;
#34227 = DIRECTION ( 'NONE',  ( 1.000000000000000000, 0.000000000000000000, 0.000000000000000000 ) ) ;
#34229 = AXIS2_PLACEMENT_3D ( 'NONE', #12166, #15912, #61161 ) ;
#34228 = CARTESIAN_POINT ( 'NONE',  ( 35.00000000000000000, 6.753013023069713405, -10.14433819232436917 ) ) ;
#34230 = CARTESIAN_POINT ( 'NONE',  ( 0.2956976708475453353, 12.25433786972505601, 0.2200030809426018197 ) ) ;
#34231 = DIRECTION ( 'NONE',  ( 0.000000000000000000, 0.7196168960969817618, 0.6943713148249615053 ) ) ;
#34232 = EDGE_CURVE ( 'NONE', #44679, #2111, #28583, .T. ) ;
#34233 = CARTESIAN_POINT ( 'NONE',  ( 0.7446945582518608164, -12.40088838629985624, -0.3561743995936417218 ) ) ;
#34234 = EDGE_LOOP ( 'NONE', ( #7534, #10671, #4985, #32316 ) ) ;
#34235 = EDGE_LOOP ( 'NONE', ( #9464, #13549, #54215, #26957 ) ) ;
#34236 = ORIENTED_EDGE ( 'NONE', *, *, #56532, .T. ) ;
#34237 = CARTESIAN_POINT ( 'NONE',  ( -22.71097035706202405, 4.510116093748279376, -2.118550233809386896 ) ) ;
#34238 = EDGE_CURVE ( 'NONE', #51547, #8029, #3163, .T. ) ;
#34239 = DIRECTION ( 'NONE',  ( -1.000000000000000000, -1.836970198721029688E-16, 0.000000000000000000 ) ) ;
#34240 = EDGE_LOOP ( 'NONE', ( #55635, #63357, #11694, #48798 ) ) ;
#34241 = LINE ( 'NONE', #49563, #19876 ) ;
#34242 = EDGE_CURVE ( 'NONE', #40631, #60763, #23273, .T. ) ;
#34243 = CIRCLE ( 'NONE', #46980, 5.000000000000000888 ) ;
#34244 = DIRECTION ( 'NONE',  ( -1.000000000000000000, 0.000000000000000000, 0.000000000000000000 ) ) ;
#34245 = ORIENTED_EDGE ( 'NONE', *, *, #18582, .T. ) ;
#34246 = CARTESIAN_POINT ( 'NONE',  ( 2.639814597422738274, 7.207158938903946321, 2.896050884406557557 ) ) ;
#34247 = DIRECTION ( 'NONE',  ( 0.000000000000000000, 1.000000000000000000, 0.000000000000000000 ) ) ;
#34248 = CARTESIAN_POINT ( 'NONE',  ( 35.00000000000000000, -9.063649021438894948, 8.146229107149494553 ) ) ;
#34249 = VERTEX_POINT ( 'NONE', #11093 ) ;
#34251 = EDGE_CURVE ( 'NONE', #28701, #63705, #45068, .T. ) ;
#34250 = ORIENTED_EDGE ( 'NONE', *, *, #59041, .F. ) ;
#34252 = DIRECTION ( 'NONE',  ( 0.3865475372811021937, -0.9046932595863048654, -0.1791957239473693231 ) ) ;
#34253 = ORIENTED_EDGE ( 'NONE', *, *, #25939, .F. ) ;
#34254 = CARTESIAN_POINT ( 'NONE',  ( 0.000000000000000000, 3.859771122243047081, 5.613913289150030295 ) ) ;
#34255 = VERTEX_POINT ( 'NONE', #48887 ) ;
#34256 = AXIS2_PLACEMENT_3D ( 'NONE', #63005, #18471, #63990 ) ;
#34257 = AXIS2_PLACEMENT_3D ( 'NONE', #651, #35550, #61803 ) ;
#34258 = EDGE_LOOP ( 'NONE', ( #7850, #46180, #27321, #32423 ) ) ;
#34259 = EDGE_LOOP ( 'NONE', ( #15598, #20368, #17662, #11330 ) ) ;
#34260 = CARTESIAN_POINT ( 'NONE',  ( 34.00000000000000000, 1.267509437117510519E-14, 0.000000000000000000 ) ) ;
#34261 = CARTESIAN_POINT ( 'NONE',  ( -0.9215452301825294290, -30.54833844081706928, -15.29585404987903452 ) ) ;
#34262 = CIRCLE ( 'NONE', #56578, 12.75000000000000178 ) ;
#34264 = AXIS2_PLACEMENT_3D ( 'NONE', #52326, #17721, #36995 ) ;
#34263 = CARTESIAN_POINT ( 'NONE',  ( 0.000000000000000000, 3.152010634611693174, 6.039758645301271933 ) ) ;
#34265 = CARTESIAN_POINT ( 'NONE',  ( 2.000000000000001776, 0.000000000000000000, 0.000000000000000000 ) ) ;
#34266 = CARTESIAN_POINT ( 'NONE',  ( -22.31328051695926007, -3.781397440874596061, 0.2528478350593901802 ) ) ;
#34267 = VERTEX_POINT ( 'NONE', #3344 ) ;
#34268 = CARTESIAN_POINT ( 'NONE',  ( 1.194176325881339151, 11.12159247766672898, 5.827386336992917748 ) ) ;
#34269 = ORIENTED_EDGE ( 'NONE', *, *, #3729, .T. ) ;
#34270 = LINE ( 'NONE', #63533, #928 ) ;
#34271 = CYLINDRICAL_SURFACE ( 'NONE', #17100, 5.000000000000000888 ) ;
#34272 = EDGE_LOOP ( 'NONE', ( #34149, #24614, #35928, #55442 ) ) ;
#34273 = DIRECTION ( 'NONE',  ( -1.000000000000000000, 0.000000000000000000, 0.000000000000000000 ) ) ;
#34274 = LINE ( 'NONE', #29938, #4205 ) ;
#34275 = CARTESIAN_POINT ( 'NONE',  ( 1.719304012338199517, 0.000000000000000000, 0.000000000000000000 ) ) ;
#34276 = ORIENTED_EDGE ( 'NONE', *, *, #51600, .T. ) ;
#34277 = AXIS2_PLACEMENT_3D ( 'NONE', #45857, #9594, #19921 ) ;
#34278 = EDGE_CURVE ( 'NONE', #37190, #1479, #33947, .T. ) ;
#34279 = VERTEX_POINT ( 'NONE', #16413 ) ;
#34280 = CARTESIAN_POINT ( 'NONE',  ( -35.04683013664716640, 0.004196202180982810774, 0.01162359816263982236 ) ) ;
#34281 = ORIENTED_EDGE ( 'NONE', *, *, #61, .F. ) ;
#34282 = CARTESIAN_POINT ( 'NONE',  ( -24.67437105727481494, -11.54489660803197282, 7.000040830933849989 ) ) ;
#34283 = DIRECTION ( 'NONE',  ( 1.000000000000000000, -0.000000000000000000, 0.000000000000000000 ) ) ;
#34284 = CIRCLE ( 'NONE', #55563, 2.899999999999995470 ) ;
#34285 = CARTESIAN_POINT ( 'NONE',  ( -27.08426504710140392, 2.202478235133278783, 0.6326154899769155238 ) ) ;
#34286 = CARTESIAN_POINT ( 'NONE',  ( 2.907497136250361880, 4.235253383576015551, 6.617189382231051908 ) ) ;
#34287 = CARTESIAN_POINT ( 'NONE',  ( 35.00000000000000000, 1.791059740004421919, -12.05416472667166339 ) ) ;
#34288 = VERTEX_POINT ( 'NONE', #2357 ) ;
#34289 = EDGE_CURVE ( 'NONE', #5802, #16616, #48828, .T. ) ;
#34290 = CARTESIAN_POINT ( 'NONE',  ( 2.177405672433136541, -2.605669267165103165, -10.89176600224354274 ) ) ;
#34291 = CARTESIAN_POINT ( 'NONE',  ( 37.00000000000000711, -0.7008968033239626472, -12.16632754454236576 ) ) ;
#34292 = EDGE_CURVE ( 'NONE', #7657, #34943, #33159, .T. ) ;
#34293 = DIRECTION ( 'NONE',  ( 0.000000000000000000, 0.000000000000000000, 1.000000000000000000 ) ) ;
#34294 = FACE_OUTER_BOUND ( 'NONE', #52801, .T. ) ;
#34295 = EDGE_CURVE ( 'NONE', #9113, #2944, #42893, .T. ) ;
#34296 = CARTESIAN_POINT ( 'NONE',  ( 0.000000000000000000, -7.203928197742085260, -2.086484728383230181 ) ) ;
#34297 = DIRECTION ( 'NONE',  ( -1.000000000000000000, 0.000000000000000000, 0.000000000000000000 ) ) ;
#34298 = DIRECTION ( 'NONE',  ( -1.000000000000000000, 0.000000000000000000, 0.000000000000000000 ) ) ;
#34299 = CIRCLE ( 'NONE', #7783, 12.74999999999999822 ) ;
#34300 = AXIS2_PLACEMENT_3D ( 'NONE', #7856, #43398, #64342 ) ;
#34301 = VECTOR ( 'NONE', #1770, 1000.000000000000000 ) ;
#34302 = AXIS2_PLACEMENT_3D ( 'NONE', #61533, #25987, #20970 ) ;
#34303 = ORIENTED_EDGE ( 'NONE', *, *, #7068, .T. ) ;
#34304 = CARTESIAN_POINT ( 'NONE',  ( 9.575800908719084958, -11.95193887484098028, -1.072919909436247154 ) ) ;
#34305 = ORIENTED_EDGE ( 'NONE', *, *, #63405, .F. ) ;
#34306 = PLANE ( 'NONE',  #65019 ) ;
#34307 = CARTESIAN_POINT ( 'NONE',  ( -35.04643116707788408, -0.004425962698862209721, 0.01135624435143547939 ) ) ;
#34308 = CARTESIAN_POINT ( 'NONE',  ( 2.835339799623982415, -7.466040501142048313, 2.367573116406950895 ) ) ;
#34309 = AXIS2_PLACEMENT_3D ( 'NONE', #13023, #32954, #17364 ) ;
#34310 = CARTESIAN_POINT ( 'NONE',  ( 2.241506898688419458, 3.851253041557103796, 6.591904579673240505 ) ) ;
#34311 = ORIENTED_EDGE ( 'NONE', *, *, #43880, .F. ) ;
#34312 = AXIS2_PLACEMENT_3D ( 'NONE', #2998, #38888, #42531 ) ;
#34313 = ORIENTED_EDGE ( 'NONE', *, *, #59303, .T. ) ;
#34314 = ORIENTED_EDGE ( 'NONE', *, *, #11762, .T. ) ;
#34315 = DIRECTION ( 'NONE',  ( -1.000000000000000000, -0.000000000000000000, 0.000000000000000000 ) ) ;
#34316 = ADVANCED_FACE ( 'NONE', ( #7659 ), #27942, .F. ) ;
#34317 = AXIS2_PLACEMENT_3D ( 'NONE', #47183, #51186, #5637 ) ;
#34318 = B_SPLINE_CURVE_WITH_KNOTS ( 'NONE', 3,
 ( #39702, #5122, #50362, #24088, #59998, #40341, #9420, #60980, #60638, #34693, #29709, #45670, #4477, #44349, #24747, #35682, #65298, #40022, #60309 ),
 .UNSPECIFIED., .F., .F.,
 ( 4, 3, 3, 3, 3, 3, 4 ),
 ( 6.759600587344756714E-18, 2.825908398831169217E-05, 4.208813692483723273E-05, 5.591713746943635389E-05, 6.279584083231494560E-05, 9.105792820296123484E-05, 0.0001153131102488860418 ),
 .UNSPECIFIED. ) ;
#34319 = B_SPLINE_CURVE_WITH_KNOTS ( 'NONE', 3,
 ( #56188, #10627, #15939, #11305, #31263, #1003, #46883 ),
 .UNSPECIFIED., .F., .F.,
 ( 4, 3, 4 ),
 ( 0.000000000000000000, 0.001700533616330528446, 0.005002426799371318192 ),
 .UNSPECIFIED. ) ;
#34320 = ORIENTED_EDGE ( 'NONE', *, *, #23042, .F. ) ;
#34321 = EDGE_CURVE ( 'NONE', #36463, #54788, #26807, .T. ) ;
#34322 = CARTESIAN_POINT ( 'NONE',  ( -22.27722022243423794, -2.391991868237149710, -2.798846704197252233 ) ) ;
#34323 = CARTESIAN_POINT ( 'NONE',  ( 145.1370849898475797, 3.309064568108273190E-14, 0.000000000000000000 ) ) ;
#34324 = CARTESIAN_POINT ( 'NONE',  ( 0.2648978790185584908, 10.53870023327863770, 6.237101853238585569 ) ) ;
#34325 = CARTESIAN_POINT ( 'NONE',  ( -10.00000000000000178, 0.000000000000000000, 0.000000000000000000 ) ) ;
#34326 = VERTEX_POINT ( 'NONE', #54195 ) ;
#34327 = CARTESIAN_POINT ( 'NONE',  ( -37.00000000000000711, 0.000000000000000000, 0.000000000000000000 ) ) ;
#34328 = CARTESIAN_POINT ( 'NONE',  ( 1.819964709950166126, -30.58339181399412254, -15.25524951094132398 ) ) ;
#34329 = LINE ( 'NONE', #54643, #16483 ) ;
#34331 = VERTEX_POINT ( 'NONE', #14271 ) ;
#34330 = CARTESIAN_POINT ( 'NONE',  ( -27.01437459610461644, -11.79277645698183186, -2.220455681983952267 ) ) ;
#34332 = EDGE_CURVE ( 'NONE', #2803, #10275, #42420, .T. ) ;
#34333 = CARTESIAN_POINT ( 'NONE',  ( 35.00000000000000000, 4.400442035670942609, -11.96656215839370674 ) ) ;
#34334 = EDGE_LOOP ( 'NONE', ( #6, #37916, #11801, #44315 ) ) ;
#34335 = CARTESIAN_POINT ( 'NONE',  ( 0.2915757698887319060, -6.312478057070384452, -10.50410115670275069 ) ) ;
#34336 = VERTEX_POINT ( 'NONE', #8968 ) ;
#34337 = CARTESIAN_POINT ( 'NONE',  ( 0.3675815128205894289, -8.093875121226016489, -9.235491948680088825 ) ) ;
#34338 = CARTESIAN_POINT ( 'NONE',  ( 0.2739690278137253410, 4.016979056590924912, -11.57167385487629474 ) ) ;
#34339 = CARTESIAN_POINT ( 'NONE',  ( 5.530133899448235191, -0.01293763278443444721, -0.009387834778845806707 ) ) ;
#34340 = CYLINDRICAL_SURFACE ( 'NONE', #44992, 4.999999999999999112 ) ;
#34341 = VECTOR ( 'NONE', #53233, 1000.000000000000000 ) ;
#34342 = PLANE ( 'NONE',  #6007 ) ;
#34343 = CARTESIAN_POINT ( 'NONE',  ( -35.00000000000000000, -10.14433819232429812, -6.753013023069823539 ) ) ;
#34344 = LINE ( 'NONE', #24703, #51357 ) ;
#34346 = VERTEX_POINT ( 'NONE', #65453 ) ;
#34345 = DIRECTION ( 'NONE',  ( 0.000000000000000000, 0.9105187689795969375, -0.4134677391718481476 ) ) ;
#34347 = ORIENTED_EDGE ( 'NONE', *, *, #47479, .F. ) ;
#34348 = CARTESIAN_POINT ( 'NONE',  ( -36.00000000000000711, 6.265926637539496191, 11.10408318471061762 ) ) ;
#34349 = ORIENTED_EDGE ( 'NONE', *, *, #31940, .F. ) ;
#34350 = CIRCLE ( 'NONE', #47138, 5.000000000000001776 ) ;
#34351 = ORIENTED_EDGE ( 'NONE', *, *, #3136, .F. ) ;
#34353 = AXIS2_PLACEMENT_3D ( 'NONE', #65633, #503, #15442 ) ;
#34352 = DIRECTION ( 'NONE',  ( 0.000000000000000000, 0.01356324068817992175, -0.9999080150203990547 ) ) ;
#34354 = CARTESIAN_POINT ( 'NONE',  ( -35.00000000000000000, -11.95840593935199792, -2.346765782874564277 ) ) ;
#34355 = CARTESIAN_POINT ( 'NONE',  ( 0.2648978790185619880, 6.008231198269132989, -10.67083876753485328 ) ) ;
#34356 = CARTESIAN_POINT ( 'NONE',  ( 0.2958664285830389651, -10.50235171906344789, 6.318165763623585285 ) ) ;
#34357 = DIRECTION ( 'NONE',  ( 0.000000000000000000, -0.01356324068817992175, 0.9999080150203990547 ) ) ;
#34358 = AXIS2_PLACEMENT_3D ( 'NONE', #59579, #14012, #19686 ) ;
#34359 = CARTESIAN_POINT ( 'NONE',  ( 0.3278977287071212499, 10.74546228373874790, -5.917385921415685424 ) ) ;
#34360 = EDGE_CURVE ( 'NONE', #12741, #39511, #19095, .T. ) ;
#34361 = CARTESIAN_POINT ( 'NONE',  ( 2.305787727787083519, 7.135468203930020792, -2.774453000917077805 ) ) ;
#34362 = EDGE_CURVE ( 'NONE', #35981, #23681, #57311, .T. ) ;
#34363 = VERTEX_POINT ( 'NONE', #35195 ) ;
#34364 = CARTESIAN_POINT ( 'NONE',  ( 16.21117406328131594, -35.00000000000000000, -4.142385751841773711 ) ) ;
#34365 = CIRCLE ( 'NONE', #1501, 12.74999999999999822 ) ;
#34366 = FACE_OUTER_BOUND ( 'NONE', #61652, .T. ) ;
#34367 = CARTESIAN_POINT ( 'NONE',  ( -17.54726996257253191, 25.00000000000000000, 3.865003848717349033 ) ) ;
#34368 = ORIENTED_EDGE ( 'NONE', *, *, #20663, .F. ) ;
#34369 = CIRCLE ( 'NONE', #56708, 12.18650000000000055 ) ;
#34370 = EDGE_CURVE ( 'NONE', #33641, #25335, #50962, .T. ) ;
#34371 = VECTOR ( 'NONE', #30707, 1000.000000000000000 ) ;
#34372 = AXIS2_PLACEMENT_3D ( 'NONE', #54639, #4413, #45602 ) ;
#34373 = LINE ( 'NONE', #3155, #45802 ) ;
#34374 = CIRCLE ( 'NONE', #47168, 6.936499999999989008 ) ;
#34375 = DIRECTION ( 'NONE',  ( 1.000000000000000000, 0.000000000000000000, 0.000000000000000000 ) ) ;
#34377 = VERTEX_POINT ( 'NONE', #64794 ) ;
#34376 = ADVANCED_FACE ( 'NONE', ( #55499 ), #18643, .T. ) ;
#34378 = DIRECTION ( 'NONE',  ( -1.000000000000000000, 0.000000000000000000, 0.000000000000000000 ) ) ;
#34379 = LINE ( 'NONE', #24394, #27188 ) ;
#34380 = DIRECTION ( 'NONE',  ( -1.000000000000000000, 0.000000000000000000, 0.000000000000000000 ) ) ;
#34381 = ADVANCED_FACE ( 'NONE', ( #8638 ), #13933, .T. ) ;
#34382 = VECTOR ( 'NONE', #60173, 1000.000000000000000 ) ;
#34383 = DIRECTION ( 'NONE',  ( -0.000000000000000000, -1.000000000000000000, -0.000000000000000000 ) ) ;
#34384 = CARTESIAN_POINT ( 'NONE',  ( -35.00000000000000000, 12.12087942037211263, -1.262958560998631796 ) ) ;
#34385 = VERTEX_POINT ( 'NONE', #59843 ) ;
#34386 = CARTESIAN_POINT ( 'NONE',  ( 2.000000000000001776, 2.664846396702499121, 6.404188155572998475 ) ) ;
#34387 = CARTESIAN_POINT ( 'NONE',  ( -8.292599671964985930, -6.469860207350497383, -10.13661589866336321 ) ) ;
#34389 = DIRECTION ( 'NONE',  ( 0.5417962735734935809, -0.000000000000000000, 0.8405098440481683086 ) ) ;
#34388 = B_SPLINE_CURVE_WITH_KNOTS ( 'NONE', 3,
 ( #31361, #35994, #7071, #56294, #26058, #46337, #61953, #61602, #46652, #46994, #51340, #1106, #6425, #51665, #1452, #56653, #6108, #777, #52321, #26367 ),
 .UNSPECIFIED., .F., .F.,
 ( 4, 2, 2, 2, 2, 2, 2, 2, 2, 4 ),
 ( 0.000000000000000000, 0.0007149072710670309949, 0.001429814542134061990, 0.001787268177667585348, 0.002144721813201108922, 0.002859629084268155638, 0.003574536355335202354, 0.004289443626402249070, 0.005004350897469296219, 0.005719258168536343369 ),
 .UNSPECIFIED. ) ;
#34390 = ORIENTED_EDGE ( 'NONE', *, *, #21629, .F. ) ;
#34391 = CARTESIAN_POINT ( 'NONE',  ( 21.90174657591892071, 13.47998113580524659, -0.7349207973210680755 ) ) ;
#34392 = DIRECTION ( 'NONE',  ( 1.000000000000000000, 0.000000000000000000, 0.000000000000000000 ) ) ;
#34393 = ORIENTED_EDGE ( 'NONE', *, *, #45870, .T. ) ;
#34394 = AXIS2_PLACEMENT_3D ( 'NONE', #21955, #1998, #42529 ) ;
#34395 = CIRCLE ( 'NONE', #24866, 5.000000000000000888 ) ;
#34396 = ORIENTED_EDGE ( 'NONE', *, *, #56355, .F. ) ;
#34397 = DIRECTION ( 'NONE',  ( 1.000000000000000000, 0.000000000000000000, 0.000000000000000000 ) ) ;
#34398 = EDGE_CURVE ( 'NONE', #63878, #19813, #22269, .T. ) ;
#34399 = VECTOR ( 'NONE', #33974, 1000.000000000000000 ) ;
#34400 = ORIENTED_EDGE ( 'NONE', *, *, #36672, .F. ) ;
#34401 = EDGE_CURVE ( 'NONE', #46319, #43456, #57496, .T. ) ;
#34402 = CARTESIAN_POINT ( 'NONE',  ( 19.28625800530496903, 6.413918128308424116, 11.87904264843580471 ) ) ;
#34403 = CARTESIAN_POINT ( 'NONE',  ( 22.88594695219327235, 3.421158645304719137, -11.50198563395279194 ) ) ;
#34404 = CARTESIAN_POINT ( 'NONE',  ( 0.2648978790185593790, -6.237101853238620208, 10.53870023327861283 ) ) ;
#34405 = CARTESIAN_POINT ( 'NONE',  ( 2.260457164927185847, -7.547495527593552467, -1.190240296002748277 ) ) ;
#34406 = VECTOR ( 'NONE', #29165, 1000.000000000000000 ) ;
#34407 = CARTESIAN_POINT ( 'NONE',  ( -37.00000000000000711, 0.000000000000000000, 0.000000000000000000 ) ) ;
#34409 = EDGE_LOOP ( 'NONE', ( #20513, #64435, #40435, #41047 ) ) ;
#34408 = DIRECTION ( 'NONE',  ( -0.000000000000000000, -0.000000000000000000, -1.000000000000000000 ) ) ;
#34410 = EDGE_CURVE ( 'NONE', #17490, #19103, #59441, .T. ) ;
#34411 = CARTESIAN_POINT ( 'NONE',  ( -29.43980975494970309, -3.641506875706030488, 25.00000000000000000 ) ) ;
#34412 = VERTEX_POINT ( 'NONE', #54535 ) ;
#34413 = FACE_OUTER_BOUND ( 'NONE', #11951, .T. ) ;
#34414 = CONICAL_SURFACE ( 'NONE', #42904, 14.13397459621556251, 0.5235987755983000369 ) ;
#34415 = ORIENTED_EDGE ( 'NONE', *, *, #50641, .F. ) ;
#34416 = EDGE_LOOP ( 'NONE', ( #32133, #16760, #6532, #2272 ) ) ;
#34417 = CARTESIAN_POINT ( 'NONE',  ( -25.13721231563192759, 11.42414658719028253, 7.194720236206205044 ) ) ;
#34418 = CARTESIAN_POINT ( 'NONE',  ( -3.619268891295738477, -30.76314776371165749, 15.03790153758943404 ) ) ;
#34419 = VECTOR ( 'NONE', #18059, 1000.000000000000000 ) ;
#34420 = PLANE ( 'NONE',  #22640 ) ;
#34421 = CARTESIAN_POINT ( 'NONE',  ( 0.2655924914740778187, -12.06787830249866467, 2.083162675473574588 ) ) ;
#34422 = DIRECTION ( 'NONE',  ( 0.000000000000000000, 0.000000000000000000, -1.000000000000000000 ) ) ;
#34423 = DIRECTION ( 'NONE',  ( -1.000000000000000000, 0.000000000000000000, 0.000000000000000000 ) ) ;
#34424 = ORIENTED_EDGE ( 'NONE', *, *, #532, .F. ) ;
#34425 = VERTEX_POINT ( 'NONE', #54848 ) ;
#34426 = CARTESIAN_POINT ( 'NONE',  ( -35.00000000000000000, -1.457575200925636416, 12.66641127287625324 ) ) ;
#34427 = VECTOR ( 'NONE', #27282, 1000.000000000000114 ) ;
#34428 = ORIENTED_EDGE ( 'NONE', *, *, #50213, .T. ) ;
#34429 = DIRECTION ( 'NONE',  ( -1.000000000000000000, 0.000000000000000000, 0.000000000000000000 ) ) ;
#34430 = CARTESIAN_POINT ( 'NONE',  ( 2.000000000000001776, 6.201547234537079234, -2.820401998297854096 ) ) ;
#34431 = LINE ( 'NONE', #3210, #21446 ) ;
#34432 = CARTESIAN_POINT ( 'NONE',  ( -37.00000000000000711, -7.376655759824951808, 9.700295462048636352 ) ) ;
#34433 = CARTESIAN_POINT ( 'NONE',  ( 2.177405672432084938, 7.702458780349609846, 8.129711416438519578 ) ) ;
#34434 = AXIS2_PLACEMENT_3D ( 'NONE', #56952, #37294, #1081 ) ;
#34435 = B_SPLINE_CURVE_WITH_KNOTS ( 'NONE', 3,
 ( #56206, #5358, #5701, #51899, #46564, #6340, #35599, #55894, #1022, #10325, #30601, #20955, #10645, #45920, #46256, #700, #41234, #61517, #15958, #36247 ),
 .UNSPECIFIED., .F., .F.,
 ( 4, 2, 2, 2, 2, 2, 2, 2, 2, 4 ),
 ( 0.000000000000000000, 0.001108655026528466330, 0.002217310053056931792, 0.003325965079585397905, 0.003880292592849631395, 0.004434620106113865319, 0.005543275132642328830, 0.006651930159170793208, 0.007760585185699257586, 0.008869240212227721964 ),
 .UNSPECIFIED. ) ;
#34436 = CARTESIAN_POINT ( 'NONE',  ( 0.000000000000000000, 0.000000000000000000, 0.000000000000000000 ) ) ;
#34437 = ADVANCED_FACE ( 'NONE', ( #9268 ), #19610, .T. ) ;
#34438 = ORIENTED_EDGE ( 'NONE', *, *, #14168, .F. ) ;
#34439 = ORIENTED_EDGE ( 'NONE', *, *, #33599, .T. ) ;
#34440 = DIRECTION ( 'NONE',  ( 0.000000000000000000, -0.01356324068817999114, 0.9999080150203989437 ) ) ;
#34441 = AXIS2_PLACEMENT_3D ( 'NONE', #17058, #62942, #57651 ) ;
#34442 = DIRECTION ( 'NONE',  ( 1.000000000000000000, 0.000000000000000000, -0.000000000000000000 ) ) ;
#34443 = AXIS2_PLACEMENT_3D ( 'NONE', #26786, #47082, #57718 ) ;
#34444 = CARTESIAN_POINT ( 'NONE',  ( -35.00000000000000000, -11.72195762423409349, -0.7536123767499773862 ) ) ;
#34445 = CARTESIAN_POINT ( 'NONE',  ( -35.00000000000000000, -8.258652103341496797, 8.352657516904644197 ) ) ;
#34446 = EDGE_CURVE ( 'NONE', #3157, #35439, #47774, .T. ) ;
#34447 = CARTESIAN_POINT ( 'NONE',  ( 37.00000000000000711, 4.705694406421931860E-17, -3.469127814946512892E-15 ) ) ;
#34448 = CARTESIAN_POINT ( 'NONE',  ( -10.90165637462999904, -7.508992741355383416, -9.360289953322597611 ) ) ;
#34449 = CARTESIAN_POINT ( 'NONE',  ( 37.25000000000000711, 1.820029539775944174E-16, -1.500000000000000222 ) ) ;
#34450 = CARTESIAN_POINT ( 'NONE',  ( -27.08423805673873375, -2.195702713475281342, -0.6554626340706090071 ) ) ;
#34451 = CARTESIAN_POINT ( 'NONE',  ( 37.00000000000000711, 4.705694406421931860E-17, -3.469127814946512892E-15 ) ) ;
#34452 = EDGE_CURVE ( 'NONE', #55405, #40269, #65647, .T. ) ;
#34453 = VERTEX_POINT ( 'NONE', #21219 ) ;
#34454 = CARTESIAN_POINT ( 'NONE',  ( 2.589278595512557235, -6.089088204448533936, -4.794929105510985501 ) ) ;
#34455 = CARTESIAN_POINT ( 'NONE',  ( 5.515539859299206427, 0.004509673239148487972, -0.004037661319611322332 ) ) ;
#34456 = CARTESIAN_POINT ( 'NONE',  ( 2.350038591458129655, 7.710465783963716291, 7.305692696275574605 ) ) ;
#34457 = EDGE_CURVE ( 'NONE', #18427, #29901, #7401, .T. ) ;
#34459 = AXIS2_PLACEMENT_3D ( 'NONE', #50889, #56537, #5339 ) ;
#34458 = AXIS2_PLACEMENT_3D ( 'NONE', #35461, #50454, #234 ) ;
#34460 = CARTESIAN_POINT ( 'NONE',  ( -18.08686583997218378, 5.151216734910788908, 25.00000000000000000 ) ) ;
#34461 = DIRECTION ( 'NONE',  ( 0.000000000000000000, 0.01356324068817998940, -0.9999080150203989437 ) ) ;
#34462 = ORIENTED_EDGE ( 'NONE', *, *, #28751, .F. ) ;
#34463 = CARTESIAN_POINT ( 'NONE',  ( -35.05012975565874456, 0.002839961651358813028, 0.01363945138521199113 ) ) ;
#34464 = DIRECTION ( 'NONE',  ( -1.000000000000000000, 0.000000000000000000, 0.000000000000000000 ) ) ;
#34465 = CARTESIAN_POINT ( 'NONE',  ( 7.919433923537877895, -32.26502814485947823, -12.92562328492908286 ) ) ;
#34466 = VERTEX_POINT ( 'NONE', #16244 ) ;
#34467 = DIRECTION ( 'NONE',  ( -1.000000000000000000, 0.000000000000000000, 0.000000000000000000 ) ) ;
#34468 = CARTESIAN_POINT ( 'NONE',  ( -28.13926220603491402, -11.82994279791709857, -6.511265657020829600 ) ) ;
#34469 = CARTESIAN_POINT ( 'NONE',  ( -22.31328051695926007, -1.076152733467184985, -3.633840107626963967 ) ) ;
#34470 = CARTESIAN_POINT ( 'NONE',  ( 0.3401186441510204994, -8.081824149807760094, 9.233880480307277594 ) ) ;
#34471 = DIRECTION ( 'NONE',  ( 0.000000000000000000, 0.01356324068817992175, -0.9999080150203990547 ) ) ;
#34472 = EDGE_CURVE ( 'NONE', #3310, #51818, #6610, .T. ) ;
#34473 = VECTOR ( 'NONE', #27733, 1000.000000000000000 ) ;
#34474 = CARTESIAN_POINT ( 'NONE',  ( 0.3675815128205912052, 12.04510820461662668, -2.391755495700480516 ) ) ;
#34475 = ORIENTED_EDGE ( 'NONE', *, *, #41731, .T. ) ;
#34476 = LINE ( 'NONE', #54777, #25914 ) ;
#34477 = CARTESIAN_POINT ( 'NONE',  ( -27.09602251845159415, 1.302811993375597277, 1.927725285105644115 ) ) ;
#34478 = CARTESIAN_POINT ( 'NONE',  ( -18.43671985620534315, 6.169215440633483816, -12.01111733792950176 ) ) ;
#34479 = CARTESIAN_POINT ( 'NONE',  ( 2.524535260912981194, -4.796565674004606983, 6.060306679219116255 ) ) ;
#34480 = CARTESIAN_POINT ( 'NONE',  ( 2.000000000000001776, -5.396716205731396876, -4.158041573745144603 ) ) ;
#34481 = CARTESIAN_POINT ( 'NONE',  ( 2.941278708680199916, 2.226055275041790349, 5.721889327162159589 ) ) ;
#34482 = CYLINDRICAL_SURFACE ( 'NONE', #31289, 4.999999999999999112 ) ;
#34483 = CARTESIAN_POINT ( 'NONE',  ( 2.241317068080784125, 1.235499051335310794, -7.533758201955659040 ) ) ;
#34484 = ORIENTED_EDGE ( 'NONE', *, *, #16136, .T. ) ;
#34485 = EDGE_LOOP ( 'NONE', ( #16016, #26558, #18037, #22591 ) ) ;
#34486 = CARTESIAN_POINT ( 'NONE',  ( 5.515539859299206427, -0.002856745161749578953, 0.005336559634876932544 ) ) ;
#34487 = ORIENTED_EDGE ( 'NONE', *, *, #52274, .T. ) ;
#34488 = EDGE_CURVE ( 'NONE', #45697, #56806, #1295, .T. ) ;
#34489 = CARTESIAN_POINT ( 'NONE',  ( -35.00000000000000000, -12.74613886779085092, 0.3137578094508798321 ) ) ;
#34490 = CARTESIAN_POINT ( 'NONE',  ( 2.941278708680199916, -1.972702289975964973, -5.814102272488608669 ) ) ;
#34491 = ORIENTED_EDGE ( 'NONE', *, *, #37923, .F. ) ;
#34492 = CARTESIAN_POINT ( 'NONE',  ( 0.3675815128205894289, 5.910255304480596550, -10.76447900494934196 ) ) ;
#34493 = CIRCLE ( 'NONE', #5862, 12.18650000000000055 ) ;
#34494 = CARTESIAN_POINT ( 'NONE',  ( 2.000000000000001776, 0.000000000000000000, 0.000000000000000000 ) ) ;
#34495 = CARTESIAN_POINT ( 'NONE',  ( 2.241352910868909643, -4.970878533273721978, -5.794346703933896059 ) ) ;
#34496 = ORIENTED_EDGE ( 'NONE', *, *, #11482, .T. ) ;
#34497 = ORIENTED_EDGE ( 'NONE', *, *, #49342, .T. ) ;
#34498 = CARTESIAN_POINT ( 'NONE',  ( 2.259025283528085737, -7.225123487442752790, -2.484282765458421860 ) ) ;
#34499 = AXIS2_PLACEMENT_3D ( 'NONE', #63528, #54575, #7697 ) ;
#34500 = DIRECTION ( 'NONE',  ( 0.000000000000000000, -0.9467777615094536969, -0.3218879778916073908 ) ) ;
#34501 = ORIENTED_EDGE ( 'NONE', *, *, #60195, .T. ) ;
#34502 = DIRECTION ( 'NONE',  ( 0.000000000000000000, 0.8009703041134147439, 0.5987040770935704304 ) ) ;
#34503 = EDGE_LOOP ( 'NONE', ( #62076, #48128, #46209, #11662 ) ) ;
#34504 = FACE_OUTER_BOUND ( 'NONE', #52581, .T. ) ;
#34505 = AXIS2_PLACEMENT_3D ( 'NONE', #5067, #4756, #39968 ) ;
#34506 = CARTESIAN_POINT ( 'NONE',  ( -4.806344283790351390, -7.508992741355383416, 25.00000000000000000 ) ) ;
#34507 = DIRECTION ( 'NONE',  ( 0.000000000000000000, 1.000000000000000000, 0.000000000000000000 ) ) ;
#34508 = CARTESIAN_POINT ( 'NONE',  ( 0.2653519890518156732, -10.60551359205155109, 6.123106317427121859 ) ) ;
#34509 = B_SPLINE_CURVE_WITH_KNOTS ( 'NONE', 3,
 ( #35931, #19367, #55914, #39634, #65232, #40948, #20007, #50612, #44953, #61228, #9690, #29980, #60563, #35287, #5053, #46589, #32270, #31608, #31931, #26307 ),
 .UNSPECIFIED., .F., .F.,
 ( 4, 2, 2, 2, 2, 2, 2, 2, 2, 4 ),
 ( 5.553824967135426632E-18, 0.002960076713079371011, 0.004440115069619054999, 0.005920153426158738554, 0.006660172604428579030, 0.007400191782698420373, 0.008140210960968261716, 0.008880230139238104795, 0.01036026849577778401, 0.01184030685231746323 ),
 .UNSPECIFIED. ) ;
#34510 = CARTESIAN_POINT ( 'NONE',  ( 0.3223008802179184173, 11.60682919296352011, 3.964361764750220285 ) ) ;
#34511 = ADVANCED_FACE ( 'NONE', ( #11258 ), #30539, .T. ) ;
#34512 = ORIENTED_EDGE ( 'NONE', *, *, #48071, .T. ) ;
#34513 = CARTESIAN_POINT ( 'NONE',  ( -19.69476066079020171, -4.201994156881551312, -11.24025111398909615 ) ) ;
#34514 = CARTESIAN_POINT ( 'NONE',  ( 3.152665057734119536, 1.848755561852129858, -7.719888720907784219 ) ) ;
#34515 = ADVANCED_FACE ( 'NONE', ( #46827 ), #20239, .T. ) ;
#34516 = DIRECTION ( 'NONE',  ( -1.000000000000000000, 0.000000000000000000, 0.000000000000000000 ) ) ;
#34517 = DIRECTION ( 'NONE',  ( 0.000000000000000000, -0.8369827122275287357, -0.5472293298355360713 ) ) ;
#34518 = CARTESIAN_POINT ( 'NONE',  ( 2.241537034860907607, -7.519304283075084250, 1.321063441155965190 ) ) ;
#34519 = CARTESIAN_POINT ( 'NONE',  ( 23.11060965093502162, -3.962616607205078356, 12.90843863291130411 ) ) ;
#34520 = DIRECTION ( 'NONE',  ( -1.000000000000000000, 0.000000000000000000, 0.000000000000000000 ) ) ;
#34521 = DIRECTION ( 'NONE',  ( 1.000000000000000000, 0.000000000000000000, 0.000000000000000000 ) ) ;
#34522 = DIRECTION ( 'NONE',  ( 0.000000000000000000, 0.1740410799127612429, 0.9847383929261617208 ) ) ;
#34523 = ORIENTED_EDGE ( 'NONE', *, *, #7127, .F. ) ;
#34524 = EDGE_CURVE ( 'NONE', #16616, #12178, #40339, .T. ) ;
#34525 = CARTESIAN_POINT ( 'NONE',  ( 0.3632410797595240770, 0.2628628737173456797, 12.27601307605976899 ) ) ;
#34526 = ORIENTED_EDGE ( 'NONE', *, *, #10893, .F. ) ;
#34527 = CARTESIAN_POINT ( 'NONE',  ( 35.00000000000000000, -11.72397916322011824, 0.7214809346829776926 ) ) ;
#34528 = CARTESIAN_POINT ( 'NONE',  ( 37.00000000000000711, 11.44858830469736333, -2.627174906297124135 ) ) ;
#34529 = CARTESIAN_POINT ( 'NONE',  ( 1.937114397841935398, 1.334979369128593163, -12.76557247858997002 ) ) ;
#34530 = CARTESIAN_POINT ( 'NONE',  ( 0.2648978790185602672, -12.03635331166813494, 2.256510822326103671 ) ) ;
#34531 = DIRECTION ( 'NONE',  ( -1.000000000000000000, 0.000000000000000000, 0.000000000000000000 ) ) ;
#34532 = ADVANCED_FACE ( 'NONE', ( #52158 ), #56481, .F. ) ;
#34533 = ORIENTED_EDGE ( 'NONE', *, *, #37503, .T. ) ;
#34534 = CARTESIAN_POINT ( 'NONE',  ( 2.350038591457884074, 0.6402934222730660707, -10.60256821300862029 ) ) ;
#34535 = CARTESIAN_POINT ( 'NONE',  ( -30.18541646480307961, -1.416020129149133888, -11.91616074890920807 ) ) ;
#34536 = CYLINDRICAL_SURFACE ( 'NONE', #23760, 4.999999999999999112 ) ;
#34537 = CARTESIAN_POINT ( 'NONE',  ( 37.00000000000000711, 11.24036214326529048, 6.018036132182037257 ) ) ;
#34538 = CARTESIAN_POINT ( 'NONE',  ( 2.000000000000001776, 0.000000000000000000, 0.000000000000000000 ) ) ;
#34539 = CIRCLE ( 'NONE', #5911, 2.899999999999995470 ) ;
#34540 = VERTEX_POINT ( 'NONE', #5288 ) ;
#34541 = DIRECTION ( 'NONE',  ( 0.000000000000000000, 0.000000000000000000, -1.000000000000000000 ) ) ;
#34542 = ORIENTED_EDGE ( 'NONE', *, *, #35161, .F. ) ;
#34543 = CARTESIAN_POINT ( 'NONE',  ( 0.3610902822527192191, -0.2623004149193758350, -12.27530799859939314 ) ) ;
#34544 = CARTESIAN_POINT ( 'NONE',  ( -15.09490394635158772, -34.00569493827280354, 8.490101771333646852 ) ) ;
#34545 = DIRECTION ( 'NONE',  ( 0.000000000000000000, 0.01356324068817998940, -0.9999080150203990547 ) ) ;
#34546 = CARTESIAN_POINT ( 'NONE',  ( 47.00000000000000711, 4.705694406421931860E-17, -3.469127814946512892E-15 ) ) ;
#34547 = AXIS2_PLACEMENT_3D ( 'NONE', #1055, #21984, #17333 ) ;
#34548 = ORIENTED_EDGE ( 'NONE', *, *, #33029, .F. ) ;
#34549 = VERTEX_POINT ( 'NONE', #50841 ) ;
#34550 = CARTESIAN_POINT ( 'NONE',  ( -27.25055598261694811, 10.68287079889101321, 5.469009518302880402 ) ) ;
#34551 = DIRECTION ( 'NONE',  ( 0.000000000000000000, 0.1118654143051546757, 0.9937233664769770103 ) ) ;
#34553 = CARTESIAN_POINT ( 'NONE',  ( 2.889800649504073782, 6.016320774579807740, 1.129261637821630693 ) ) ;
#34552 =( BOUNDED_CURVE ( )  B_SPLINE_CURVE ( 3, ( #56487, #642, #10933, #26230 ),
 .UNSPECIFIED., .F., .F. ) 
 B_SPLINE_CURVE_WITH_KNOTS ( ( 4, 4 ),
 ( 1.825784944079407834, 1.859903487831931601 ),
 .UNSPECIFIED. ) 
 CURVE ( )  GEOMETRIC_REPRESENTATION_ITEM ( )  RATIONAL_B_SPLINE_CURVE ( ( 1.000000000000000000, 0.9999029961002143807, 0.9999029961002143807, 1.000000000000000000 ) ) 
 REPRESENTATION_ITEM ( '' )  );
#34554 = CARTESIAN_POINT ( 'NONE',  ( 2.241449424704146320, 4.860179885671878530, -5.887589908049596588 ) ) ;
#34555 = DIRECTION ( 'NONE',  ( -1.000000000000000000, 0.000000000000000000, 0.000000000000000000 ) ) ;
#34556 = CARTESIAN_POINT ( 'NONE',  ( 2.653899356900482509, 6.596318473603900223, -4.109946795501497441 ) ) ;
#34557 = DIRECTION ( 'NONE',  ( 1.000000000000000000, 0.000000000000000000, 0.000000000000000000 ) ) ;
#34558 = DIRECTION ( 'NONE',  ( -1.000000000000000000, 0.000000000000000000, 0.000000000000000000 ) ) ;
#34559 = EDGE_LOOP ( 'NONE', ( #32434, #30528, #1747, #54914 ) ) ;
#34560 = ORIENTED_EDGE ( 'NONE', *, *, #26682, .F. ) ;
#34561 = ORIENTED_EDGE ( 'NONE', *, *, #8248, .F. ) ;
#34562 = ADVANCED_FACE ( 'NONE', ( #36846 ), #56726, .F. ) ;
#34563 = AXIS2_PLACEMENT_3D ( 'NONE', #48947, #22689, #32959 ) ;
#34564 = CARTESIAN_POINT ( 'NONE',  ( -36.00000000000000711, 6.950793414699792727, 10.68873102412845277 ) ) ;
#34565 = EDGE_LOOP ( 'NONE', ( #17043, #26805, #33291, #49871 ) ) ;
#34566 = FACE_OUTER_BOUND ( 'NONE', #59144, .T. ) ;
#34567 = VERTEX_POINT ( 'NONE', #26223 ) ;
#34568 = CARTESIAN_POINT ( 'NONE',  ( -14.29135464769095520, 7.782112657557433089, 25.00000000000000000 ) ) ;
#34569 = DIRECTION ( 'NONE',  ( -1.000000000000000000, 0.000000000000000000, -0.000000000000000000 ) ) ;
#34570 = CARTESIAN_POINT ( 'NONE',  ( -27.08776759928964850, -2.229418711698780253, -0.5731512436792201015 ) ) ;
#34571 = ORIENTED_EDGE ( 'NONE', *, *, #27310, .T. ) ;
#34572 = ORIENTED_EDGE ( 'NONE', *, *, #36121, .F. ) ;
#34573 = DIRECTION ( 'NONE',  ( 0.000000000000000000, 0.000000000000000000, 1.000000000000000000 ) ) ;
#34574 = VERTEX_POINT ( 'NONE', #56139 ) ;
#34575 = DIRECTION ( 'NONE',  ( 0.000000000000000000, 0.4935949184179261873, -0.8696919319575183716 ) ) ;
#34576 = EDGE_LOOP ( 'NONE', ( #27783, #21150, #12708, #8763 ) ) ;
#34577 = ORIENTED_EDGE ( 'NONE', *, *, #18344, .T. ) ;
#34578 = ORIENTED_EDGE ( 'NONE', *, *, #19546, .F. ) ;
#34579 = DIRECTION ( 'NONE',  ( 1.000000000000000000, 0.000000000000000000, 0.000000000000000000 ) ) ;
#34580 = CARTESIAN_POINT ( 'NONE',  ( -35.00000000000000000, 2.185196060783882288, 11.54110654723649709 ) ) ;
#34581 = ADVANCED_FACE ( 'NONE', ( #10258 ), #22730, .F. ) ;
#34582 = CARTESIAN_POINT ( 'NONE',  ( 1.000000000000000888, 2.315790869867065283, 7.133520354428103616 ) ) ;
#34583 = CARTESIAN_POINT ( 'NONE',  ( -22.35190811654612375, -0.2457675311904815585, -3.898012445334722909 ) ) ;
#34584 = VERTEX_POINT ( 'NONE', #48482 ) ;
#34585 = CARTESIAN_POINT ( 'NONE',  ( 2.284126774967659923, -7.131638985093294636, -2.764365694977863441 ) ) ;
#34586 = CIRCLE ( 'NONE', #45178, 7.499999999999988454 ) ;
#34587 = ORIENTED_EDGE ( 'NONE', *, *, #3253, .T. ) ;
#34588 = DIRECTION ( 'NONE',  ( 1.000000000000000000, 0.000000000000000000, 0.000000000000000000 ) ) ;
#34589 = EDGE_CURVE ( 'NONE', #17286, #743, #61604, .T. ) ;
#34590 = CYLINDRICAL_SURFACE ( 'NONE', #58510, 12.18650000000000055 ) ;
#34591 = EDGE_CURVE ( 'NONE', #23145, #65150, #46765, .T. ) ;
#34592 = EDGE_LOOP ( 'NONE', ( #34000, #62716, #60392, #32748 ) ) ;
#34593 = CARTESIAN_POINT ( 'NONE',  ( 0.2648978790185584908, -10.67083876753496341, 6.008231198268946471 ) ) ;
#34594 = DIRECTION ( 'NONE',  ( 0.000000000000000000, 0.01356324068818000848, -0.9999080150203990547 ) ) ;
#34595 = CARTESIAN_POINT ( 'NONE',  ( -10.00000000000000178, 0.000000000000000000, 0.000000000000000000 ) ) ;
#34596 = ORIENTED_EDGE ( 'NONE', *, *, #36722, .F. ) ;
#34597 = B_SPLINE_CURVE_WITH_KNOTS ( 'NONE', 3,
 ( #31750, #56046, #51084, #45749, #50748, #21124, #30764, #45413, #61356, #6185 ),
 .UNSPECIFIED., .F., .F.,
 ( 4, 3, 3, 4 ),
 ( 1.226634733346699349E-18, 6.607638129004513277E-05, 9.911389841680585955E-05, 0.0001667630577588622028 ),
 .UNSPECIFIED. ) ;
#34598 = ORIENTED_EDGE ( 'NONE', *, *, #40602, .T. ) ;
#34599 = ADVANCED_FACE ( 'NONE', ( #47813 ), #7233, .T. ) ;
#34600 = CARTESIAN_POINT ( 'NONE',  ( 2.297017764050093280, -7.651182381906875385, 0.1647869190091477420 ) ) ;
#34601 = ORIENTED_EDGE ( 'NONE', *, *, #222, .T. ) ;
#34602 = ADVANCED_FACE ( 'NONE', ( #58126, #17884 ), #38486, .F. ) ;
#34603 = CARTESIAN_POINT ( 'NONE',  ( 35.00000000000000000, 4.705694406421931860E-17, -3.469127814946512892E-15 ) ) ;
#34604 = DIRECTION ( 'NONE',  ( 0.000000000000000000, -0.1740410799127470598, -0.9847383929261643853 ) ) ;
#34605 = CYLINDRICAL_SURFACE ( 'NONE', #13312, 12.75000000000000178 ) ;
#34606 = CARTESIAN_POINT ( 'NONE',  ( -3.517042058461139042, 9.903124696108923430, 6.789431062153663099 ) ) ;
#34607 = CARTESIAN_POINT ( 'NONE',  ( 9.687175622948609899, 11.98570860552671391, -0.5854820436212360146 ) ) ;
#34608 = ORIENTED_EDGE ( 'NONE', *, *, #43540, .T. ) ;
#34609 = DIRECTION ( 'NONE',  ( -1.000000000000000000, 0.000000000000000000, 0.000000000000000000 ) ) ;
#34610 = CARTESIAN_POINT ( 'NONE',  ( -29.92777678363736626, -3.750539801530011985, 12.96855624952674724 ) ) ;
#34611 = ADVANCED_FACE ( 'NONE', ( #22551 ), #2754, .F. ) ;
#34612 = CYLINDRICAL_SURFACE ( 'NONE', #6363, 24.00000000000000000 ) ;
#34613 = EDGE_CURVE ( 'NONE', #53149, #27041, #32173, .T. ) ;
#34614 = CARTESIAN_POINT ( 'NONE',  ( -22.28506771379528573, 2.571716811880577325, -2.697635452840750681 ) ) ;
#34615 = CARTESIAN_POINT ( 'NONE',  ( -22.27384469013076185, 0.9835229356382479970, -3.548341908721023952 ) ) ;
#34616 = DIRECTION ( 'NONE',  ( 0.000000000000000000, -0.01356324068817998940, 0.9999080150203990547 ) ) ;
#34617 = VECTOR ( 'NONE', #50316, 1000.000000000000000 ) ;
#34618 = ORIENTED_EDGE ( 'NONE', *, *, #39709, .T. ) ;
#34619 = CARTESIAN_POINT ( 'NONE',  ( 35.00000000000000000, -0.4993900848168272288, -12.17626345777663488 ) ) ;
#34620 = AXIS2_PLACEMENT_3D ( 'NONE', #22347, #32635, #31994 ) ;
#34621 = ORIENTED_EDGE ( 'NONE', *, *, #9099, .T. ) ;
#34622 = FACE_OUTER_BOUND ( 'NONE', #7488, .T. ) ;
#34623 = CARTESIAN_POINT ( 'NONE',  ( 2.000000000000001776, -2.315790869867006219, -7.133520354428148025 ) ) ;
#34624 = DIRECTION ( 'NONE',  ( 0.000000000000000000, 0.01356324068817998940, -0.9999080150203989437 ) ) ;
#34625 = CARTESIAN_POINT ( 'NONE',  ( 2.241509619876136838, 3.784042210004710416, 6.630717740088868162 ) ) ;
#34626 = VERTEX_POINT ( 'NONE', #2931 ) ;
#34627 = B_SPLINE_CURVE_WITH_KNOTS ( 'NONE', 3,
 ( #21552, #41820, #31823, #47160, #35518, #61124, #15558, #619, #1274, #1609, #20879, #934, #52138, #25538, #26521, #16226 ),
 .UNSPECIFIED., .F., .F.,
 ( 4, 3, 3, 3, 3, 4 ),
 ( 0.000000000000000000, 0.0003017745587525247591, 0.0006035491769808746078, 0.0009053241094668185249, 0.001207275924539397789, 0.001510325902531782461 ),
 .UNSPECIFIED. ) ;
#34628 = EDGE_LOOP ( 'NONE', ( #52987, #59938, #41773, #1962 ) ) ;
#34629 = ORIENTED_EDGE ( 'NONE', *, *, #31405, .T. ) ;
#34630 = CARTESIAN_POINT ( 'NONE',  ( -27.10719052120871098, 2.261993590776037788, -0.6736837626858775963 ) ) ;
#34631 = ADVANCED_FACE ( 'NONE', ( #38145 ), #2150, .T. ) ;
#34632 = FACE_OUTER_BOUND ( 'NONE', #2399, .T. ) ;
#34633 = ORIENTED_EDGE ( 'NONE', *, *, #694, .T. ) ;
#34634 = DIRECTION ( 'NONE',  ( 0.000000000000000000, 0.01356324068817992175, -0.9999080150203990547 ) ) ;
#34635 = CARTESIAN_POINT ( 'NONE',  ( -37.00000000000000711, 0.000000000000000000, 0.000000000000000000 ) ) ;
#34636 = DIRECTION ( 'NONE',  ( -0.000000000000000000, -1.000000000000000000, -0.000000000000000000 ) ) ;
#34637 = ORIENTED_EDGE ( 'NONE', *, *, #52209, .F. ) ;
#34638 = CARTESIAN_POINT ( 'NONE',  ( 36.00000000000000711, 9.076753354953998709, -8.954052073409638268 ) ) ;
#34639 = CARTESIAN_POINT ( 'NONE',  ( -14.91771861688873635, -28.90354855594910433, -11.53870211790012412 ) ) ;
#34640 = FACE_OUTER_BOUND ( 'NONE', #32819, .T. ) ;
#34642 = ORIENTED_EDGE ( 'NONE', *, *, #10514, .T. ) ;
#34641 = DIRECTION ( 'NONE',  ( -1.000000000000000000, 0.000000000000000000, 0.000000000000000000 ) ) ;
#34643 = CARTESIAN_POINT ( 'NONE',  ( -22.27384469013075829, -3.548341908721032389, -0.9835229356382479970 ) ) ;
#34644 = ORIENTED_EDGE ( 'NONE', *, *, #2689, .T. ) ;
#34645 = CARTESIAN_POINT ( 'NONE',  ( 37.00000000000000711, 12.01765980939841860, -2.021542716731445921 ) ) ;
#34646 = ADVANCED_FACE ( 'NONE', ( #53476 ), #18216, .T. ) ;
#34647 = ORIENTED_EDGE ( 'NONE', *, *, #26864, .T. ) ;
#34648 = DIRECTION ( 'NONE',  ( -0.7290028908350527637, 0.000000000000000000, 0.6845106172691086677 ) ) ;
#34649 = CARTESIAN_POINT ( 'NONE',  ( 12.73158684737537349, -11.67291052772676885, -2.789930929895412248 ) ) ;
#34650 = CARTESIAN_POINT ( 'NONE',  ( -37.00000000000000711, 11.35427606708812753, -4.426194442447118682 ) ) ;
#34651 = DIRECTION ( 'NONE',  ( -1.000000000000000000, 0.000000000000000000, 0.000000000000000000 ) ) ;
#34652 = FACE_OUTER_BOUND ( 'NONE', #49404, .T. ) ;
#34653 = EDGE_CURVE ( 'NONE', #939, #34331, #1108, .T. ) ;
#34654 = CARTESIAN_POINT ( 'NONE',  ( -27.09483304420798433, -0.1669215111592733392, -2.317106154747427649 ) ) ;
#34655 = DIRECTION ( 'NONE',  ( 0.000000000000000000, 0.000000000000000000, -1.000000000000000000 ) ) ;
#34657 = ORIENTED_EDGE ( 'NONE', *, *, #9356, .F. ) ;
#34656 = DIRECTION ( 'NONE',  ( 0.000000000000000000, -0.9635499925192253512, 0.2675283385292119842 ) ) ;
#34658 = EDGE_LOOP ( 'NONE', ( #11068, #1779, #58040, #52159 ) ) ;
#34659 = CARTESIAN_POINT ( 'NONE',  ( 36.00000000000000711, -11.01837265713068703, 6.415447294506815723 ) ) ;
#34660 = ORIENTED_EDGE ( 'NONE', *, *, #64560, .T. ) ;
#34661 = EDGE_CURVE ( 'NONE', #34740, #56858, #32329, .T. ) ;
#34662 = ORIENTED_EDGE ( 'NONE', *, *, #2765, .T. ) ;
#34663 = CYLINDRICAL_SURFACE ( 'NONE', #59333, 4.999999999999999112 ) ;
#34664 = CARTESIAN_POINT ( 'NONE',  ( 2.000000000000001776, -4.444115772890149252, 5.163689623839303522 ) ) ;
#34665 = CARTESIAN_POINT ( 'NONE',  ( 2.305787727787084407, 4.792270232040973355, -5.970480882365174047 ) ) ;
#34666 = VECTOR ( 'NONE', #32118, 1000.000000000000000 ) ;
#34667 = CARTESIAN_POINT ( 'NONE',  ( 5.515539859299206427, -0.001241880655086631752, 0.005924322247674733248 ) ) ;
#34668 = CARTESIAN_POINT ( 'NONE',  ( 0.2648978790185593790, 10.67083876753491900, 6.008231198269021078 ) ) ;
#34669 = CARTESIAN_POINT ( 'NONE',  ( 2.288423627606498201, 7.242304196985708487, 2.464337058689050064 ) ) ;
#34670 = AXIS2_PLACEMENT_3D ( 'NONE', #15006, #25012, #44957 ) ;
#34671 = CYLINDRICAL_SURFACE ( 'NONE', #57842, 2.899999999999994582 ) ;
#34672 = VERTEX_POINT ( 'NONE', #13842 ) ;
#34673 = ADVANCED_FACE ( 'NONE', ( #40102 ), #29797, .T. ) ;
#34674 = DIRECTION ( 'NONE',  ( -1.000000000000000000, -1.685093406416449860E-16, 1.011030131491581592E-17 ) ) ;
#34675 = DIRECTION ( 'NONE',  ( 1.000000000000000000, -0.000000000000000000, -0.000000000000000000 ) ) ;
#34676 = CARTESIAN_POINT ( 'NONE',  ( -17.87652388884287191, -5.106857196458570947, 12.49754165357240510 ) ) ;
#34677 = EDGE_CURVE ( 'NONE', #47206, #1585, #53130, .T. ) ;
#34678 = EDGE_LOOP ( 'NONE', ( #30674, #36877, #36056, #53052 ) ) ;
#34679 = EDGE_CURVE ( 'NONE', #22010, #13960, #38818, .T. ) ;
#34680 = EDGE_CURVE ( 'NONE', #22627, #26468, #14, .T. ) ;
#34681 = CARTESIAN_POINT ( 'NONE',  ( 44.83472798829955508, -0.9996270273486139724, -15.30615170800020586 ) ) ;
#34682 = EDGE_CURVE ( 'NONE', #20446, #55528, #8884, .T. ) ;
#34683 = CARTESIAN_POINT ( 'NONE',  ( -2.532614230583022152, 25.00000000000000000, 4.026315189028233377 ) ) ;
#34684 = DIRECTION ( 'NONE',  ( -1.000000000000000000, 0.000000000000000000, 0.000000000000000000 ) ) ;
#34685 = ORIENTED_EDGE ( 'NONE', *, *, #41921, .F. ) ;
#34686 = CARTESIAN_POINT ( 'NONE',  ( 2.253265082352434945, 6.678225412356993296, -3.707567016433741980 ) ) ;
#34687 = CARTESIAN_POINT ( 'NONE',  ( 37.00000000000000711, -0.4993900848168272288, -12.17626345777663666 ) ) ;
#34688 = CARTESIAN_POINT ( 'NONE',  ( 3.959660738498543608, 6.970283272837293431, 9.778486319596556342 ) ) ;
#34689 = DIRECTION ( 'NONE',  ( 1.000000000000000000, 0.000000000000000000, 0.000000000000000000 ) ) ;
#34690 = DIRECTION ( 'NONE',  ( 1.000000000000000000, 0.000000000000000000, 0.000000000000000000 ) ) ;
#34691 = EDGE_LOOP ( 'NONE', ( #30975, #25816, #53556, #53324 ) ) ;
#34692 = AXIS2_PLACEMENT_3D ( 'NONE', #34983, #19406, #34015 ) ;
#34693 = CARTESIAN_POINT ( 'NONE',  ( 2.260457164927188511, 0.1384509728649064020, 7.639515169785717319 ) ) ;
#34694 = CARTESIAN_POINT ( 'NONE',  ( -22.27711351828769892, 3.534923377568743419, 1.028167152775488535 ) ) ;
#34695 = LINE ( 'NONE', #3012, #21221 ) ;
#34696 = ORIENTED_EDGE ( 'NONE', *, *, #37646, .F. ) ;
#34697 = DIRECTION ( 'NONE',  ( 0.000000000000000000, 0.8696919319575167062, 0.4935949184179292404 ) ) ;
#34698 = LINE ( 'NONE', #50023, #44675 ) ;
#34699 = ORIENTED_EDGE ( 'NONE', *, *, #46551, .T. ) ;
#34700 = EDGE_LOOP ( 'NONE', ( #19285, #53398, #54938, #61955 ) ) ;
#34701 = EDGE_LOOP ( 'NONE', ( #52710, #59632, #36008, #4781 ) ) ;
#34702 = CARTESIAN_POINT ( 'NONE',  ( -35.00000000000000000, -1.171570255487366152, -11.68758509253249400 ) ) ;
#34703 = ADVANCED_FACE ( 'NONE', ( #49776 ), #60080, .T. ) ;
#34704 = AXIS2_PLACEMENT_3D ( 'NONE', #30963, #41262, #30628 ) ;
#34705 = ORIENTED_EDGE ( 'NONE', *, *, #22444, .F. ) ;
#34706 = CARTESIAN_POINT ( 'NONE',  ( 1.549075743845218955, -12.34675572956545153, -2.862200647102061346 ) ) ;
#34707 = CARTESIAN_POINT ( 'NONE',  ( -19.47984447937493613, -1.416020129149132334, 25.00000000000000000 ) ) ;
#34708 = CARTESIAN_POINT ( 'NONE',  ( 0.2676618633000455993, -6.262131165853799253, 10.52491907319759967 ) ) ;
#34709 = CARTESIAN_POINT ( 'NONE',  ( -22.31328051695926007, -2.109671368890623455, -3.148362328073181615 ) ) ;
#34710 = CARTESIAN_POINT ( 'NONE',  ( -14.32520573871325631, -34.50054679313745964, 8.085438606780256166 ) ) ;
#34711 = LINE ( 'NONE', #49075, #59975 ) ;
#34713 = EDGE_LOOP ( 'NONE', ( #53444, #37834, #61196, #1463 ) ) ;
#34712 = CARTESIAN_POINT ( 'NONE',  ( 1.287602823385180839, 7.659913635102068241, 9.987902848012801371 ) ) ;
#34714 = CARTESIAN_POINT ( 'NONE',  ( 35.00000000000000000, 5.391785509271111110, 10.43555801961468887 ) ) ;
#34715 = ORIENTED_EDGE ( 'NONE', *, *, #34046, .F. ) ;
#34716 = CARTESIAN_POINT ( 'NONE',  ( 35.00000000000000000, -7.215058775251181444, 9.821084925794645315 ) ) ;
#34717 = VERTEX_POINT ( 'NONE', #60394 ) ;
#34718 = EDGE_CURVE ( 'NONE', #53581, #7512, #12764, .T. ) ;
#34719 = ORIENTED_EDGE ( 'NONE', *, *, #36737, .F. ) ;
#34720 = CARTESIAN_POINT ( 'NONE',  ( -22.31328051695926007, -0.8849444482787947042, 3.685074213229300621 ) ) ;
#34721 = CARTESIAN_POINT ( 'NONE',  ( 10.72528909898963789, -29.54774166152794734, 10.19639468772756530 ) ) ;
#34722 = CARTESIAN_POINT ( 'NONE',  ( -22.27384469013076185, -0.3730095848193254460, -3.663183248998795882 ) ) ;
#34723 = DIRECTION ( 'NONE',  ( -1.000000000000000000, 0.000000000000000000, 0.000000000000000000 ) ) ;
#34724 = DIRECTION ( 'NONE',  ( -1.000000000000000000, -0.000000000000000000, 0.000000000000000000 ) ) ;
#34725 = CARTESIAN_POINT ( 'NONE',  ( 2.000000000000001776, 6.935703035393448346, -0.1051458740707923722 ) ) ;
#34726 = VERTEX_POINT ( 'NONE', #28500 ) ;
#34727 =( BOUNDED_SURFACE ( )  B_SPLINE_SURFACE ( 3, 1, ( 
 ( #60199, #56187 ),
 ( #46239, #35244 ),
 ( #50245, #65496 ),
 ( #9996, #4359 ) ),
 .UNSPECIFIED., .F., .F., .F. ) 
 B_SPLINE_SURFACE_WITH_KNOTS ( ( 4, 4 ),
 ( 2, 2 ),
 ( 0.000000000000000000, 1.000000000000000000 ),
 ( 0.000000000000000000, 1.000000000000000000 ),
 .UNSPECIFIED. ) 
 GEOMETRIC_REPRESENTATION_ITEM ( )  RATIONAL_B_SPLINE_SURFACE ( (
 ( 1.000000000000000000, 1.000000000000000000),
 ( 0.6933888150995267674, 0.9895912004443193632),
 ( 0.6933888150995267674, 0.9895912004443193632),
 ( 1.000000000000000000, 1.000000000000000000) ) ) 
 REPRESENTATION_ITEM ( '' )  SURFACE ( )  );
#34728 = ORIENTED_EDGE ( 'NONE', *, *, #24430, .T. ) ;
#34729 = CARTESIAN_POINT ( 'NONE',  ( 5.520433897694421610, -0.01505375422439122687, 0.0005131706886599850161 ) ) ;
#34730 = ORIENTED_EDGE ( 'NONE', *, *, #36465, .F. ) ;
#34731 = EDGE_CURVE ( 'NONE', #53501, #32268, #32941, .T. ) ;
#34732 = ORIENTED_EDGE ( 'NONE', *, *, #22826, .F. ) ;
#34733 = CARTESIAN_POINT ( 'NONE',  ( 2.000000000000001776, 0.000000000000000000, 0.000000000000000000 ) ) ;
#34734 = CARTESIAN_POINT ( 'NONE',  ( -22.27706089016750113, 0.9798385173596402264, -3.548384797797537793 ) ) ;
#34735 = CARTESIAN_POINT ( 'NONE',  ( 1.283627346226613009, -12.28700367512546343, 2.725559306498961831 ) ) ;
#34736 = EDGE_CURVE ( 'NONE', #23637, #42619, #54775, .T. ) ;
#34737 = DIRECTION ( 'NONE',  ( 0.000000000000000000, -0.1081190184239488317, 0.9941379571543589311 ) ) ;
#34738 = CARTESIAN_POINT ( 'NONE',  ( 8.937200413559443390, 4.476360154859203355, 25.00000000000000000 ) ) ;
#34739 = LINE ( 'NONE', #4183, #7907 ) ;
#34740 = VERTEX_POINT ( 'NONE', #14499 ) ;
#34741 = ORIENTED_EDGE ( 'NONE', *, *, #49428, .F. ) ;
#34742 = DIRECTION ( 'NONE',  ( 0.000000000000000000, 0.000000000000000000, 1.000000000000000000 ) ) ;
#34743 = FACE_OUTER_BOUND ( 'NONE', #36304, .T. ) ;
#34744 = VECTOR ( 'NONE', #57417, 1000.000000000000000 ) ;
#34745 = LINE ( 'NONE', #64679, #44656 ) ;
#34746 = EDGE_CURVE ( 'NONE', #35130, #47761, #21276, .T. ) ;
#34747 = ORIENTED_EDGE ( 'NONE', *, *, #33623, .T. ) ;
#34748 = CARTESIAN_POINT ( 'NONE',  ( -27.74314290831961927, 13.27105638519637054, -2.536820231170034301 ) ) ;
#34749 = AXIS2_PLACEMENT_3D ( 'NONE', #35467, #38917, #13624 ) ;
#34750 = EDGE_CURVE ( 'NONE', #35169, #52094, #13806, .T. ) ;
#34751 = CARTESIAN_POINT ( 'NONE',  ( 0.000000000000000000, 244.9489742783177917, 23.99999999999999289 ) ) ;
#34752 = DIRECTION ( 'NONE',  ( 1.000000000000000000, 0.000000000000000000, 0.000000000000000000 ) ) ;
#34753 = EDGE_CURVE ( 'NONE', #29901, #37187, #8230, .T. ) ;
#34754 = CARTESIAN_POINT ( 'NONE',  ( 2.305787727787083519, 5.970480882365222897, 4.792270232040915623 ) ) ;
#34755 = DIRECTION ( 'NONE',  ( 1.000000000000000000, 0.000000000000000000, 0.000000000000000000 ) ) ;
#34756 = ORIENTED_EDGE ( 'NONE', *, *, #5950, .F. ) ;
#34757 = DIRECTION ( 'NONE',  ( 0.000000000000000000, 0.9985334138511235968, 0.05413890858542115547 ) ) ;
#34758 = CARTESIAN_POINT ( 'NONE',  ( 5.514970785353741078, 0.004324946436530306346, -0.001897634820904968824 ) ) ;
#34759 = DIRECTION ( 'NONE',  ( 1.000000000000000000, 0.000000000000000000, 0.000000000000000000 ) ) ;
#34760 = EDGE_CURVE ( 'NONE', #10376, #15607, #11602, .T. ) ;
#34761 = DIRECTION ( 'NONE',  ( -0.8214942970785323872, -0.5702167306099040767, 0.000000000000000000 ) ) ;
#34762 = CARTESIAN_POINT ( 'NONE',  ( 3.291290029914074378, 8.250315036047103590, 10.68561190601527855 ) ) ;
#34763 = ORIENTED_EDGE ( 'NONE', *, *, #33640, .F. ) ;
#34764 = CARTESIAN_POINT ( 'NONE',  ( 2.259025283528085737, -2.484282765458397435, 7.225123487442759895 ) ) ;
#34765 = LINE ( 'NONE', #45750, #4670 ) ;
#34766 = CARTESIAN_POINT ( 'NONE',  ( 6.676753782886446942, -28.39896155677452683, -11.13103273143453720 ) ) ;
#34767 = ORIENTED_EDGE ( 'NONE', *, *, #25523, .T. ) ;
#34768 = LINE ( 'NONE', #20490, #49343 ) ;
#34769 = CARTESIAN_POINT ( 'NONE',  ( -22.49803948133826026, 4.343047530463596928, -0.1132714802761584233 ) ) ;
#34770 = CARTESIAN_POINT ( 'NONE',  ( -22.27710395300133328, -0.9291085174899353927, -3.562137928983406088 ) ) ;
#34771 = CARTESIAN_POINT ( 'NONE',  ( 0.7446945582506544481, 12.40088838629945300, 0.3561743995932071249 ) ) ;
#34772 = CARTESIAN_POINT ( 'NONE',  ( -9.764253471131736362, -12.49999450231236153, -5.102826708558637847 ) ) ;
#34773 = CIRCLE ( 'NONE', #61366, 12.18650000000000055 ) ;
#34774 = DIRECTION ( 'NONE',  ( 0.000000000000000000, -0.2618041379715704275, 0.9651210252299774472 ) ) ;
#34775 = ORIENTED_EDGE ( 'NONE', *, *, #65354, .F. ) ;
#34776 = DIRECTION ( 'NONE',  ( 0.000000000000000000, 0.000000000000000000, 1.000000000000000000 ) ) ;
#34777 = EDGE_CURVE ( 'NONE', #16609, #63997, #45116, .T. ) ;
#34778 = LINE ( 'NONE', #61068, #37242 ) ;
#34779 = VECTOR ( 'NONE', #22333, 1000.000000000000000 ) ;
#34780 = CARTESIAN_POINT ( 'NONE',  ( 0.000000000000000000, 5.860254403322016969, 3.474373880649828550 ) ) ;
#34781 = DIRECTION ( 'NONE',  ( -1.000000000000000000, 0.000000000000000000, -0.000000000000000000 ) ) ;
#34782 = DIRECTION ( 'NONE',  ( -1.000000000000000000, 0.000000000000000000, 0.000000000000000000 ) ) ;
#34783 = CARTESIAN_POINT ( 'NONE',  ( 0.000000000000000000, 1.523986892267801462E-15, 12.15774668701806149 ) ) ;
#34784 = DIRECTION ( 'NONE',  ( 0.000000000000000000, 0.7790879021242484992, -0.6269146997508012742 ) ) ;
#34785 = CARTESIAN_POINT ( 'NONE',  ( 2.273267844203311849, 1.178226273334160412, -7.553702825375153473 ) ) ;
#34786 = ORIENTED_EDGE ( 'NONE', *, *, #8748, .F. ) ;
#34787 = ORIENTED_EDGE ( 'NONE', *, *, #22453, .F. ) ;
#34788 = DIRECTION ( 'NONE',  ( 0.000000000000000000, -0.9346839223284501008, 0.3554799084909069928 ) ) ;
#34789 = ORIENTED_EDGE ( 'NONE', *, *, #49065, .T. ) ;
#34790 = EDGE_CURVE ( 'NONE', #38454, #22430, #49951, .T. ) ;
#34791 = CIRCLE ( 'NONE', #41160, 12.74999999999999822 ) ;
#34792 = CARTESIAN_POINT ( 'NONE',  ( 0.000000000000000000, -45.00000000000000000, 0.000000000000000000 ) ) ;
#34793 = VECTOR ( 'NONE', #59779, 1000.000000000000000 ) ;
#34794 = CARTESIAN_POINT ( 'NONE',  ( 35.00000000000000000, -11.07407352312215387, -3.916263239775311433 ) ) ;
#34795 = VERTEX_POINT ( 'NONE', #56059 ) ;
#34796 = CARTESIAN_POINT ( 'NONE',  ( -35.00000000000000000, 0.000000000000000000, 0.000000000000000000 ) ) ;
#34797 = CARTESIAN_POINT ( 'NONE',  ( 35.00000000000000000, -12.21925492305364536, -3.640372113593510761 ) ) ;
#34798 = CARTESIAN_POINT ( 'NONE',  ( 23.48675979904455957, 2.894400836696811918, 13.18980151006969415 ) ) ;
#34799 = VERTEX_POINT ( 'NONE', #46113 ) ;
#34800 = ORIENTED_EDGE ( 'NONE', *, *, #17934, .T. ) ;
#34801 = DIRECTION ( 'NONE',  ( -1.000000000000000000, 0.000000000000000000, 0.000000000000000000 ) ) ;
#34802 = EDGE_CURVE ( 'NONE', #3877, #53943, #62050, .T. ) ;
#34803 = ADVANCED_FACE ( 'NONE', ( #40434 ), #9483, .F. ) ;
#34804 = ORIENTED_EDGE ( 'NONE', *, *, #34122, .T. ) ;
#34805 = CARTESIAN_POINT ( 'NONE',  ( -47.00000000000000711, 0.000000000000000000, 0.000000000000000000 ) ) ;
#34806 = EDGE_LOOP ( 'NONE', ( #57757, #63497, #41044, #2620 ) ) ;
#34807 = CARTESIAN_POINT ( 'NONE',  ( 35.00000000000000000, 1.903127969211351189, 11.59095880812005497 ) ) ;
#34808 = EDGE_CURVE ( 'NONE', #3067, #45140, #57358, .T. ) ;
#34809 = LINE ( 'NONE', #45800, #63428 ) ;
#34810 = CARTESIAN_POINT ( 'NONE',  ( 2.440552418640494992, -4.020120046181088647, 6.568204543009814600 ) ) ;
#34811 = DIRECTION ( 'NONE',  ( 0.000000000000000000, 0.000000000000000000, 1.000000000000000000 ) ) ;
#34812 = CARTESIAN_POINT ( 'NONE',  ( 0.3341166715381236330, 11.61315925169694729, 3.958014133396652312 ) ) ;
#34813 = VERTEX_POINT ( 'NONE', #30776 ) ;
#34814 = CARTESIAN_POINT ( 'NONE',  ( 1.719304012339881282, -12.20344780066076318, 3.626341562669963992 ) ) ;
#34815 = FACE_OUTER_BOUND ( 'NONE', #57646, .T. ) ;
#34816 = CARTESIAN_POINT ( 'NONE',  ( 35.00000000000000000, 6.102719229070673990, -10.54834585426222304 ) ) ;
#34817 = DIRECTION ( 'NONE',  ( 1.000000000000000000, 0.000000000000000000, -0.000000000000000000 ) ) ;
#34818 = CARTESIAN_POINT ( 'NONE',  ( 12.87184510392629200, 12.70280640453755794, -4.586614403938258810 ) ) ;
#34819 = CARTESIAN_POINT ( 'NONE',  ( 0.9296196016848956578, 0.4155906739605440547, -12.46069139398492176 ) ) ;
#34820 = DIRECTION ( 'NONE',  ( -1.000000000000000000, -0.000000000000000000, 0.000000000000000000 ) ) ;
#34821 = CARTESIAN_POINT ( 'NONE',  ( 0.000000000000000000, 0.000000000000000000, 0.000000000000000000 ) ) ;
#34822 = DIRECTION ( 'NONE',  ( -0.000000000000000000, -0.000000000000000000, -1.000000000000000000 ) ) ;
#34823 = EDGE_CURVE ( 'NONE', #58530, #51219, #25820, .T. ) ;
#34824 = CIRCLE ( 'NONE', #3025, 5.000000000000000888 ) ;
#34825 = ORIENTED_EDGE ( 'NONE', *, *, #4882, .T. ) ;
#34826 = CARTESIAN_POINT ( 'NONE',  ( 0.2648978790185602672, 0.1321385342562404197, 12.24533305150758089 ) ) ;
#34827 = CIRCLE ( 'NONE', #64600, 7.499999999999988454 ) ;
#34828 = ORIENTED_EDGE ( 'NONE', *, *, #39476, .T. ) ;
#34829 = DIRECTION ( 'NONE',  ( 0.000000000000000000, 0.2618041379715633776, -0.9651210252299794456 ) ) ;
#34830 = DIRECTION ( 'NONE',  ( 1.000000000000000000, 0.000000000000000000, 0.000000000000000000 ) ) ;
#34831 = CARTESIAN_POINT ( 'NONE',  ( 2.241509619876138171, -4.936617871859544593, 5.823675573301060560 ) ) ;
#34832 = VECTOR ( 'NONE', #10068, 1000.000000000000000 ) ;
#34833 = CARTESIAN_POINT ( 'NONE',  ( 0.2652384529303136174, -12.04846370803830524, 2.191562200667146687 ) ) ;
#34834 = CARTESIAN_POINT ( 'NONE',  ( 2.368238019615418466, 5.070835960313035962, 5.763545178420164561 ) ) ;
#34835 = VERTEX_POINT ( 'NONE', #20823 ) ;
#34836 = CARTESIAN_POINT ( 'NONE',  ( 5.515539859299206427, -0.006049968793488395835, -0.0001942659352248416859 ) ) ;
#34837 = CARTESIAN_POINT ( 'NONE',  ( 2.305787727787084407, 0.1666591538752685842, 7.654065630109507801 ) ) ;
#34838 = CARTESIAN_POINT ( 'NONE',  ( -27.08871896697694837, 2.082324523415888695, 0.9878677378266799147 ) ) ;
#34839 = CARTESIAN_POINT ( 'NONE',  ( 1.372161826076019109, 2.769012792636492026, 12.30755118281438243 ) ) ;
#34840 = ADVANCED_FACE ( 'NONE', ( #36090 ), #35453, .T. ) ;
#34841 = CARTESIAN_POINT ( 'NONE',  ( 36.00000000000000711, -11.90598845858536947, -4.561791185930373693 ) ) ;
#34842 = VERTEX_POINT ( 'NONE', #50759 ) ;
#34843 = CARTESIAN_POINT ( 'NONE',  ( 0.000000000000000000, -1.018311147294094443, -6.861346417234492456 ) ) ;
#34844 = ORIENTED_EDGE ( 'NONE', *, *, #43841, .F. ) ;
#34845 = DIRECTION ( 'NONE',  ( 0.000000000000000000, 0.000000000000000000, 1.000000000000000000 ) ) ;
#34846 = CARTESIAN_POINT ( 'NONE',  ( -13.30196514322326529, -33.37310655729285003, 10.51054543287779097 ) ) ;
#34847 = LINE ( 'NONE', #9585, #64971 ) ;
#34848 = DIRECTION ( 'NONE',  ( -1.000000000000000000, 0.000000000000000000, 0.000000000000000000 ) ) ;
#34849 = CIRCLE ( 'NONE', #5182, 5.000000000000000000 ) ;
#34850 = ORIENTED_EDGE ( 'NONE', *, *, #11035, .T. ) ;
#34851 = ORIENTED_EDGE ( 'NONE', *, *, #47684, .T. ) ;
#34852 = CARTESIAN_POINT ( 'NONE',  ( 0.000000000000000000, 4.376687952327412034, -5.220963330856592144 ) ) ;
#34853 = VERTEX_POINT ( 'NONE', #56755 ) ;
#34854 = EDGE_CURVE ( 'NONE', #13076, #43273, #15605, .T. ) ;
#34855 = FACE_OUTER_BOUND ( 'NONE', #8258, .T. ) ;
#34856 = DIRECTION ( 'NONE',  ( 1.000000000000000000, 0.000000000000000000, 0.000000000000000000 ) ) ;
#34857 = CARTESIAN_POINT ( 'NONE',  ( -22.27709082389155171, -3.541295940224330252, -1.005749854561710510 ) ) ;
#34858 = DIRECTION ( 'NONE',  ( -1.000000000000000000, 0.000000000000000000, 0.000000000000000000 ) ) ;
#34860 = DIRECTION ( 'NONE',  ( 0.000000000000000000, -0.7790879021242573810, 0.6269146997507903940 ) ) ;
#34859 = AXIS2_PLACEMENT_3D ( 'NONE', #62377, #23146, #52759 ) ;
#34861 = CARTESIAN_POINT ( 'NONE',  ( 35.00000000000000000, -5.921969905510278132, 10.14408668126219304 ) ) ;
#34862 = FACE_OUTER_BOUND ( 'NONE', #42982, .T. ) ;
#34863 = ORIENTED_EDGE ( 'NONE', *, *, #32021, .F. ) ;
#34865 = ORIENTED_EDGE ( 'NONE', *, *, #5471, .T. ) ;
#34864 = CARTESIAN_POINT ( 'NONE',  ( -22.46225619532222950, 0.1595555201818359137, 4.233934615764590959 ) ) ;
#34866 = ORIENTED_EDGE ( 'NONE', *, *, #16787, .F. ) ;
#34867 = FACE_OUTER_BOUND ( 'NONE', #43240, .T. ) ;
#34868 = VECTOR ( 'NONE', #41789, 1000.000000000000000 ) ;
#34869 = CYLINDRICAL_SURFACE ( 'NONE', #54450, 13.50000000000000178 ) ;
#34870 = EDGE_CURVE ( 'NONE', #37505, #5308, #16456, .T. ) ;
#34871 = VERTEX_POINT ( 'NONE', #10841 ) ;
#34872 = CARTESIAN_POINT ( 'NONE',  ( 2.000000000000001776, 6.767909380267608022, 2.119450094687897579 ) ) ;
#34874 = ORIENTED_EDGE ( 'NONE', *, *, #53986, .T. ) ;
#34873 = VECTOR ( 'NONE', #7900, 1000.000000000000114 ) ;
#34875 = CIRCLE ( 'NONE', #42276, 12.18649999999999878 ) ;
#34876 = CYLINDRICAL_SURFACE ( 'NONE', #58823, 4.999999999999999112 ) ;
#34877 = CARTESIAN_POINT ( 'NONE',  ( 3.709820702086316757, -10.52816917254576623, -8.451371970425016755 ) ) ;
#34878 = CARTESIAN_POINT ( 'NONE',  ( 0.000000000000000000, -33.00000000000000000, 0.000000000000000000 ) ) ;
#34879 = CARTESIAN_POINT ( 'NONE',  ( 5.650485762548542290, -9.979623674447639203, 6.674921982999905801 ) ) ;
#34880 = ORIENTED_EDGE ( 'NONE', *, *, #32637, .T. ) ;
#34881 = EDGE_LOOP ( 'NONE', ( #13813, #40643, #15859, #27149 ) ) ;
#34882 = AXIS2_PLACEMENT_3D ( 'NONE', #13651, #64517, #13981 ) ;
#34883 = CARTESIAN_POINT ( 'NONE',  ( -47.00000000000000711, 0.000000000000000000, 0.000000000000000000 ) ) ;
#34884 = ORIENTED_EDGE ( 'NONE', *, *, #42693, .F. ) ;
#34885 = ADVANCED_FACE ( 'NONE', ( #31129 ), #51440, .T. ) ;
#34886 = EDGE_CURVE ( 'NONE', #28625, #43866, #7450, .T. ) ;
#34887 = CARTESIAN_POINT ( 'NONE',  ( 0.3537226245948384418, 11.62199823003439292, -3.952322262392271579 ) ) ;
#34888 = EDGE_LOOP ( 'NONE', ( #44143, #15153, #32218, #55686 ) ) ;
#34889 = ORIENTED_EDGE ( 'NONE', *, *, #57375, .F. ) ;
#34890 = CIRCLE ( 'NONE', #5169, 5.000000000000000888 ) ;
#34891 = VERTEX_POINT ( 'NONE', #2531 ) ;
#34892 = DIRECTION ( 'NONE',  ( 0.000000000000000000, 0.01356324068817998940, -0.9999080150203990547 ) ) ;
#34893 = CARTESIAN_POINT ( 'NONE',  ( -5.894163417187625598, -31.16155000483812998, -14.52685451767917080 ) ) ;
#34894 = CARTESIAN_POINT ( 'NONE',  ( -27.35552965826137140, 2.810569013793760007, -1.320216934008374920 ) ) ;
#34895 = CARTESIAN_POINT ( 'NONE',  ( -22.65999102136915866, -2.911035239830966681, 3.858590659383635213 ) ) ;
#34896 = ORIENTED_EDGE ( 'NONE', *, *, #57328, .F. ) ;
#34897 = CARTESIAN_POINT ( 'NONE',  ( 2.261269890821707484, -2.481875047313262250, -7.226741992146552995 ) ) ;
#34898 = ORIENTED_EDGE ( 'NONE', *, *, #54595, .F. ) ;
#34899 = CARTESIAN_POINT ( 'NONE',  ( 35.00000000000000000, 4.732539170486261604, -11.23004253107766282 ) ) ;
#34900 = DIRECTION ( 'NONE',  ( -1.000000000000000000, 0.000000000000000000, 0.000000000000000000 ) ) ;
#34901 = ORIENTED_EDGE ( 'NONE', *, *, #58894, .F. ) ;
#34902 = CARTESIAN_POINT ( 'NONE',  ( -27.01437459610461644, 10.69338818478080455, -8.240233560378637634 ) ) ;
#34903 = CARTESIAN_POINT ( 'NONE',  ( 26.47552525366476672, 11.32202890774585491, 3.984464554639796763 ) ) ;
#34904 = CARTESIAN_POINT ( 'NONE',  ( 2.280717697723833037, -6.699799459371637234, -3.687451363405637839 ) ) ;
#34905 = AXIS2_PLACEMENT_3D ( 'NONE', #18811, #49087, #38425 ) ;
#34906 = ORIENTED_EDGE ( 'NONE', *, *, #26868, .F. ) ;
#34907 = CARTESIAN_POINT ( 'NONE',  ( 2.273267844204866606, -7.643541951623946673, 0.1513603614830237865 ) ) ;
#34908 = AXIS2_PLACEMENT_3D ( 'NONE', #23077, #13411, #24061 ) ;
#34909 = ORIENTED_EDGE ( 'NONE', *, *, #19448, .F. ) ;
#34910 = CARTESIAN_POINT ( 'NONE',  ( 0.2767916011545367705, 10.70244578860295981, 5.959903879715624520 ) ) ;
#34911 = CYLINDRICAL_SURFACE ( 'NONE', #59519, 12.75000000000000178 ) ;
#34912 = CARTESIAN_POINT ( 'NONE',  ( 2.963017218115624907, 7.004145770368821466, -3.599595431209413388 ) ) ;
#34913 = CARTESIAN_POINT ( 'NONE',  ( 2.000000000000001776, 6.883677378339475794, 0.8544109087186002593 ) ) ;
#34914 = CARTESIAN_POINT ( 'NONE',  ( -37.00000000000000711, -10.59380114696474884, 7.094637218249319588 ) ) ;
#34915 = ORIENTED_EDGE ( 'NONE', *, *, #62573, .F. ) ;
#34916 = EDGE_CURVE ( 'NONE', #44487, #36493, #64781, .T. ) ;
#34917 = DIRECTION ( 'NONE',  ( -1.000000000000000000, 0.000000000000000000, -0.000000000000000000 ) ) ;
#34918 = DIRECTION ( 'NONE',  ( -1.000000000000000000, 0.000000000000000000, 0.000000000000000000 ) ) ;
#34919 = CARTESIAN_POINT ( 'NONE',  ( -22.30625920655495165, -2.750410778797871547, -2.610366806364701642 ) ) ;
#34920 = DIRECTION ( 'NONE',  ( 1.000000000000000000, 0.000000000000000000, 0.000000000000000000 ) ) ;
#34921 = VECTOR ( 'NONE', #14496, 1000.000000000000000 ) ;
#34922 = ADVANCED_FACE ( 'NONE', ( #47094 ), #36769, .T. ) ;
#34923 = CIRCLE ( 'NONE', #3131, 12.75000000000000178 ) ;
#34924 = DIRECTION ( 'NONE',  ( 0.000000000000000000, -0.01356324068817991828, 0.9999080150203990547 ) ) ;
#34925 =( BOUNDED_CURVE ( )  B_SPLINE_CURVE ( 3, ( #21083, #61649, #16102, #36389 ),
 .UNSPECIFIED., .F., .F. ) 
 B_SPLINE_CURVE_WITH_KNOTS ( ( 4, 4 ),
 ( 3.908502672100578668, 3.937696279019239132 ),
 .UNSPECIFIED. ) 
 CURVE ( )  GEOMETRIC_REPRESENTATION_ITEM ( )  RATIONAL_B_SPLINE_CURVE ( ( 1.000000000000000000, 0.9999289790372866138, 0.9999289790372866138, 1.000000000000000000 ) ) 
 REPRESENTATION_ITEM ( '' )  );
#34926 = CARTESIAN_POINT ( 'NONE',  ( 2.241352910868908310, 2.689314586382351546, 7.145045428366586293 ) ) ;
#34927 = CARTESIAN_POINT ( 'NONE',  ( 2.280717697723835258, -5.957695241725366131, -4.794838658391083364 ) ) ;
#34928 = DIRECTION ( 'NONE',  ( -1.000000000000000000, 0.000000000000000000, 0.000000000000000000 ) ) ;
#34929 = DIRECTION ( 'NONE',  ( -1.000000000000000000, 0.000000000000000000, -0.000000000000000000 ) ) ;
#34930 = AXIS2_PLACEMENT_3D ( 'NONE', #13425, #23412, #59011 ) ;
#34931 = EDGE_CURVE ( 'NONE', #54137, #49507, #55259, .T. ) ;
#34932 = ORIENTED_EDGE ( 'NONE', *, *, #5842, .F. ) ;
#34933 = DIRECTION ( 'NONE',  ( 0.000000000000000000, 0.9551603052523468529, -0.2960891610144545938 ) ) ;
#34935 = ORIENTED_EDGE ( 'NONE', *, *, #17797, .F. ) ;
#34934 = ADVANCED_FACE ( 'NONE', ( #47421 ), #27769, .T. ) ;
#34936 = CARTESIAN_POINT ( 'NONE',  ( -14.11589373245165469, 8.250315036047107142, -8.713914264323175729 ) ) ;
#34937 = CARTESIAN_POINT ( 'NONE',  ( 35.00000000000000000, -6.547236723513950807, 9.752226076388957665 ) ) ;
#34938 = CARTESIAN_POINT ( 'NONE',  ( 35.00000000000000000, 4.705694406421931860E-17, -3.469127814946512892E-15 ) ) ;
#34939 = CARTESIAN_POINT ( 'NONE',  ( 2.241352910868908754, -1.243507963608043498, -7.532448145350521429 ) ) ;
#34940 = EDGE_CURVE ( 'NONE', #43097, #16340, #22457, .T. ) ;
#34941 = VERTEX_POINT ( 'NONE', #17143 ) ;
#34942 = ORIENTED_EDGE ( 'NONE', *, *, #21685, .F. ) ;
#34943 = VERTEX_POINT ( 'NONE', #31761 ) ;
#34944 = DIRECTION ( 'NONE',  ( -0.3939253465568944290, 0.1500280335741595583, -0.9068155327749417571 ) ) ;
#34946 = CARTESIAN_POINT ( 'NONE',  ( -35.00000000000000000, 0.000000000000000000, 0.000000000000000000 ) ) ;
#34945 = CIRCLE ( 'NONE', #8448, 5.000000000000000000 ) ;
#34947 = EDGE_CURVE ( 'NONE', #62776, #1482, #28677, .T. ) ;
#34948 = VERTEX_POINT ( 'NONE', #57728 ) ;
#34949 = LINE ( 'NONE', #45951, #23881 ) ;
#34950 = LINE ( 'NONE', #29986, #18791 ) ;
#34951 = CYLINDRICAL_SURFACE ( 'NONE', #42869, 12.75000000000000178 ) ;
#34952 = EDGE_LOOP ( 'NONE', ( #49464, #19636, #23544, #16337 ) ) ;
#34953 = CARTESIAN_POINT ( 'NONE',  ( -27.22222364661110916, -10.76538614228702428, 5.304738902579489768 ) ) ;
#34954 = VECTOR ( 'NONE', #48936, 1000.000000000000000 ) ;
#34955 = ADVANCED_FACE ( 'NONE', ( #63335, #37084 ), #12149, .F. ) ;
#34956 = CARTESIAN_POINT ( 'NONE',  ( -4.505835087370986258, -30.89562805149607172, -14.87534964460527753 ) ) ;
#34957 = DIRECTION ( 'NONE',  ( 1.000000000000000000, -0.000000000000000000, -0.000000000000000000 ) ) ;
#34959 = EDGE_LOOP ( 'NONE', ( #62690, #53973, #36407, #31276 ) ) ;
#34958 = CARTESIAN_POINT ( 'NONE',  ( 11.86932257037118532, -8.667155996924371664, -8.300945040779890149 ) ) ;
#34960 = DIRECTION ( 'NONE',  ( 1.000000000000000000, 0.000000000000000000, 0.000000000000000000 ) ) ;
#34961 = VERTEX_POINT ( 'NONE', #11810 ) ;
#34962 = DIRECTION ( 'NONE',  ( -1.000000000000000000, 0.000000000000000000, 0.000000000000000000 ) ) ;
#34963 = ORIENTED_EDGE ( 'NONE', *, *, #46482, .F. ) ;
#34964 = DIRECTION ( 'NONE',  ( 1.000000000000000000, -0.000000000000000000, -0.000000000000000000 ) ) ;
#34965 = CARTESIAN_POINT ( 'NONE',  ( 13.33826709797422794, -11.16011261617231121, -4.415959474372655791 ) ) ;
#34966 = VECTOR ( 'NONE', #17650, 1000.000000000000114 ) ;
#34967 = DIRECTION ( 'NONE',  ( 0.000000000000000000, -0.01356324068817998940, 0.9999080150203990547 ) ) ;
#34968 = DIRECTION ( 'NONE',  ( 0.000000000000000000, -0.01356324068817991828, 0.9999080150203990547 ) ) ;
#34969 = CARTESIAN_POINT ( 'NONE',  ( 1.000000000000000888, 5.662015959325201742, 4.918493191653995567 ) ) ;
#34970 = CARTESIAN_POINT ( 'NONE',  ( -27.08429572838383947, -2.089332284968714593, -0.9410937941434025511 ) ) ;
#34971 = CARTESIAN_POINT ( 'NONE',  ( 2.251152103363648571, 5.769488058190800572, -5.004701566805173307 ) ) ;
#34972 = CARTESIAN_POINT ( 'NONE',  ( 37.00000000000000711, 9.217970097227837556, 7.971186206369369032 ) ) ;
#34973 = FACE_OUTER_BOUND ( 'NONE', #52364, .T. ) ;
#34975 = VERTEX_POINT ( 'NONE', #27433 ) ;
#34974 = DIRECTION ( 'NONE',  ( 1.000000000000000000, 0.000000000000000000, -0.000000000000000000 ) ) ;
#34976 = EDGE_CURVE ( 'NONE', #6394, #52020, #41475, .T. ) ;
#34977 = VECTOR ( 'NONE', #58199, 1000.000000000000000 ) ;
#34978 = ORIENTED_EDGE ( 'NONE', *, *, #58580, .T. ) ;
#34979 = CARTESIAN_POINT ( 'NONE',  ( 35.00000000000000000, 0.3137578094511070947, 12.74613886779083849 ) ) ;
#34980 = ORIENTED_EDGE ( 'NONE', *, *, #29602, .T. ) ;
#34981 = ORIENTED_EDGE ( 'NONE', *, *, #16291, .F. ) ;
#34982 = CARTESIAN_POINT ( 'NONE',  ( 25.05309951391468459, 8.823569016628493245, -8.132934882857099979 ) ) ;
#34983 = CARTESIAN_POINT ( 'NONE',  ( 3.152665057734040488, 0.000000000000000000, 0.000000000000000000 ) ) ;
#34984 = AXIS2_PLACEMENT_3D ( 'NONE', #1316, #27540, #17588 ) ;
#34985 = CARTESIAN_POINT ( 'NONE',  ( 5.516018279890452902, 0.005331956019561711300, -0.004180585980734999839 ) ) ;
#34986 = CARTESIAN_POINT ( 'NONE',  ( -22.28236030719477867, 1.572829798448341698, -3.345835236227589604 ) ) ;
#34987 = CARTESIAN_POINT ( 'NONE',  ( 0.2657645697724699274, 10.68050050043099297, -5.991637049003132098 ) ) ;
#34988 = DIRECTION ( 'NONE',  ( 1.000000000000000000, 0.000000000000000000, -0.000000000000000000 ) ) ;
#34989 = EDGE_LOOP ( 'NONE', ( #15728, #18045, #19217, #14615 ) ) ;
#34990 = CARTESIAN_POINT ( 'NONE',  ( 2.639814597422732056, -6.111633106000453175, 4.793557287999607119 ) ) ;
#34991 = DIRECTION ( 'NONE',  ( 0.000000000000000000, 0.01356324068817998940, -0.9999080150203990547 ) ) ;
#34992 = DIRECTION ( 'NONE',  ( -1.000000000000000000, 0.000000000000000000, 0.000000000000000000 ) ) ;
#34993 = ORIENTED_EDGE ( 'NONE', *, *, #42145, .F. ) ;
#34994 = EDGE_CURVE ( 'NONE', #12280, #26022, #12460, .T. ) ;
#34995 = VECTOR ( 'NONE', #3003, 1000.000000000000000 ) ;
#34996 = CIRCLE ( 'NONE', #32913, 12.18650000000000055 ) ;
#34997 = CIRCLE ( 'NONE', #50942, 7.499999999999988454 ) ;
#34998 = CARTESIAN_POINT ( 'NONE',  ( 40.23304019309009760, -1.796181362175405249, 19.88949158386753524 ) ) ;
#34999 = CARTESIAN_POINT ( 'NONE',  ( 35.00000000000000000, 4.705694406421931860E-17, -3.469127814946512892E-15 ) ) ;
#35000 = CARTESIAN_POINT ( 'NONE',  ( -10.00000000000000178, 0.000000000000000000, 0.000000000000000000 ) ) ;
#35001 = ORIENTED_EDGE ( 'NONE', *, *, #60502, .F. ) ;
#35002 = CYLINDRICAL_SURFACE ( 'NONE', #57454, 4.999999999999999112 ) ;
#35003 = CARTESIAN_POINT ( 'NONE',  ( 4.563054428376214666, -30.91385115595774735, 14.84911024294817850 ) ) ;
#35004 = FACE_OUTER_BOUND ( 'NONE', #56542, .T. ) ;
#35005 = AXIS2_PLACEMENT_3D ( 'NONE', #42473, #17892, #7582 ) ;
#35006 = EDGE_CURVE ( 'NONE', #23475, #4911, #18155, .T. ) ;
#35007 = LINE ( 'NONE', #59995, #58639 ) ;
#35008 = DIRECTION ( 'NONE',  ( -1.000000000000000000, 0.000000000000000000, -0.000000000000000000 ) ) ;
#35009 = AXIS2_PLACEMENT_3D ( 'NONE', #47179, #33166, #12231 ) ;
#35010 = ORIENTED_EDGE ( 'NONE', *, *, #3875, .F. ) ;
#35011 = EDGE_CURVE ( 'NONE', #63287, #32302, #28336, .T. ) ;
#35012 = CARTESIAN_POINT ( 'NONE',  ( -37.00000000000000711, -11.65150730582933392, -1.488153103997089888 ) ) ;
#35013 = CARTESIAN_POINT ( 'NONE',  ( -9.514691729518425234, -11.30278532684398485, -4.051020386293188835 ) ) ;
#35014 = CARTESIAN_POINT ( 'NONE',  ( -22.29770266787582500, 3.593535545924351648, -1.047554374660431442 ) ) ;
#35015 = EDGE_LOOP ( 'NONE', ( #18581, #44871, #58986, #53058 ) ) ;
#35016 = LINE ( 'NONE', #130, #9610 ) ;
#35017 = DIRECTION ( 'NONE',  ( 1.000000000000000000, 0.000000000000000000, -0.000000000000000000 ) ) ;
#35018 = EDGE_CURVE ( 'NONE', #25502, #29592, #35982, .T. ) ;
#35019 = VERTEX_POINT ( 'NONE', #61934 ) ;
#35020 = VECTOR ( 'NONE', #60418, 1000.000000000000000 ) ;
#35021 = VERTEX_POINT ( 'NONE', #51649 ) ;
#35022 = ORIENTED_EDGE ( 'NONE', *, *, #47465, .T. ) ;
#35023 = ORIENTED_EDGE ( 'NONE', *, *, #28819, .T. ) ;
#35024 = LINE ( 'NONE', #36364, #54648 ) ;
#35025 = DIRECTION ( 'NONE',  ( 0.000000000000000000, -0.8989688749565204473, -0.4380125133593880671 ) ) ;
#35026 = CARTESIAN_POINT ( 'NONE',  ( 0.3002738374340813143, -6.323236184341188171, 10.50101454678642021 ) ) ;
#35027 = DIRECTION ( 'NONE',  ( 0.000000000000000000, 0.000000000000000000, 1.000000000000000000 ) ) ;
#35028 = EDGE_CURVE ( 'NONE', #27429, #22010, #57404, .T. ) ;
#35029 = CARTESIAN_POINT ( 'NONE',  ( 0.3654063281920716388, -10.76363796011281337, -5.910280591919169879 ) ) ;
#35030 = CARTESIAN_POINT ( 'NONE',  ( 24.80306200676344019, -1.716780947678923308, -13.39180189726039316 ) ) ;
#35033 = EDGE_LOOP ( 'NONE', ( #42568, #41837, #31578, #55034 ) ) ;
#35032 = CARTESIAN_POINT ( 'NONE',  ( 47.00000000000000711, 4.705694406421931860E-17, -3.469127814946512892E-15 ) ) ;
#35031 = B_SPLINE_CURVE_WITH_KNOTS ( 'NONE', 3,
 ( #58072, #22149, #22486, #48751, #13168, #2210, #33449, #42090, #53742, #37444, #63045, #28448, #3203, #57755, #62372, #47759 ),
 .UNSPECIFIED., .F., .F.,
 ( 4, 3, 3, 3, 3, 4 ),
 ( 0.000000000000000000, 0.0003017745587525256807, 0.0006035491769808747162, 0.0009053241094668175492, 0.001207275924539396488, 0.001510325902531783112 ),
 .UNSPECIFIED. ) ;
#35034 = DIRECTION ( 'NONE',  ( 0.9947400562552481951, -0.1024315404614497965, 0.000000000000000000 ) ) ;
#35035 = EDGE_CURVE ( 'NONE', #8899, #3390, #54237, .T. ) ;
#35036 = EDGE_LOOP ( 'NONE', ( #44812, #3073, #19415, #1137 ) ) ;
#35037 = CARTESIAN_POINT ( 'NONE',  ( 5.516018279890452902, 0.001397286410094419331, 0.006629829924290476899 ) ) ;
#35038 = ORIENTED_EDGE ( 'NONE', *, *, #27876, .F. ) ;
#35039 = ORIENTED_EDGE ( 'NONE', *, *, #43068, .T. ) ;
#35040 = CARTESIAN_POINT ( 'NONE',  ( -22.29195009621226475, -0.8975732442595466543, 3.616122380634891886 ) ) ;
#35041 = ADVANCED_FACE ( 'NONE', ( #45651 ), #11384, .T. ) ;
#35042 = CARTESIAN_POINT ( 'NONE',  ( 6.263846918918718920, -28.63916073140924112, 12.80708683763934808 ) ) ;
#35043 = CYLINDRICAL_SURFACE ( 'NONE', #53508, 12.75000000000000178 ) ;
#35044 = CIRCLE ( 'NONE', #21299, 12.74999999999999822 ) ;
#35045 = VECTOR ( 'NONE', #45083, 1000.000000000000000 ) ;
#35046 = AXIS2_PLACEMENT_3D ( 'NONE', #35968, #36313, #46312 ) ;
#35048 = VECTOR ( 'NONE', #58712, 1000.000000000000000 ) ;
#35047 = CARTESIAN_POINT ( 'NONE',  ( 19.56743653832047514, -33.00000000000000000, 5.000000000000001776 ) ) ;
#35049 = DIRECTION ( 'NONE',  ( 0.000000000000000000, -0.01356324068817991828, 0.9999080150203990547 ) ) ;
#35050 = CARTESIAN_POINT ( 'NONE',  ( 2.251152103361937939, 5.930529991875680196, 4.812779263777095196 ) ) ;
#35052 = VERTEX_POINT ( 'NONE', #5106 ) ;
#35051 = ADVANCED_FACE ( 'NONE', ( #31655 ), #14884, .F. ) ;
#35053 = ORIENTED_EDGE ( 'NONE', *, *, #25662, .F. ) ;
#35054 = CARTESIAN_POINT ( 'NONE',  ( -35.00000000000000000, 7.817492529713985228, -9.348667969174325520 ) ) ;
#35055 = ORIENTED_EDGE ( 'NONE', *, *, #16528, .T. ) ;
#35056 = EDGE_CURVE ( 'NONE', #36640, #39147, #34033, .T. ) ;
#35057 = VERTEX_POINT ( 'NONE', #30676 ) ;
#35058 = LINE ( 'NONE', #51047, #15740 ) ;
#35059 = FACE_OUTER_BOUND ( 'NONE', #15776, .T. ) ;
#35060 = CARTESIAN_POINT ( 'NONE',  ( 18.74194725139314954, 1.365073709202341279, 11.92510536682598676 ) ) ;
#35062 = AXIS2_PLACEMENT_3D ( 'NONE', #8159, #58727, #2865 ) ;
#35061 = CARTESIAN_POINT ( 'NONE',  ( -22.27722019094931483, 1.249795790945223972, -3.463038365117172557 ) ) ;
#35063 = CARTESIAN_POINT ( 'NONE',  ( 3.152665057736164123, 5.461013642407259283, 5.761241965767907480 ) ) ;
#35064 = CARTESIAN_POINT ( 'NONE',  ( 2.177405672431368622, 1.276675186593990263, -11.12610351585605173 ) ) ;
#35065 = AXIS2_PLACEMENT_3D ( 'NONE', #21824, #52412, #17479 ) ;
#35066 = EDGE_LOOP ( 'NONE', ( #8025, #2084, #49285, #27591 ) ) ;
#35067 = ORIENTED_EDGE ( 'NONE', *, *, #31973, .F. ) ;
#35068 = CARTESIAN_POINT ( 'NONE',  ( -37.00000000000000711, 0.000000000000000000, 0.000000000000000000 ) ) ;
#35069 = CARTESIAN_POINT ( 'NONE',  ( 2.257661810676416803, 7.499185766072606008, -1.459225434025898327 ) ) ;
#35070 = AXIS2_PLACEMENT_3D ( 'NONE', #23891, #24517, #65714 ) ;
#35071 = CARTESIAN_POINT ( 'NONE',  ( -10.00000000000000178, 0.000000000000000000, 0.000000000000000000 ) ) ;
#35072 = EDGE_CURVE ( 'NONE', #35989, #54252, #60847, .T. ) ;
#35073 = CARTESIAN_POINT ( 'NONE',  ( 6.786836467603172274, -6.651659772632933176, 9.989835789978261715 ) ) ;
#35074 = CARTESIAN_POINT ( 'NONE',  ( 3.347841273039249721, -10.61118957148187825, 5.603807266321171987 ) ) ;
#35075 = CIRCLE ( 'NONE', #27645, 5.000000000000001776 ) ;
#35076 = DIRECTION ( 'NONE',  ( -1.000000000000000000, -0.000000000000000000, 0.000000000000000000 ) ) ;
#35077 = DIRECTION ( 'NONE',  ( 1.000000000000000000, -0.000000000000000000, -0.000000000000000000 ) ) ;
#35078 = CARTESIAN_POINT ( 'NONE',  ( 1.452237505248555660, -12.55261342181974626, -1.611965288198859314 ) ) ;
#35079 = CIRCLE ( 'NONE', #49979, 2.899999999999995026 ) ;
#35080 = ORIENTED_EDGE ( 'NONE', *, *, #5860, .T. ) ;
#35081 = CARTESIAN_POINT ( 'NONE',  ( 2.655192694322446201, -3.822392723569365991, -8.807900729504780202 ) ) ;
#35082 = DIRECTION ( 'NONE',  ( -1.000000000000000000, 0.000000000000000000, 0.000000000000000000 ) ) ;
#35083 = EDGE_CURVE ( 'NONE', #13688, #11147, #5385, .T. ) ;
#35084 = CARTESIAN_POINT ( 'NONE',  ( 2.903928887688265625, -6.032681461746786766, -6.365315087929473314 ) ) ;
#35085 = CIRCLE ( 'NONE', #59517, 12.75000000000000178 ) ;
#35086 = AXIS2_PLACEMENT_3D ( 'NONE', #31504, #57120, #52130 ) ;
#35087 = CIRCLE ( 'NONE', #55293, 4.999999999999998224 ) ;
#35088 = EDGE_CURVE ( 'NONE', #22685, #31409, #1094, .T. ) ;
#35089 = CARTESIAN_POINT ( 'NONE',  ( -1.327480008007509151E-11, -31.03649492335491544, -14.44372008463338908 ) ) ;
#35090 = DIRECTION ( 'NONE',  ( 0.000000000000000000, -0.01356324068817998940, 0.9999080150203990547 ) ) ;
#35091 = ORIENTED_EDGE ( 'NONE', *, *, #42781, .F. ) ;
#35092 = CARTESIAN_POINT ( 'NONE',  ( 2.247112776671467582, -2.501955819907531353, 7.214825360831409462 ) ) ;
#35093 = DIRECTION ( 'NONE',  ( 1.000000000000000000, 0.000000000000000000, 0.000000000000000000 ) ) ;
#35094 = CARTESIAN_POINT ( 'NONE',  ( 14.32183389819027930, -34.49933334076765590, -8.089813643623637418 ) ) ;
#35095 = ORIENTED_EDGE ( 'NONE', *, *, #19539, .F. ) ;
#35096 = CARTESIAN_POINT ( 'NONE',  ( 1.375507693217726590, -6.813306181534734662, 10.61839108744977445 ) ) ;
#35097 = CARTESIAN_POINT ( 'NONE',  ( -28.25663979408810889, -12.49293946602661443, -5.125494512094520339 ) ) ;
#35098 = DIRECTION ( 'NONE',  ( 0.000000000000000000, 0.01356324068817992175, -0.9999080150203990547 ) ) ;
#35099 = EDGE_CURVE ( 'NONE', #44602, #49587, #30824, .T. ) ;
#35101 = ORIENTED_EDGE ( 'NONE', *, *, #34026, .F. ) ;
#35100 = FACE_OUTER_BOUND ( 'NONE', #11744, .T. ) ;
#35102 = DIRECTION ( 'NONE',  ( 0.000000000000000000, 0.6478160128811893959, -0.7617968321374922747 ) ) ;
#35103 = VECTOR ( 'NONE', #12558, 1000.000000000000000 ) ;
#35104 = DIRECTION ( 'NONE',  ( 0.000000000000000000, -0.3807014730195286134, 0.9246979985058695339 ) ) ;
#35105 = ORIENTED_EDGE ( 'NONE', *, *, #54743, .T. ) ;
#35106 = AXIS2_PLACEMENT_3D ( 'NONE', #25128, #10155, #25447 ) ;
#35107 = CARTESIAN_POINT ( 'NONE',  ( 0.3278977287071211388, 7.693417476735527671, 9.554671284920326357 ) ) ;
#35108 = AXIS2_PLACEMENT_3D ( 'NONE', #19051, #49647, #24696 ) ;
#35109 = CARTESIAN_POINT ( 'NONE',  ( -27.09861164373112885, 1.303360234155700015, 1.936722219469616091 ) ) ;
#35111 = CARTESIAN_POINT ( 'NONE',  ( 0.3675815128205894289, -9.574637318041910206, -7.689697408877373519 ) ) ;
#35110 =( BOUNDED_SURFACE ( )  B_SPLINE_SURFACE ( 3, 1, ( 
 ( #41368, #11137 ),
 ( #56709, #10144 ),
 ( #36046, #14774 ),
 ( #5506, #9805 ) ),
 .UNSPECIFIED., .F., .F., .F. ) 
 B_SPLINE_SURFACE_WITH_KNOTS ( ( 4, 4 ),
 ( 2, 2 ),
 ( 0.000000000000000000, 1.000000000000000000 ),
 ( 0.000000000000000000, 1.000000000000000000 ),
 .UNSPECIFIED. ) 
 GEOMETRIC_REPRESENTATION_ITEM ( )  RATIONAL_B_SPLINE_SURFACE ( (
 ( 1.000000000000000000, 1.000000000000000000),
 ( 0.6933888150995267674, 0.9895912004443193632),
 ( 0.6933888150995267674, 0.9895912004443193632),
 ( 1.000000000000000000, 1.000000000000000000) ) ) 
 REPRESENTATION_ITEM ( '' )  SURFACE ( )  );
#35112 = CARTESIAN_POINT ( 'NONE',  ( 1.462291587751302302, -1.569662666436036469, -12.54737685278425197 ) ) ;
#35113 = CARTESIAN_POINT ( 'NONE',  ( -22.30625920655495165, 3.687109008463850479, 0.8854385781085043483 ) ) ;
#35114 = DIRECTION ( 'NONE',  ( 0.000000000000000000, 0.01356324068817998073, -0.9999080150203990547 ) ) ;
#35115 = CARTESIAN_POINT ( 'NONE',  ( 2.305787727787084407, 1.164987321564833422, -7.566723232958059597 ) ) ;
#35116 = ORIENTED_EDGE ( 'NONE', *, *, #21422, .F. ) ;
#35117 = DIRECTION ( 'NONE',  ( 0.000000000000000000, 0.01356324068817998940, -0.9999080150203990547 ) ) ;
#35118 = CIRCLE ( 'NONE', #44665, 5.000000000000000888 ) ;
#35119 = ORIENTED_EDGE ( 'NONE', *, *, #20482, .T. ) ;
#35120 = ADVANCED_FACE ( 'NONE', ( #41455 ), #11863, .T. ) ;
#35121 = B_SPLINE_CURVE_WITH_KNOTS ( 'NONE', 3,
 ( #53706, #8140, #28411, #22443, #43708, #33724, #38728, #42708, #54021, #49055 ),
 .UNSPECIFIED., .F., .F.,
 ( 4, 2, 2, 2, 4 ),
 ( 0.005719258168536343369, 0.006386639034606452631, 0.007054019900676561892, 0.007721400766746672889, 0.008388781632816783018 ),
 .UNSPECIFIED. ) ;
#35122 = CARTESIAN_POINT ( 'NONE',  ( 0.2759803524722169721, 11.44482553421631010, 4.367180139677351747 ) ) ;
#35123 = EDGE_CURVE ( 'NONE', #51803, #61423, #15856, .T. ) ;
#35124 = FACE_OUTER_BOUND ( 'NONE', #55946, .T. ) ;
#35125 = ORIENTED_EDGE ( 'NONE', *, *, #10484, .T. ) ;
#35127 = CARTESIAN_POINT ( 'NONE',  ( 2.000000000000001776, 4.376687952327412034, -5.220963330856592144 ) ) ;
#35126 = AXIS2_PLACEMENT_3D ( 'NONE', #53588, #63524, #12008 ) ;
#35128 = CARTESIAN_POINT ( 'NONE',  ( 11.52778293799294396, 11.81657713697700629, -2.095136543809601903 ) ) ;
#35129 = DIRECTION ( 'NONE',  ( 0.000000000000000000, 0.01356324068817992175, -0.9999080150203990547 ) ) ;
#35130 = VERTEX_POINT ( 'NONE', #11537 ) ;
#35131 = EDGE_LOOP ( 'NONE', ( #16261, #61535, #10307, #6730 ) ) ;
#35132 = ADVANCED_FACE ( 'NONE', ( #5601 ), #17193, .T. ) ;
#35133 = FACE_OUTER_BOUND ( 'NONE', #25989, .T. ) ;
#35134 = CIRCLE ( 'NONE', #42587, 12.18649999999999878 ) ;
#35135 = ORIENTED_EDGE ( 'NONE', *, *, #24953, .F. ) ;
#35136 = DIRECTION ( 'NONE',  ( -1.000000000000000000, 0.000000000000000000, 0.000000000000000000 ) ) ;
#35137 = VERTEX_POINT ( 'NONE', #22171 ) ;
#35138 = CARTESIAN_POINT ( 'NONE',  ( -27.08579483061202708, 2.287150433979704633, -0.2015567301747461515 ) ) ;
#35139 = CARTESIAN_POINT ( 'NONE',  ( -29.67854887312627810, -0.9836058970513458233, 11.96157915316133113 ) ) ;
#35140 = AXIS2_PLACEMENT_3D ( 'NONE', #51081, #41395, #21469 ) ;
#35141 = CIRCLE ( 'NONE', #61737, 12.75000000000000178 ) ;
#35142 = CARTESIAN_POINT ( 'NONE',  ( 3.047904605210424389, -4.313929735713912805, 6.622084192655478319 ) ) ;
#35143 = CARTESIAN_POINT ( 'NONE',  ( 0.2648978790185584908, -10.67083876753496341, 6.008231198268946471 ) ) ;
#35144 = VECTOR ( 'NONE', #58111, 1000.000000000000000 ) ;
#35145 = DIRECTION ( 'NONE',  ( -1.000000000000000000, 0.000000000000000000, 0.000000000000000000 ) ) ;
#35146 = ORIENTED_EDGE ( 'NONE', *, *, #46062, .T. ) ;
#35147 = CARTESIAN_POINT ( 'NONE',  ( 2.288423627607476529, 7.648392725410192661, -0.1612945702822020377 ) ) ;
#35148 = CARTESIAN_POINT ( 'NONE',  ( 22.48401433917421244, 10.66787085122025047, -5.506576138129045006 ) ) ;
#35149 = DIRECTION ( 'NONE',  ( 0.000000000000000000, -0.9718671068226484300, 0.2355298848897412201 ) ) ;
#35150 = CARTESIAN_POINT ( 'NONE',  ( 12.45309242253974880, 13.08615109455304726, -3.321667012947705722 ) ) ;
#35151 = CARTESIAN_POINT ( 'NONE',  ( 37.00000000000000711, 5.273331777780336793, -10.49591321039682690 ) ) ;
#35152 = CYLINDRICAL_SURFACE ( 'NONE', #22530, 5.000000000000000888 ) ;
#35153 = DIRECTION ( 'NONE',  ( 0.000000000000000000, -0.01356324068817999114, 0.9999080150203989437 ) ) ;
#35154 = DIRECTION ( 'NONE',  ( 0.000000000000000000, 0.000000000000000000, -1.000000000000000000 ) ) ;
#35155 = VECTOR ( 'NONE', #34423, 1000.000000000000000 ) ;
#35156 = AXIS2_PLACEMENT_3D ( 'NONE', #19684, #24990, #65522 ) ;
#35157 = EDGE_CURVE ( 'NONE', #65319, #53863, #37468, .T. ) ;
#35158 = ORIENTED_EDGE ( 'NONE', *, *, #63713, .T. ) ;
#35159 = CARTESIAN_POINT ( 'NONE',  ( 0.2647959493198550618, 0.1469673141001566208, 12.24513905663510549 ) ) ;
#35160 = AXIS2_PLACEMENT_3D ( 'NONE', #55049, #9476, #29763 ) ;
#35161 = EDGE_CURVE ( 'NONE', #21899, #16286, #36491, .T. ) ;
#35162 = ORIENTED_EDGE ( 'NONE', *, *, #1087, .T. ) ;
#35163 = CARTESIAN_POINT ( 'NONE',  ( 35.00000000000000000, -12.08216339958901564, -1.591260454995201412 ) ) ;
#35164 = CARTESIAN_POINT ( 'NONE',  ( 0.2648978790185602672, -12.24533305150758267, 0.1321385342561976484 ) ) ;
#35165 = CARTESIAN_POINT ( 'NONE',  ( -36.00000000000000711, -12.16893194857547655, -3.805206332242601075 ) ) ;
#35166 = AXIS2_PLACEMENT_3D ( 'NONE', #24349, #13394, #33678 ) ;
#35167 = CARTESIAN_POINT ( 'NONE',  ( 35.00000000000000000, 4.705694406421931860E-17, -3.469127814946512892E-15 ) ) ;
#35168 = CARTESIAN_POINT ( 'NONE',  ( 2.276905613633474434, 2.469846004795502648, -7.236369456722756333 ) ) ;
#35169 = VERTEX_POINT ( 'NONE', #31496 ) ;
#35170 = CARTESIAN_POINT ( 'NONE',  ( 5.515188684475870851, -0.005320786921497274412, 0.0005703990286342659364 ) ) ;
#35172 = VECTOR ( 'NONE', #33464, 1000.000000000000227 ) ;
#35171 = CARTESIAN_POINT ( 'NONE',  ( 2.524535260912004198, 2.434550409953288863, -7.335347545455379148 ) ) ;
#35173 = ADVANCED_FACE ( 'NONE', ( #25871 ), #12030, .F. ) ;
#35174 = CARTESIAN_POINT ( 'NONE',  ( -37.00000000000000711, -11.59605747147783106, -5.300372733891765442 ) ) ;
#35175 = DIRECTION ( 'NONE',  ( 0.000000000000000000, 0.01356324068817998940, -0.9999080150203990547 ) ) ;
#35176 = FACE_OUTER_BOUND ( 'NONE', #19031, .T. ) ;
#35177 = CIRCLE ( 'NONE', #25658, 12.75000000000000178 ) ;
#35178 = DIRECTION ( 'NONE',  ( 0.000000000000000000, 0.01356324068817991828, -0.9999080150203990547 ) ) ;
#35179 = VERTEX_POINT ( 'NONE', #61416 ) ;
#35180 = CARTESIAN_POINT ( 'NONE',  ( 5.530133899448235191, 0.003876417824003331770, 0.01550764871776277344 ) ) ;
#35181 = ORIENTED_EDGE ( 'NONE', *, *, #59896, .T. ) ;
#35182 = VECTOR ( 'NONE', #41172, 1000.000000000000000 ) ;
#35183 = CARTESIAN_POINT ( 'NONE',  ( 0.2652384770603652409, 12.24598129987882444, 0.06606665821602195066 ) ) ;
#35185 = EDGE_CURVE ( 'NONE', #65463, #57020, #26506, .T. ) ;
#35184 = CARTESIAN_POINT ( 'NONE',  ( -23.41523303002441736, -4.252418708693351590, 1.997501275420731748 ) ) ;
#35186 = ADVANCED_FACE ( 'NONE', ( #5935, #1256 ), #21536, .F. ) ;
#35187 = LINE ( 'NONE', #60468, #32034 ) ;
#35188 = EDGE_CURVE ( 'NONE', #9403, #60864, #62397, .T. ) ;
#35189 = DIRECTION ( 'NONE',  ( 1.000000000000000000, 0.000000000000000000, 0.000000000000000000 ) ) ;
#35190 = AXIS2_PLACEMENT_3D ( 'NONE', #6964, #63448, #57181 ) ;
#35191 = AXIS2_PLACEMENT_3D ( 'NONE', #7818, #2516, #22787 ) ;
#35192 = VERTEX_POINT ( 'NONE', #6573 ) ;
#35193 = ORIENTED_EDGE ( 'NONE', *, *, #50249, .T. ) ;
#35194 = B_SPLINE_CURVE_WITH_KNOTS ( 'NONE', 3,
 ( #59071, #39081, #29749, #24791, #13479, #45070, #23823, #48756, #55035, #44084, #64356, #13175, #33762, #44721, #65005, #4176, #43753, #64034, #49430 ),
 .UNSPECIFIED., .F., .F.,
 ( 4, 3, 3, 3, 3, 3, 4 ),
 ( 6.447129612864634281E-18, 2.825908398831150243E-05, 4.208813692483755799E-05, 5.591713746943746520E-05, 6.279584083231628730E-05, 9.105792820296214286E-05, 0.0001153131102488863264 ),
 .UNSPECIFIED. ) ;
#35195 = CARTESIAN_POINT ( 'NONE',  ( 2.241352910868908310, 4.843133558968128582, 5.901537464758471074 ) ) ;
#35196 = EDGE_LOOP ( 'NONE', ( #29062, #3839, #47494, #15506 ) ) ;
#35197 = DIRECTION ( 'NONE',  ( -1.000000000000000000, 0.000000000000000000, 0.000000000000000000 ) ) ;
#35198 = DIRECTION ( 'NONE',  ( 0.000000000000000000, -0.1740410799127470598, -0.9847383929261643853 ) ) ;
#35199 = DIRECTION ( 'NONE',  ( 0.000000000000000000, 0.000000000000000000, -1.000000000000000000 ) ) ;
#35200 = CARTESIAN_POINT ( 'NONE',  ( 0.2833330754217401881, 12.25052326018167470, 0.2021515668286114065 ) ) ;
#35201 = CARTESIAN_POINT ( 'NONE',  ( 37.00000000000000711, -10.39746860227895731, -7.379373053628834889 ) ) ;
#35202 = B_SPLINE_CURVE_WITH_KNOTS ( 'NONE', 3,
 ( #28651, #33647, #17036, #13360, #8376, #57627, #62914, #52945, #47966, #2422, #22700, #58268, #12689, #53282, #7726, #28015, #48316, #2767 ),
 .UNSPECIFIED., .F., .F.,
 ( 4, 2, 2, 2, 2, 2, 2, 2, 4 ),
 ( 0.000000000000000000, 0.001109628529027648818, 0.002219257058055297636, 0.003328885587082946670, 0.004438514116110595271, 0.005548142645138243872, 0.006657771174165893341, 0.007767399703193541942, 0.008877028232221188808 ),
 .UNSPECIFIED. ) ;
#35203 = DIRECTION ( 'NONE',  ( -1.000000000000000000, -0.000000000000000000, 0.000000000000000000 ) ) ;
#35204 = CARTESIAN_POINT ( 'NONE',  ( -37.00000000000000711, -2.250029553613845934, 12.54989509947650284 ) ) ;
#35205 = ORIENTED_EDGE ( 'NONE', *, *, #38568, .F. ) ;
#35207 = ORIENTED_EDGE ( 'NONE', *, *, #51389, .F. ) ;
#35206 = CARTESIAN_POINT ( 'NONE',  ( 1.198791140418999035, -11.12379938352691156, 5.826488554585893986 ) ) ;
#35208 = VERTEX_POINT ( 'NONE', #10892 ) ;
#35209 = CARTESIAN_POINT ( 'NONE',  ( -35.04709527796842394, -0.01012471662513968196, -0.007095259204994638913 ) ) ;
#35210 = EDGE_CURVE ( 'NONE', #6781, #36007, #16547, .T. ) ;
#35211 = AXIS2_PLACEMENT_3D ( 'NONE', #65448, #8961, #49540 ) ;
#35212 = FACE_OUTER_BOUND ( 'NONE', #47469, .T. ) ;
#35213 = ORIENTED_EDGE ( 'NONE', *, *, #64943, .F. ) ;
#35214 = VECTOR ( 'NONE', #6907, 1000.000000000000000 ) ;
#35215 = ADVANCED_FACE ( 'NONE', ( #57778 ), #36817, .T. ) ;
#35216 = LINE ( 'NONE', #9964, #30012 ) ;
#35217 = ORIENTED_EDGE ( 'NONE', *, *, #18269, .T. ) ;
#35218 = CARTESIAN_POINT ( 'NONE',  ( -2.952869152607106251, -11.39722960915210592, 3.755417052241485365 ) ) ;
#35219 = CARTESIAN_POINT ( 'NONE',  ( 35.00000000000000000, 4.705694406421931860E-17, -3.469127814946512892E-15 ) ) ;
#35220 = DIRECTION ( 'NONE',  ( 1.000000000000000000, 0.000000000000000000, -0.000000000000000000 ) ) ;
#35221 = CARTESIAN_POINT ( 'NONE',  ( 6.812204945636112896, -4.138731716409435712, 11.26369831714195335 ) ) ;
#35222 = ORIENTED_EDGE ( 'NONE', *, *, #32199, .T. ) ;
#35223 = VECTOR ( 'NONE', #15746, 1000.000000000000000 ) ;
#35224 = ORIENTED_EDGE ( 'NONE', *, *, #24929, .T. ) ;
#35225 = DIRECTION ( 'NONE',  ( 0.000000000000000000, 0.8276889981568877896, 0.5611870653623862726 ) ) ;
#35226 = ORIENTED_EDGE ( 'NONE', *, *, #33640, .T. ) ;
#35227 = CARTESIAN_POINT ( 'NONE',  ( 0.3053067050349176359, 11.59706307017088811, -3.975408458060398331 ) ) ;
#35228 = ORIENTED_EDGE ( 'NONE', *, *, #52240, .F. ) ;
#35229 = VECTOR ( 'NONE', #22086, 1000.000000000000000 ) ;
#35230 = VERTEX_POINT ( 'NONE', #47464 ) ;
#35231 = ORIENTED_EDGE ( 'NONE', *, *, #48735, .T. ) ;
#35232 = CARTESIAN_POINT ( 'NONE',  ( 2.889800649504073782, 5.267262008933668582, 3.118861721612583793 ) ) ;
#35233 = CARTESIAN_POINT ( 'NONE',  ( -1.994964832131321808, -25.76766306558318220, 15.60102351411471666 ) ) ;
#35234 = DIRECTION ( 'NONE',  ( 1.000000000000000000, -0.000000000000000000, 0.000000000000000000 ) ) ;
#35235 = DIRECTION ( 'NONE',  ( 0.000000000000000000, 0.000000000000000000, -1.000000000000000000 ) ) ;
#35236 = ORIENTED_EDGE ( 'NONE', *, *, #36409, .F. ) ;
#35237 = EDGE_CURVE ( 'NONE', #32084, #18779, #37037, .T. ) ;
#35238 = LINE ( 'NONE', #29593, #46019 ) ;
#35239 = VECTOR ( 'NONE', #21442, 1000.000000000000000 ) ;
#35240 = ORIENTED_EDGE ( 'NONE', *, *, #53758, .T. ) ;
#35241 = DIRECTION ( 'NONE',  ( 0.000000000000000000, -0.9346839223284501008, 0.3554799084909069928 ) ) ;
#35242 = CARTESIAN_POINT ( 'NONE',  ( 0.000000000000000000, -6.250523986463956128, -3.007653927006670003 ) ) ;
#35243 = VERTEX_POINT ( 'NONE', #32783 ) ;
#35244 = CARTESIAN_POINT ( 'NONE',  ( 0.9232058338315048962, 6.559496812049809833, -10.60677148422237259 ) ) ;
#35245 = CARTESIAN_POINT ( 'NONE',  ( 27.47563550582765757, 10.97366218211726974, 4.866891853559282666 ) ) ;
#35246 = CARTESIAN_POINT ( 'NONE',  ( -28.66013792860432119, 1.826836065344828564, -0.1826938850344149434 ) ) ;
#35247 = AXIS2_PLACEMENT_3D ( 'NONE', #6852, #47090, #17476 ) ;
#35248 = VECTOR ( 'NONE', #7514, 1000.000000000000000 ) ;
#35249 = CIRCLE ( 'NONE', #28854, 6.936499999999989896 ) ;
#35250 = ORIENTED_EDGE ( 'NONE', *, *, #55751, .T. ) ;
#35251 = FACE_OUTER_BOUND ( 'NONE', #35036, .T. ) ;
#35252 = EDGE_CURVE ( 'NONE', #659, #11368, #33777, .T. ) ;
#35253 = VERTEX_POINT ( 'NONE', #48454 ) ;
#35254 = CARTESIAN_POINT ( 'NONE',  ( 2.000000000000001776, -6.606214214351046721, -2.114938770769991372 ) ) ;
#35255 = CARTESIAN_POINT ( 'NONE',  ( 0.6473888112830261665, 9.687359867659798951, 7.698027285532502262 ) ) ;
#35256 = CARTESIAN_POINT ( 'NONE',  ( -17.77323790556441452, -29.67638950762373895, 8.606028548248493948 ) ) ;
#35257 = DIRECTION ( 'NONE',  ( 0.000000000000000000, -0.9105187689795999351, 0.4134677391718417638 ) ) ;
#35258 = CARTESIAN_POINT ( 'NONE',  ( 12.36235005266927978, 8.714858184812433350, -8.258156698578600796 ) ) ;
#35259 = ORIENTED_EDGE ( 'NONE', *, *, #22119, .T. ) ;
#35260 = B_SPLINE_CURVE_WITH_KNOTS ( 'NONE', 3,
 ( #14406, #44660, #24735, #15064, #60625, #113, #9104, #29074 ),
 .UNSPECIFIED., .F., .F.,
 ( 4, 2, 2, 4 ),
 ( 0.009775493497823107072, 0.01050469463799914675, 0.01123389577817518817, 0.01269229805852726926 ),
 .UNSPECIFIED. ) ;
#35261 = CARTESIAN_POINT ( 'NONE',  ( 37.00000000000000711, 4.705694406421931860E-17, -3.469127814946512892E-15 ) ) ;
#35262 = LINE ( 'NONE', #23, #22738 ) ;
#35263 = CARTESIAN_POINT ( 'NONE',  ( 2.406456491627547933, -2.427896847125293078, -10.14681500355714228 ) ) ;
#35264 = CARTESIAN_POINT ( 'NONE',  ( 2.931247277082678071, 3.607110715259749689, 6.988361004535447840 ) ) ;
#35265 = CIRCLE ( 'NONE', #63943, 12.75000000000000178 ) ;
#35266 = AXIS2_PLACEMENT_3D ( 'NONE', #44943, #55245, #65530 ) ;
#35267 = EDGE_CURVE ( 'NONE', #50238, #7848, #28725, .T. ) ;
#35268 = DIRECTION ( 'NONE',  ( -1.000000000000000000, -0.000000000000000000, -0.000000000000000000 ) ) ;
#35269 = AXIS2_PLACEMENT_3D ( 'NONE', #39971, #55266, #20345 ) ;
#35270 = CARTESIAN_POINT ( 'NONE',  ( -22.31328051695926007, 3.685074213229321494, 0.8849444482787824917 ) ) ;
#35272 = ADVANCED_FACE ( 'NONE', ( #22851 ), #27481, .T. ) ;
#35271 = CARTESIAN_POINT ( 'NONE',  ( -35.04643116707788408, -0.009112266603810564858, 0.008094444324481878117 ) ) ;
#35273 = CARTESIAN_POINT ( 'NONE',  ( 2.177405672432016104, -1.276675186593669187, 11.12610351585390411 ) ) ;
#35274 = FACE_OUTER_BOUND ( 'NONE', #60103, .T. ) ;
#35275 = EDGE_CURVE ( 'NONE', #51572, #6221, #43103, .T. ) ;
#35276 = EDGE_LOOP ( 'NONE', ( #43568, #58657, #5841, #47748 ) ) ;
#35277 = CARTESIAN_POINT ( 'NONE',  ( -27.10422407540562162, -1.306850885988421362, -1.954655484501059970 ) ) ;
#35278 = VECTOR ( 'NONE', #1672, 1000.000000000000000 ) ;
#35279 = EDGE_LOOP ( 'NONE', ( #38146, #51171, #65503, #18792 ) ) ;
#35280 = DIRECTION ( 'NONE',  ( 0.000000000000000000, -0.5472293298355157543, 0.8369827122275419473 ) ) ;
#35281 = FACE_OUTER_BOUND ( 'NONE', #11796, .T. ) ;
#35282 = CARTESIAN_POINT ( 'NONE',  ( 0.3665391374699464300, -0.2638605131388023217, 12.27992639892678106 ) ) ;
#35283 = VERTEX_POINT ( 'NONE', #63069 ) ;
#35284 = VECTOR ( 'NONE', #3358, 1000.000000000000000 ) ;
#35285 = VERTEX_POINT ( 'NONE', #53763 ) ;
#35286 = ORIENTED_EDGE ( 'NONE', *, *, #56007, .F. ) ;
#35287 = CARTESIAN_POINT ( 'NONE',  ( 28.68872621665320821, -10.58213401676968246, 5.662857775278662409 ) ) ;
#35288 = EDGE_CURVE ( 'NONE', #33595, #44052, #43479, .T. ) ;
#35289 = VECTOR ( 'NONE', #58871, 1000.000000000000000 ) ;
#35291 = CIRCLE ( 'NONE', #10860, 5.000000000000000000 ) ;
#35290 = CARTESIAN_POINT ( 'NONE',  ( -20.79170840334646542, -11.34110549087206898, -3.921648409140116698 ) ) ;
#35292 = ORIENTED_EDGE ( 'NONE', *, *, #6802, .T. ) ;
#35293 = LINE ( 'NONE', #49950, #58097 ) ;
#35294 = CARTESIAN_POINT ( 'NONE',  ( -17.83419946441818027, -9.720786832536937538, 7.036071585506806336 ) ) ;
#35295 = ORIENTED_EDGE ( 'NONE', *, *, #51730, .T. ) ;
#35296 = CARTESIAN_POINT ( 'NONE',  ( -22.31328051695926007, 0.2528478350594092761, 3.781397440874584071 ) ) ;
#35297 = CARTESIAN_POINT ( 'NONE',  ( -4.228765754682466849, -26.75056327283501290, -15.92880586833495649 ) ) ;
#35298 = CYLINDRICAL_SURFACE ( 'NONE', #58989, 4.999999999999999112 ) ;
#35300 = ORIENTED_EDGE ( 'NONE', *, *, #47085, .T. ) ;
#35299 = DIRECTION ( 'NONE',  ( 0.2475719085175094591, 6.192417051524157726E-18, -0.9688695217174487784 ) ) ;
#35301 = CARTESIAN_POINT ( 'NONE',  ( -25.54417658651491863, 7.498517398407837931, 11.22596262356930197 ) ) ;
#35302 = VERTEX_POINT ( 'NONE', #12846 ) ;
#35303 = FACE_OUTER_BOUND ( 'NONE', #64987, .T. ) ;
#35304 = ORIENTED_EDGE ( 'NONE', *, *, #59311, .T. ) ;
#35305 = CARTESIAN_POINT ( 'NONE',  ( 2.000000000000001776, 4.444115772890121718, 5.163689623839328391 ) ) ;
#35306 = FACE_OUTER_BOUND ( 'NONE', #46350, .T. ) ;
#35307 = CARTESIAN_POINT ( 'NONE',  ( -2.195494320936263843, -31.13300424730153892, 14.33890400575774215 ) ) ;
#35308 = CARTESIAN_POINT ( 'NONE',  ( 1.719304012340734378, -7.017415949613340587, -10.62216384465587282 ) ) ;
#35309 = EDGE_CURVE ( 'NONE', #38796, #918, #53440, .T. ) ;
#35310 = CIRCLE ( 'NONE', #63985, 12.74999999999999822 ) ;
#35311 = CARTESIAN_POINT ( 'NONE',  ( -22.39032720737626292, -2.936932155721161397, -2.746561316202171810 ) ) ;
#35312 = CARTESIAN_POINT ( 'NONE',  ( 0.2801149460245160872, -12.24954625471155722, 0.1962575296604981423 ) ) ;
#35313 = FACE_OUTER_BOUND ( 'NONE', #42240, .T. ) ;
#35314 = CARTESIAN_POINT ( 'NONE',  ( -27.08419642509983305, 2.239682169453941274, -0.4837273216074968185 ) ) ;
#35315 = FACE_OUTER_BOUND ( 'NONE', #35827, .T. ) ;
#35317 = VERTEX_POINT ( 'NONE', #47783 ) ;
#35316 = CARTESIAN_POINT ( 'NONE',  ( -7.489022030332961322, -8.034049540753116503, -10.84914964302385521 ) ) ;
#35318 = CARTESIAN_POINT ( 'NONE',  ( -28.66013792860432119, 1.071635578228296470, 1.490739498621012071 ) ) ;
#35319 = ORIENTED_EDGE ( 'NONE', *, *, #41410, .T. ) ;
#35320 = DIRECTION ( 'NONE',  ( 0.000000000000000000, 0.000000000000000000, -1.000000000000000000 ) ) ;
#35321 = VERTEX_POINT ( 'NONE', #7885 ) ;
#35322 = AXIS2_PLACEMENT_3D ( 'NONE', #12256, #32519, #61478 ) ;
#35323 = VERTEX_POINT ( 'NONE', #23161 ) ;
#35324 = CARTESIAN_POINT ( 'NONE',  ( 37.00000000000000711, 11.59095880812004964, -1.903127969211395598 ) ) ;
#35325 = DIRECTION ( 'NONE',  ( 1.000000000000000000, 0.000000000000000000, 0.000000000000000000 ) ) ;
#35326 = DIRECTION ( 'NONE',  ( 1.000000000000000000, 0.000000000000000000, 0.000000000000000000 ) ) ;
#35327 = DIRECTION ( 'NONE',  ( -1.000000000000000000, 0.000000000000000000, 0.000000000000000000 ) ) ;
#35328 = CARTESIAN_POINT ( 'NONE',  ( 2.256373768221671128, 7.223078030709081609, 2.487510024223419158 ) ) ;
#35329 = LINE ( 'NONE', #54968, #12143 ) ;
#35330 = EDGE_CURVE ( 'NONE', #52081, #1502, #63481, .T. ) ;
#35331 =( BOUNDED_CURVE ( )  B_SPLINE_CURVE ( 3, ( #17822, #47755, #1876, #63356 ),
 .UNSPECIFIED., .F., .F. ) 
 B_SPLINE_CURVE_WITH_KNOTS ( ( 4, 4 ),
 ( 4.456175814406320157, 4.486258350949901441 ),
 .UNSPECIFIED. ) 
 CURVE ( )  GEOMETRIC_REPRESENTATION_ITEM ( )  RATIONAL_B_SPLINE_CURVE ( ( 1.000000000000000000, 0.9999245881713708650, 0.9999245881713708650, 1.000000000000000000 ) ) 
 REPRESENTATION_ITEM ( '' )  );
#35332 = EDGE_LOOP ( 'NONE', ( #48311, #19121, #15113, #59535 ) ) ;
#35333 = DIRECTION ( 'NONE',  ( 1.836970198721029688E-16, -1.000000000000000000, 0.000000000000000000 ) ) ;
#35334 = CARTESIAN_POINT ( 'NONE',  ( 37.00000000000000711, 4.705694406421931860E-17, -3.469127814946512892E-15 ) ) ;
#35335 = ADVANCED_FACE ( 'NONE', ( #43770 ), #43424, .T. ) ;
#35336 = CARTESIAN_POINT ( 'NONE',  ( 0.5572780756279746006, 12.09922454589784380, 2.443667122521326007 ) ) ;
#35337 = EDGE_LOOP ( 'NONE', ( #18620, #26338, #48106, #14347 ) ) ;
#35338 = VECTOR ( 'NONE', #17648, 1000.000000000000000 ) ;
#35339 = AXIS2_PLACEMENT_3D ( 'NONE', #29491, #18584, #54792 ) ;
#35340 = AXIS2_PLACEMENT_3D ( 'NONE', #60373, #29455, #39773 ) ;
#35341 = AXIS2_PLACEMENT_3D ( 'NONE', #11013, #35615, #20324 ) ;
#35342 = EDGE_CURVE ( 'NONE', #15192, #37781, #12507, .T. ) ;
#35343 = LINE ( 'NONE', #60623, #54320 ) ;
#35344 = CIRCLE ( 'NONE', #42801, 12.18649999999999700 ) ;
#35345 = DIRECTION ( 'NONE',  ( 0.000000000000000000, 0.4935949184179262983, -0.8696919319575183716 ) ) ;
#35346 = CARTESIAN_POINT ( 'NONE',  ( 35.00000000000000000, -3.704519465651390675, -11.60979404548633731 ) ) ;
#35347 = VERTEX_POINT ( 'NONE', #12195 ) ;
#35349 = EDGE_CURVE ( 'NONE', #45593, #21947, #26636, .T. ) ;
#35348 = CARTESIAN_POINT ( 'NONE',  ( 0.2648978790185602672, 1.996248716311790128, -12.08224454301446826 ) ) ;
#35350 = CARTESIAN_POINT ( 'NONE',  ( 16.78995969943036570, -34.48221411999240615, 5.258039666742008400 ) ) ;
#35351 = CARTESIAN_POINT ( 'NONE',  ( 3.878049410135225639, 5.417590671930183177, 10.70984159994429596 ) ) ;
#35352 = VECTOR ( 'NONE', #20653, 1000.000000000000000 ) ;
#35353 = AXIS2_PLACEMENT_3D ( 'NONE', #4229, #3914, #30150 ) ;
#35354 = EDGE_CURVE ( 'NONE', #33621, #16066, #45721, .T. ) ;
#35355 = DIRECTION ( 'NONE',  ( 0.000000000000000000, 0.000000000000000000, -1.000000000000000000 ) ) ;
#35356 = DIRECTION ( 'NONE',  ( -1.000000000000000000, 0.000000000000000000, 0.000000000000000000 ) ) ;
#35357 = ORIENTED_EDGE ( 'NONE', *, *, #62017, .F. ) ;
#35358 = DIRECTION ( 'NONE',  ( 0.000000000000000000, 0.000000000000000000, -1.000000000000000000 ) ) ;
#35359 = CARTESIAN_POINT ( 'NONE',  ( 3.426384734005718524, 5.858157115608569221, -10.47507226477059383 ) ) ;
#35360 = AXIS2_PLACEMENT_3D ( 'NONE', #17004, #16682, #22312 ) ;
#35361 = DIRECTION ( 'NONE',  ( 0.000000000000000000, 0.9796553971857748788, 0.2006870767258854826 ) ) ;
#35362 = ORIENTED_EDGE ( 'NONE', *, *, #1281, .F. ) ;
#35363 = CARTESIAN_POINT ( 'NONE',  ( 9.958180664929905390, 1.092159088654170329, 13.45683414571523429 ) ) ;
#35364 = CARTESIAN_POINT ( 'NONE',  ( 0.000000000000000000, -7.248432822490231686, -1.926193556693109654 ) ) ;
#35365 = ORIENTED_EDGE ( 'NONE', *, *, #23302, .F. ) ;
#35366 = VERTEX_POINT ( 'NONE', #52773 ) ;
#35367 = EDGE_LOOP ( 'NONE', ( #31106, #63795, #31842, #44454 ) ) ;
#35368 = CIRCLE ( 'NONE', #33247, 2.899999999999994582 ) ;
#35369 = ORIENTED_EDGE ( 'NONE', *, *, #28100, .F. ) ;
#35370 = CARTESIAN_POINT ( 'NONE',  ( 37.00000000000000711, 4.705694406421931860E-17, -3.469127814946512892E-15 ) ) ;
#35371 = CARTESIAN_POINT ( 'NONE',  ( 27.62838931380291996, 25.00000000000000000, -3.066727421130092779 ) ) ;
#35372 = DIRECTION ( 'NONE',  ( 1.000000000000000000, 0.000000000000000000, 0.000000000000000000 ) ) ;
#35373 = CARTESIAN_POINT ( 'NONE',  ( -22.71097035706202760, -2.118550233809395777, -4.510116093748293586 ) ) ;
#35374 = DIRECTION ( 'NONE',  ( 0.3939253465568943735, 0.3234796780324362686, -0.8603393047164948904 ) ) ;
#35375 = CARTESIAN_POINT ( 'NONE',  ( -12.58725039716645000, -33.86007533429943095, 10.00564543523592320 ) ) ;
#35376 = CARTESIAN_POINT ( 'NONE',  ( 24.67726771998958668, 0.8588187409780198012, -13.47840055350262212 ) ) ;
#35378 = VERTEX_POINT ( 'NONE', #48771 ) ;
#35377 = DIRECTION ( 'NONE',  ( -1.000000000000000000, 0.000000000000000000, 0.000000000000000000 ) ) ;
#35379 = DIRECTION ( 'NONE',  ( 1.000000000000000000, 0.000000000000000000, 0.000000000000000000 ) ) ;
#35380 = ORIENTED_EDGE ( 'NONE', *, *, #55385, .F. ) ;
#35381 = CIRCLE ( 'NONE', #22694, 7.499999999999988454 ) ;
#35382 = DIRECTION ( 'NONE',  ( 1.000000000000000000, 0.000000000000000000, -0.000000000000000000 ) ) ;
#35383 = ORIENTED_EDGE ( 'NONE', *, *, #28080, .T. ) ;
#35384 = VECTOR ( 'NONE', #51700, 1000.000000000000000 ) ;
#35385 = ORIENTED_EDGE ( 'NONE', *, *, #33567, .T. ) ;
#35386 = CARTESIAN_POINT ( 'NONE',  ( 0.2956976708475548277, 9.528782683728200809, -7.708404409946551183 ) ) ;
#35387 = CARTESIAN_POINT ( 'NONE',  ( 13.74768401152558894, -28.58623978001741861, 12.41178146356747192 ) ) ;
#35389 = FACE_OUTER_BOUND ( 'NONE', #9880, .T. ) ;
#35388 = AXIS2_PLACEMENT_3D ( 'NONE', #55660, #19759, #64951 ) ;
#35390 = EDGE_CURVE ( 'NONE', #44685, #41165, #22513, .T. ) ;
#35391 = DIRECTION ( 'NONE',  ( -1.000000000000000000, 0.000000000000000000, -0.000000000000000000 ) ) ;
#35392 = CARTESIAN_POINT ( 'NONE',  ( 2.000000000000001776, 0.000000000000000000, 0.000000000000000000 ) ) ;
#35393 = LINE ( 'NONE', #64659, #12919 ) ;
#35394 = ORIENTED_EDGE ( 'NONE', *, *, #57442, .T. ) ;
#35395 = VERTEX_POINT ( 'NONE', #34098 ) ;
#35396 = CARTESIAN_POINT ( 'NONE',  ( -27.04788180060269553, -2.650714769830309070, -1.844972430941769215 ) ) ;
#35397 = VERTEX_POINT ( 'NONE', #45396 ) ;
#35398 = CIRCLE ( 'NONE', #22699, 5.000000000000000888 ) ;
#35399 = EDGE_LOOP ( 'NONE', ( #31680, #45094, #32506, #57236 ) ) ;
#35400 = AXIS2_PLACEMENT_3D ( 'NONE', #57875, #52866, #7297 ) ;
#35401 = DIRECTION ( 'NONE',  ( -1.000000000000000000, 0.000000000000000000, 0.000000000000000000 ) ) ;
#35402 = CARTESIAN_POINT ( 'NONE',  ( 10.48620311856346454, 8.250315036047107142, -8.713914264323181058 ) ) ;
#35403 = DIRECTION ( 'NONE',  ( 1.000000000000000000, 0.000000000000000000, 0.000000000000000000 ) ) ;
#35404 = DIRECTION ( 'NONE',  ( 0.000000000000000000, 0.000000000000000000, 1.000000000000000000 ) ) ;
#35405 = CARTESIAN_POINT ( 'NONE',  ( -22.27722022243424149, 1.227876413014602708, -3.470949075637792092 ) ) ;
#35406 = AXIS2_PLACEMENT_3D ( 'NONE', #59684, #55680, #19452 ) ;
#35407 = DIRECTION ( 'NONE',  ( -0.000000000000000000, -1.000000000000000000, -0.000000000000000000 ) ) ;
#35408 = EDGE_CURVE ( 'NONE', #7420, #30257, #39351, .T. ) ;
#35409 = FACE_OUTER_BOUND ( 'NONE', #2406, .T. ) ;
#35410 = VERTEX_POINT ( 'NONE', #29445 ) ;
#35411 = AXIS2_PLACEMENT_3D ( 'NONE', #24761, #60995, #29725 ) ;
#35412 = EDGE_CURVE ( 'NONE', #24790, #57555, #25632, .T. ) ;
#35413 = ORIENTED_EDGE ( 'NONE', *, *, #51277, .T. ) ;
#35414 = CIRCLE ( 'NONE', #51347, 5.000000000000000000 ) ;
#35415 = EDGE_CURVE ( 'NONE', #28121, #24059, #44400, .T. ) ;
#35416 = DIRECTION ( 'NONE',  ( 0.000000000000000000, -0.01356324068817991828, 0.9999080150203990547 ) ) ;
#35417 = FILL_AREA_STYLE ('',( #15134 ) ) ;
#35418 = B_SPLINE_CURVE_WITH_KNOTS ( 'NONE', 3,
 ( #42524, #17289, #56198, #25964, #23252, #58518, #37571, #43517, #48864, #22944, #2332, #58181, #7291, #63798, #2991, #8290, #3319, #27922, #18282, #8609, #38881, #33564, #38546, #58866, #13282, #18623 ),
 .UNSPECIFIED., .F., .F.,
 ( 4, 2, 2, 2, 2, 2, 2, 2, 2, 2, 2, 2, 4 ),
 ( 0.000000000000000000, 0.001187878019264044637, 0.001781817028896066739, 0.002375756038528089274, 0.002969695048160110509, 0.003563634057792131309, 0.004157573067424152544, 0.004751512077056174212, 0.005345451086688195012, 0.005939390096320216680, 0.007127268115584260884, 0.008315146134848305087, 0.009503024154112350158 ),
 .UNSPECIFIED. ) ;
#35419 = CARTESIAN_POINT ( 'NONE',  ( 6.661533233520612107, -4.211056110068225777, -12.82664335996205196 ) ) ;
#35420 = CARTESIAN_POINT ( 'NONE',  ( 6.529851256712529306, -4.705937351017101200, 11.04517589364730235 ) ) ;
#35421 = CIRCLE ( 'NONE', #6775, 12.18650000000000055 ) ;
#35422 = CARTESIAN_POINT ( 'NONE',  ( -22.71097035706202760, 2.118550233809425087, 4.510116093748266053 ) ) ;
#35423 = EDGE_CURVE ( 'NONE', #3983, #21953, #19184, .T. ) ;
#35424 = CARTESIAN_POINT ( 'NONE',  ( 24.35413283551385177, -1.441936682210068099, -13.42734599445702415 ) ) ;
#35425 = EDGE_CURVE ( 'NONE', #42626, #46347, #34745, .T. ) ;
#35426 = CARTESIAN_POINT ( 'NONE',  ( -36.00000000000000711, -9.621072037177057723, 8.366449238204328509 ) ) ;
#35427 = CARTESIAN_POINT ( 'NONE',  ( 2.589278595512946701, 6.089088204448742658, 4.794929105510930434 ) ) ;
#35428 = ORIENTED_EDGE ( 'NONE', *, *, #55773, .T. ) ;
#35429 = VECTOR ( 'NONE', #42071, 1000.000000000000000 ) ;
#35430 = CARTESIAN_POINT ( 'NONE',  ( 2.406456491624145766, -4.152987573058577908, -9.571062220827512235 ) ) ;
#35431 = CARTESIAN_POINT ( 'NONE',  ( 5.515188684475870851, 0.004442604682416617309, -0.002983184900675344906 ) ) ;
#35432 = VECTOR ( 'NONE', #23897, 1000.000000000000000 ) ;
#35433 = CARTESIAN_POINT ( 'NONE',  ( 0.000000000000000000, 4.604744433234757572, -5.919993978425451608 ) ) ;
#35434 = ADVANCED_FACE ( 'NONE', ( #45728 ), #14789, .T. ) ;
#35435 = CIRCLE ( 'NONE', #15271, 7.499999999999988454 ) ;
#35436 = ADVANCED_FACE ( 'NONE', ( #65662 ), #14150, .T. ) ;
#35437 = CARTESIAN_POINT ( 'NONE',  ( -9.179144435738862740, -32.64956785250165439, -12.36195000407440148 ) ) ;
#35438 = CARTESIAN_POINT ( 'NONE',  ( 2.305787727787084407, -5.970480882365253983, 4.792270232040873879 ) ) ;
#35439 = VERTEX_POINT ( 'NONE', #50416 ) ;
#35440 = CARTESIAN_POINT ( 'NONE',  ( -18.52069857313810175, -4.381854579544467221, -12.76954371343036954 ) ) ;
#35441 = CARTESIAN_POINT ( 'NONE',  ( 1.452237505248552996, -12.64182585313125706, -0.5922625322518334512 ) ) ;
#35442 = AXIS2_PLACEMENT_3D ( 'NONE', #37471, #47786, #58426 ) ;
#35444 = EDGE_CURVE ( 'NONE', #36108, #37474, #39422, .T. ) ;
#35443 = CARTESIAN_POINT ( 'NONE',  ( 18.66975156949834513, -28.88996333714986875, -7.079161351701957372 ) ) ;
#35445 = ORIENTED_EDGE ( 'NONE', *, *, #40300, .T. ) ;
#35446 = DIRECTION ( 'NONE',  ( 0.000000000000000000, -0.01356324068817992175, 0.9999080150203990547 ) ) ;
#35447 = CYLINDRICAL_SURFACE ( 'NONE', #52295, 4.999999999999999112 ) ;
#35448 = FACE_OUTER_BOUND ( 'NONE', #47220, .T. ) ;
#35449 = CIRCLE ( 'NONE', #45009, 5.000000000000002665 ) ;
#35451 = ORIENTED_EDGE ( 'NONE', *, *, #24358, .T. ) ;
#35450 = CARTESIAN_POINT ( 'NONE',  ( 2.639814597422733833, 1.095525832903487817, 7.689608172406200204 ) ) ;
#35452 = FACE_OUTER_BOUND ( 'NONE', #18988, .T. ) ;
#35453 = CYLINDRICAL_SURFACE ( 'NONE', #9575, 5.000000000000000888 ) ;
#35454 = VERTEX_POINT ( 'NONE', #54745 ) ;
#35455 = CARTESIAN_POINT ( 'NONE',  ( 0.2869720083484343376, 7.715523637151767922, 9.519277517057126659 ) ) ;
#35456 = DIRECTION ( 'NONE',  ( -1.000000000000000000, 0.000000000000000000, 0.000000000000000000 ) ) ;
#35457 = DIRECTION ( 'NONE',  ( 0.000000000000000000, -0.9346839223284580944, 0.3554799084908867868 ) ) ;
#35458 = DIRECTION ( 'NONE',  ( 1.000000000000000000, 0.000000000000000000, 0.000000000000000000 ) ) ;
#35459 = CARTESIAN_POINT ( 'NONE',  ( 37.00000000000000711, 4.705694406421931860E-17, -3.469127814946512892E-15 ) ) ;
#35460 = CIRCLE ( 'NONE', #4702, 4.999999999999999112 ) ;
#35461 = CARTESIAN_POINT ( 'NONE',  ( -37.00000000000000711, 0.000000000000000000, 0.000000000000000000 ) ) ;
#35462 = CARTESIAN_POINT ( 'NONE',  ( -27.08429572838383947, 0.6096735944848206135, -2.208905845566032866 ) ) ;
#35463 = ORIENTED_EDGE ( 'NONE', *, *, #59935, .F. ) ;
#35464 = DIRECTION ( 'NONE',  ( -1.000000000000000000, 0.000000000000000000, 0.000000000000000000 ) ) ;
#35465 = ORIENTED_EDGE ( 'NONE', *, *, #20103, .T. ) ;
#35466 = FILL_AREA_STYLE ('',( #41768 ) ) ;
#35467 = CARTESIAN_POINT ( 'NONE',  ( -47.00000000000000711, 0.000000000000000000, 0.000000000000000000 ) ) ;
#35468 = CARTESIAN_POINT ( 'NONE',  ( 16.78263030916553333, -12.17295508002144011, 5.836879698929882565 ) ) ;
#35469 = EDGE_CURVE ( 'NONE', #5947, #52522, #58513, .T. ) ;
#35470 = EDGE_CURVE ( 'NONE', #45493, #23985, #59722, .T. ) ;
#35471 = AXIS2_PLACEMENT_3D ( 'NONE', #50651, #20373, #20709 ) ;
#35472 = DIRECTION ( 'NONE',  ( 0.000000000000000000, 0.01356324068817998940, -0.9999080150203990547 ) ) ;
#35473 = VERTEX_POINT ( 'NONE', #9164 ) ;
#35474 = CYLINDRICAL_SURFACE ( 'NONE', #8569, 12.18650000000000055 ) ;
#35475 = CYLINDRICAL_SURFACE ( 'NONE', #60305, 7.499999999999988454 ) ;
#35476 = CARTESIAN_POINT ( 'NONE',  ( -22.27715239060371744, -1.072868796692241888, 3.521735673127119881 ) ) ;
#35477 = ORIENTED_EDGE ( 'NONE', *, *, #39954, .F. ) ;
#35478 = EDGE_LOOP ( 'NONE', ( #6018, #35080, #55026, #16186, #23558, #6047, #27570, #29825, #9744, #56671, #11414, #9292, #51731, #47950, #57913, #42196, #65541, #54701, #31503, #24638, #26070, #8789, #11434, #30199, #26906, #39784, #56831, #62370, #56859, #43980, #248, #15857, #17591, #49623, #52022, #38873, #54576, #28344, #10852, #1634, #30882, #8041, #64556, #28613, #38969, #64675, #13340, #24294, #42182, #50794, #59080, #58307, #40844, #44858, #9604, #22041, #34475, #12501, #29671, #10572, #56219, #57447, #19637, #37137, #5631, #21240, #2036, #37983, #4144, #53415, #12269, #34587, #10669, #5806, #25997, #44924, #48513, #63918, #33364, #31069, #65042, #63837, #7589, #49344, #40367, #49801, #20186, #48084, #62907, #51843, #40865, #30039, #32388, #9146, #58667, #47523, #15185, #32646, #63953, #5268, #7414, #45268, #29029, #20238, #28462, #35465, #49836, #38417, #63019, #34621, #49415, #1924 ) ) ;
#35479 = CARTESIAN_POINT ( 'NONE',  ( 2.573738926104375047, 0.2352053552898537014, -7.741646296020610052 ) ) ;
#35480 = AXIS2_PLACEMENT_3D ( 'NONE', #22126, #17803, #52733 ) ;
#35481 = EDGE_CURVE ( 'NONE', #14609, #8090, #6519, .T. ) ;
#35482 = CIRCLE ( 'NONE', #17461, 5.000000000000000888 ) ;
#35483 = ORIENTED_EDGE ( 'NONE', *, *, #52799, .T. ) ;
#35484 = DIRECTION ( 'NONE',  ( 0.000000000000000000, 0.000000000000000000, 1.000000000000000000 ) ) ;
#35485 = DIRECTION ( 'NONE',  ( -1.000000000000000000, 0.000000000000000000, 0.000000000000000000 ) ) ;
#35486 = CARTESIAN_POINT ( 'NONE',  ( 5.515539859299206427, -0.001241880655086973709, -0.005924322247675104479 ) ) ;
#35487 = CARTESIAN_POINT ( 'NONE',  ( -29.63048194961400483, -0.3368890121124099024, 11.99716775028113425 ) ) ;
#35488 = CARTESIAN_POINT ( 'NONE',  ( -35.00000000000000000, -11.66953048682402283, 3.511814412392074480 ) ) ;
#35489 = CARTESIAN_POINT ( 'NONE',  ( 0.2648978790185619880, -10.53870023327867855, 6.237101853238509186 ) ) ;
#35490 = EDGE_CURVE ( 'NONE', #2448, #27489, #108, .T. ) ;
#35491 = CARTESIAN_POINT ( 'NONE',  ( 3.152665057734040488, 0.000000000000000000, 0.000000000000000000 ) ) ;
#35492 = VERTEX_POINT ( 'NONE', #3882 ) ;
#35493 = CARTESIAN_POINT ( 'NONE',  ( 2.244591118396557672, 7.634724215899723276, -0.1074970442784372593 ) ) ;
#35494 = CARTESIAN_POINT ( 'NONE',  ( 23.00365627137244573, 10.16437141043587289, -6.387237743053422179 ) ) ;
#35495 = EDGE_CURVE ( 'NONE', #22815, #17671, #7552, .T. ) ;
#35496 = CARTESIAN_POINT ( 'NONE',  ( 2.241526690369556540, 5.859443871527043157, 4.894066724724273953 ) ) ;
#35497 = CARTESIAN_POINT ( 'NONE',  ( 2.241506898688417682, -7.511570207700569490, 1.364429914801493338 ) ) ;
#35498 = VECTOR ( 'NONE', #43025, 1000.000000000000000 ) ;
#35499 = FACE_OUTER_BOUND ( 'NONE', #33386, .T. ) ;
#35500 = LINE ( 'NONE', #55797, #59693 ) ;
#35501 = DIRECTION ( 'NONE',  ( 0.000000000000000000, -0.6876994588534294239, 0.7259954919231249582 ) ) ;
#35502 = CYLINDRICAL_SURFACE ( 'NONE', #11896, 5.000000000000000888 ) ;
#35503 = AXIS2_PLACEMENT_3D ( 'NONE', #51105, #61710, #56764 ) ;
#35504 = EDGE_LOOP ( 'NONE', ( #4023, #2715, #47724, #24705 ) ) ;
#35505 = DIRECTION ( 'NONE',  ( -1.000000000000000000, 0.000000000000000000, 0.000000000000000000 ) ) ;
#35506 = EDGE_LOOP ( 'NONE', ( #39373, #14389, #37189, #33871 ) ) ;
#35507 = DIRECTION ( 'NONE',  ( 0.000000000000000000, -0.3218879778915842427, 0.9467777615094616905 ) ) ;
#35508 = LINE ( 'NONE', #40838, #50028 ) ;
#35509 = CONICAL_SURFACE ( 'NONE', #21720, 7.938172270156617749, 1.280189991382167047 ) ;
#35510 = EDGE_CURVE ( 'NONE', #52527, #36765, #9678, .T. ) ;
#35511 = CARTESIAN_POINT ( 'NONE',  ( 0.2646305136544065406, 11.46223899740599883, 4.312539723326170638 ) ) ;
#35512 = CARTESIAN_POINT ( 'NONE',  ( 2.653899356899763973, -7.694895988366324602, -1.091629880170596811 ) ) ;
#35513 = CARTESIAN_POINT ( 'NONE',  ( 2.273267844204675647, 2.472013099045248463, -7.234348261136679170 ) ) ;
#35514 = ADVANCED_FACE ( 'NONE', ( #24804 ), #45085, .T. ) ;
#35515 = ORIENTED_EDGE ( 'NONE', *, *, #52818, .T. ) ;
#35516 = FACE_OUTER_BOUND ( 'NONE', #20084, .T. ) ;
#35517 = CARTESIAN_POINT ( 'NONE',  ( 2.241352910868909643, -3.744764251557037849, 6.652881166698498383 ) ) ;
#35518 = CARTESIAN_POINT ( 'NONE',  ( 0.7400311444011727913, -1.803686700615490635, 12.27261279799597560 ) ) ;
#35519 = CARTESIAN_POINT ( 'NONE',  ( 2.241536586108912488, -6.614789707676438368, -3.811784405792419950 ) ) ;
#35520 = EDGE_CURVE ( 'NONE', #36018, #57723, #36218, .T. ) ;
#35521 = EDGE_CURVE ( 'NONE', #22936, #63998, #60703, .T. ) ;
#35522 = CARTESIAN_POINT ( 'NONE',  ( -35.00000000000000000, -11.39945968423475264, 5.710938531231672499 ) ) ;
#35523 = CARTESIAN_POINT ( 'NONE',  ( 35.00000000000000000, 4.705694406421931860E-17, -3.469127814946512892E-15 ) ) ;
#35524 =( BOUNDED_CURVE ( )  B_SPLINE_CURVE ( 3, ( #38923, #38591, #7330, #12640 ),
 .UNSPECIFIED., .F., .F. ) 
 B_SPLINE_CURVE_WITH_KNOTS ( ( 4, 4 ),
 ( 1.632078076156195046, 1.647829253658086746 ),
 .UNSPECIFIED. ) 
 CURVE ( )  GEOMETRIC_REPRESENTATION_ITEM ( )  RATIONAL_B_SPLINE_CURVE ( ( 1.000000000000000000, 0.9999793251408052308, 0.9999793251408052308, 1.000000000000000000 ) ) 
 REPRESENTATION_ITEM ( '' )  );
#35525 = ORIENTED_EDGE ( 'NONE', *, *, #35018, .F. ) ;
#35527 = EDGE_CURVE ( 'NONE', #2866, #41816, #5978, .T. ) ;
#35526 = CARTESIAN_POINT ( 'NONE',  ( -35.00000000000000000, 2.968224442958403486, 11.81949347079748058 ) ) ;
#35528 = ORIENTED_EDGE ( 'NONE', *, *, #10879, .F. ) ;
#35529 = CARTESIAN_POINT ( 'NONE',  ( -28.66013792860432119, -0.7552004871165356459, 1.673433383655430484 ) ) ;
#35530 = DIRECTION ( 'NONE',  ( -1.000000000000000000, 0.000000000000000000, 0.000000000000000000 ) ) ;
#35531 = CARTESIAN_POINT ( 'NONE',  ( 29.16097522612058413, -8.612999037061474183, 8.368222170583779373 ) ) ;
#35532 = DIRECTION ( 'NONE',  ( 1.000000000000000000, -0.000000000000000000, 0.000000000000000000 ) ) ;
#35533 = VERTEX_POINT ( 'NONE', #15468 ) ;
#35534 = VERTEX_POINT ( 'NONE', #22018 ) ;
#35535 = CARTESIAN_POINT ( 'NONE',  ( 5.515188684475870851, 0.004322737127823972868, 0.003154373509839877594 ) ) ;
#35536 = VERTEX_POINT ( 'NONE', #48308 ) ;
#35537 = CARTESIAN_POINT ( 'NONE',  ( 2.276198483117255922, -6.543270001966377869, -3.955655305430039625 ) ) ;
#35538 = DIRECTION ( 'NONE',  ( 0.3865475372811021937, 0.5778504531710993986, 0.7187975063895742922 ) ) ;
#35539 = CARTESIAN_POINT ( 'NONE',  ( -22.27715239060371744, -3.521735673127123878, -1.072868796692257209 ) ) ;
#35540 = CARTESIAN_POINT ( 'NONE',  ( 0.5572780756278378211, 9.256402261579090407, 8.165890079445167871 ) ) ;
#35541 = CARTESIAN_POINT ( 'NONE',  ( 0.8320506296491578802, 9.275353261146646489, -8.282532257448718127 ) ) ;
#35542 = CARTESIAN_POINT ( 'NONE',  ( 5.515539859299206427, 0.006049968793488819975, -0.0001942659352250742744 ) ) ;
#35543 = CARTESIAN_POINT ( 'NONE',  ( 3.291290029914074378, 8.250315036047103590, 25.00000000000000000 ) ) ;
#35544 = VERTEX_POINT ( 'NONE', #15779 ) ;
#35545 = AXIS2_PLACEMENT_3D ( 'NONE', #59543, #48597, #58581 ) ;
#35546 = CARTESIAN_POINT ( 'NONE',  ( 2.639814597422741826, -2.414168779979533941, -7.382549681340934811 ) ) ;
#35547 = ORIENTED_EDGE ( 'NONE', *, *, #36805, .F. ) ;
#35548 = CARTESIAN_POINT ( 'NONE',  ( 0.5547464869798235387, -2.442933571354888755, -12.09851097165511646 ) ) ;
#35549 = AXIS2_PLACEMENT_3D ( 'NONE', #29651, #24687, #56241 ) ;
#35550 = DIRECTION ( 'NONE',  ( -1.000000000000000000, 0.000000000000000000, 0.000000000000000000 ) ) ;
#35551 = ADVANCED_FACE ( 'NONE', ( #62560 ), #56030, .T. ) ;
#35552 = ORIENTED_EDGE ( 'NONE', *, *, #2091, .T. ) ;
#35553 = FACE_OUTER_BOUND ( 'NONE', #27420, .T. ) ;
#35554 = EDGE_CURVE ( 'NONE', #23085, #55514, #35733, .T. ) ;
#35555 = ORIENTED_EDGE ( 'NONE', *, *, #46326, .T. ) ;
#35556 = CARTESIAN_POINT ( 'NONE',  ( 18.84867683979355846, 25.00000000000000000, 12.12095735156415088 ) ) ;
#35557 = CARTESIAN_POINT ( 'NONE',  ( 6.192035194031760170, -8.543018847948518513, -10.45909626451002161 ) ) ;
#35558 = CARTESIAN_POINT ( 'NONE',  ( 0.2646305136544072623, 2.256625640822473411, -12.03696649559612553 ) ) ;
#35559 = CARTESIAN_POINT ( 'NONE',  ( 7.278301338833046863, -5.781067271407755115, 10.51827409704459093 ) ) ;
#35560 = ORIENTED_EDGE ( 'NONE', *, *, #64246, .F. ) ;
#35561 = ORIENTED_EDGE ( 'NONE', *, *, #58765, .T. ) ;
#35562 = CARTESIAN_POINT ( 'NONE',  ( 2.440552418640496324, -6.765628357760804512, 3.678171968408304959 ) ) ;
#35563 = ORIENTED_EDGE ( 'NONE', *, *, #31018, .F. ) ;
#35564 = DIRECTION ( 'NONE',  ( 0.000000000000000000, -0.2149704402110115264, -0.9766205557100894330 ) ) ;
#35565 = ORIENTED_EDGE ( 'NONE', *, *, #63145, .F. ) ;
#35566 = EDGE_CURVE ( 'NONE', #22574, #20918, #36916, .T. ) ;
#35567 = ORIENTED_EDGE ( 'NONE', *, *, #14987, .T. ) ;
#35568 = EDGE_LOOP ( 'NONE', ( #26304, #20329, #50858, #21773 ) ) ;
#35569 = CARTESIAN_POINT ( 'NONE',  ( 2.589278595512759740, -5.779442428606794913, 5.163950571302105885 ) ) ;
#35570 = CARTESIAN_POINT ( 'NONE',  ( -10.65145977119705201, -26.92745566885138686, 13.64141904900985836 ) ) ;
#35571 = DIRECTION ( 'NONE',  ( 0.000000000000000000, 0.000000000000000000, 1.000000000000000000 ) ) ;
#35572 = DIRECTION ( 'NONE',  ( 0.000000000000000000, 0.9551603052523490733, -0.2960891610144476549 ) ) ;
#35573 = DIRECTION ( 'NONE',  ( -1.000000000000000000, 0.000000000000000000, -0.000000000000000000 ) ) ;
#35574 = EDGE_LOOP ( 'NONE', ( #40895, #35205, #60238, #40306 ) ) ;
#35575 = CARTESIAN_POINT ( 'NONE',  ( 2.305787727787084407, -2.461236246751023593, -7.249469779319933416 ) ) ;
#35576 = ORIENTED_EDGE ( 'NONE', *, *, #54686, .F. ) ;
#35577 = FACE_OUTER_BOUND ( 'NONE', #18390, .T. ) ;
#35578 = CYLINDRICAL_SURFACE ( 'NONE', #20344, 5.000000000000000888 ) ;
#35579 = ADVANCED_FACE ( 'NONE', ( #47955 ), #57617, .T. ) ;
#35580 = VECTOR ( 'NONE', #48988, 1000.000000000000000 ) ;
#35581 = ORIENTED_EDGE ( 'NONE', *, *, #33430, .F. ) ;
#35582 = CARTESIAN_POINT ( 'NONE',  ( 0.2869720083484343376, -10.71444492121020708, 5.945302302873217926 ) ) ;
#35583 = CARTESIAN_POINT ( 'NONE',  ( 0.9232058338315048962, -9.306586124266539528, -8.301689855530263173 ) ) ;
#35584 = CARTESIAN_POINT ( 'NONE',  ( 2.000000000000001776, 7.203928197742101247, 2.086484728383167564 ) ) ;
#35585 = EDGE_CURVE ( 'NONE', #61650, #29988, #6481, .T. ) ;
#35586 = EDGE_LOOP ( 'NONE', ( #35701, #42233, #35996, #44913, #2959, #52015 ) ) ;
#35587 = DIRECTION ( 'NONE',  ( -1.000000000000000000, 0.000000000000000000, 0.000000000000000000 ) ) ;
#35588 = AXIS2_PLACEMENT_3D ( 'NONE', #35261, #55570, #10010 ) ;
#35589 = EDGE_LOOP ( 'NONE', ( #14262, #33226, #32310, #42142 ) ) ;
#35590 = DIRECTION ( 'NONE',  ( 0.000000000000000000, 0.000000000000000000, -1.000000000000000000 ) ) ;
#35591 = CARTESIAN_POINT ( 'NONE',  ( -10.65145977119704845, -26.92745566885138331, -13.64141904900985836 ) ) ;
#35592 = CARTESIAN_POINT ( 'NONE',  ( -4.047649113456393444, -26.73415408998407372, 15.95376587162193260 ) ) ;
#35593 = CARTESIAN_POINT ( 'NONE',  ( 2.305787727787084407, -3.682701754025465846, -6.711944854845862451 ) ) ;
#35594 = DIRECTION ( 'NONE',  ( -1.000000000000000000, 0.000000000000000000, 0.000000000000000000 ) ) ;
#35595 = VERTEX_POINT ( 'NONE', #12035 ) ;
#35596 = DIRECTION ( 'NONE',  ( 0.000000000000000000, -0.01356324068818000328, 0.9999080150203990547 ) ) ;
#35597 = LINE ( 'NONE', #15634, #46042 ) ;
#35598 = DIRECTION ( 'NONE',  ( -1.000000000000000000, -0.000000000000000000, 0.000000000000000000 ) ) ;
#35599 = CARTESIAN_POINT ( 'NONE',  ( 21.98021488419000136, -12.96235417471537943, -3.789643664872785145 ) ) ;
#35600 = ADVANCED_FACE ( 'NONE', ( #2065 ), #16321, .F. ) ;
#35601 = VECTOR ( 'NONE', #8661, 1000.000000000000000 ) ;
#35602 = EDGE_CURVE ( 'NONE', #28220, #8078, #50053, .T. ) ;
#35603 = CARTESIAN_POINT ( 'NONE',  ( 0.3474126878361798454, 12.27082419038178429, -0.2587235634078462465 ) ) ;
#35605 = EDGE_CURVE ( 'NONE', #9767, #57779, #41537, .T. ) ;
#35604 = CARTESIAN_POINT ( 'NONE',  ( -35.00000000000000000, -5.814360711498210321, -10.70999494708499000 ) ) ;
#35606 = CARTESIAN_POINT ( 'NONE',  ( -22.27834755396594346, 1.338300169228711090, -3.434702243602646199 ) ) ;
#35607 = CARTESIAN_POINT ( 'NONE',  ( -7.393613020821579340, -5.386680228572943818, -10.72686196631678968 ) ) ;
#35608 = CARTESIAN_POINT ( 'NONE',  ( 2.247206125382827935, 0.1157489416152577000, -7.635476611656031309 ) ) ;
#35609 = CIRCLE ( 'NONE', #8061, 12.18650000000000055 ) ;
#35610 = EDGE_CURVE ( 'NONE', #13885, #4816, #42954, .T. ) ;
#35611 = VERTEX_POINT ( 'NONE', #64855 ) ;
#35612 = VERTEX_POINT ( 'NONE', #38283 ) ;
#35613 = DIRECTION ( 'NONE',  ( -1.000000000000000000, -1.836970198721029688E-16, -0.000000000000000000 ) ) ;
#35614 = CARTESIAN_POINT ( 'NONE',  ( 33.44920912455760487, -2.804301875032225944, -22.47723755754418562 ) ) ;
#35615 = DIRECTION ( 'NONE',  ( 1.000000000000000000, 0.000000000000000000, 0.000000000000000000 ) ) ;
#35616 = CARTESIAN_POINT ( 'NONE',  ( 2.242819959140783137, -1.224821922055089773, -7.536009875295528460 ) ) ;
#35617 = ORIENTED_EDGE ( 'NONE', *, *, #23972, .F. ) ;
#35618 = ORIENTED_EDGE ( 'NONE', *, *, #7887, .F. ) ;
#35619 = ORIENTED_EDGE ( 'NONE', *, *, #41590, .F. ) ;
#35620 = CARTESIAN_POINT ( 'NONE',  ( 0.2648978790185584908, -12.24533305150758089, -0.1321385342563691223 ) ) ;
#35621 = CARTESIAN_POINT ( 'NONE',  ( -22.59969328935897082, 1.672297795814042143, 4.339503524536170609 ) ) ;
#35622 = VERTEX_POINT ( 'NONE', #13030 ) ;
#35623 = CARTESIAN_POINT ( 'NONE',  ( 25.00000000000000711, -3.797884998337192286, -25.00000000000000000 ) ) ;
#35624 = DIRECTION ( 'NONE',  ( 1.000000000000000000, 0.000000000000000000, 0.000000000000000000 ) ) ;
#35625 = DIRECTION ( 'NONE',  ( -1.000000000000000000, -0.000000000000000000, 0.000000000000000000 ) ) ;
#35626 = EDGE_CURVE ( 'NONE', #3473, #38228, #64693, .T. ) ;
#35627 = ORIENTED_EDGE ( 'NONE', *, *, #61961, .T. ) ;
#35628 = AXIS2_PLACEMENT_3D ( 'NONE', #64691, #3234, #58779 ) ;
#35629 = CARTESIAN_POINT ( 'NONE',  ( -22.27786964138239867, 0.3434379038477919366, 3.667590411551997054 ) ) ;
#35630 = CARTESIAN_POINT ( 'NONE',  ( -3.619268891295734480, -30.76314776371165749, -15.03790153758943582 ) ) ;
#35631 = CARTESIAN_POINT ( 'NONE',  ( -35.00000000000000000, -11.61175578952785159, -1.771820996347277966 ) ) ;
#35632 = VERTEX_POINT ( 'NONE', #43271 ) ;
#35633 = DIRECTION ( 'NONE',  ( 0.000000000000000000, -0.9868265225415245867, -0.1617819965527747539 ) ) ;
#35634 = EDGE_LOOP ( 'NONE', ( #1381, #53337, #64504, #11530 ) ) ;
#35635 = CARTESIAN_POINT ( 'NONE',  ( 37.00000000000000711, -7.717887834988180984, 8.854740511458926377 ) ) ;
#35636 = ORIENTED_EDGE ( 'NONE', *, *, #24377, .F. ) ;
#35637 = CARTESIAN_POINT ( 'NONE',  ( 13.18551377979218486, -11.38597202338936754, -3.795551372338616947 ) ) ;
#35638 = CIRCLE ( 'NONE', #30339, 5.000000000000000000 ) ;
#35639 = CARTESIAN_POINT ( 'NONE',  ( -15.99047871552748390, -35.00000000000000000, 5.006074194136941991 ) ) ;
#35640 = CARTESIAN_POINT ( 'NONE',  ( 35.00000000000000000, 11.54110654723649176, -2.185196060783925809 ) ) ;
#35641 = CARTESIAN_POINT ( 'NONE',  ( -37.00000000000000711, 9.240395740215735287, -7.251710744571480127 ) ) ;
#35642 = CARTESIAN_POINT ( 'NONE',  ( 0.3223008802179250232, -12.26274332232494046, 0.2444878876722800243 ) ) ;
#35643 = PLANE ( 'NONE',  #5356 ) ;
#35644 = CARTESIAN_POINT ( 'NONE',  ( -27.08456565417852602, -0.2166646653334006467, -2.282055114149017072 ) ) ;
#35645 = CARTESIAN_POINT ( 'NONE',  ( 2.665405856346777291, -3.808819464940497390, 8.776564688671616210 ) ) ;
#35647 = ORIENTED_EDGE ( 'NONE', *, *, #21466, .F. ) ;
#35646 = DIRECTION ( 'NONE',  ( -1.000000000000000000, 0.000000000000000000, 0.000000000000000000 ) ) ;
#35648 = DIRECTION ( 'NONE',  ( -1.000000000000000000, 0.000000000000000000, 0.000000000000000000 ) ) ;
#35649 = ORIENTED_EDGE ( 'NONE', *, *, #19810, .F. ) ;
#35650 = CARTESIAN_POINT ( 'NONE',  ( 0.3537226245948354997, -4.442821955543875490, 11.44347094181050473 ) ) ;
#35651 = ORIENTED_EDGE ( 'NONE', *, *, #65610, .F. ) ;
#35652 = CARTESIAN_POINT ( 'NONE',  ( 35.00000000000000000, 12.66641127287627633, 1.457575200925409709 ) ) ;
#35653 = EDGE_CURVE ( 'NONE', #14422, #31670, #13941, .T. ) ;
#35654 = VERTEX_POINT ( 'NONE', #58941 ) ;
#35655 = CARTESIAN_POINT ( 'NONE',  ( -35.00000000000000000, 0.000000000000000000, 0.000000000000000000 ) ) ;
#35656 = CARTESIAN_POINT ( 'NONE',  ( 1.719304012341537957, 12.20344780066137602, -3.626341562669237906 ) ) ;
#35657 = CARTESIAN_POINT ( 'NONE',  ( 22.57855258442564761, -4.427776684447072952, 11.15324139578564910 ) ) ;
#35658 = CYLINDRICAL_SURFACE ( 'NONE', #30586, 12.74999999999999822 ) ;
#35659 = EDGE_CURVE ( 'NONE', #5010, #34891, #21370, .T. ) ;
#35660 = CARTESIAN_POINT ( 'NONE',  ( 11.99083905025486629, 8.556418439408664867, -8.415045165346294098 ) ) ;
#35661 = VERTEX_POINT ( 'NONE', #53929 ) ;
#35662 = DIRECTION ( 'NONE',  ( 0.000000000000000000, 0.000000000000000000, 1.000000000000000000 ) ) ;
#35663 = ORIENTED_EDGE ( 'NONE', *, *, #60632, .T. ) ;
#35664 = CARTESIAN_POINT ( 'NONE',  ( 2.717984159218876261, 0.2836133496098577345, 7.788152353088898749 ) ) ;
#35665 = CARTESIAN_POINT ( 'NONE',  ( 35.00000000000000000, -10.49626516989275515, -7.238157050195593634 ) ) ;
#35666 = CARTESIAN_POINT ( 'NONE',  ( 0.2651627923886305527, -7.803990550466243015, -9.437479615842727654 ) ) ;
#35667 = VERTEX_POINT ( 'NONE', #13999 ) ;
#35668 = CARTESIAN_POINT ( 'NONE',  ( -27.08430418657510330, -0.9470735946412819350, 2.086666645150418109 ) ) ;
#35669 = ADVANCED_FACE ( 'NONE', ( #8367 ), #3406, .T. ) ;
#35670 = AXIS2_PLACEMENT_3D ( 'NONE', #3159, #23422, #13751 ) ;
#35671 = CARTESIAN_POINT ( 'NONE',  ( 49.96127604611442052, -0.007915161567782847199, 1.618137530678326552 ) ) ;
#35672 = FACE_OUTER_BOUND ( 'NONE', #6301, .T. ) ;
#35673 = CARTESIAN_POINT ( 'NONE',  ( -35.00000000000000000, 11.86701198550360203, -2.772148766915989881 ) ) ;
#35674 = ORIENTED_EDGE ( 'NONE', *, *, #45550, .F. ) ;
#35675 = DIRECTION ( 'NONE',  ( 0.000000000000000000, 0.9346839223284554299, -0.3554799084908935036 ) ) ;
#35676 = CARTESIAN_POINT ( 'NONE',  ( 5.011577697835214451, -30.99110506585922664, 14.75067033891186696 ) ) ;
#35677 = CARTESIAN_POINT ( 'NONE',  ( 2.350038591458104342, -10.60256821300789909, -0.6402934222729869118 ) ) ;
#35678 = EDGE_CURVE ( 'NONE', #24291, #18737, #43677, .T. ) ;
#35679 = CARTESIAN_POINT ( 'NONE',  ( 22.88594695219327235, 3.421158645304719137, 25.00000000000000000 ) ) ;
#35680 = DIRECTION ( 'NONE',  ( -1.000000000000000000, 0.000000000000000000, -0.000000000000000000 ) ) ;
#35681 = ORIENTED_EDGE ( 'NONE', *, *, #53660, .F. ) ;
#35682 = CARTESIAN_POINT ( 'NONE',  ( 2.244591118396559004, 0.1074970442784154295, 7.634724215899725941 ) ) ;
#35683 = DIRECTION ( 'NONE',  ( 0.000000000000000000, 0.000000000000000000, 1.000000000000000000 ) ) ;
#35684 = CARTESIAN_POINT ( 'NONE',  ( -22.29018399051993882, 3.576688584977253171, -1.024613686459438622 ) ) ;
#35685 = VERTEX_POINT ( 'NONE', #54259 ) ;
#35686 = CARTESIAN_POINT ( 'NONE',  ( 12.19629890822712426, 0.02883110402050519452, 13.50000000000000355 ) ) ;
#35687 = CARTESIAN_POINT ( 'NONE',  ( 2.241352910868908310, 6.569501556381442953, 3.889181972941473386 ) ) ;
#35688 = ORIENTED_EDGE ( 'NONE', *, *, #41600, .T. ) ;
#35689 = ORIENTED_EDGE ( 'NONE', *, *, #30403, .F. ) ;
#35690 = ORIENTED_EDGE ( 'NONE', *, *, #4155, .T. ) ;
#35691 = VERTEX_POINT ( 'NONE', #9023 ) ;
#35692 = DIRECTION ( 'NONE',  ( -1.000000000000000000, -0.000000000000000000, -0.000000000000000000 ) ) ;
#35693 = DIRECTION ( 'NONE',  ( 0.000000000000000000, -1.000000000000000000, 0.000000000000000000 ) ) ;
#35694 = DIRECTION ( 'NONE',  ( 0.000000000000000000, -0.6478160128812003871, 0.7617968321374831708 ) ) ;
#35695 = CARTESIAN_POINT ( 'NONE',  ( 8.937200413559445167, 4.820982231796476114, 10.99527590820397549 ) ) ;
#35696 = EDGE_CURVE ( 'NONE', #43264, #58366, #19003, .T. ) ;
#35697 = DIRECTION ( 'NONE',  ( 0.000000000000000000, 0.9289767198167898643, 0.3701381553399182289 ) ) ;
#35698 = CARTESIAN_POINT ( 'NONE',  ( -15.66605021877826331, -34.92947327577397942, 5.825441821991796942 ) ) ;
#35699 = DIRECTION ( 'NONE',  ( 1.000000000000000000, 0.000000000000000000, 0.000000000000000000 ) ) ;
#35701 = ORIENTED_EDGE ( 'NONE', *, *, #30925, .T. ) ;
#35700 = CARTESIAN_POINT ( 'NONE',  ( -32.16141091265169649, 25.00000000000000000, 5.384978440493686236 ) ) ;
#35702 = EDGE_CURVE ( 'NONE', #55428, #48647, #2068, .T. ) ;
#35703 = DIRECTION ( 'NONE',  ( 1.000000000000000000, -0.000000000000000000, 0.000000000000000000 ) ) ;
#35704 = ORIENTED_EDGE ( 'NONE', *, *, #45442, .T. ) ;
#35705 = CARTESIAN_POINT ( 'NONE',  ( 5.515539859299206427, 0.001886660928063890567, 0.005751553894234958178 ) ) ;
#35706 = VERTEX_POINT ( 'NONE', #41228 ) ;
#35707 = ORIENTED_EDGE ( 'NONE', *, *, #13428, .F. ) ;
#35708 = CARTESIAN_POINT ( 'NONE',  ( -27.28573687977896611, 2.255103317860400303, 1.818142657385544148 ) ) ;
#35709 = CARTESIAN_POINT ( 'NONE',  ( 19.43600551875679017, -29.99999999999999645, 5.447264023289953627 ) ) ;
#35710 = LINE ( 'NONE', #15109, #38578 ) ;
#35711 = EDGE_CURVE ( 'NONE', #56844, #64727, #44922, .T. ) ;
#35712 = DIRECTION ( 'NONE',  ( 0.000000000000000000, 0.01356324068817998940, -0.9999080150203989437 ) ) ;
#35713 = CIRCLE ( 'NONE', #10231, 2.899999999999994582 ) ;
#35714 = CARTESIAN_POINT ( 'NONE',  ( -35.00000000000000000, 10.01317267707896441, -6.946017217729827387 ) ) ;
#35715 = VERTEX_POINT ( 'NONE', #34913 ) ;
#35716 =( BOUNDED_SURFACE ( )  B_SPLINE_SURFACE ( 3, 1, ( 
 ( #58990, #12734 ),
 ( #6543, #63945 ),
 ( #13401, #11198 ),
 ( #63282, #41774 ) ),
 .UNSPECIFIED., .F., .F., .F. ) 
 B_SPLINE_SURFACE_WITH_KNOTS ( ( 4, 4 ),
 ( 2, 2 ),
 ( 0.000000000000000000, 1.000000000000000000 ),
 ( 0.000000000000000000, 1.000000000000000000 ),
 .UNSPECIFIED. ) 
 GEOMETRIC_REPRESENTATION_ITEM ( )  RATIONAL_B_SPLINE_SURFACE ( (
 ( 1.000000000000000000, 1.000000000000000000),
 ( 0.6933888150995267674, 0.9895912004443193632),
 ( 0.6933888150995267674, 0.9895912004443193632),
 ( 1.000000000000000000, 1.000000000000000000) ) ) 
 REPRESENTATION_ITEM ( '' )  SURFACE ( )  );
#35717 = ORIENTED_EDGE ( 'NONE', *, *, #22772, .T. ) ;
#35718 = CARTESIAN_POINT ( 'NONE',  ( -23.18047892478189098, -3.933989833240145728, -2.738168160732700862 ) ) ;
#35719 = ORIENTED_EDGE ( 'NONE', *, *, #38840, .T. ) ;
#35720 = EDGE_CURVE ( 'NONE', #53292, #11231, #29949, .T. ) ;
#35721 = ORIENTED_EDGE ( 'NONE', *, *, #24729, .T. ) ;
#35722 = DIRECTION ( 'NONE',  ( 0.000000000000000000, 0.000000000000000000, 1.000000000000000000 ) ) ;
#35723 = CARTESIAN_POINT ( 'NONE',  ( 9.517144231691849754, 7.406568589130381852, -9.443085440640070161 ) ) ;
#35724 = CARTESIAN_POINT ( 'NONE',  ( 0.2648321136542701182, 0.1417061099916467892, -12.24520788540325711 ) ) ;
#35725 = B_SPLINE_CURVE_WITH_KNOTS ( 'NONE', 3,
 ( #62183, #10319, #58184, #6669, #63472, #23254, #26939, #57870, #48544, #12602, #17944, #38206, #58520, #37891, #27578, #12949 ),
 .UNSPECIFIED., .F., .F.,
 ( 4, 3, 3, 3, 3, 4 ),
 ( 1.955623278354240332E-15, 0.0002126834539180125759, 0.0004253519300367125471, 0.0006380165497225470357, 0.0007442707582429773042, 0.0009453531351407216520 ),
 .UNSPECIFIED. ) ;
#35726 = CARTESIAN_POINT ( 'NONE',  ( 0.4613984246114871679, -12.07219521825821751, 2.415907815801364489 ) ) ;
#35727 = CARTESIAN_POINT ( 'NONE',  ( -22.27706485742869091, 0.9832726768967819941, -3.547445275915930285 ) ) ;
#35728 = CARTESIAN_POINT ( 'NONE',  ( -5.440908200706632059, -0.9287346933962611351, -11.96401310621655334 ) ) ;
#35729 = ORIENTED_EDGE ( 'NONE', *, *, #29636, .F. ) ;
#35730 = ORIENTED_EDGE ( 'NONE', *, *, #38364, .F. ) ;
#35731 = DIRECTION ( 'NONE',  ( -1.000000000000000000, 0.000000000000000000, -0.000000000000000000 ) ) ;
#35732 = DIRECTION ( 'NONE',  ( 0.000000000000000000, 0.1118654143051615868, 0.9937233664769762331 ) ) ;
#35733 = LINE ( 'NONE', #42269, #45765 ) ;
#35734 = DIRECTION ( 'NONE',  ( -1.000000000000000000, 0.000000000000000000, -0.000000000000000000 ) ) ;
#35735 = CARTESIAN_POINT ( 'NONE',  ( -22.70624764888619751, -4.591418580540049810, 2.547047087672836163 ) ) ;
#35736 = CARTESIAN_POINT ( 'NONE',  ( 0.000000000000000000, 3.230174184210066191, 5.998318953995321223 ) ) ;
#35737 = CARTESIAN_POINT ( 'NONE',  ( 1.957321625297526957, 1.110016547387106423, -11.94976366055458961 ) ) ;
#35738 = CARTESIAN_POINT ( 'NONE',  ( -27.08419642509983305, -2.181485315953910042, -0.7009209357102740290 ) ) ;
#35739 = ORIENTED_EDGE ( 'NONE', *, *, #20674, .F. ) ;
#35740 = CARTESIAN_POINT ( 'NONE',  ( -27.10719052120871098, 2.116547233941204809, 1.044362304621460069 ) ) ;
#35741 = CARTESIAN_POINT ( 'NONE',  ( 35.00000000000000000, -2.905556151562703082, -11.38112321385050052 ) ) ;
#35742 = DIRECTION ( 'NONE',  ( -1.000000000000000000, 0.000000000000000000, -0.000000000000000000 ) ) ;
#35743 = CIRCLE ( 'NONE', #19826, 5.000000000000000000 ) ;
#35744 = EDGE_CURVE ( 'NONE', #27609, #41185, #37261, .T. ) ;
#35745 = AXIS2_PLACEMENT_3D ( 'NONE', #60245, #64563, #4071 ) ;
#35746 = PLANE ( 'NONE',  #42593 ) ;
#35747 = CARTESIAN_POINT ( 'NONE',  ( 2.844750968616169828, -7.242618984642912316, 2.990088422897453579 ) ) ;
#35748 = ORIENTED_EDGE ( 'NONE', *, *, #1087, .F. ) ;
#35749 = CARTESIAN_POINT ( 'NONE',  ( -17.29080932782789048, -8.561852795175090236, -10.44285877056046452 ) ) ;
#35750 = CARTESIAN_POINT ( 'NONE',  ( 0.3665391374699472626, -12.04754782681758662, 2.392238720110420047 ) ) ;
#35751 = CARTESIAN_POINT ( 'NONE',  ( 2.245754705088394587, 1.216173395688240566, 7.538396044169875410 ) ) ;
#35752 = ORIENTED_EDGE ( 'NONE', *, *, #53472, .F. ) ;
#35753 = CARTESIAN_POINT ( 'NONE',  ( 0.7446945582511163009, -6.508900271375360091, 10.56139717223417840 ) ) ;
#35754 = CARTESIAN_POINT ( 'NONE',  ( -17.89006668746826989, 6.205840224181938147, -10.27317841523973385 ) ) ;
#35755 = FACE_OUTER_BOUND ( 'NONE', #9937, .T. ) ;
#35757 = VERTEX_POINT ( 'NONE', #368 ) ;
#35756 = CARTESIAN_POINT ( 'NONE',  ( 2.373367633546869637, 1.154895193356632488, 7.591069096728999099 ) ) ;
#35758 = DIRECTION ( 'NONE',  ( 1.000000000000000000, 0.000000000000000000, -0.000000000000000000 ) ) ;
#35759 = EDGE_CURVE ( 'NONE', #65068, #53931, #8604, .T. ) ;
#35760 = CARTESIAN_POINT ( 'NONE',  ( 2.524535260912516677, -7.335347545455598528, -2.434550409953180949 ) ) ;
#35761 = ORIENTED_EDGE ( 'NONE', *, *, #32300, .F. ) ;
#35762 = CARTESIAN_POINT ( 'NONE',  ( -35.00000000000000000, -4.561791185930498926, 11.90598845858532151 ) ) ;
#35763 = DIRECTION ( 'NONE',  ( 0.000000000000000000, 0.000000000000000000, 1.000000000000000000 ) ) ;
#35764 = CARTESIAN_POINT ( 'NONE',  ( -27.15525204139121840, -2.440367606305310133, -0.5628609503965597005 ) ) ;
#35765 = CARTESIAN_POINT ( 'NONE',  ( 35.00000000000000000, -9.677500615117850202, 6.657191900728419043 ) ) ;
#35766 = EDGE_CURVE ( 'NONE', #1625, #13124, #18201, .T. ) ;
#35767 = CARTESIAN_POINT ( 'NONE',  ( 0.09505445835107248498, -0.1369421331495652150, -13.50000000000000355 ) ) ;
#35768 = ADVANCED_FACE ( 'NONE', ( #36239 ), #9654, .T. ) ;
#35769 = CARTESIAN_POINT ( 'NONE',  ( -18.36869280200905408, 3.942838040574673464, 12.91355658646968685 ) ) ;
#35770 = CARTESIAN_POINT ( 'NONE',  ( 0.3654063281920754136, 11.44627072062585071, -4.446369912832391691 ) ) ;
#35771 = ADVANCED_FACE ( 'NONE', ( #46250 ), #60533, .T. ) ;
#35772 = ORIENTED_EDGE ( 'NONE', *, *, #42650, .F. ) ;
#35773 = CARTESIAN_POINT ( 'NONE',  ( 35.00000000000000000, -9.752226076388938125, -6.547236723513990775 ) ) ;
#35774 = VERTEX_POINT ( 'NONE', #14634 ) ;
#35775 = PRESENTATION_STYLE_ASSIGNMENT (( #45780 ) ) ;
#35776 = DIRECTION ( 'NONE',  ( -1.000000000000000000, 0.000000000000000000, 0.000000000000000000 ) ) ;
#35777 = CARTESIAN_POINT ( 'NONE',  ( 0.3106921474978435183, 11.43920276778357348, 4.414111574791866666 ) ) ;
#35778 = EDGE_CURVE ( 'NONE', #20776, #12091, #48971, .T. ) ;
#35779 = CARTESIAN_POINT ( 'NONE',  ( -37.00000000000000711, 10.75351884295727700, -4.725891942574793170 ) ) ;
#35780 = EDGE_LOOP ( 'NONE', ( #22768, #4905, #59184, #24002 ) ) ;
#35781 = CARTESIAN_POINT ( 'NONE',  ( -22.28506771379528573, -0.8783543640076993952, 3.622079238249907629 ) ) ;
#35782 = FACE_OUTER_BOUND ( 'NONE', #41366, .T. ) ;
#35784 = EDGE_CURVE ( 'NONE', #44220, #59359, #19504, .T. ) ;
#35783 = CARTESIAN_POINT ( 'NONE',  ( -22.27721038036499834, -1.315315479297498369, 3.438655654856794364 ) ) ;
#35785 = ORIENTED_EDGE ( 'NONE', *, *, #6903, .F. ) ;
#35786 = ORIENTED_EDGE ( 'NONE', *, *, #24455, .T. ) ;
#35787 = DIRECTION ( 'NONE',  ( 0.000000000000000000, 0.000000000000000000, 1.000000000000000000 ) ) ;
#35788 = ORIENTED_EDGE ( 'NONE', *, *, #57958, .T. ) ;
#35789 = DIRECTION ( 'NONE',  ( 0.000000000000000000, 0.000000000000000000, 1.000000000000000000 ) ) ;
#35790 = VECTOR ( 'NONE', #4017, 1000.000000000000000 ) ;
#35791 = CARTESIAN_POINT ( 'NONE',  ( 1.452237505248555660, 4.880303821311009926, 11.67686475128081369 ) ) ;
#35792 = FACE_OUTER_BOUND ( 'NONE', #4437, .T. ) ;
#35793 = CARTESIAN_POINT ( 'NONE',  ( -29.54875962971174630, 0.3031974620720156444, 12.00375708844796030 ) ) ;
#35794 = DIRECTION ( 'NONE',  ( -1.000000000000000000, -0.000000000000000000, -0.000000000000000000 ) ) ;
#35795 = CARTESIAN_POINT ( 'NONE',  ( 2.000000000000001776, 7.387287142779349836, 1.295372019972174549 ) ) ;
#35796 = AXIS2_PLACEMENT_3D ( 'NONE', #9139, #25419, #39734 ) ;
#35797 = ADVANCED_FACE ( 'NONE', ( #55888 ), #30594, .T. ) ;
#35798 = CARTESIAN_POINT ( 'NONE',  ( -22.31328051695926007, -1.076152733467184985, -3.633840107626963967 ) ) ;
#35799 = EDGE_LOOP ( 'NONE', ( #3709, #60319, #3984, #4681 ) ) ;
#35800 = CARTESIAN_POINT ( 'NONE',  ( -37.00000000000000711, -2.544412758415929066, 11.91791701451265340 ) ) ;
#35801 = CARTESIAN_POINT ( 'NONE',  ( 24.44951845548068547, 9.131659704386734688, -7.789979626095448140 ) ) ;
#35802 = CARTESIAN_POINT ( 'NONE',  ( 5.516018279890452902, 0.005976902763919037485, -0.003191189039764858598 ) ) ;
#35803 = CARTESIAN_POINT ( 'NONE',  ( 12.53742808369427131, 13.03983582561033927, -3.499595080473846487 ) ) ;
#35804 = CARTESIAN_POINT ( 'NONE',  ( -37.00000000000000711, 10.49626516989271074, 7.238157050195668241 ) ) ;
#35805 = CARTESIAN_POINT ( 'NONE',  ( 0.3675815128205912052, -11.44679196252412368, 4.447030445008141264 ) ) ;
#35806 = CARTESIAN_POINT ( 'NONE',  ( 3.152665057734119536, 7.281573230474295499, 3.161213418913482620 ) ) ;
#35807 = CARTESIAN_POINT ( 'NONE',  ( 37.00000000000000711, 8.534258022646096009, -8.699265615723016154 ) ) ;
#35808 = ORIENTED_EDGE ( 'NONE', *, *, #31161, .T. ) ;
#35809 = DIRECTION ( 'NONE',  ( -1.000000000000000000, 0.000000000000000000, 0.000000000000000000 ) ) ;
#35810 = ORIENTED_EDGE ( 'NONE', *, *, #53963, .T. ) ;
#35811 = CARTESIAN_POINT ( 'NONE',  ( 5.514970785353741078, -0.003929719953530088142, 0.002619824551223746099 ) ) ;
#35812 = CARTESIAN_POINT ( 'NONE',  ( 5.514624014163232779, -0.0008859786816842371007, 0.004045310349816136873 ) ) ;
#35813 = CARTESIAN_POINT ( 'NONE',  ( 0.2653519991613830786, -12.06397323649777320, 2.104847849998821907 ) ) ;
#35814 = CARTESIAN_POINT ( 'NONE',  ( 0.3665391374699467075, -5.911453292029529294, -10.76665847464319015 ) ) ;
#35815 = VERTEX_POINT ( 'NONE', #63163 ) ;
#35816 = DIRECTION ( 'NONE',  ( -1.000000000000000000, 0.000000000000000000, 0.000000000000000000 ) ) ;
#35817 = CARTESIAN_POINT ( 'NONE',  ( -30.07590672654234254, -2.992774906073117247, -11.62765303320213128 ) ) ;
#35818 = CARTESIAN_POINT ( 'NONE',  ( 25.00000000000000355, -3.797884998337192286, 23.99999999999999289 ) ) ;
#35819 = CARTESIAN_POINT ( 'NONE',  ( -22.27719381268171617, 2.588413841766863843, 2.618044180756106343 ) ) ;
#35820 = EDGE_CURVE ( 'NONE', #47279, #38770, #51097, .T. ) ;
#35821 = CARTESIAN_POINT ( 'NONE',  ( 29.36289517528272697, -4.666195979332560917, 11.05608984446922527 ) ) ;
#35822 = CARTESIAN_POINT ( 'NONE',  ( -27.35552965826137140, 1.773915698030573473, -2.548625910254528559 ) ) ;
#35823 = CIRCLE ( 'NONE', #47685, 12.75000000000000178 ) ;
#35824 = EDGE_CURVE ( 'NONE', #28364, #42839, #59585, .T. ) ;
#35825 = EDGE_LOOP ( 'NONE', ( #8659, #63510, #49936, #16870 ) ) ;
#35826 = CARTESIAN_POINT ( 'NONE',  ( -27.10307689719148883, -0.5470785519251840645, 2.283215755733933428 ) ) ;
#35827 = EDGE_LOOP ( 'NONE', ( #20616, #49816, #42224, #62440, #49943, #39901 ) ) ;
#35828 = CARTESIAN_POINT ( 'NONE',  ( 0.2801149460245144773, -0.1962575296604573138, -12.24954625471156255 ) ) ;
#35829 = CARTESIAN_POINT ( 'NONE',  ( 2.241352910868908310, 7.202080440908741998, 2.532612177304466972 ) ) ;
#35830 = EDGE_CURVE ( 'NONE', #53824, #32797, #1016, .T. ) ;
#35831 = CIRCLE ( 'NONE', #59237, 6.936499999999990784 ) ;
#35832 = CARTESIAN_POINT ( 'NONE',  ( 29.23591692263869390, -7.592124157161351583, 9.304424942147701216 ) ) ;
#35833 = CARTESIAN_POINT ( 'NONE',  ( -9.211673578334142576, -3.291588394019901553, 11.54079650380478483 ) ) ;
#35834 = ADVANCED_FACE ( 'NONE', ( #17290 ), #6334, .T. ) ;
#35835 = ORIENTED_EDGE ( 'NONE', *, *, #57035, .T. ) ;
#35836 = CIRCLE ( 'NONE', #15676, 5.000000000000000000 ) ;
#35837 = ORIENTED_EDGE ( 'NONE', *, *, #28570, .F. ) ;
#35838 = CARTESIAN_POINT ( 'NONE',  ( 5.514624014163232779, -0.003278974416024624076, 0.002529391395135295768 ) ) ;
#35839 = ORIENTED_EDGE ( 'NONE', *, *, #61850, .T. ) ;
#35840 = FACE_OUTER_BOUND ( 'NONE', #28944, .T. ) ;
#35841 = CARTESIAN_POINT ( 'NONE',  ( 2.941278708680199916, -3.842273877444530417, -4.788765081995669526 ) ) ;
#35842 = CARTESIAN_POINT ( 'NONE',  ( 0.3665391374699467075, 10.50279796150436873, 6.368473106897165614 ) ) ;
#35843 = CARTESIAN_POINT ( 'NONE',  ( 9.687175622948608122, -13.48729812737142986, -0.5854820436212360146 ) ) ;
#35844 = CARTESIAN_POINT ( 'NONE',  ( 35.00000000000000000, 4.705694406421931860E-17, -3.469127814946512892E-15 ) ) ;
#35845 = ADVANCED_FACE ( 'NONE', ( #47549 ), #26280, .T. ) ;
#35846 = DIRECTION ( 'NONE',  ( 1.000000000000000000, 0.000000000000000000, 0.000000000000000000 ) ) ;
#35847 = FACE_OUTER_BOUND ( 'NONE', #57664, .T. ) ;
#35848 = ORIENTED_EDGE ( 'NONE', *, *, #56293, .F. ) ;
#35849 = EDGE_CURVE ( 'NONE', #64706, #45642, #17846, .T. ) ;
#35850 = DIRECTION ( 'NONE',  ( 1.000000000000000000, -0.000000000000000000, 0.000000000000000000 ) ) ;
#35851 = ORIENTED_EDGE ( 'NONE', *, *, #31753, .T. ) ;
#35852 = CARTESIAN_POINT ( 'NONE',  ( -22.27715239060371744, 2.513478159995859773, 2.689999469426664014 ) ) ;
#35853 = CARTESIAN_POINT ( 'NONE',  ( 0.3675815128205894289, 10.50067073900651771, 6.367184624550202621 ) ) ;
#35854 = CARTESIAN_POINT ( 'NONE',  ( 47.00000000000000711, 4.705694406421931860E-17, -3.469127814946512892E-15 ) ) ;
#35855 = ORIENTED_EDGE ( 'NONE', *, *, #12359, .F. ) ;
#35856 = CARTESIAN_POINT ( 'NONE',  ( 2.000000000000001776, -6.539067737394505642, 2.314222412769772586 ) ) ;
#35857 = ORIENTED_EDGE ( 'NONE', *, *, #4528, .T. ) ;
#35858 = CARTESIAN_POINT ( 'NONE',  ( -35.00000000000000000, -3.614449339633411196, -11.17622378668010441 ) ) ;
#35859 = CARTESIAN_POINT ( 'NONE',  ( 4.496966607327446575, -10.17674880801902404, -8.871149476859031324 ) ) ;
#35861 = ADVANCED_FACE ( 'NONE', ( #42199 ), #57869, .T. ) ;
#35860 = CARTESIAN_POINT ( 'NONE',  ( 35.00000000000000000, 9.896810808925392777, -7.110831038798317572 ) ) ;
#35862 = CARTESIAN_POINT ( 'NONE',  ( 7.302528884010846433, -6.186995576375307060, 10.28474183025580047 ) ) ;
#35863 = ORIENTED_EDGE ( 'NONE', *, *, #5223, .F. ) ;
#35864 = ORIENTED_EDGE ( 'NONE', *, *, #56963, .T. ) ;
#35865 = LINE ( 'NONE', #5661, #33193 ) ;
#35867 = ORIENTED_EDGE ( 'NONE', *, *, #53503, .T. ) ;
#35866 = EDGE_CURVE ( 'NONE', #49268, #46786, #16326, .T. ) ;
#35868 = CARTESIAN_POINT ( 'NONE',  ( 0.7400311444011690165, -11.77295732453931976, -3.907401494355040139 ) ) ;
#35869 = ORIENTED_EDGE ( 'NONE', *, *, #42942, .F. ) ;
#35870 = EDGE_LOOP ( 'NONE', ( #10439, #16451, #34825, #17848 ) ) ;
#35872 = EDGE_CURVE ( 'NONE', #36323, #64793, #27577, .T. ) ;
#35871 = ORIENTED_EDGE ( 'NONE', *, *, #46187, .F. ) ;
#35873 = DIRECTION ( 'NONE',  ( -1.000000000000000000, 0.000000000000000000, -0.000000000000000000 ) ) ;
#35875 = CIRCLE ( 'NONE', #50758, 5.000000000000000000 ) ;
#35874 = CARTESIAN_POINT ( 'NONE',  ( 1.634816307074477892, 11.67158647524040660, 5.013416918607531692 ) ) ;
#35876 = CARTESIAN_POINT ( 'NONE',  ( 0.2646305136544072623, -4.312539723326208829, 11.46223899740598817 ) ) ;
#35877 = CARTESIAN_POINT ( 'NONE',  ( 2.261269890822072526, 2.744033622443712961, -7.131324074141551783 ) ) ;
#35878 = CARTESIAN_POINT ( 'NONE',  ( -35.00000000000000000, 11.66953048682404415, -3.511814412391998541 ) ) ;
#35879 = VERTEX_POINT ( 'NONE', #16954 ) ;
#35880 = EDGE_CURVE ( 'NONE', #38116, #886, #24549, .T. ) ;
#35881 = EDGE_CURVE ( 'NONE', #42619, #21169, #33042, .T. ) ;
#35882 = DIRECTION ( 'NONE',  ( -0.7738190875236917732, 0.000000000000000000, 0.6334066780386838902 ) ) ;
#35883 = CIRCLE ( 'NONE', #56064, 12.18649999999999878 ) ;
#35884 = EDGE_LOOP ( 'NONE', ( #60794, #62635, #33546, #15173 ) ) ;
#35885 = CARTESIAN_POINT ( 'NONE',  ( -35.00000000000000000, 11.59095880812008161, -1.903127969211228621 ) ) ;
#35886 = CARTESIAN_POINT ( 'NONE',  ( -37.00000000000000711, 0.000000000000000000, 0.000000000000000000 ) ) ;
#35887 = ADVANCED_FACE ( 'NONE', ( #32881 ), #27365, .F. ) ;
#35888 = CIRCLE ( 'NONE', #62420, 5.000000000000000888 ) ;
#35889 = CARTESIAN_POINT ( 'NONE',  ( 0.2646305136544065406, -7.972778379581487940, -9.296005949277303060 ) ) ;
#35890 = CARTESIAN_POINT ( 'NONE',  ( -27.72177753345763307, 12.14326761761198092, -5.905282218285447193 ) ) ;
#35891 = DIRECTION ( 'NONE',  ( 1.000000000000000000, 0.000000000000000000, 0.000000000000000000 ) ) ;
#35892 = CARTESIAN_POINT ( 'NONE',  ( 2.770579946183332698, -7.804957730865690557, -0.3031629740256557293 ) ) ;
#35893 = AXIS2_PLACEMENT_3D ( 'NONE', #27906, #48216, #7624 ) ;
#35894 = ORIENTED_EDGE ( 'NONE', *, *, #40975, .F. ) ;
#35895 = CYLINDRICAL_SURFACE ( 'NONE', #3593, 6.936499999999988120 ) ;
#35896 =( BOUNDED_SURFACE ( )  B_SPLINE_SURFACE ( 3, 1, ( 
 ( #43672, #7790 ),
 ( #8771, #38702 ),
 ( #44019, #3811 ),
 ( #38357, #29056 ) ),
 .UNSPECIFIED., .F., .F., .F. ) 
 B_SPLINE_SURFACE_WITH_KNOTS ( ( 4, 4 ),
 ( 2, 2 ),
 ( 0.000000000000000000, 1.000000000000000000 ),
 ( 0.000000000000000000, 1.000000000000000000 ),
 .UNSPECIFIED. ) 
 GEOMETRIC_REPRESENTATION_ITEM ( )  RATIONAL_B_SPLINE_SURFACE ( (
 ( 1.000000000000000000, 1.000000000000000000),
 ( 0.9856612449720755231, 0.9999558406602322425),
 ( 0.9856612449720755231, 0.9999558406602322425),
 ( 1.000000000000000000, 1.000000000000000000) ) ) 
 REPRESENTATION_ITEM ( '' )  SURFACE ( )  );
#35897 = EDGE_LOOP ( 'NONE', ( #584, #60182, #41033, #8319 ) ) ;
#35898 = CARTESIAN_POINT ( 'NONE',  ( -24.29429707091690815, -10.54430068311935464, 8.439581701646471146 ) ) ;
#35899 = DIRECTION ( 'NONE',  ( 0.000000000000000000, 0.4134677391718450945, 0.9105187689795982697 ) ) ;
#35900 = CARTESIAN_POINT ( 'NONE',  ( -1.009501604528838081, -26.56249173023641674, 16.21092882686939518 ) ) ;
#35901 = CARTESIAN_POINT ( 'NONE',  ( 2.262775599885880062, -3.697834000591908143, -6.687241191563379594 ) ) ;
#35902 = CARTESIAN_POINT ( 'NONE',  ( 2.241352910868908754, 7.503490710578232914, 1.407733736974891681 ) ) ;
#35903 = ORIENTED_EDGE ( 'NONE', *, *, #50243, .F. ) ;
#35904 = DIRECTION ( 'NONE',  ( 1.000000000000000000, -0.000000000000000000, 0.000000000000000000 ) ) ;
#35905 = DIRECTION ( 'NONE',  ( -1.000000000000000000, 0.000000000000000000, 0.000000000000000000 ) ) ;
#35906 = CARTESIAN_POINT ( 'NONE',  ( 21.90174657591892071, 11.97747433400151884, -0.7349207973210698519 ) ) ;
#35907 = CARTESIAN_POINT ( 'NONE',  ( 2.963017218115618245, 3.599595431209491991, 7.004145770368786827 ) ) ;
#35908 = EDGE_CURVE ( 'NONE', #42345, #15993, #63890, .T. ) ;
#35909 = DIRECTION ( 'NONE',  ( -1.000000000000000000, 0.000000000000000000, 0.000000000000000000 ) ) ;
#35910 = AXIS2_PLACEMENT_3D ( 'NONE', #64664, #39410, #59708 ) ;
#35911 = FACE_OUTER_BOUND ( 'NONE', #32666, .T. ) ;
#35912 = CARTESIAN_POINT ( 'NONE',  ( -35.04643116707788408, 0.001845126042312322800, 0.01204777744935429939 ) ) ;
#35913 = CARTESIAN_POINT ( 'NONE',  ( 2.903928887688530303, -0.9983813550131019898, 8.712847781148955306 ) ) ;
#35914 = CARTESIAN_POINT ( 'NONE',  ( 37.00000000000000711, 11.86701198550356295, -2.772148766916162632 ) ) ;
#35915 = EDGE_CURVE ( 'NONE', #34835, #59884, #61755, .T. ) ;
#35916 = AXIS2_PLACEMENT_3D ( 'NONE', #12926, #58495, #58843 ) ;
#35917 = VERTEX_POINT ( 'NONE', #58867 ) ;
#35918 = CIRCLE ( 'NONE', #13627, 5.000000000000000000 ) ;
#35919 = CIRCLE ( 'NONE', #7275, 12.74999999999999822 ) ;
#35920 = ORIENTED_EDGE ( 'NONE', *, *, #54291, .T. ) ;
#35921 = DIRECTION ( 'NONE',  ( -1.000000000000000000, 0.000000000000000000, -0.000000000000000000 ) ) ;
#35922 = CARTESIAN_POINT ( 'NONE',  ( 0.2638984909335720941, -9.508791614589142682, -7.718810690099158656 ) ) ;
#35923 = CARTESIAN_POINT ( 'NONE',  ( 35.00000000000000000, 8.927548052240892318, -8.295159312811890118 ) ) ;
#35924 = AXIS2_PLACEMENT_3D ( 'NONE', #42185, #41211, #51875 ) ;
#35925 = CARTESIAN_POINT ( 'NONE',  ( 0.2739690278137235091, -1.946552041162990410, 12.09341522051409612 ) ) ;
#35926 = ORIENTED_EDGE ( 'NONE', *, *, #34216, .T. ) ;
#35927 = EDGE_CURVE ( 'NONE', #8838, #5064, #1255, .T. ) ;
#35928 = ORIENTED_EDGE ( 'NONE', *, *, #18085, .F. ) ;
#35929 = AXIS2_PLACEMENT_3D ( 'NONE', #29443, #59386, #7880 ) ;
#35930 = ORIENTED_EDGE ( 'NONE', *, *, #20655, .F. ) ;
#35931 = CARTESIAN_POINT ( 'NONE',  ( 29.51976981715666781, -4.571419055710073565, 11.09513982864076276 ) ) ;
#35932 = CARTESIAN_POINT ( 'NONE',  ( -22.27720412283625961, 0.7407051501189994003, 3.606406551442356001 ) ) ;
#35933 = ORIENTED_EDGE ( 'NONE', *, *, #53920, .T. ) ;
#35934 = CYLINDRICAL_SURFACE ( 'NONE', #34704, 4.999999999999999112 ) ;
#35935 = DIRECTION ( 'NONE',  ( 1.000000000000000000, -0.000000000000000000, -0.000000000000000000 ) ) ;
#35936 = ORIENTED_EDGE ( 'NONE', *, *, #3982, .T. ) ;
#35937 = CARTESIAN_POINT ( 'NONE',  ( -22.28023996335807411, 0.3233044107360884545, 3.676538434326150906 ) ) ;
#35938 = CARTESIAN_POINT ( 'NONE',  ( 11.12775972613913211, -27.93149659178525823, -13.86083901436714427 ) ) ;
#35939 = CARTESIAN_POINT ( 'NONE',  ( 5.515188684475870851, 0.005194992164431481291, 0.001283816547384742691 ) ) ;
#35940 = ORIENTED_EDGE ( 'NONE', *, *, #35481, .F. ) ;
#35941 = CARTESIAN_POINT ( 'NONE',  ( 36.00000000000000711, -12.16893194857552629, -3.805206332242430101 ) ) ;
#35942 = VERTEX_POINT ( 'NONE', #18624 ) ;
#35943 = CARTESIAN_POINT ( 'NONE',  ( 35.00000000000000000, 6.265926637539650734, 11.10408318471052347 ) ) ;
#35944 = VERTEX_POINT ( 'NONE', #2681 ) ;
#35945 = DIRECTION ( 'NONE',  ( -0.9582930651793754029, -0.08045274594386239708, -0.2742293873734352738 ) ) ;
#35946 = EDGE_CURVE ( 'NONE', #45709, #36827, #25641, .T. ) ;
#35947 = DIRECTION ( 'NONE',  ( 0.000000000000000000, 0.01356324068817998940, -0.9999080150203990547 ) ) ;
#35948 = DIRECTION ( 'NONE',  ( -1.000000000000000000, 0.000000000000000000, 0.000000000000000000 ) ) ;
#35949 = CARTESIAN_POINT ( 'NONE',  ( 22.57855258442565116, 3.026812727784649493, 11.61199400236328749 ) ) ;
#35951 = DIRECTION ( 'NONE',  ( -1.000000000000000000, 0.000000000000000000, 0.000000000000000000 ) ) ;
#35950 = VECTOR ( 'NONE', #59901, 1000.000000000000000 ) ;
#35952 = B_SPLINE_CURVE_WITH_KNOTS ( 'NONE', 3,
 ( #29233, #64151, #39521, #50175, #34534, #49529, #18627 ),
 .UNSPECIFIED., .F., .F.,
 ( 4, 3, 4 ),
 ( 0.000000000000000000, 0.001700533616330558153, 0.005002426799371352019 ),
 .UNSPECIFIED. ) ;
#35953 = DIRECTION ( 'NONE',  ( 1.000000000000000000, 0.000000000000000000, 0.000000000000000000 ) ) ;
#35954 = LINE ( 'NONE', #30989, #19761 ) ;
#35955 = FACE_OUTER_BOUND ( 'NONE', #8730, .T. ) ;
#35957 = ORIENTED_EDGE ( 'NONE', *, *, #19492, .F. ) ;
#35956 = LINE ( 'NONE', #56257, #38452 ) ;
#35958 = EDGE_CURVE ( 'NONE', #5651, #32797, #50323, .T. ) ;
#35959 = CARTESIAN_POINT ( 'NONE',  ( 2.177405672432779049, 10.73538068360231534, 3.189307221896654720 ) ) ;
#35960 = ORIENTED_EDGE ( 'NONE', *, *, #58418, .T. ) ;
#35961 = VECTOR ( 'NONE', #60605, 1000.000000000000000 ) ;
#35962 = CARTESIAN_POINT ( 'NONE',  ( 0.000000000000000000, 0.000000000000000000, 0.000000000000000000 ) ) ;
#35963 = ORIENTED_EDGE ( 'NONE', *, *, #4440, .F. ) ;
#35964 = DIRECTION ( 'NONE',  ( -1.000000000000000000, 0.000000000000000000, 0.000000000000000000 ) ) ;
#35965 = EDGE_CURVE ( 'NONE', #49980, #26098, #7982, .T. ) ;
#35966 = ORIENTED_EDGE ( 'NONE', *, *, #13736, .T. ) ;
#35967 = CARTESIAN_POINT ( 'NONE',  ( 0.2767916011545372701, 8.018602152763861568, 9.260929738915262277 ) ) ;
#35968 = CARTESIAN_POINT ( 'NONE',  ( -35.00000000000000000, 0.000000000000000000, 0.000000000000000000 ) ) ;
#35969 = CARTESIAN_POINT ( 'NONE',  ( -27.09342121492585420, -2.227768580955212574, 0.6436068655225369861 ) ) ;
#35970 = CARTESIAN_POINT ( 'NONE',  ( 47.00000000000000711, 4.705694406421931860E-17, -3.469127814946512892E-15 ) ) ;
#35971 = CIRCLE ( 'NONE', #59344, 5.000000000000000000 ) ;
#35972 = DIRECTION ( 'NONE',  ( 0.000000000000000000, 0.000000000000000000, 1.000000000000000000 ) ) ;
#35973 = ORIENTED_EDGE ( 'NONE', *, *, #62828, .F. ) ;
#35974 = DIRECTION ( 'NONE',  ( 1.000000000000000000, 0.000000000000000000, 0.000000000000000000 ) ) ;
#35975 = CIRCLE ( 'NONE', #922, 12.18649999999999878 ) ;
#35976 = ORIENTED_EDGE ( 'NONE', *, *, #1218, .T. ) ;
#35977 = CARTESIAN_POINT ( 'NONE',  ( 9.575800908719084958, -13.45729701195359240, -1.072919909436246266 ) ) ;
#35978 = FACE_OUTER_BOUND ( 'NONE', #16510, .T. ) ;
#35979 = AXIS2_PLACEMENT_3D ( 'NONE', #5928, #27163, #26184 ) ;
#35980 = CYLINDRICAL_SURFACE ( 'NONE', #36030, 5.000000000000000888 ) ;
#35981 = VERTEX_POINT ( 'NONE', #8947 ) ;
#35982 = LINE ( 'NONE', #15704, #62697 ) ;
#35983 = EDGE_CURVE ( 'NONE', #25281, #19321, #63800, .T. ) ;
#35984 = EDGE_CURVE ( 'NONE', #64903, #19934, #42608, .T. ) ;
#35985 = CARTESIAN_POINT ( 'NONE',  ( -29.92777678363736626, -3.750539801530011985, 12.96855624952674724 ) ) ;
#35986 = CARTESIAN_POINT ( 'NONE',  ( 35.00000000000000000, 4.705694406421931860E-17, -3.469127814946512892E-15 ) ) ;
#35987 = CARTESIAN_POINT ( 'NONE',  ( -37.00000000000000711, -0.9416912585473466990, -12.71517666308949046 ) ) ;
#35988 = DIRECTION ( 'NONE',  ( -1.000000000000000000, 0.000000000000000000, 0.000000000000000000 ) ) ;
#35989 = VERTEX_POINT ( 'NONE', #23253 ) ;
#35990 = CARTESIAN_POINT ( 'NONE',  ( -35.00000000000000000, 0.000000000000000000, 0.000000000000000000 ) ) ;
#35991 = DIRECTION ( 'NONE',  ( -1.000000000000000000, -0.000000000000000000, 0.000000000000000000 ) ) ;
#35992 = CARTESIAN_POINT ( 'NONE',  ( -35.00000000000000000, 10.32377448871677039, -6.475373545682193033 ) ) ;
#35993 = ADVANCED_FACE ( 'NONE', ( #38548 ), #8293, .T. ) ;
#35994 = CARTESIAN_POINT ( 'NONE',  ( -14.51082951660905529, 7.864361836847419518, 10.97323765135710261 ) ) ;
#35995 = CARTESIAN_POINT ( 'NONE',  ( 19.09840580349259298, -7.043236883969886897, 11.53925104275845470 ) ) ;
#35996 = ORIENTED_EDGE ( 'NONE', *, *, #25355, .F. ) ;
#35997 = CIRCLE ( 'NONE', #55151, 2.899999999999996358 ) ;
#35998 = DIRECTION ( 'NONE',  ( -1.000000000000000000, 0.000000000000000000, 0.000000000000000000 ) ) ;
#35999 = DIRECTION ( 'NONE',  ( 1.000000000000000000, 0.000000000000000000, 0.000000000000000000 ) ) ;
#36000 = CARTESIAN_POINT ( 'NONE',  ( -22.27756824490284515, 3.558840239148769236, -0.9472004376381198965 ) ) ;
#36001 = ORIENTED_EDGE ( 'NONE', *, *, #51205, .T. ) ;
#36002 = CARTESIAN_POINT ( 'NONE',  ( -35.00000000000000000, -9.321877890560388735, -7.146664589318012517 ) ) ;
#36003 = DIRECTION ( 'NONE',  ( 1.000000000000000000, 0.000000000000000000, 0.000000000000000000 ) ) ;
#36004 = ORIENTED_EDGE ( 'NONE', *, *, #54965, .T. ) ;
#36005 = EDGE_CURVE ( 'NONE', #13243, #15906, #9736, .T. ) ;
#36006 = EDGE_CURVE ( 'NONE', #48006, #54727, #53278, .T. ) ;
#36007 = VERTEX_POINT ( 'NONE', #4945 ) ;
#36008 = ORIENTED_EDGE ( 'NONE', *, *, #7972, .T. ) ;
#36009 = EDGE_CURVE ( 'NONE', #6304, #50524, #44753, .T. ) ;
#36010 = CIRCLE ( 'NONE', #46630, 12.18649999999999878 ) ;
#36011 = CARTESIAN_POINT ( 'NONE',  ( -27.08421723179412410, -1.681635392574622800, 1.556274442127711044 ) ) ;
#36012 = ORIENTED_EDGE ( 'NONE', *, *, #25289, .T. ) ;
#36013 = CARTESIAN_POINT ( 'NONE',  ( -25.00000000000000355, -9.999999999999998224, 1.530808498934191521E-15 ) ) ;
#36014 = CARTESIAN_POINT ( 'NONE',  ( 1.549075743846070496, -11.66216484053767921, -4.962709020480940758 ) ) ;
#36015 = AXIS2_PLACEMENT_3D ( 'NONE', #29241, #49221, #18634 ) ;
#36016 = DIRECTION ( 'NONE',  ( 0.000000000000000000, -0.01356324068817991828, 0.9999080150203990547 ) ) ;
#36017 = CARTESIAN_POINT ( 'NONE',  ( 0.9232167919969108683, -0.4134278310082157293, -12.45862789703290829 ) ) ;
#36018 = VERTEX_POINT ( 'NONE', #19896 ) ;
#36019 = CARTESIAN_POINT ( 'NONE',  ( 0.3665391374699464300, 3.952034409876296284, 11.62960183138728354 ) ) ;
#36021 = B_SPLINE_CURVE_WITH_KNOTS ( 'NONE', 3,
 ( #49759, #50096, #51080, #542, #45100, #24477, #15151, #19509, #25802, #20147, #19829, #40088, #29779, #35437, #41075, #20483, #46095, #65035, #60067, #4551, #65364, #60377, #25141, #20807, #14803, #35089 ),
 .UNSPECIFIED., .F., .F.,
 ( 4, 2, 2, 2, 2, 2, 2, 2, 2, 2, 2, 2, 4 ),
 ( 0.000000000000000000, 0.002619749957742739058, 0.003929624936614107070, 0.005239499915485476382, 0.006549374894356846562, 0.007859249873228217609, 0.01047899983097095103, 0.01309874978871368618, 0.01440862476758505810, 0.01571849974645642828, 0.01833824970419916517, 0.01964812468307053708, 0.02095799966194190206 ),
 .UNSPECIFIED. ) ;
#36020 = CARTESIAN_POINT ( 'NONE',  ( -17.03240540343445630, -28.50880493221823286, 9.306303259374256953 ) ) ;
#36022 = CARTESIAN_POINT ( 'NONE',  ( 0.2648978790185602672, -4.063980959785125080, 11.55204314799262555 ) ) ;
#36024 = EDGE_LOOP ( 'NONE', ( #50668, #37000, #12965, #54704 ) ) ;
#36023 = CARTESIAN_POINT ( 'NONE',  ( 0.2638984909335720941, 8.023974293733179053, 9.252728947331103626 ) ) ;
#36025 = CARTESIAN_POINT ( 'NONE',  ( 35.00000000000000000, -2.905556151562703082, -11.38112321385050052 ) ) ;
#36026 = B_SPLINE_CURVE_WITH_KNOTS ( 'NONE', 3,
 ( #23888, #9211, #4246, #64417, #3624, #44152, #28211, #8904, #18239, #18889, #63435, #17903, #53815, #23217, #48830, #43478, #33188, #43825, #13244, #14206, #44455, #34492 ),
 .UNSPECIFIED., .F., .F.,
 ( 4, 3, 3, 3, 3, 3, 3, 4 ),
 ( 8.940560153363745023E-19, 4.449119708436590826E-05, 6.626296329540418823E-05, 8.803456484962658983E-05, 0.0001098060367612806366, 0.0001315774408628531860, 0.0001760698110411187023, 0.0001829697163287827787 ),
 .UNSPECIFIED. ) ;
#36027 = ORIENTED_EDGE ( 'NONE', *, *, #27240, .F. ) ;
#36028 = CARTESIAN_POINT ( 'NONE',  ( 35.00000000000000000, -1.738225594540085517, -12.63095688309028475 ) ) ;
#36029 = ORIENTED_EDGE ( 'NONE', *, *, #21794, .T. ) ;
#36030 = AXIS2_PLACEMENT_3D ( 'NONE', #49997, #34992, #65281 ) ;
#36031 = EDGE_LOOP ( 'NONE', ( #29899, #50852, #18955, #6648 ) ) ;
#36032 = DIRECTION ( 'NONE',  ( 0.000000000000000000, -0.9847383929261599445, 0.1740410799127720953 ) ) ;
#36033 = CARTESIAN_POINT ( 'NONE',  ( 7.125164966885773055, -31.43290117443686071, 14.16047883281854425 ) ) ;
#36034 = ADVANCED_FACE ( 'NONE', ( #25880 ), #285, .F. ) ;
#36035 = CYLINDRICAL_SURFACE ( 'NONE', #63013, 12.18650000000000055 ) ;
#36036 = ORIENTED_EDGE ( 'NONE', *, *, #25299, .T. ) ;
#36037 = FACE_OUTER_BOUND ( 'NONE', #51952, .T. ) ;
#36038 = DIRECTION ( 'NONE',  ( 1.000000000000000000, -0.000000000000000000, 0.000000000000000000 ) ) ;
#36039 = CARTESIAN_POINT ( 'NONE',  ( 0.000000000000000000, 2.473437528934240515, -7.080403010454960011 ) ) ;
#36040 = ORIENTED_EDGE ( 'NONE', *, *, #9151, .F. ) ;
#36041 = EDGE_CURVE ( 'NONE', #28445, #30406, #60714, .T. ) ;
#36042 = ORIENTED_EDGE ( 'NONE', *, *, #54503, .F. ) ;
#36043 = CARTESIAN_POINT ( 'NONE',  ( 0.3278977287071221380, 12.03512402322223274, 2.374069413450185184 ) ) ;
#36044 = ORIENTED_EDGE ( 'NONE', *, *, #41482, .F. ) ;
#36045 = ORIENTED_EDGE ( 'NONE', *, *, #54316, .T. ) ;
#36046 = CARTESIAN_POINT ( 'NONE',  ( 5.520433897694421610, 0.01473594271720232718, 0.003119431460922271037 ) ) ;
#36047 = FACE_OUTER_BOUND ( 'NONE', #28764, .T. ) ;
#36048 = CARTESIAN_POINT ( 'NONE',  ( -22.28169757117798966, 0.9284931499057414994, -3.576542310004389602 ) ) ;
#36049 = CARTESIAN_POINT ( 'NONE',  ( 17.41946928281426921, -8.203725127357042624, 8.773628054256990438 ) ) ;
#36050 = CARTESIAN_POINT ( 'NONE',  ( -22.27706485742869091, 1.508175983031630585, -3.358064672837109743 ) ) ;
#36051 = DIRECTION ( 'NONE',  ( 0.000000000000000000, 0.01356324068817998940, -0.9999080150203989437 ) ) ;
#36052 = VECTOR ( 'NONE', #20875, 1000.000000000000000 ) ;
#36053 = VECTOR ( 'NONE', #21783, 1000.000000000000000 ) ;
#36054 = CARTESIAN_POINT ( 'NONE',  ( 22.88594695219327235, 3.421158645304719137, -11.50198563395279194 ) ) ;
#36055 = VECTOR ( 'NONE', #44025, 1000.000000000000114 ) ;
#36056 = ORIENTED_EDGE ( 'NONE', *, *, #35958, .T. ) ;
#36057 = DIRECTION ( 'NONE',  ( 0.000000000000000000, 0.000000000000000000, 1.000000000000000000 ) ) ;
#36058 = DIRECTION ( 'NONE',  ( 0.000000000000000000, 0.000000000000000000, -1.000000000000000000 ) ) ;
#36059 = CARTESIAN_POINT ( 'NONE',  ( -2.788988918599723199, -8.522892352054020293, 10.47550790974846358 ) ) ;
#36060 = AXIS2_PLACEMENT_3D ( 'NONE', #21906, #20596, #56148 ) ;
#36061 = CARTESIAN_POINT ( 'NONE',  ( 37.00000000000000711, 4.705694406421931860E-17, -3.469127814946512892E-15 ) ) ;
#36062 = CARTESIAN_POINT ( 'NONE',  ( -22.30625920655495165, -3.635849356906410534, 1.076742202099151946 ) ) ;
#36063 = AXIS2_PLACEMENT_3D ( 'NONE', #39871, #60152, #14577 ) ;
#36064 = ADVANCED_FACE ( 'NONE', ( #24556 ), #55473, .T. ) ;
#36065 = DIRECTION ( 'NONE',  ( 1.000000000000000000, -0.000000000000000000, -0.000000000000000000 ) ) ;
#36066 = CARTESIAN_POINT ( 'NONE',  ( 10.62525021964948913, 0.6055412984861371362, -11.98539912922879758 ) ) ;
#36067 = ORIENTED_EDGE ( 'NONE', *, *, #59476, .T. ) ;
#36068 = CARTESIAN_POINT ( 'NONE',  ( 0.2653519789438754661, 10.61653328464227641, 6.104019611498609166 ) ) ;
#36069 = FACE_OUTER_BOUND ( 'NONE', #45546, .T. ) ;
#36070 = DIRECTION ( 'NONE',  ( 1.000000000000000000, -0.000000000000000000, 0.000000000000000000 ) ) ;
#36071 = AXIS2_PLACEMENT_3D ( 'NONE', #44883, #34247, #8987 ) ;
#36072 = ADVANCED_FACE ( 'NONE', ( #24894 ), #4451, .T. ) ;
#36073 = CARTESIAN_POINT ( 'NONE',  ( 12.27843880161849199, 0.5230167770466689348, -13.48988925457417842 ) ) ;
#36074 = CARTESIAN_POINT ( 'NONE',  ( 37.00000000000000711, 4.705694406421931860E-17, -3.469127814946512892E-15 ) ) ;
#36075 = ORIENTED_EDGE ( 'NONE', *, *, #23684, .F. ) ;
#36076 = CARTESIAN_POINT ( 'NONE',  ( -17.63187738893816814, -5.505153328604047935, -12.32741040139104349 ) ) ;
#36077 = DIRECTION ( 'NONE',  ( -1.000000000000000000, 0.000000000000000000, 0.000000000000000000 ) ) ;
#36078 = CARTESIAN_POINT ( 'NONE',  ( 2.258463476536646475, 1.192666169132632570, 7.546439757228810663 ) ) ;
#36079 = ORIENTED_EDGE ( 'NONE', *, *, #13789, .F. ) ;
#36080 = CARTESIAN_POINT ( 'NONE',  ( -35.00000000000000000, 0.000000000000000000, 0.000000000000000000 ) ) ;
#36081 = CARTESIAN_POINT ( 'NONE',  ( -15.23343484266066383, 7.971175414668098647, -8.970033181536839706 ) ) ;
#36082 = DIRECTION ( 'NONE',  ( 0.000000000000000000, -0.01356324068817998940, 0.9999080150203990547 ) ) ;
#36083 = ADVANCED_FACE ( 'NONE', ( #9248 ), #60134, .T. ) ;
#36084 = B_SPLINE_CURVE_WITH_KNOTS ( 'NONE', 3,
 ( #3298, #7964, #28231, #23237, #18608, #38862, #59156, #13567, #60774, #50795, #9232, #8925, #65411, #3948, #15209, #29839, #59794, #49817, #24536 ),
 .UNSPECIFIED., .F., .F.,
 ( 4, 3, 3, 3, 3, 3, 4 ),
 ( 2.168404344971008868E-19, 2.831840207499545546E-05, 4.217266859840393823E-05, 5.602024318395990336E-05, 6.290810167969312265E-05, 9.120440630944972487E-05, 0.0001153103026479762659 ),
 .UNSPECIFIED. ) ;
#36086 = EDGE_LOOP ( 'NONE', ( #49276, #52435, #40651, #23128 ) ) ;
#36085 = CARTESIAN_POINT ( 'NONE',  ( 47.00000000000000711, 4.705694406421931860E-17, -3.469127814946512892E-15 ) ) ;
#36087 = CARTESIAN_POINT ( 'NONE',  ( -36.00000000000000711, -11.39945968423475264, 5.710938531231672499 ) ) ;
#36088 = CIRCLE ( 'NONE', #42446, 12.18650000000000055 ) ;
#36089 = AXIS2_PLACEMENT_3D ( 'NONE', #6897, #31806, #32140 ) ;
#36090 = FACE_OUTER_BOUND ( 'NONE', #18970, .T. ) ;
#36091 = VERTEX_POINT ( 'NONE', #60452 ) ;
#36092 = LINE ( 'NONE', #56396, #28051 ) ;
#36093 = DIRECTION ( 'NONE',  ( -1.000000000000000000, 0.000000000000000000, 0.000000000000000000 ) ) ;
#36094 = DIRECTION ( 'NONE',  ( -1.000000000000000000, 0.000000000000000000, -0.000000000000000000 ) ) ;
#36095 = CARTESIAN_POINT ( 'NONE',  ( 1.109979610372146652, -1.701361252868426988, -12.41172293674716443 ) ) ;
#36096 =( BOUNDED_CURVE ( )  B_SPLINE_CURVE ( 3, ( #11790, #32072, #56948, #21694 ),
 .UNSPECIFIED., .F., .F. ) 
 B_SPLINE_CURVE_WITH_KNOTS ( ( 4, 4 ),
 ( 2.698962753596566788, 2.780459056254051209 ),
 .UNSPECIFIED. ) 
 CURVE ( )  GEOMETRIC_REPRESENTATION_ITEM ( )  RATIONAL_B_SPLINE_CURVE ( ( 1.000000000000000000, 0.9994466059659545820, 0.9994466059659545820, 1.000000000000000000 ) ) 
 REPRESENTATION_ITEM ( '' )  );
#36097 = CARTESIAN_POINT ( 'NONE',  ( -35.05175862995318425, 0.008837625261041981428, -0.008949502803503109338 ) ) ;
#36098 = CARTESIAN_POINT ( 'NONE',  ( -17.54726996257253191, 25.00000000000000000, 3.865003848717349033 ) ) ;
#36099 = ORIENTED_EDGE ( 'NONE', *, *, #27094, .F. ) ;
#36100 = CARTESIAN_POINT ( 'NONE',  ( 2.259830038564999644, -5.015955067335966966, 5.763537486834654722 ) ) ;
#36101 = ORIENTED_EDGE ( 'NONE', *, *, #26282, .F. ) ;
#36102 = DIRECTION ( 'NONE',  ( -1.000000000000000000, 0.000000000000000000, 0.000000000000000000 ) ) ;
#36103 = AXIS2_PLACEMENT_3D ( 'NONE', #17575, #12550, #43144 ) ;
#36104 = EDGE_CURVE ( 'NONE', #11407, #33979, #2314, .T. ) ;
#36105 = DIRECTION ( 'NONE',  ( 0.9486832985018464059, 0.000000000000000000, -0.3162277646628405270 ) ) ;
#36106 = CARTESIAN_POINT ( 'NONE',  ( -36.00000000000000711, 9.390600770287994337, 8.624332853796092380 ) ) ;
#36108 = VERTEX_POINT ( 'NONE', #20874 ) ;
#36107 = AXIS2_PLACEMENT_3D ( 'NONE', #5888, #26147, #41411 ) ;
#36109 = CARTESIAN_POINT ( 'NONE',  ( -32.16141091265169649, 25.00000000000000000, 5.384978440493686236 ) ) ;
#36110 = CARTESIAN_POINT ( 'NONE',  ( -24.39340877539587993, -9.142083323587534949, 7.776330322708387754 ) ) ;
#36111 = CARTESIAN_POINT ( 'NONE',  ( -22.27722019094931127, -1.249795790945194440, 3.463038365117186324 ) ) ;
#36112 = ORIENTED_EDGE ( 'NONE', *, *, #15666, .T. ) ;
#36113 = ORIENTED_EDGE ( 'NONE', *, *, #21769, .F. ) ;
#36114 = CARTESIAN_POINT ( 'NONE',  ( 28.33146005156584479, -12.08694127755678416, 6.025141712200583477 ) ) ;
#36115 = ORIENTED_EDGE ( 'NONE', *, *, #1755, .T. ) ;
#36116 = AXIS2_PLACEMENT_3D ( 'NONE', #51118, #56083, #26170 ) ;
#36117 = CARTESIAN_POINT ( 'NONE',  ( -35.00000000000000000, 11.74226168163341555, 0.3025107581131598611 ) ) ;
#36118 = CARTESIAN_POINT ( 'NONE',  ( 0.9232058338315058954, 4.617996777200573888, 11.58467545991555525 ) ) ;
#36119 = CARTESIAN_POINT ( 'NONE',  ( -37.00000000000000711, 0.000000000000000000, 0.000000000000000000 ) ) ;
#36120 = CYLINDRICAL_SURFACE ( 'NONE', #39038, 5.000000000000000888 ) ;
#36121 = EDGE_CURVE ( 'NONE', #27224, #65758, #51151, .T. ) ;
#36122 = CARTESIAN_POINT ( 'NONE',  ( -22.66110217412718342, 0.6585288088160327069, -4.900671186447929983 ) ) ;
#36123 = CARTESIAN_POINT ( 'NONE',  ( -35.00000000000000000, 3.916263239775508165, -11.07407352312208459 ) ) ;
#36124 = DIRECTION ( 'NONE',  ( -1.000000000000000000, 0.000000000000000000, 0.000000000000000000 ) ) ;
#36125 = ORIENTED_EDGE ( 'NONE', *, *, #20088, .F. ) ;
#36126 = CARTESIAN_POINT ( 'NONE',  ( 0.5572780756284647641, -11.70006938410064912, 3.933334466452514722 ) ) ;
#36127 = AXIS2_PLACEMENT_3D ( 'NONE', #65383, #34781, #20505 ) ;
#36128 = DIRECTION ( 'NONE',  ( -1.000000000000000000, 0.000000000000000000, -0.000000000000000000 ) ) ;
#36129 = CARTESIAN_POINT ( 'NONE',  ( -35.00000000000000000, -11.78977382767499194, 4.245927698352018886 ) ) ;
#36130 = CARTESIAN_POINT ( 'NONE',  ( -9.278753422987154664, 10.79879054606790767, -5.236717350350218680 ) ) ;
#36131 = DIRECTION ( 'NONE',  ( 1.000000000000000000, 0.000000000000000000, -0.000000000000000000 ) ) ;
#36132 = DIRECTION ( 'NONE',  ( 0.000000000000000000, 0.9970832820307041766, 0.07632122047556146038 ) ) ;
#36133 = CARTESIAN_POINT ( 'NONE',  ( -35.00000000000000000, -10.70999494708497046, 5.814360711498253842 ) ) ;
#36134 = DIRECTION ( 'NONE',  ( 0.000000000000000000, 0.000000000000000000, -1.000000000000000000 ) ) ;
#36135 = EDGE_CURVE ( 'NONE', #1460, #13960, #17145, .T. ) ;
#36136 = ORIENTED_EDGE ( 'NONE', *, *, #8788, .T. ) ;
#36137 = CIRCLE ( 'NONE', #26616, 5.000000000000000888 ) ;
#36139 = ORIENTED_EDGE ( 'NONE', *, *, #17851, .F. ) ;
#36138 = VECTOR ( 'NONE', #56620, 1000.000000000000000 ) ;
#36140 = AXIS2_PLACEMENT_3D ( 'NONE', #48716, #33728, #18475 ) ;
#36141 = DIRECTION ( 'NONE',  ( -1.000000000000000000, 0.000000000000000000, 0.000000000000000000 ) ) ;
#36142 = B_SPLINE_CURVE_WITH_KNOTS ( 'NONE', 3,
 ( #39166, #48520, #59459, #28229, #53518, #43496, #63776 ),
 .UNSPECIFIED., .F., .F.,
 ( 4, 3, 4 ),
 ( 0.000000000000000000, 0.001700533616330569429, 0.005002426799371238395 ),
 .UNSPECIFIED. ) ;
#36143 = EDGE_CURVE ( 'NONE', #35685, #3821, #42427, .T. ) ;
#36144 = ORIENTED_EDGE ( 'NONE', *, *, #33703, .T. ) ;
#36145 = CARTESIAN_POINT ( 'NONE',  ( 5.515188684475870851, -0.003857086913166418371, 0.003709313826050277332 ) ) ;
#36146 = FACE_OUTER_BOUND ( 'NONE', #321, .T. ) ;
#36147 = CARTESIAN_POINT ( 'NONE',  ( 0.2638984909335716500, -4.001111175853667490, -11.57533005135182869 ) ) ;
#36148 = EDGE_CURVE ( 'NONE', #62968, #44872, #15865, .T. ) ;
#36149 = DIRECTION ( 'NONE',  ( 1.000000000000000000, -0.000000000000000000, -0.000000000000000000 ) ) ;
#36150 = B_SPLINE_CURVE_WITH_KNOTS ( 'NONE', 3,
 ( #50990, #14723, #50354, #59991, #55313, #9753, #4801, #34686, #15068, #31026, #54982, #55658, #9410, #45337, #29700, #50008, #4467, #19757, #40013 ),
 .UNSPECIFIED., .F., .F.,
 ( 4, 3, 3, 3, 3, 3, 4 ),
 ( 0.000000000000000000, 2.831840207499875211E-05, 4.217266859840889846E-05, 5.602024318396385392E-05, 6.290810167969526395E-05, 9.120440630945454957E-05, 0.0001153103026479750733 ),
 .UNSPECIFIED. ) ;
#36151 = ORIENTED_EDGE ( 'NONE', *, *, #22167, .F. ) ;
#36152 = CARTESIAN_POINT ( 'NONE',  ( 0.000000000000000000, -0.8935325819929111901, 7.446583077151331942 ) ) ;
#36153 = DIRECTION ( 'NONE',  ( 0.000000000000000000, -0.8009703041134103030, -0.5987040770935764256 ) ) ;
#36154 = CARTESIAN_POINT ( 'NONE',  ( 0.3675815128205894289, -12.13672785388551389, 1.872154644482044938 ) ) ;
#36155 = CARTESIAN_POINT ( 'NONE',  ( 0.000000000000000000, -45.00000000000000000, -22.50555349946515804 ) ) ;
#36156 = AXIS2_PLACEMENT_3D ( 'NONE', #41027, #35377, #61310 ) ;
#36157 = EDGE_CURVE ( 'NONE', #12453, #20190, #7616, .T. ) ;
#36158 = CARTESIAN_POINT ( 'NONE',  ( 1.719304012339826659, -12.64775761152879596, -1.452142814149639305 ) ) ;
#36159 = AXIS2_PLACEMENT_3D ( 'NONE', #44620, #40963, #30640 ) ;
#36160 = CARTESIAN_POINT ( 'NONE',  ( -35.00000000000000000, 0.000000000000000000, 0.000000000000000000 ) ) ;
#36161 = ORIENTED_EDGE ( 'NONE', *, *, #28519, .F. ) ;
#36162 = VECTOR ( 'NONE', #25195, 1000.000000000000000 ) ;
#36163 = DIRECTION ( 'NONE',  ( 0.000000000000000000, 0.000000000000000000, -1.000000000000000000 ) ) ;
#36164 = VERTEX_POINT ( 'NONE', #16557 ) ;
#36165 = CARTESIAN_POINT ( 'NONE',  ( 1.719304012341273280, -2.961219984259375160, -12.38166659046469675 ) ) ;
#36166 = CARTESIAN_POINT ( 'NONE',  ( 0.000000000000000000, 0.000000000000000000, 0.000000000000000000 ) ) ;
#36167 = ADVANCED_FACE ( 'NONE', ( #42123 ), #57104, .F. ) ;
#36168 = CIRCLE ( 'NONE', #19198, 12.18650000000000233 ) ;
#36169 = DIRECTION ( 'NONE',  ( -1.000000000000000000, 0.000000000000000000, 0.000000000000000000 ) ) ;
#36170 = CARTESIAN_POINT ( 'NONE',  ( -35.00000000000000000, -0.7214809346827719683, -11.72397916322013245 ) ) ;
#36171 = VERTEX_POINT ( 'NONE', #22524 ) ;
#36172 = ORIENTED_EDGE ( 'NONE', *, *, #59381, .F. ) ;
#36174 = EDGE_CURVE ( 'NONE', #34363, #14439, #48706, .T. ) ;
#36173 = CARTESIAN_POINT ( 'NONE',  ( -30.18541646480307250, -1.416020129149132112, 11.91616074890920096 ) ) ;
#36175 = EDGE_LOOP ( 'NONE', ( #60721, #58135, #8468, #21062 ) ) ;
#36176 = AXIS2_PLACEMENT_3D ( 'NONE', #29037, #45300, #19053 ) ;
#36177 = CARTESIAN_POINT ( 'NONE',  ( 2.177405672432031203, 6.173731551722755562, 9.343720763423021936 ) ) ;
#36178 = CARTESIAN_POINT ( 'NONE',  ( 35.00000000000000000, -11.65554240571056077, 1.456211999474460672 ) ) ;
#36179 = DIRECTION ( 'NONE',  ( 0.000000000000000000, 0.01356324068817992175, -0.9999080150203990547 ) ) ;
#36180 = DIRECTION ( 'NONE',  ( -1.000000000000000000, 0.000000000000000000, 0.000000000000000000 ) ) ;
#36181 = FACE_OUTER_BOUND ( 'NONE', #50280, .T. ) ;
#36182 = CARTESIAN_POINT ( 'NONE',  ( -11.08973503868622856, -9.548835897016632046, 9.557198817210366570 ) ) ;
#36183 = CARTESIAN_POINT ( 'NONE',  ( -5.440603711307418600, -0.9287262547304560023, 11.96401375240336939 ) ) ;
#36184 = EDGE_LOOP ( 'NONE', ( #44627, #32670, #39356, #31606 ) ) ;
#36185 = AXIS2_PLACEMENT_3D ( 'NONE', #39371, #34392, #54698 ) ;
#36186 = CARTESIAN_POINT ( 'NONE',  ( 3.047904605210435935, -2.299870214474486030, -7.561255571389412289 ) ) ;
#36187 = ORIENTED_EDGE ( 'NONE', *, *, #44968, .F. ) ;
#36188 = CARTESIAN_POINT ( 'NONE',  ( -35.00000000000000000, 0.000000000000000000, 0.000000000000000000 ) ) ;
#36189 = DIRECTION ( 'NONE',  ( -1.000000000000000000, 0.000000000000000000, 0.000000000000000000 ) ) ;
#36190 = CARTESIAN_POINT ( 'NONE',  ( -27.08704841010891684, 1.888108843317904517, -1.313007237775874136 ) ) ;
#36191 = VECTOR ( 'NONE', #60790, 1000.000000000000000 ) ;
#36192 = VECTOR ( 'NONE', #21577, 1000.000000000000000 ) ;
#36193 = VERTEX_POINT ( 'NONE', #47472 ) ;
#36194 = CARTESIAN_POINT ( 'NONE',  ( -17.03240540343445630, -29.48295256022971955, 9.532950799341300296 ) ) ;
#36195 = ORIENTED_EDGE ( 'NONE', *, *, #48896, .F. ) ;
#36196 = CARTESIAN_POINT ( 'NONE',  ( -2.672122885467072440, -11.33640012973145694, 3.936387307894340548 ) ) ;
#36197 = CARTESIAN_POINT ( 'NONE',  ( -35.00000000000000000, 0.000000000000000000, 0.000000000000000000 ) ) ;
#36198 = AXIS2_PLACEMENT_3D ( 'NONE', #15770, #60691, #4850 ) ;
#36199 = DIRECTION ( 'NONE',  ( 0.000000000000000000, 0.01356324068817998940, -0.9999080150203990547 ) ) ;
#36200 = CARTESIAN_POINT ( 'NONE',  ( -28.93866847389638153, -3.371687389997700901, -23.68754010782029340 ) ) ;
#36201 = EDGE_LOOP ( 'NONE', ( #59652, #10039, #718, #12958 ) ) ;
#36202 = EDGE_LOOP ( 'NONE', ( #6138, #10435, #8075, #51868, #52936, #10501 ) ) ;
#36203 = CARTESIAN_POINT ( 'NONE',  ( 3.337809848554626146, 5.204416062760586215, 12.45815437626194289 ) ) ;
#36204 = ORIENTED_EDGE ( 'NONE', *, *, #64995, .F. ) ;
#36205 = CARTESIAN_POINT ( 'NONE',  ( 35.00000000000000000, 4.705694406421931860E-17, -3.469127814946512892E-15 ) ) ;
#36206 = EDGE_LOOP ( 'NONE', ( #54475, #42544, #18228, #4201 ) ) ;
#36207 = ORIENTED_EDGE ( 'NONE', *, *, #15390, .F. ) ;
#36208 = ORIENTED_EDGE ( 'NONE', *, *, #4528, .F. ) ;
#36209 = AXIS2_PLACEMENT_3D ( 'NONE', #37103, #26166, #62369 ) ;
#36210 = DIRECTION ( 'NONE',  ( 0.000000000000000000, 0.000000000000000000, 1.000000000000000000 ) ) ;
#36211 = CARTESIAN_POINT ( 'NONE',  ( -4.968020780095185884, -25.99038707641917156, 15.26464785194326979 ) ) ;
#36212 = EDGE_CURVE ( 'NONE', #21740, #1650, #52133, .T. ) ;
#36213 = AXIS2_PLACEMENT_3D ( 'NONE', #16372, #13339, #1737 ) ;
#36214 = CARTESIAN_POINT ( 'NONE',  ( 2.305787727787084407, -1.164987321564681100, -7.566723232958083578 ) ) ;
#36215 = CARTESIAN_POINT ( 'NONE',  ( 2.268878695253353950, 2.752970156154584291, -7.130600918714350200 ) ) ;
#36216 = CARTESIAN_POINT ( 'NONE',  ( 35.00000000000000000, 4.705694406421931860E-17, -3.469127814946512892E-15 ) ) ;
#36217 = ORIENTED_EDGE ( 'NONE', *, *, #33920, .T. ) ;
#36218 = CIRCLE ( 'NONE', #5442, 7.499999999999988454 ) ;
#36219 = DIRECTION ( 'NONE',  ( 0.000000000000000000, -0.8369827122275401710, -0.5472293298355184188 ) ) ;
#36220 = CIRCLE ( 'NONE', #39404, 12.75000000000000178 ) ;
#36221 = VERTEX_POINT ( 'NONE', #46473 ) ;
#36222 = CARTESIAN_POINT ( 'NONE',  ( -29.60265935865812637, -3.677894516095094879, -12.98940028976120509 ) ) ;
#36223 = CARTESIAN_POINT ( 'NONE',  ( -3.171556313731246579, 12.42408210250854772, 5.292542471626417111 ) ) ;
#36224 = CIRCLE ( 'NONE', #30913, 5.000000000000000000 ) ;
#36225 = CARTESIAN_POINT ( 'NONE',  ( 0.2653519890538383330, 0.02202236966339091162, -12.24619734961521544 ) ) ;
#36226 = DIRECTION ( 'NONE',  ( 0.000000000000000000, 0.01356324068817992175, -0.9999080150203990547 ) ) ;
#36227 = DIRECTION ( 'NONE',  ( -0.000000000000000000, -1.000000000000000000, -0.000000000000000000 ) ) ;
#36228 = CIRCLE ( 'NONE', #27735, 12.74999999999999822 ) ;
#36229 = CARTESIAN_POINT ( 'NONE',  ( 1.020182472824579412, -10.59341968305535175, -6.631405022220755008 ) ) ;
#36230 = EDGE_CURVE ( 'NONE', #56661, #32997, #63895, .T. ) ;
#36231 = ORIENTED_EDGE ( 'NONE', *, *, #3872, .T. ) ;
#36232 = DIRECTION ( 'NONE',  ( 0.000000000000000000, 0.4134677391718449280, 0.9105187689795983808 ) ) ;
#36233 = AXIS2_PLACEMENT_3D ( 'NONE', #40466, #60767, #1579 ) ;
#36234 = ORIENTED_EDGE ( 'NONE', *, *, #46259, .T. ) ;
#36235 = EDGE_CURVE ( 'NONE', #13608, #42115, #10901, .T. ) ;
#36236 = CARTESIAN_POINT ( 'NONE',  ( 0.000000000000000000, -35.00000000000000000, 0.000000000000000000 ) ) ;
#36237 = CARTESIAN_POINT ( 'NONE',  ( -35.00000000000000000, -11.74614673114904129, -0.01609748574457297438 ) ) ;
#36238 = CARTESIAN_POINT ( 'NONE',  ( 2.705197763288545776, 6.142723737672452167, -4.789125516644054947 ) ) ;
#36240 = CIRCLE ( 'NONE', #26708, 5.000000000000000888 ) ;
#36239 = FACE_OUTER_BOUND ( 'NONE', #25401, .T. ) ;
#36241 = EDGE_CURVE ( 'NONE', #49252, #23349, #17009, .T. ) ;
#36242 = CARTESIAN_POINT ( 'NONE',  ( -28.67667724226168602, -1.049259427760474983, -1.574547667005680607 ) ) ;
#36243 = VERTEX_POINT ( 'NONE', #13196 ) ;
#36244 = DIRECTION ( 'NONE',  ( 0.000000000000000000, -0.01356324068817991828, 0.9999080150203990547 ) ) ;
#36245 = DIRECTION ( 'NONE',  ( 1.000000000000000000, -0.000000000000000000, -0.000000000000000000 ) ) ;
#36246 = DIRECTION ( 'NONE',  ( 1.000000000000000000, 0.000000000000000000, 0.000000000000000000 ) ) ;
#36247 = CARTESIAN_POINT ( 'NONE',  ( 25.05309951391468459, -10.77522019223763827, -8.132934882857099979 ) ) ;
#36248 = AXIS2_PLACEMENT_3D ( 'NONE', #2083, #41984, #27344 ) ;
#36249 = AXIS2_PLACEMENT_3D ( 'NONE', #51067, #25452, #55387 ) ;
#36250 = VECTOR ( 'NONE', #63986, 1000.000000000000000 ) ;
#36251 = EDGE_CURVE ( 'NONE', #43919, #45722, #3362, .T. ) ;
#36252 = CARTESIAN_POINT ( 'NONE',  ( 0.2767916011545383248, 12.24854187541374628, -0.1897947303543257302 ) ) ;
#36253 = EDGE_CURVE ( 'NONE', #5722, #38595, #60679, .T. ) ;
#36254 = DIRECTION ( 'NONE',  ( -1.000000000000000000, 0.000000000000000000, 0.000000000000000000 ) ) ;
#36255 = CARTESIAN_POINT ( 'NONE',  ( 0.9296196016843304433, -5.870433615766820878, -10.99907063288908304 ) ) ;
#36256 = CARTESIAN_POINT ( 'NONE',  ( -27.08416813689868263, 1.759517419957079554, -1.467601568343266827 ) ) ;
#36257 = CARTESIAN_POINT ( 'NONE',  ( 2.251139882113957214, 0.1241612276497709028, -7.636654603229075633 ) ) ;
#36258 = EDGE_CURVE ( 'NONE', #44901, #24100, #43721, .T. ) ;
#36259 = CIRCLE ( 'NONE', #5492, 12.74999999999999822 ) ;
#36260 = VECTOR ( 'NONE', #10404, 1000.000000000000000 ) ;
#36261 = EDGE_LOOP ( 'NONE', ( #50361, #41897, #17258, #25932 ) ) ;
#36263 = EDGE_CURVE ( 'NONE', #53566, #13432, #40491, .T. ) ;
#36262 = CIRCLE ( 'NONE', #34117, 5.000000000000000888 ) ;
#36264 = ORIENTED_EDGE ( 'NONE', *, *, #56697, .F. ) ;
#36265 = CARTESIAN_POINT ( 'NONE',  ( -22.59969328935898858, 4.339503524536204360, -1.672297795814005505 ) ) ;
#36266 = CARTESIAN_POINT ( 'NONE',  ( 22.00000000000000711, -20.00000000000000000, 2.449293598294706907E-15 ) ) ;
#36267 = DIRECTION ( 'NONE',  ( -1.000000000000000000, -0.000000000000000000, 0.000000000000000000 ) ) ;
#36268 = AXIS2_PLACEMENT_3D ( 'NONE', #7412, #52672, #42999 ) ;
#36269 = EDGE_CURVE ( 'NONE', #44459, #55375, #51895, .T. ) ;
#36270 = CARTESIAN_POINT ( 'NONE',  ( 0.2834382757447995727, -1.927645269570966269, 12.09963924911735411 ) ) ;
#36271 = ORIENTED_EDGE ( 'NONE', *, *, #51870, .F. ) ;
#36272 = AXIS2_PLACEMENT_3D ( 'NONE', #40738, #180, #6158 ) ;
#36273 = VERTEX_POINT ( 'NONE', #48135 ) ;
#36274 = VERTEX_POINT ( 'NONE', #2593 ) ;
#36275 = LINE ( 'NONE', #6050, #19583 ) ;
#36276 = CARTESIAN_POINT ( 'NONE',  ( -22.27722019117890540, 0.6494988092404053726, 3.623917154020592335 ) ) ;
#36277 = ORIENTED_EDGE ( 'NONE', *, *, #12308, .F. ) ;
#36278 = CARTESIAN_POINT ( 'NONE',  ( 37.25000000000000711, -27.53407839942726909, 1.504154570186529094 ) ) ;
#36279 = CIRCLE ( 'NONE', #20390, 12.73084802173761787 ) ;
#36280 = DIRECTION ( 'NONE',  ( 1.000000000000000000, 0.000000000000000000, 0.000000000000000000 ) ) ;
#36281 = EDGE_LOOP ( 'NONE', ( #9990, #2799, #35704, #21152 ) ) ;
#36282 = CARTESIAN_POINT ( 'NONE',  ( -22.27704833740210333, 0.3581593033281407767, 3.663709865074111338 ) ) ;
#36283 = CARTESIAN_POINT ( 'NONE',  ( 12.91449914267889731, -28.36597991684663000, -12.93464570467139119 ) ) ;
#36284 = CARTESIAN_POINT ( 'NONE',  ( -35.00000000000000000, -2.968224442958318665, -11.81949347079750012 ) ) ;
#36285 = EDGE_LOOP ( 'NONE', ( #45553, #21251, #26159, #61182 ) ) ;
#36287 = AXIS2_PLACEMENT_3D ( 'NONE', #24174, #54112, #33512 ) ;
#36286 = CARTESIAN_POINT ( 'NONE',  ( 0.3218525148189835816, 12.11874253990393413, -1.888670068297527260 ) ) ;
#36288 = ORIENTED_EDGE ( 'NONE', *, *, #15879, .T. ) ;
#36289 = CYLINDRICAL_SURFACE ( 'NONE', #27341, 12.18649999999999878 ) ;
#36290 = ORIENTED_EDGE ( 'NONE', *, *, #38376, .T. ) ;
#36291 = DIRECTION ( 'NONE',  ( 1.000000000000000000, -0.000000000000000000, -0.000000000000000000 ) ) ;
#36292 = CARTESIAN_POINT ( 'NONE',  ( 2.241352910868909643, -4.970878533273721978, -5.794346703933896059 ) ) ;
#36293 = CARTESIAN_POINT ( 'NONE',  ( 2.257661810676418579, 3.936095962955294958, 6.547845034191107416 ) ) ;
#36294 = CARTESIAN_POINT ( 'NONE',  ( -26.90845769821730471, 3.274239888503029938, 0.2771906250059949506 ) ) ;
#36295 = AXIS2_PLACEMENT_3D ( 'NONE', #3909, #4220, #64394 ) ;
#36296 = EDGE_CURVE ( 'NONE', #22708, #32746, #28809, .T. ) ;
#36297 = AXIS2_PLACEMENT_3D ( 'NONE', #47964, #41974, #21719 ) ;
#36299 = VECTOR ( 'NONE', #2082, 1000.000000000000000 ) ;
#36298 = DIRECTION ( 'NONE',  ( 0.000000000000000000, -0.01356324068817998940, 0.9999080150203990547 ) ) ;
#36300 = LINE ( 'NONE', #57253, #38271 ) ;
#36301 = LINE ( 'NONE', #20360, #23992 ) ;
#36302 = CARTESIAN_POINT ( 'NONE',  ( 0.2652384770603670172, 4.126289928142402808, 11.53005438969045393 ) ) ;
#36304 = EDGE_LOOP ( 'NONE', ( #26741, #4746, #652, #2784 ) ) ;
#36303 = LINE ( 'NONE', #5085, #46964 ) ;
#36305 = CARTESIAN_POINT ( 'NONE',  ( -35.00000000000000000, -11.53507381115581687, -2.216820770815207897 ) ) ;
#36306 =( BOUNDED_CURVE ( )  B_SPLINE_CURVE ( 3, ( #47740, #6203, #56400, #17150 ),
 .UNSPECIFIED., .F., .F. ) 
 B_SPLINE_CURVE_WITH_KNOTS ( ( 4, 4 ),
 ( 4.960697898119300397, 4.993371868946114844 ),
 .UNSPECIFIED. ) 
 CURVE ( )  GEOMETRIC_REPRESENTATION_ITEM ( )  RATIONAL_B_SPLINE_CURVE ( ( 1.000000000000000000, 0.9999110362812402286, 0.9999110362812402286, 1.000000000000000000 ) ) 
 REPRESENTATION_ITEM ( '' )  );
#36307 = ORIENTED_EDGE ( 'NONE', *, *, #54426, .T. ) ;
#36308 = CARTESIAN_POINT ( 'NONE',  ( -37.00000000000000711, 6.946017217729938409, 10.01317267707888981 ) ) ;
#36309 = DIRECTION ( 'NONE',  ( -1.000000000000000000, 0.000000000000000000, 0.000000000000000000 ) ) ;
#36310 = ORIENTED_EDGE ( 'NONE', *, *, #59374, .T. ) ;
#36311 = EDGE_CURVE ( 'NONE', #59870, #56327, #61397, .T. ) ;
#36312 = DIRECTION ( 'NONE',  ( 0.000000000000000000, 0.3193015301359806712, -0.9476531711828022342 ) ) ;
#36313 = DIRECTION ( 'NONE',  ( -1.000000000000000000, 0.000000000000000000, 0.000000000000000000 ) ) ;
#36314 = DIRECTION ( 'NONE',  ( 0.000000000000000000, -0.01356324068817998940, 0.9999080150203990547 ) ) ;
#36316 = AXIS2_PLACEMENT_3D ( 'NONE', #6943, #26551, #27529 ) ;
#36315 = DIRECTION ( 'NONE',  ( 0.000000000000000000, -1.000000000000000000, 0.000000000000000000 ) ) ;
#36317 = AXIS2_PLACEMENT_3D ( 'NONE', #23610, #33580, #42889 ) ;
#36318 = CARTESIAN_POINT ( 'NONE',  ( -35.00000000000000000, -5.143145423404362759, 11.66664283989677919 ) ) ;
#36319 = ADVANCED_FACE ( 'NONE', ( #18540 ), #3887, .T. ) ;
#36320 = ORIENTED_EDGE ( 'NONE', *, *, #53780, .T. ) ;
#36321 = CARTESIAN_POINT ( 'NONE',  ( 5.536195898058073439, 0.004027525919832433861, 0.007485416011287818715 ) ) ;
#36322 = CIRCLE ( 'NONE', #29960, 5.000000000000000888 ) ;
#36323 = VERTEX_POINT ( 'NONE', #13503 ) ;
#36324 = DIRECTION ( 'NONE',  ( 0.000000000000000000, -0.01356324068817998940, 0.9999080150203990547 ) ) ;
#36325 = AXIS2_PLACEMENT_3D ( 'NONE', #415, #20684, #30636 ) ;
#36326 = FACE_OUTER_BOUND ( 'NONE', #17074, .T. ) ;
#36327 = DIRECTION ( 'NONE',  ( 0.000000000000000000, 0.5767582926624911233, 0.8169148498130316405 ) ) ;
#36328 = EDGE_CURVE ( 'NONE', #18651, #58059, #47191, .T. ) ;
#36329 = ORIENTED_EDGE ( 'NONE', *, *, #34653, .T. ) ;
#36330 = CARTESIAN_POINT ( 'NONE',  ( -27.08429572838383947, -0.9410937941433956677, 2.089332284968712816 ) ) ;
#36331 = VECTOR ( 'NONE', #48215, 1000.000000000000000 ) ;
#36332 = CARTESIAN_POINT ( 'NONE',  ( -35.04834644901396956, -0.004537648929134079599, -0.01306875526352651966 ) ) ;
#36333 = CARTESIAN_POINT ( 'NONE',  ( -29.68541646480307250, -1.416020129149132334, 11.91616074890920451 ) ) ;
#36334 = EDGE_CURVE ( 'NONE', #2181, #41862, #36262, .T. ) ;
#36335 = DIRECTION ( 'NONE',  ( 1.000000000000000000, -0.000000000000000000, 0.000000000000000000 ) ) ;
#36336 = CARTESIAN_POINT ( 'NONE',  ( 8.676118928743548508, 5.971998260216028420, 12.11395822404814737 ) ) ;
#36337 = DIRECTION ( 'NONE',  ( -0.3162277663656185012, -0.1673616205762862574, -0.9338040949457712125 ) ) ;
#36338 = CARTESIAN_POINT ( 'NONE',  ( 12.10998784662220551, 10.46621227226785322, -8.526922110106907482 ) ) ;
#36339 = DIRECTION ( 'NONE',  ( 1.000000000000000000, -0.000000000000000000, -0.000000000000000000 ) ) ;
#36340 = AXIS2_PLACEMENT_3D ( 'NONE', #45771, #50766, #20829 ) ;
#36341 = B_SPLINE_CURVE_WITH_KNOTS ( 'NONE', 3,
 ( #51367, #26082, #61630, #26727, #6784, #27058, #57660, #31693, #12076, #2109, #32356, #32664, #2457, #62604, #57317, #42644 ),
 .UNSPECIFIED., .F., .F.,
 ( 4, 3, 3, 3, 3, 4 ),
 ( 2.668793006540488735E-15, 0.0002126834539179618081, 0.0004253519300366075421, 0.0006380165497223889591, 0.0007442707582427920141, 0.0009453531351420071905 ),
 .UNSPECIFIED. ) ;
#36342 = EDGE_CURVE ( 'NONE', #49437, #54019, #11812, .T. ) ;
#36343 = VECTOR ( 'NONE', #8148, 1000.000000000000000 ) ;
#36344 = AXIS2_PLACEMENT_3D ( 'NONE', #37742, #58035, #32722 ) ;
#36345 = ORIENTED_EDGE ( 'NONE', *, *, #2287, .F. ) ;
#36346 = EDGE_CURVE ( 'NONE', #65266, #42915, #5186, .T. ) ;
#36347 = DIRECTION ( 'NONE',  ( 1.000000000000000000, 0.000000000000000000, 0.000000000000000000 ) ) ;
#36348 = DIRECTION ( 'NONE',  ( 0.000000000000000000, -0.01356324068817998940, 0.9999080150203990547 ) ) ;
#36349 = VERTEX_POINT ( 'NONE', #10478 ) ;
#36350 = CARTESIAN_POINT ( 'NONE',  ( 1.198791140417307499, 10.60778679489402165, 6.720248575442116845 ) ) ;
#36351 = DIRECTION ( 'NONE',  ( -1.000000000000000000, 0.000000000000000000, 0.000000000000000000 ) ) ;
#36352 = DIRECTION ( 'NONE',  ( 0.000000000000000000, 0.1081190184239417679, -0.9941379571543595972 ) ) ;
#36353 = VERTEX_POINT ( 'NONE', #59732 ) ;
#36354 = EDGE_CURVE ( 'NONE', #13375, #35130, #56452, .T. ) ;
#36355 = DIRECTION ( 'NONE',  ( 0.000000000000000000, -0.4380125133594036657, 0.8989688749565127868 ) ) ;
#36356 = FACE_OUTER_BOUND ( 'NONE', #42632, .T. ) ;
#36357 = ORIENTED_EDGE ( 'NONE', *, *, #11145, .F. ) ;
#36358 = CARTESIAN_POINT ( 'NONE',  ( 3.152665057736013132, 7.281573230473836311, -3.161213418915250095 ) ) ;
#36359 = ORIENTED_EDGE ( 'NONE', *, *, #33411, .F. ) ;
#36360 = ORIENTED_EDGE ( 'NONE', *, *, #44469, .T. ) ;
#36361 = CIRCLE ( 'NONE', #60766, 5.000000000000000000 ) ;
#36362 = CARTESIAN_POINT ( 'NONE',  ( -27.08418179957658367, -1.713622993062712707, 1.521007404704310062 ) ) ;
#36363 = ORIENTED_EDGE ( 'NONE', *, *, #48769, .T. ) ;
#36364 = CARTESIAN_POINT ( 'NONE',  ( 36.00000000000000711, -4.237174932027312657, -12.02534193257719686 ) ) ;
#36365 = CARTESIAN_POINT ( 'NONE',  ( 0.2646305136544065406, -7.770320294339235545, 9.465888453932937097 ) ) ;
#36366 = CARTESIAN_POINT ( 'NONE',  ( 36.00000000000000711, -8.830544224263011444, -9.196955404009264257 ) ) ;
#36367 = DIRECTION ( 'NONE',  ( 0.000000000000000000, -0.8276889981568840149, -0.5611870653623919347 ) ) ;
#36368 = ORIENTED_EDGE ( 'NONE', *, *, #36690, .T. ) ;
#36369 = AXIS2_PLACEMENT_3D ( 'NONE', #52593, #16986, #31307 ) ;
#36370 = FACE_OUTER_BOUND ( 'NONE', #5436, .T. ) ;
#36371 = AXIS2_PLACEMENT_3D ( 'NONE', #65399, #65717, #5234 ) ;
#36372 = CARTESIAN_POINT ( 'NONE',  ( 9.989421171649008002, -29.02163280020532099, 8.890648868200056398 ) ) ;
#36373 = CARTESIAN_POINT ( 'NONE',  ( -17.80575138031851878, 11.79421038511453901, 2.237023554643799539 ) ) ;
#36375 = ORIENTED_EDGE ( 'NONE', *, *, #6159, .F. ) ;
#36374 = CARTESIAN_POINT ( 'NONE',  ( 5.514970785353741078, -0.0005190732562558867313, -0.004694330894494369230 ) ) ;
#36376 = CARTESIAN_POINT ( 'NONE',  ( 2.241352910868908310, -2.532612177304491397, 7.202080440908734005 ) ) ;
#36377 = VERTEX_POINT ( 'NONE', #4198 ) ;
#36378 = DIRECTION ( 'NONE',  ( 0.000000000000000000, 0.01356324068817998940, -0.9999080150203990547 ) ) ;
#36379 = ORIENTED_EDGE ( 'NONE', *, *, #44826, .F. ) ;
#36380 = B_SPLINE_CURVE_WITH_KNOTS ( 'NONE', 3,
 ( #18366, #63546, #28321, #58256, #53613, #58605, #48307, #18019, #28642, #43270 ),
 .UNSPECIFIED., .F., .F.,
 ( 4, 3, 3, 4 ),
 ( 8.673617379884035472E-19, 6.607638129004487527E-05, 9.911389841680542587E-05, 0.0001667630577588620944 ),
 .UNSPECIFIED. ) ;
#36381 = ORIENTED_EDGE ( 'NONE', *, *, #296, .T. ) ;
#36382 = FACE_OUTER_BOUND ( 'NONE', #12139, .T. ) ;
#36383 = CARTESIAN_POINT ( 'NONE',  ( 2.241352910868908754, -4.843133558968088614, -5.901537464758503937 ) ) ;
#36384 = DIRECTION ( 'NONE',  ( -1.000000000000000000, 0.000000000000000000, 0.000000000000000000 ) ) ;
#36386 = EDGE_CURVE ( 'NONE', #27622, #47144, #64935, .T. ) ;
#36385 = ORIENTED_EDGE ( 'NONE', *, *, #55003, .T. ) ;
#36387 = FACE_OUTER_BOUND ( 'NONE', #56415, .T. ) ;
#36388 = CARTESIAN_POINT ( 'NONE',  ( 10.57504247840390832, 8.113525156875750710, 8.843426623829298450 ) ) ;
#36389 = CARTESIAN_POINT ( 'NONE',  ( -18.25006854224444908, -9.443202773001939221, -9.647586298549935435 ) ) ;
#36390 = ORIENTED_EDGE ( 'NONE', *, *, #37901, .F. ) ;
#36391 = AXIS2_PLACEMENT_3D ( 'NONE', #45687, #26390, #35697 ) ;
#36392 = ADVANCED_FACE ( 'NONE', ( #14476 ), #39213, .F. ) ;
#36393 = VERTEX_POINT ( 'NONE', #39430 ) ;
#36394 = CARTESIAN_POINT ( 'NONE',  ( 35.00000000000000000, -12.01765980939840439, 2.021542716731525413 ) ) ;
#36395 = ORIENTED_EDGE ( 'NONE', *, *, #36988, .T. ) ;
#36396 = CIRCLE ( 'NONE', #61879, 12.74999999999999822 ) ;
#36397 = ORIENTED_EDGE ( 'NONE', *, *, #21882, .T. ) ;
#36398 = EDGE_CURVE ( 'NONE', #32962, #58250, #16103, .T. ) ;
#36399 = FACE_OUTER_BOUND ( 'NONE', #18510, .T. ) ;
#36400 = DIRECTION ( 'NONE',  ( -1.000000000000000000, 0.000000000000000000, 0.000000000000000000 ) ) ;
#36401 = LINE ( 'NONE', #56711, #36053 ) ;
#36402 = CARTESIAN_POINT ( 'NONE',  ( 1.719304012338199517, 0.000000000000000000, 0.000000000000000000 ) ) ;
#36403 = LINE ( 'NONE', #16767, #7185 ) ;
#36404 = VECTOR ( 'NONE', #26206, 1000.000000000000000 ) ;
#36405 = DIRECTION ( 'NONE',  ( 0.000000000000000000, -0.3193015301359872216, 0.9476531711827999027 ) ) ;
#36406 = CARTESIAN_POINT ( 'NONE',  ( -22.27722019117890895, -0.6723250025933638074, -3.619826115298663272 ) ) ;
#36407 = ORIENTED_EDGE ( 'NONE', *, *, #29710, .T. ) ;
#36408 = CARTESIAN_POINT ( 'NONE',  ( -22.27786964138239867, -3.004507515156368491, 2.131221155130652356 ) ) ;
#36409 = EDGE_CURVE ( 'NONE', #34795, #55862, #20475, .T. ) ;
#36410 = CARTESIAN_POINT ( 'NONE',  ( -37.00000000000000711, 11.38112321385055026, -2.905556151562505462 ) ) ;
#36411 = VECTOR ( 'NONE', #60540, 1000.000000000000114 ) ;
#36412 = EDGE_CURVE ( 'NONE', #55375, #46695, #1947, .T. ) ;
#36413 = AXIS2_PLACEMENT_3D ( 'NONE', #57477, #57814, #36849 ) ;
#36414 = CARTESIAN_POINT ( 'NONE',  ( 2.000000000000001776, 5.860254403322016969, 3.474373880649828550 ) ) ;
#36415 = CARTESIAN_POINT ( 'NONE',  ( -22.59983133926800392, 2.272383229042392649, 4.058100437359447810 ) ) ;
#36416 = CARTESIAN_POINT ( 'NONE',  ( 24.23078042079723815, -1.962945746166874228, -13.35767736023731089 ) ) ;
#36417 = CARTESIAN_POINT ( 'NONE',  ( 3.848470891359772494, 5.223518357594018724, -10.80573223417720108 ) ) ;
#36418 = AXIS2_PLACEMENT_3D ( 'NONE', #41286, #61570, #30349 ) ;
#36419 = CARTESIAN_POINT ( 'NONE',  ( 35.00000000000000000, -10.02106554660713833, -7.882940143791742571 ) ) ;
#36420 = ORIENTED_EDGE ( 'NONE', *, *, #57185, .F. ) ;
#36421 = CARTESIAN_POINT ( 'NONE',  ( 2.177405672429650885, -4.457418613958688880, -10.27382588316896950 ) ) ;
#36422 = CARTESIAN_POINT ( 'NONE',  ( -35.00000000000000000, 0.000000000000000000, 0.000000000000000000 ) ) ;
#36423 = CARTESIAN_POINT ( 'NONE',  ( 9.160076034430323588, -32.64719971958564315, 12.35384511440123134 ) ) ;
#36424 = EDGE_CURVE ( 'NONE', #57471, #31543, #62239, .T. ) ;
#36425 = ADVANCED_FACE ( 'NONE', ( #21111 ), #26436, .T. ) ;
#36426 = CARTESIAN_POINT ( 'NONE',  ( -26.40204056389466913, 10.43732693397312694, 5.922310247585463650 ) ) ;
#36427 = CARTESIAN_POINT ( 'NONE',  ( 0.3665391374699467075, 12.04754782681757419, 2.392238720110499983 ) ) ;
#36428 = ORIENTED_EDGE ( 'NONE', *, *, #1738, .T. ) ;
#36429 = CARTESIAN_POINT ( 'NONE',  ( -36.00000000000000711, 10.59380114696480391, -7.094637218249241428 ) ) ;
#36430 = PLANE ( 'NONE',  #50229 ) ;
#36431 = CARTESIAN_POINT ( 'NONE',  ( 2.259830038565000532, 1.190932096469649260, 7.547174990768408698 ) ) ;
#36432 = VERTEX_POINT ( 'NONE', #534 ) ;
#36433 = ADVANCED_FACE ( 'NONE', ( #846 ), #62646, .T. ) ;
#36434 = DIRECTION ( 'NONE',  ( -1.000000000000000000, 0.000000000000000000, 0.000000000000000000 ) ) ;
#36435 = CARTESIAN_POINT ( 'NONE',  ( -16.61479760455914345, 7.633023783503033677, -9.260229731437394918 ) ) ;
#36436 = CARTESIAN_POINT ( 'NONE',  ( 0.3665391374699467075, 11.62960183138732617, -3.952034409876181709 ) ) ;
#36437 = VECTOR ( 'NONE', #24924, 1000.000000000000000 ) ;
#36438 = AXIS2_PLACEMENT_3D ( 'NONE', #52819, #7249, #2639 ) ;
#36440 = ORIENTED_EDGE ( 'NONE', *, *, #57708, .F. ) ;
#36439 = CARTESIAN_POINT ( 'NONE',  ( 2.573738926104373714, 1.112690714006538073, 7.664876274722913330 ) ) ;
#36441 = CARTESIAN_POINT ( 'NONE',  ( -35.00000000000000000, 12.70128625845194215, -1.113475361586357515 ) ) ;
#36442 = AXIS2_PLACEMENT_3D ( 'NONE', #34041, #19430, #40015 ) ;
#36443 = CIRCLE ( 'NONE', #44937, 5.000000000000000888 ) ;
#36444 = CARTESIAN_POINT ( 'NONE',  ( -23.18047892478188743, -4.776019214182017691, -0.4043282704081637702 ) ) ;
#36445 = VERTEX_POINT ( 'NONE', #1179 ) ;
#36446 = CARTESIAN_POINT ( 'NONE',  ( -22.27706485742869091, 3.547445275915927176, 0.9832726768967369191 ) ) ;
#36447 = CARTESIAN_POINT ( 'NONE',  ( 19.56743653832047158, -33.00000000000000000, 5.000000000000007994 ) ) ;
#36448 = CYLINDRICAL_SURFACE ( 'NONE', #33285, 5.000000000000000000 ) ;
#36449 = DIRECTION ( 'NONE',  ( -1.000000000000000000, 0.000000000000000000, 0.000000000000000000 ) ) ;
#36450 = CARTESIAN_POINT ( 'NONE',  ( -35.00000000000000000, 0.000000000000000000, 0.000000000000000000 ) ) ;
#36451 = AXIS2_PLACEMENT_3D ( 'NONE', #38276, #33306, #63880 ) ;
#36452 = DIRECTION ( 'NONE',  ( -0.000000000000000000, -1.000000000000000000, -0.000000000000000000 ) ) ;
#36454 = ORIENTED_EDGE ( 'NONE', *, *, #19970, .F. ) ;
#36453 = CARTESIAN_POINT ( 'NONE',  ( 5.514970785353741078, -0.002093325033904051488, -0.004233694591582509194 ) ) ;
#36455 = ORIENTED_EDGE ( 'NONE', *, *, #2503, .T. ) ;
#36456 = CARTESIAN_POINT ( 'NONE',  ( 24.54939449645449301, 1.221378253082901821, -11.94324836227821329 ) ) ;
#36457 = VECTOR ( 'NONE', #48238, 999.9999999999998863 ) ;
#36458 = VERTEX_POINT ( 'NONE', #5529 ) ;
#36459 = CARTESIAN_POINT ( 'NONE',  ( 1.283627346226609234, -11.62704807385636130, 4.817767733507167804 ) ) ;
#36460 = AXIS2_PLACEMENT_3D ( 'NONE', #29478, #14503, #14824 ) ;
#36461 = CARTESIAN_POINT ( 'NONE',  ( 35.00000000000000000, 11.90598845858539789, 4.561791185930283099 ) ) ;
#36462 = CARTESIAN_POINT ( 'NONE',  ( 2.000000000000001776, 6.812627895098307462, -0.04423456934727655609 ) ) ;
#36463 = VERTEX_POINT ( 'NONE', #52047 ) ;
#36464 = DIRECTION ( 'NONE',  ( -1.000000000000000000, 0.000000000000000000, 0.000000000000000000 ) ) ;
#36465 = EDGE_CURVE ( 'NONE', #38516, #15834, #57556, .T. ) ;
#36466 = AXIS2_PLACEMENT_3D ( 'NONE', #50694, #60014, #25406 ) ;
#36467 = CARTESIAN_POINT ( 'NONE',  ( -24.80591845283671049, -9.916447262152498610, 6.760652199599259227 ) ) ;
#36468 = FACE_BOUND ( 'NONE', #12159, .T. ) ;
#36469 = ORIENTED_EDGE ( 'NONE', *, *, #2172, .T. ) ;
#36470 = VECTOR ( 'NONE', #22589, 1000.000000000000000 ) ;
#36471 = EDGE_LOOP ( 'NONE', ( #24223, #53607, #48227, #18828 ) ) ;
#36472 = CARTESIAN_POINT ( 'NONE',  ( 3.031336079629336044, 7.694633165537301700, -1.779751109289334110 ) ) ;
#36473 = ORIENTED_EDGE ( 'NONE', *, *, #5551, .F. ) ;
#36474 = CARTESIAN_POINT ( 'NONE',  ( 5.516018279890452902, 0.005042957932158584518, -0.004525000489649788973 ) ) ;
#36475 = DIRECTION ( 'NONE',  ( -1.000000000000000000, 0.000000000000000000, 0.000000000000000000 ) ) ;
#36476 = CARTESIAN_POINT ( 'NONE',  ( 2.000000000000001776, -3.155844197800055539, -6.177028383390492650 ) ) ;
#36477 = CARTESIAN_POINT ( 'NONE',  ( 22.36482863261543486, 25.00000000000000000, -0.9234811557364158707 ) ) ;
#36478 = CARTESIAN_POINT ( 'NONE',  ( 2.000000000000001776, 5.997115278587678233, -3.485633455389450130 ) ) ;
#36479 = CARTESIAN_POINT ( 'NONE',  ( 37.00000000000000711, 4.705694406421931860E-17, -3.469127814946512892E-15 ) ) ;
#36480 = CARTESIAN_POINT ( 'NONE',  ( 2.249013661412230469, 7.499157010299435377, 1.444210756221575576 ) ) ;
#36481 = VERTEX_POINT ( 'NONE', #36419 ) ;
#36482 = CARTESIAN_POINT ( 'NONE',  ( 0.6511581176963838757, -11.73752429815123932, 3.919972364658685926 ) ) ;
#36483 = CARTESIAN_POINT ( 'NONE',  ( 2.639814597422743159, 4.103563379978107051, -6.594772041715895483 ) ) ;
#36484 = ADVANCED_FACE ( 'NONE', ( #41388 ), #46034, .F. ) ;
#36485 = CARTESIAN_POINT ( 'NONE',  ( 2.241352910868910531, 5.901537464758454199, 4.843133558968147234 ) ) ;
#36487 = DIRECTION ( 'NONE',  ( 1.000000000000000000, 0.000000000000000000, -0.000000000000000000 ) ) ;
#36486 = AXIS2_PLACEMENT_3D ( 'NONE', #2148, #53691, #18457 ) ;
#36488 = CARTESIAN_POINT ( 'NONE',  ( 37.00000000000000711, -2.250029553613672295, 12.54989509947652770 ) ) ;
#36489 = CARTESIAN_POINT ( 'NONE',  ( 1.937114397841932290, 7.538912286488345771, 10.38782037574618933 ) ) ;
#36490 = AXIS2_PLACEMENT_3D ( 'NONE', #54947, #24698, #14379 ) ;
#36491 = LINE ( 'NONE', #62725, #2206 ) ;
#36492 = ADVANCED_FACE ( 'NONE', ( #46085 ), #20801, .T. ) ;
#36493 = VERTEX_POINT ( 'NONE', #15787 ) ;
#36494 = AXIS2_PLACEMENT_3D ( 'NONE', #26615, #6350, #37823 ) ;
#36495 = EDGE_LOOP ( 'NONE', ( #49909, #15946, #55497, #20476 ) ) ;
#36496 = CARTESIAN_POINT ( 'NONE',  ( 37.00000000000000711, 4.705694406421931860E-17, -3.469127814946512892E-15 ) ) ;
#36497 =( BOUNDED_SURFACE ( )  B_SPLINE_SURFACE ( 3, 1, ( 
 ( #2156, #22433 ),
 ( #48393, #58349 ),
 ( #3160, #12771 ),
 ( #33059, #53365 ) ),
 .UNSPECIFIED., .F., .F., .F. ) 
 B_SPLINE_SURFACE_WITH_KNOTS ( ( 4, 4 ),
 ( 2, 2 ),
 ( 0.000000000000000000, 1.000000000000000000 ),
 ( 0.000000000000000000, 1.000000000000000000 ),
 .UNSPECIFIED. ) 
 GEOMETRIC_REPRESENTATION_ITEM ( )  RATIONAL_B_SPLINE_SURFACE ( (
 ( 1.000000000000000000, 1.000000000000000000),
 ( 0.6933888150995267674, 0.9895912004443193632),
 ( 0.6933888150995267674, 0.9895912004443193632),
 ( 1.000000000000000000, 1.000000000000000000) ) ) 
 REPRESENTATION_ITEM ( '' )  SURFACE ( )  );
#36498 = AXIS2_PLACEMENT_3D ( 'NONE', #55408, #61060, #14179 ) ;
#36499 = ORIENTED_EDGE ( 'NONE', *, *, #18640, .T. ) ;
#36500 = CARTESIAN_POINT ( 'NONE',  ( -22.31213670151049300, -3.777944311993720383, 0.2530575063956070347 ) ) ;
#36501 = CARTESIAN_POINT ( 'NONE',  ( 0.000000000000000000, 2.469490258309423591, 6.482025155313315246 ) ) ;
#36502 = CARTESIAN_POINT ( 'NONE',  ( 2.290907136833271185, 4.792500160339683291, 5.963935563308448096 ) ) ;
#36503 = CARTESIAN_POINT ( 'NONE',  ( -35.00000000000000000, 0.000000000000000000, 0.000000000000000000 ) ) ;
#36504 = ORIENTED_EDGE ( 'NONE', *, *, #1205, .T. ) ;
#36505 = AXIS2_PLACEMENT_3D ( 'NONE', #60716, #51421, #26441 ) ;
#36506 = CARTESIAN_POINT ( 'NONE',  ( 5.514970785353741078, -0.001326349372336609999, -0.004532877335078314314 ) ) ;
#36507 = CYLINDRICAL_SURFACE ( 'NONE', #26858, 5.000000000000000888 ) ;
#36508 = CARTESIAN_POINT ( 'NONE',  ( 1.719304012339844867, -12.64775761152577971, 1.452142814149586902 ) ) ;
#36509 = CARTESIAN_POINT ( 'NONE',  ( 3.152665057733776699, 4.377619405892044568, -6.622010822086680015 ) ) ;
#36510 = EDGE_CURVE ( 'NONE', #37450, #41989, #56501, .T. ) ;
#36511 = AXIS2_PLACEMENT_3D ( 'NONE', #16735, #47997, #17060 ) ;
#36512 = DIRECTION ( 'NONE',  ( 0.3939253465568944290, 0.1500280335741414617, 0.9068155327749447547 ) ) ;
#36513 = CARTESIAN_POINT ( 'NONE',  ( 2.276905613633648962, 2.759436818562492011, 7.130967020394704647 ) ) ;
#36514 =( BOUNDED_SURFACE ( )  B_SPLINE_SURFACE ( 3, 1, ( 
 ( #46613, #56606 ),
 ( #30990, #45971 ),
 ( #21689, #57594 ),
 ( #47292, #61908 ) ),
 .UNSPECIFIED., .F., .F., .F. ) 
 B_SPLINE_SURFACE_WITH_KNOTS ( ( 4, 4 ),
 ( 2, 2 ),
 ( 0.000000000000000000, 1.000000000000000000 ),
 ( 0.000000000000000000, 1.000000000000000000 ),
 .UNSPECIFIED. ) 
 GEOMETRIC_REPRESENTATION_ITEM ( )  RATIONAL_B_SPLINE_SURFACE ( (
 ( 1.000000000000000000, 1.000000000000000000),
 ( 0.9942764183789327692, 0.8450855930916580938),
 ( 0.9942764183789327692, 0.8450855930916580938),
 ( 1.000000000000000000, 1.000000000000000000) ) ) 
 REPRESENTATION_ITEM ( '' )  SURFACE ( )  );
#36515 = ORIENTED_EDGE ( 'NONE', *, *, #30815, .F. ) ;
#36516 = AXIS2_PLACEMENT_3D ( 'NONE', #4855, #39415, #60045 ) ;
#36517 = DIRECTION ( 'NONE',  ( 0.000000000000000000, 0.01356324068817998940, -0.9999080150203990547 ) ) ;
#36518 = EDGE_LOOP ( 'NONE', ( #48200, #51987, #31257, #28006 ) ) ;
#36519 = CARTESIAN_POINT ( 'NONE',  ( -35.04709527796842394, -0.01012471662513968196, -0.007095259204994638913 ) ) ;
#36520 = CARTESIAN_POINT ( 'NONE',  ( 2.000000000000001776, 5.097042323172538580, -5.501832381651401427 ) ) ;
#36521 = DIRECTION ( 'NONE',  ( -1.000000000000000000, 0.000000000000000000, 0.000000000000000000 ) ) ;
#36522 = CARTESIAN_POINT ( 'NONE',  ( 26.08439714455133185, -11.40113243194250359, 3.743551691817327942 ) ) ;
#36523 = DIRECTION ( 'NONE',  ( -1.000000000000000000, 0.000000000000000000, 0.000000000000000000 ) ) ;
#36524 = EDGE_CURVE ( 'NONE', #7826, #65529, #47067, .T. ) ;
#36525 = CIRCLE ( 'NONE', #45019, 1.500000000000000444 ) ;
#36526 = EDGE_LOOP ( 'NONE', ( #6424, #26989, #61821, #65569 ) ) ;
#36527 = ORIENTED_EDGE ( 'NONE', *, *, #39849, .F. ) ;
#36528 = DIRECTION ( 'NONE',  ( 1.000000000000000000, 0.000000000000000000, 0.000000000000000000 ) ) ;
#36529 = ORIENTED_EDGE ( 'NONE', *, *, #45870, .F. ) ;
#36530 = CARTESIAN_POINT ( 'NONE',  ( 0.3534040366549966450, 0.2453052870633498916, 11.99999999999999112 ) ) ;
#36531 = DIRECTION ( 'NONE',  ( 0.000000000000000000, 0.01356324068817998940, -0.9999080150203990547 ) ) ;
#36532 = CYLINDRICAL_SURFACE ( 'NONE', #47983, 4.999999999999999112 ) ;
#36533 = CARTESIAN_POINT ( 'NONE',  ( -27.28563798457901513, 2.528380693767735110, -1.413023339712106141 ) ) ;
#36534 = DIRECTION ( 'NONE',  ( 0.000000000000000000, 0.01356324068817998940, -0.9999080150203989437 ) ) ;
#36535 = CARTESIAN_POINT ( 'NONE',  ( -35.04643116707788408, -0.003844232202718234070, 0.01156612771643049375 ) ) ;
#36536 = CARTESIAN_POINT ( 'NONE',  ( -9.565563870443305916, -2.937820479959865061, 11.63604098864692737 ) ) ;
#36537 = ORIENTED_EDGE ( 'NONE', *, *, #52170, .T. ) ;
#36538 = AXIS2_PLACEMENT_3D ( 'NONE', #52832, #35948, #46607 ) ;
#36539 = CARTESIAN_POINT ( 'NONE',  ( 0.3675815128205912052, 12.13672785388552811, -1.872154644481959895 ) ) ;
#36540 = ORIENTED_EDGE ( 'NONE', *, *, #17502, .F. ) ;
#36541 = CARTESIAN_POINT ( 'NONE',  ( 21.74721992753864441, -13.45929105453497776, -1.114420066137331133 ) ) ;
#36542 = CARTESIAN_POINT ( 'NONE',  ( 2.827825597296803828, 8.073505504738418992, -4.031992772938910008 ) ) ;
#36543 = ORIENTED_EDGE ( 'NONE', *, *, #53865, .F. ) ;
#36544 = CARTESIAN_POINT ( 'NONE',  ( 41.00000000000000711, -25.49198847189177997, 0.7539676769129244338 ) ) ;
#36545 = CARTESIAN_POINT ( 'NONE',  ( -22.27715239060371744, 3.586346956688105436, -0.8317362037004153441 ) ) ;
#36546 = ORIENTED_EDGE ( 'NONE', *, *, #50179, .F. ) ;
#36547 = CARTESIAN_POINT ( 'NONE',  ( 47.00000000000000711, 4.705694406421931860E-17, -3.469127814946512892E-15 ) ) ;
#36548 = ADVANCED_FACE ( 'NONE', ( #51415, #5865 ), #62329, .F. ) ;
#36549 = CLOSED_SHELL ( 'NONE', ( #44276, #27411, #33894, #33695 ) ) ;
#36550 = CARTESIAN_POINT ( 'NONE',  ( -15.59741926309910021, -34.17135967094492344, -7.744809993483719346 ) ) ;
#36551 = CARTESIAN_POINT ( 'NONE',  ( 35.00000000000000000, -9.913596905230168232, -8.017674001891750279 ) ) ;
#36552 = ORIENTED_EDGE ( 'NONE', *, *, #31510, .F. ) ;
#36553 = VERTEX_POINT ( 'NONE', #33398 ) ;
#36554 = CARTESIAN_POINT ( 'NONE',  ( 37.25000000000000711, -1.694065894508793271E-18, 4.500000000000001776 ) ) ;
#36555 = EDGE_CURVE ( 'NONE', #34975, #19210, #38377, .T. ) ;
#36556 = ORIENTED_EDGE ( 'NONE', *, *, #38635, .F. ) ;
#36557 = DIRECTION ( 'NONE',  ( -1.000000000000000000, 0.000000000000000000, 0.000000000000000000 ) ) ;
#36558 = ORIENTED_EDGE ( 'NONE', *, *, #27900, .F. ) ;
#36559 = ORIENTED_EDGE ( 'NONE', *, *, #12308, .T. ) ;
#36560 = VERTEX_POINT ( 'NONE', #7452 ) ;
#36561 = CARTESIAN_POINT ( 'NONE',  ( -35.00000000000000000, 6.657191900728318679, 9.677500615117924809 ) ) ;
#36562 = AXIS2_PLACEMENT_3D ( 'NONE', #12124, #7134, #27414 ) ;
#36563 = DIRECTION ( 'NONE',  ( -1.000000000000000000, 0.000000000000000000, 0.000000000000000000 ) ) ;
#36564 = CARTESIAN_POINT ( 'NONE',  ( 2.373367633546871414, -1.154895193356581196, -7.591069096729007093 ) ) ;
#36566 = EDGE_CURVE ( 'NONE', #63705, #49222, #16189, .T. ) ;
#36565 = CARTESIAN_POINT ( 'NONE',  ( 2.276198483117258586, 2.759333101207245953, -7.130755363255136814 ) ) ;
#36567 = DIRECTION ( 'NONE',  ( 0.000000000000000000, 0.01356324068817998940, -0.9999080150203990547 ) ) ;
#36568 = ORIENTED_EDGE ( 'NONE', *, *, #1859, .F. ) ;
#36569 = CARTESIAN_POINT ( 'NONE',  ( 16.94767514662584418, 12.18332229639727160, 5.815258616132746639 ) ) ;
#36570 = VERTEX_POINT ( 'NONE', #39033 ) ;
#36571 = DIRECTION ( 'NONE',  ( -1.000000000000000000, 0.000000000000000000, 0.000000000000000000 ) ) ;
#36572 = AXIS2_PLACEMENT_3D ( 'NONE', #55698, #40051, #65635 ) ;
#36573 = CARTESIAN_POINT ( 'NONE',  ( -27.10512513516276556, 0.6711200423626966227, 2.256292013315166489 ) ) ;
#36574 = CARTESIAN_POINT ( 'NONE',  ( 0.2650492594609233921, 0.1101156276918464766, -12.24562116224018382 ) ) ;
#36575 = EDGE_CURVE ( 'NONE', #40874, #13727, #42661, .T. ) ;
#36576 = CARTESIAN_POINT ( 'NONE',  ( 0.2648978790185593790, 1.996248716311628479, 12.08224454301449313 ) ) ;
#36577 = CARTESIAN_POINT ( 'NONE',  ( 29.23580817562944745, 7.598662642114378585, 9.298966629028747377 ) ) ;
#36579 = DIRECTION ( 'NONE',  ( 1.000000000000000000, 0.000000000000000000, 0.000000000000000000 ) ) ;
#36578 = AXIS2_PLACEMENT_3D ( 'NONE', #12514, #13195, #48780 ) ;
#36580 = CIRCLE ( 'NONE', #31302, 7.499999999999988454 ) ;
#36581 = ORIENTED_EDGE ( 'NONE', *, *, #57506, .F. ) ;
#36582 = CARTESIAN_POINT ( 'NONE',  ( -35.00000000000000000, 12.15823808070322798, 0.8294751490779768144 ) ) ;
#36583 = ORIENTED_EDGE ( 'NONE', *, *, #51284, .T. ) ;
#36584 = CARTESIAN_POINT ( 'NONE',  ( 3.152665057736177445, 3.161213418915486795, 7.281573230473766145 ) ) ;
#36585 = CARTESIAN_POINT ( 'NONE',  ( 17.69916095700584080, -28.67478364583445583, -8.521665482016093307 ) ) ;
#36586 = CARTESIAN_POINT ( 'NONE',  ( 9.836964722002420558, -27.64452029744604999, 14.41904541651817340 ) ) ;
#36587 = CARTESIAN_POINT ( 'NONE',  ( -27.08935880048753120, -0.6272370006475039839, -2.219773948423735099 ) ) ;
#36588 = CYLINDRICAL_SURFACE ( 'NONE', #15827, 4.000030059823568074 ) ;
#36589 = VERTEX_POINT ( 'NONE', #32707 ) ;
#36590 = AXIS2_PLACEMENT_3D ( 'NONE', #5811, #50031, #5135 ) ;
#36591 = VECTOR ( 'NONE', #63729, 1000.000000000000000 ) ;
#36592 = CARTESIAN_POINT ( 'NONE',  ( -35.00000000000000000, 5.273331777780488672, -10.49591321039675229 ) ) ;
#36593 = CARTESIAN_POINT ( 'NONE',  ( 0.2706063244538028378, 2.299194104693242036, -12.03021891034989110 ) ) ;
#36594 = LINE ( 'NONE', #61516, #35352 ) ;
#36595 = CARTESIAN_POINT ( 'NONE',  ( 2.000000000000001776, -6.643843315911796665, -1.507714007300762660 ) ) ;
#36596 = LINE ( 'NONE', #26291, #63720 ) ;
#36597 = LINE ( 'NONE', #21645, #39167 ) ;
#36598 = CARTESIAN_POINT ( 'NONE',  ( 35.00000000000000000, 10.62137734850267989, 5.015831474386340361 ) ) ;
#36600 = AXIS2_PLACEMENT_3D ( 'NONE', #29042, #49351, #3797 ) ;
#36599 = APPLICATION_CONTEXT ( 'automotive_design' ) ;
#36601 = CARTESIAN_POINT ( 'NONE',  ( 3.152665057734108878, -7.886634106564198277, 0.9030954876737806725 ) ) ;
#36602 = CARTESIAN_POINT ( 'NONE',  ( 2.242819959140646358, 0.1024002568250429734, -7.634209046698936518 ) ) ;
#36603 = EDGE_CURVE ( 'NONE', #59070, #7715, #59324, .T. ) ;
#36604 = VERTEX_POINT ( 'NONE', #2508 ) ;
#36605 = VERTEX_POINT ( 'NONE', #33054 ) ;
#36606 = CARTESIAN_POINT ( 'NONE',  ( 2.524535260912772472, -6.580044328001124043, 4.054303386867624148 ) ) ;
#36607 = CARTESIAN_POINT ( 'NONE',  ( 45.77739315166651579, -0.8244463642989235952, 12.03838484699754652 ) ) ;
#36608 = CARTESIAN_POINT ( 'NONE',  ( 0.8320506296491662068, -7.696193170530679417, 9.767350172724400537 ) ) ;
#36609 = DIRECTION ( 'NONE',  ( -1.000000000000000000, 0.000000000000000000, 0.000000000000000000 ) ) ;
#36610 = VERTEX_POINT ( 'NONE', #17778 ) ;
#36611 = VERTEX_POINT ( 'NONE', #28092 ) ;
#36612 = ORIENTED_EDGE ( 'NONE', *, *, #18240, .F. ) ;
#36613 = CARTESIAN_POINT ( 'NONE',  ( 35.00000000000000000, 9.908974237959730758, 6.307491713048920090 ) ) ;
#36614 = AXIS2_PLACEMENT_3D ( 'NONE', #30671, #50981, #55297 ) ;
#36615 = CARTESIAN_POINT ( 'NONE',  ( -22.31328051695926007, 1.076152733467212741, 3.633840107626929328 ) ) ;
#36616 = ADVANCED_FACE ( 'NONE', ( #27742 ), #4475, .F. ) ;
#36617 = ORIENTED_EDGE ( 'NONE', *, *, #52044, .F. ) ;
#36618 = CARTESIAN_POINT ( 'NONE',  ( 37.25000000000000711, -27.21021009056489248, -4.500000000000000888 ) ) ;
#36619 = DIRECTION ( 'NONE',  ( -1.000000000000000000, -0.000000000000000000, 0.000000000000000000 ) ) ;
#36620 = VERTEX_POINT ( 'NONE', #53361 ) ;
#36621 = CARTESIAN_POINT ( 'NONE',  ( -22.29677679919927868, 0.2674217835791047326, 3.730758197825078337 ) ) ;
#36622 = EDGE_CURVE ( 'NONE', #15993, #41767, #45498, .T. ) ;
#36623 = CARTESIAN_POINT ( 'NONE',  ( 10.72528909898949401, -29.54774166153168835, -10.19639468772673219 ) ) ;
#36624 = CARTESIAN_POINT ( 'NONE',  ( 24.88498457265327346, -1.132774965307099979, 11.94809602833619699 ) ) ;
#36625 = ORIENTED_EDGE ( 'NONE', *, *, #24094, .F. ) ;
#36626 = DIRECTION ( 'NONE',  ( -1.000000000000000000, -0.000000000000000000, 0.000000000000000000 ) ) ;
#36627 = EDGE_CURVE ( 'NONE', #63262, #14422, #34037, .T. ) ;
#36628 = B_SPLINE_CURVE_WITH_KNOTS ( 'NONE', 3,
 ( #47766, #22836, #42098, #52446, #62081, #37114, #57416, #43091, #16532, #32452, #46778, #27155, #56788, #63367, #17177, #11846, #53078, #32127 ),
 .UNSPECIFIED., .F., .F.,
 ( 4, 2, 2, 2, 2, 2, 2, 2, 4 ),
 ( 0.004326619632261259271, 0.005066079377112942678, 0.005805539121964627819, 0.006544998866816312960, 0.007284458611667997234, 0.008023918356519681508, 0.008763378101371366649, 0.009502837846223051790, 0.01024229759107473693 ),
 .UNSPECIFIED. ) ;
#36629 = ORIENTED_EDGE ( 'NONE', *, *, #64470, .F. ) ;
#36630 = AXIS2_PLACEMENT_3D ( 'NONE', #1639, #19705, #39639 ) ;
#36631 = FACE_OUTER_BOUND ( 'NONE', #31802, .T. ) ;
#36632 = CARTESIAN_POINT ( 'NONE',  ( 2.000000000000001776, -1.779948802829750543, -6.576141558201276993 ) ) ;
#36633 = CARTESIAN_POINT ( 'NONE',  ( -12.63451720667688072, -33.87771254755728734, 9.962109630954579131 ) ) ;
#36634 = FACE_OUTER_BOUND ( 'NONE', #32610, .T. ) ;
#36635 = DIRECTION ( 'NONE',  ( 0.000000000000000000, 0.01356324068818000848, -0.9999080150203990547 ) ) ;
#36637 = ADVANCED_FACE ( 'NONE', ( #30037 ), #50005, .T. ) ;
#36636 = CARTESIAN_POINT ( 'NONE',  ( 9.746551792753381349, 1.290882055502603931, 11.93221949516759750 ) ) ;
#36638 = CARTESIAN_POINT ( 'NONE',  ( -30.18541646480307250, -2.213624975795535299, -13.34140603515871604 ) ) ;
#36639 = CARTESIAN_POINT ( 'NONE',  ( 8.500415212161144041, 5.252658130439442630, -10.79141609758813480 ) ) ;
#36640 = VERTEX_POINT ( 'NONE', #40673 ) ;
#36641 = CARTESIAN_POINT ( 'NONE',  ( -28.67667724226168602, 1.049259427760474983, 1.574547667005656404 ) ) ;
#36642 = CIRCLE ( 'NONE', #46245, 4.999999999999999112 ) ;
#36643 = VERTEX_POINT ( 'NONE', #25376 ) ;
#36644 = FACE_OUTER_BOUND ( 'NONE', #45784, .T. ) ;
#36645 = EDGE_CURVE ( 'NONE', #25311, #64820, #35260, .T. ) ;
#36646 = CARTESIAN_POINT ( 'NONE',  ( 37.00000000000000711, 11.70009620280413110, 1.039216533672774112 ) ) ;
#36647 = ORIENTED_EDGE ( 'NONE', *, *, #32545, .T. ) ;
#36648 = DIRECTION ( 'NONE',  ( 0.000000000000000000, 0.000000000000000000, 1.000000000000000000 ) ) ;
#36649 = FACE_OUTER_BOUND ( 'NONE', #58925, .T. ) ;
#36650 = CYLINDRICAL_SURFACE ( 'NONE', #33346, 6.595312090839647645 ) ;
#36651 = CARTESIAN_POINT ( 'NONE',  ( -35.04582288351658548, 0.01249938581186572396, 0.002280196168871053385 ) ) ;
#36652 = CIRCLE ( 'NONE', #2699, 5.000000000000000888 ) ;
#36653 = DIRECTION ( 'NONE',  ( 0.000000000000000000, 0.000000000000000000, 1.000000000000000000 ) ) ;
#36654 = ORIENTED_EDGE ( 'NONE', *, *, #11958, .T. ) ;
#36655 = CARTESIAN_POINT ( 'NONE',  ( 1.937114397841935398, -7.538912286488415049, 10.38782037574614137 ) ) ;
#36656 = ADVANCED_FACE ( 'NONE', ( #19087 ), #54350, .T. ) ;
#36657 = ORIENTED_EDGE ( 'NONE', *, *, #32266, .F. ) ;
#36658 = CARTESIAN_POINT ( 'NONE',  ( 2.963017218115608031, -6.272673870919120986, 4.761166637500490850 ) ) ;
#36659 = EDGE_CURVE ( 'NONE', #24086, #4327, #5535, .T. ) ;
#36660 = DIRECTION ( 'NONE',  ( 0.000000000000000000, 0.01356324068817998940, -0.9999080150203989437 ) ) ;
#36661 = CARTESIAN_POINT ( 'NONE',  ( 5.520433897694421610, 0.01491416502703810966, -0.002108682515300329928 ) ) ;
#36662 = ORIENTED_EDGE ( 'NONE', *, *, #18479, .T. ) ;
#36663 = CARTESIAN_POINT ( 'NONE',  ( 0.3610902822527234379, -4.444884365376528201, -11.44530431865297793 ) ) ;
#36664 = VECTOR ( 'NONE', #60959, 1000.000000000000000 ) ;
#36665 = CARTESIAN_POINT ( 'NONE',  ( 29.10724821778045168, 10.83570424563273882, 8.063006356801381003 ) ) ;
#36666 = DIRECTION ( 'NONE',  ( -1.000000000000000000, 0.000000000000000000, 0.000000000000000000 ) ) ;
#36667 = DIRECTION ( 'NONE',  ( 1.000000000000000000, 0.000000000000000000, 0.000000000000000000 ) ) ;
#36668 = CARTESIAN_POINT ( 'NONE',  ( 9.166623160528491354, 6.959806824555357707, 11.57358056643181676 ) ) ;
#36669 = DIRECTION ( 'NONE',  ( -1.000000000000000000, 0.000000000000000000, -0.000000000000000000 ) ) ;
#36670 = CARTESIAN_POINT ( 'NONE',  ( 2.256373768223412846, -5.765785888499252998, 5.011614056001910456 ) ) ;
#36671 = CARTESIAN_POINT ( 'NONE',  ( -23.41523303002442091, -2.683951991546276172, 3.856096202952846941 ) ) ;
#36672 = EDGE_CURVE ( 'NONE', #2417, #57580, #28874, .T. ) ;
#36673 = ORIENTED_EDGE ( 'NONE', *, *, #7126, .T. ) ;
#36674 = DIRECTION ( 'NONE',  ( 0.000000000000000000, 0.8696919319575202589, 0.4935949184179230231 ) ) ;
#36675 = CARTESIAN_POINT ( 'NONE',  ( 0.2869720083484376127, -12.25163264065381341, -0.2084396331387939061 ) ) ;
#36676 = CIRCLE ( 'NONE', #12235, 5.000000000000000000 ) ;
#36677 = EDGE_LOOP ( 'NONE', ( #23642, #56149, #24236, #51719 ) ) ;
#36678 = DIRECTION ( 'NONE',  ( -0.000000000000000000, -0.000000000000000000, -1.000000000000000000 ) ) ;
#36679 = CARTESIAN_POINT ( 'NONE',  ( 3.353434147978485047, 5.295522092567586547, -10.77037561067536053 ) ) ;
#36680 = CARTESIAN_POINT ( 'NONE',  ( -7.971178810570282103, 8.542040713314987599, -10.47297027589238816 ) ) ;
#36681 = VERTEX_POINT ( 'NONE', #3824 ) ;
#36682 = CARTESIAN_POINT ( 'NONE',  ( -22.66110217412718697, -2.622110956932569348, 4.192227617777433579 ) ) ;
#36683 = ORIENTED_EDGE ( 'NONE', *, *, #5192, .F. ) ;
#36684 = EDGE_CURVE ( 'NONE', #41624, #36171, #3413, .T. ) ;
#36685 = DIRECTION ( 'NONE',  ( 0.000000000000000000, 0.000000000000000000, -1.000000000000000000 ) ) ;
#36686 = ORIENTED_EDGE ( 'NONE', *, *, #49325, .T. ) ;
#36687 = ORIENTED_EDGE ( 'NONE', *, *, #62506, .F. ) ;
#36688 = AXIS2_PLACEMENT_3D ( 'NONE', #26317, #16667, #7022 ) ;
#36689 = CARTESIAN_POINT ( 'NONE',  ( -27.08426504710140392, -1.649100202714204988, 1.591094357919263569 ) ) ;
#36690 = EDGE_CURVE ( 'NONE', #36827, #55926, #14086, .T. ) ;
#36691 = ORIENTED_EDGE ( 'NONE', *, *, #34790, .F. ) ;
#36692 = CARTESIAN_POINT ( 'NONE',  ( -25.68896891816097039, -10.12442625007511232, 6.443155052333052524 ) ) ;
#36693 = CARTESIAN_POINT ( 'NONE',  ( -22.31328051695926007, -3.633840107626937765, 1.076152733467191869 ) ) ;
#36694 = DIRECTION ( 'NONE',  ( 0.000000000000000000, -0.7617968321374810614, -0.6478160128812026075 ) ) ;
#36695 = CARTESIAN_POINT ( 'NONE',  ( 9.588299228810004848, 6.688210644983048958, 9.969111302884179793 ) ) ;
#36696 = ORIENTED_EDGE ( 'NONE', *, *, #13430, .F. ) ;
#36697 =( BOUNDED_SURFACE ( )  B_SPLINE_SURFACE ( 3, 1, ( 
 ( #8802, #34050 ),
 ( #33413, #28742 ),
 ( #49692, #23432 ),
 ( #38391, #19099 ) ),
 .UNSPECIFIED., .F., .F., .F. ) 
 B_SPLINE_SURFACE_WITH_KNOTS ( ( 4, 4 ),
 ( 2, 2 ),
 ( 0.000000000000000000, 1.000000000000000000 ),
 ( 0.000000000000000000, 1.000000000000000000 ),
 .UNSPECIFIED. ) 
 GEOMETRIC_REPRESENTATION_ITEM ( )  RATIONAL_B_SPLINE_SURFACE ( (
 ( 1.000000000000000000, 1.000000000000000000),
 ( 0.9257577194822556033, 0.9980522942447415113),
 ( 0.9257577194822556033, 0.9980522942447415113),
 ( 1.000000000000000000, 1.000000000000000000) ) ) 
 REPRESENTATION_ITEM ( '' )  SURFACE ( )  );
#36698 = DIRECTION ( 'NONE',  ( -1.000000000000000000, 0.000000000000000000, 0.000000000000000000 ) ) ;
#36699 = CARTESIAN_POINT ( 'NONE',  ( 0.8665813290829081916, -31.03691730605172694, 14.44326482629603881 ) ) ;
#36700 = CARTESIAN_POINT ( 'NONE',  ( -36.00000000000000711, -3.805206332242558886, 12.16893194857548899 ) ) ;
#36702 = VERTEX_POINT ( 'NONE', #4122 ) ;
#36701 = DIRECTION ( 'NONE',  ( -1.000000000000000000, 0.000000000000000000, 0.000000000000000000 ) ) ;
#36703 = DIRECTION ( 'NONE',  ( 1.000000000000000000, 0.000000000000000000, -0.000000000000000000 ) ) ;
#36704 = ADVANCED_FACE ( 'NONE', ( #24390 ), #41343, .F. ) ;
#36705 = VERTEX_POINT ( 'NONE', #65287 ) ;
#36706 = CARTESIAN_POINT ( 'NONE',  ( 3.152665057734095555, 3.546019893116337141, 7.102135024645864547 ) ) ;
#36707 = EDGE_LOOP ( 'NONE', ( #35125, #26877, #59276, #13634 ) ) ;
#36708 = CARTESIAN_POINT ( 'NONE',  ( 2.241352910868908310, 4.970878533273761946, 5.794346703933863196 ) ) ;
#36709 = DIRECTION ( 'NONE',  ( -1.000000000000000000, -0.000000000000000000, 0.000000000000000000 ) ) ;
#36710 = CARTESIAN_POINT ( 'NONE',  ( 2.259830038564998311, -7.639319632525574555, -0.1377140217659982568 ) ) ;
#36711 = VECTOR ( 'NONE', #49833, 1000.000000000000000 ) ;
#36712 = B_SPLINE_CURVE_WITH_KNOTS ( 'NONE', 3,
 ( #61807, #5987, #55849, #51202, #36545, #10946, #7498, #31233, #56853, #10599, #43075, #17499, #2550, #63353, #16263, #10276, #42739, #20605, #17817, #972, #56158, #61467 ),
 .UNSPECIFIED., .F., .F.,
 ( 4, 3, 3, 3, 3, 3, 3, 4 ),
 ( 0.000000000000000000, 6.990956068646414663E-05, 0.0001398191187764043317, 0.0002097286751720214631, 0.0002796382307041358844, 0.0003495477861619810203, 0.0004194573423310285747, 0.0005586102576333144961 ),
 .UNSPECIFIED. ) ;
#36713 = ORIENTED_EDGE ( 'NONE', *, *, #13778, .F. ) ;
#36714 = CARTESIAN_POINT ( 'NONE',  ( -47.00000000000000711, 0.000000000000000000, 0.000000000000000000 ) ) ;
#36715 = CARTESIAN_POINT ( 'NONE',  ( 5.516018279890452902, -0.004525000489649737799, -0.005042957932158631355 ) ) ;
#36716 = DIRECTION ( 'NONE',  ( 0.000000000000000000, 0.000000000000000000, 1.000000000000000000 ) ) ;
#36717 = ORIENTED_EDGE ( 'NONE', *, *, #25004, .T. ) ;
#36718 = ORIENTED_EDGE ( 'NONE', *, *, #927, .T. ) ;
#36719 = FACE_OUTER_BOUND ( 'NONE', #42663, .T. ) ;
#36720 = ORIENTED_EDGE ( 'NONE', *, *, #49929, .F. ) ;
#36721 = EDGE_CURVE ( 'NONE', #6288, #24332, #40540, .T. ) ;
#36722 = EDGE_CURVE ( 'NONE', #18994, #30591, #49068, .T. ) ;
#36723 = ORIENTED_EDGE ( 'NONE', *, *, #52524, .T. ) ;
#36724 = DIRECTION ( 'NONE',  ( 1.000000000000000000, 0.000000000000000000, 0.000000000000000000 ) ) ;
#36725 = CYLINDRICAL_SURFACE ( 'NONE', #63599, 4.999999999999999112 ) ;
#36726 = DIRECTION ( 'NONE',  ( -0.000000000000000000, -1.000000000000000000, -0.000000000000000000 ) ) ;
#36727 = CARTESIAN_POINT ( 'NONE',  ( -22.28856623400852399, 1.018212315222208675, 3.573466130470470237 ) ) ;
#36728 = EDGE_CURVE ( 'NONE', #56510, #45342, #4798, .T. ) ;
#36729 = DIRECTION ( 'NONE',  ( 0.000000000000000000, 0.9467777615094560284, 0.3218879778916007295 ) ) ;
#36730 = CYLINDRICAL_SURFACE ( 'NONE', #47972, 12.18649999999999878 ) ;
#36731 = CIRCLE ( 'NONE', #4891, 12.18649999999999878 ) ;
#36732 = ADVANCED_FACE ( 'NONE', ( #35672 ), #26049, .T. ) ;
#36733 = LINE ( 'NONE', #47382, #38547 ) ;
#36734 = EDGE_CURVE ( 'NONE', #45182, #18937, #11389, .T. ) ;
#36735 = AXIS2_PLACEMENT_3D ( 'NONE', #21549, #16560, #25884 ) ;
#36736 = ORIENTED_EDGE ( 'NONE', *, *, #34401, .F. ) ;
#36737 = EDGE_CURVE ( 'NONE', #1560, #16664, #7364, .T. ) ;
#36738 = FACE_OUTER_BOUND ( 'NONE', #6194, .T. ) ;
#36739 = CARTESIAN_POINT ( 'NONE',  ( -2.952869152607111136, -4.384817011589735358, 11.17020052527586138 ) ) ;
#36740 = AXIS2_PLACEMENT_3D ( 'NONE', #57331, #63285, #11754 ) ;
#36741 = CARTESIAN_POINT ( 'NONE',  ( 0.2956976708475473892, 4.397965666276587804, -11.44006538352181757 ) ) ;
#36742 = FACE_OUTER_BOUND ( 'NONE', #64960, .T. ) ;
#36743 = CARTESIAN_POINT ( 'NONE',  ( 16.94767514662583352, -12.18332229639725206, 5.815258616132748415 ) ) ;
#36744 = CARTESIAN_POINT ( 'NONE',  ( 3.941273214955026472, 6.020113200743838711, -10.38315790873123134 ) ) ;
#36745 = DIRECTION ( 'NONE',  ( 0.000000000000000000, 0.01356324068817998940, -0.9999080150203990547 ) ) ;
#36746 = ORIENTED_EDGE ( 'NONE', *, *, #50736, .F. ) ;
#36747 = CARTESIAN_POINT ( 'NONE',  ( -37.00000000000000711, -10.25474254703948418, -6.584150480049660636 ) ) ;
#36748 = CARTESIAN_POINT ( 'NONE',  ( 0.3401186441510232750, -1.878666403202251534, -12.12646044229291853 ) ) ;
#36749 = DIRECTION ( 'NONE',  ( 0.000000000000000000, -0.6051742151937716807, 0.7960930657056387583 ) ) ;
#36750 = DIRECTION ( 'NONE',  ( -1.000000000000000000, -1.836970198721029688E-16, 0.000000000000000000 ) ) ;
#36751 = B_SPLINE_CURVE_WITH_KNOTS ( 'NONE', 3,
 ( #34448, #60056, #39101, #9484, #8856, #59729, #45090, #18538, #29149, #23843, #38792, #18840, #3885, #44103, #14794, #59395, #65355, #64685, #34105, #24146, #14156, #29768 ),
 .UNSPECIFIED., .F., .F.,
 ( 4, 2, 2, 2, 2, 2, 2, 2, 2, 2, 4 ),
 ( 0.003235587836267140010, 0.004470998178832687707, 0.005088703350115462640, 0.005706408521398236705, 0.006941818863963784836, 0.008177229206529331232, 0.009412639549094879363, 0.01064804989166042749, 0.01126575506294320156, 0.01188346023422597736, 0.01311887057679152896 ),
 .UNSPECIFIED. ) ;
#36752 = EDGE_CURVE ( 'NONE', #33727, #16920, #20380, .T. ) ;
#36753 = CARTESIAN_POINT ( 'NONE',  ( 8.957787800376372900, 4.005583820372585535, -12.89440042502234363 ) ) ;
#36754 = CARTESIAN_POINT ( 'NONE',  ( -35.00000000000000000, -4.339012074900030491, 10.91536515067646818 ) ) ;
#36755 = ORIENTED_EDGE ( 'NONE', *, *, #37931, .F. ) ;
#36756 = CARTESIAN_POINT ( 'NONE',  ( -19.47984447937493613, -3.750539801530005768, -12.96855624952674724 ) ) ;
#36757 = CYLINDRICAL_SURFACE ( 'NONE', #46050, 4.445031439545090279 ) ;
#36758 = CARTESIAN_POINT ( 'NONE',  ( 2.284126774967666140, 1.171808575345623327, 7.558363379199187548 ) ) ;
#36759 = VERTEX_POINT ( 'NONE', #35987 ) ;
#36760 = CARTESIAN_POINT ( 'NONE',  ( 2.491965175174354119, 6.787433375639490230, 3.673871285745579307 ) ) ;
#36761 = CARTESIAN_POINT ( 'NONE',  ( -15.47675659650424329, 7.964312849573895292, -8.976208599246165321 ) ) ;
#36762 = CARTESIAN_POINT ( 'NONE',  ( 0.000000000000000000, 3.795144977083636739, 6.468916029978800886 ) ) ;
#36763 = EDGE_CURVE ( 'NONE', #50717, #54601, #19345, .T. ) ;
#36765 = VERTEX_POINT ( 'NONE', #16045 ) ;
#36764 = CYLINDRICAL_SURFACE ( 'NONE', #65724, 4.999999999999999112 ) ;
#36766 = DIRECTION ( 'NONE',  ( 1.000000000000000000, -0.000000000000000000, -0.000000000000000000 ) ) ;
#36767 = B_SPLINE_CURVE_WITH_KNOTS ( 'NONE', 3,
 ( #34337, #40632, #23609, #43533, #53866, #58533, #59185, #53551, #8304, #48245, #8960, #7652, #28577, #27935, #63815, #32893 ),
 .UNSPECIFIED., .F., .F.,
 ( 4, 3, 3, 3, 3, 4 ),
 ( 5.963111948670274387E-19, 0.0003017745587525257891, 0.0006035491769808736320, 0.0009053241094668170071, 0.001207275924540513433, 0.001510325902534028712 ),
 .UNSPECIFIED. ) ;
#36768 = AXIS2_PLACEMENT_3D ( 'NONE', #17736, #63583, #8400 ) ;
#36769 = CYLINDRICAL_SURFACE ( 'NONE', #18104, 5.000000000000000888 ) ;
#36770 = ORIENTED_EDGE ( 'NONE', *, *, #38371, .F. ) ;
#36771 = DIRECTION ( 'NONE',  ( 0.000000000000000000, -0.01356324068817998940, 0.9999080150203990547 ) ) ;
#36772 = DIRECTION ( 'NONE',  ( 0.000000000000000000, -0.01356324068817998940, 0.9999080150203990547 ) ) ;
#36774 = AXIS2_PLACEMENT_3D ( 'NONE', #52642, #7066, #11711 ) ;
#36773 = CARTESIAN_POINT ( 'NONE',  ( 35.00000000000000000, 5.814360711498443912, 10.70999494708485678 ) ) ;
#36775 = DIRECTION ( 'NONE',  ( -1.000000000000000000, -0.000000000000000000, 0.000000000000000000 ) ) ;
#36776 = PLANE ( 'NONE',  #20399 ) ;
#36777 = CARTESIAN_POINT ( 'NONE',  ( 35.00000000000000000, 11.73463472867580393, 3.287724142101285274 ) ) ;
#36779 = ORIENTED_EDGE ( 'NONE', *, *, #65600, .T. ) ;
#36778 = CARTESIAN_POINT ( 'NONE',  ( 0.2717059086739053719, 11.44824199474648552, -4.354191483751156611 ) ) ;
#36780 = EDGE_CURVE ( 'NONE', #54418, #65236, #17198, .T. ) ;
#36781 = EDGE_LOOP ( 'NONE', ( #44747, #40053, #14388, #5286 ) ) ;
#36782 = CARTESIAN_POINT ( 'NONE',  ( 2.241532322987418890, -0.01048837931141704399, 7.634455956583345859 ) ) ;
#36783 = EDGE_LOOP ( 'NONE', ( #5513, #11649, #48251, #38569 ) ) ;
#36784 = CARTESIAN_POINT ( 'NONE',  ( 0.000000000000000000, 0.000000000000000000, 0.000000000000000000 ) ) ;
#36785 = EDGE_CURVE ( 'NONE', #65370, #32930, #36322, .T. ) ;
#36786 = DIRECTION ( 'NONE',  ( 0.000000000000000000, -0.2149704402110317047, 0.9766205557100849921 ) ) ;
#36787 = CARTESIAN_POINT ( 'NONE',  ( 2.990245332647718079, 0.9653152459624684267, 8.426135047918773324 ) ) ;
#36788 = B_SPLINE_CURVE_WITH_KNOTS ( 'NONE', 3,
 ( #33643, #38961, #13673, #29309, #49296, #59571, #9329, #28647, #14003, #19342, #49604, #29614, #24003, #4044, #50263, #48953 ),
 .UNSPECIFIED., .F., .F.,
 ( 4, 3, 3, 3, 3, 4 ),
 ( 0.000000000000000000, 0.0002999043160757735530, 0.0005998071753051757021, 0.0008997092107375666671, 0.001204458948195450806, 0.001510329163476011082 ),
 .UNSPECIFIED. ) ;
#36789 = CYLINDRICAL_SURFACE ( 'NONE', #11807, 12.18650000000000055 ) ;
#36790 = VERTEX_POINT ( 'NONE', #46003 ) ;
#36791 = CARTESIAN_POINT ( 'NONE',  ( 5.516018279890452902, 0.005976902763919037485, -0.003191189039764858598 ) ) ;
#36792 = FACE_OUTER_BOUND ( 'NONE', #38092, .T. ) ;
#36793 = DIRECTION ( 'NONE',  ( 0.000000000000000000, -0.9796553971857762111, -0.2006870767258790988 ) ) ;
#36794 = ORIENTED_EDGE ( 'NONE', *, *, #46641, .F. ) ;
#36795 = VERTEX_POINT ( 'NONE', #51657 ) ;
#36796 = CARTESIAN_POINT ( 'NONE',  ( 28.67692623539176466, -11.72617184382499644, 6.700251934688060018 ) ) ;
#36797 = ORIENTED_EDGE ( 'NONE', *, *, #11782, .T. ) ;
#36798 = DIRECTION ( 'NONE',  ( 0.000000000000000000, 0.01356324068817998940, -0.9999080150203989437 ) ) ;
#36799 = CARTESIAN_POINT ( 'NONE',  ( 0.3665391374699472626, -3.952034409876374443, 11.62960183138725689 ) ) ;
#36800 = DIRECTION ( 'NONE',  ( 1.000000000000000000, -0.000000000000000000, 0.000000000000000000 ) ) ;
#36801 = ADVANCED_FACE ( 'NONE', ( #6101 ), #16707, .T. ) ;
#36802 = CARTESIAN_POINT ( 'NONE',  ( 1.836970198721029589E-15, -30.00000000000000000, 15.00000000000000000 ) ) ;
#36803 = DIRECTION ( 'NONE',  ( 0.000000000000000000, -0.01356324068818000328, 0.9999080150203990547 ) ) ;
#36804 = CARTESIAN_POINT ( 'NONE',  ( 1.719304012338834786, 2.961219984257995819, 12.38166659046419227 ) ) ;
#36805 = EDGE_CURVE ( 'NONE', #28625, #29524, #46644, .T. ) ;
#36806 = LINE ( 'NONE', #52107, #411 ) ;
#36807 = ORIENTED_EDGE ( 'NONE', *, *, #58622, .T. ) ;
#36808 = DIRECTION ( 'NONE',  ( 0.000000000000000000, 0.01356324068817998940, -0.9999080150203990547 ) ) ;
#36809 = ORIENTED_EDGE ( 'NONE', *, *, #10181, .F. ) ;
#36810 = EDGE_CURVE ( 'NONE', #58284, #33621, #16145, .T. ) ;
#36811 = CARTESIAN_POINT ( 'NONE',  ( 3.047904605210438156, 4.313929735713965208, -6.622084192655445456 ) ) ;
#36812 = CARTESIAN_POINT ( 'NONE',  ( -1.734723475976807094E-15, -3.469446951953614189E-15, 25.00000000000000000 ) ) ;
#36813 = CARTESIAN_POINT ( 'NONE',  ( 3.152665057734040488, 0.000000000000000000, 0.000000000000000000 ) ) ;
#36814 = CARTESIAN_POINT ( 'NONE',  ( -35.00000000000000000, 1.113475361586490298, 12.70128625845193326 ) ) ;
#36815 = DIRECTION ( 'NONE',  ( 0.000000000000000000, 0.3218879778915972878, -0.9467777615094571386 ) ) ;
#36816 = VECTOR ( 'NONE', #52091, 1000.000000000000000 ) ;
#36817 = CYLINDRICAL_SURFACE ( 'NONE', #51054, 5.000000000000000888 ) ;
#36818 = ORIENTED_EDGE ( 'NONE', *, *, #65487, .F. ) ;
#36819 = VERTEX_POINT ( 'NONE', #40999 ) ;
#36820 = LINE ( 'NONE', #15222, #62000 ) ;
#36821 = EDGE_CURVE ( 'NONE', #14095, #60939, #21467, .T. ) ;
#36822 = ORIENTED_EDGE ( 'NONE', *, *, #27108, .F. ) ;
#36823 = CARTESIAN_POINT ( 'NONE',  ( 1.000000000000000888, -6.664893814313694875, -3.439359016433563898 ) ) ;
#36824 = CARTESIAN_POINT ( 'NONE',  ( -36.00000000000000711, -9.506317355798310942, -8.496612874013262484 ) ) ;
#36825 = CARTESIAN_POINT ( 'NONE',  ( 2.255723233588966536, 4.808373255828867876, 5.936060085173582301 ) ) ;
#36826 = CARTESIAN_POINT ( 'NONE',  ( 2.261269890822072082, 1.464004156081748942, -7.499479675451353522 ) ) ;
#36827 = VERTEX_POINT ( 'NONE', #1766 ) ;
#36828 = CARTESIAN_POINT ( 'NONE',  ( -35.04582288351658548, -0.008224400713808234509, 0.009684687560342908341 ) ) ;
#36829 = LINE ( 'NONE', #5949, #36404 ) ;
#36830 = CARTESIAN_POINT ( 'NONE',  ( -37.00000000000000711, 10.54834585426219995, 6.102719229070713070 ) ) ;
#36831 = CARTESIAN_POINT ( 'NONE',  ( -30.66651853351973145, -3.164325622109353642, 24.36290982288814888 ) ) ;
#36832 = PRODUCT_RELATED_PRODUCT_CATEGORY ( 'part', '', ( #33856 ) ) ;
#36833 = CARTESIAN_POINT ( 'NONE',  ( 0.3002738374340819805, 6.323236184341269883, -10.50101454678637936 ) ) ;
#36834 = EDGE_CURVE ( 'NONE', #2995, #41256, #1311, .T. ) ;
#36835 = DIRECTION ( 'NONE',  ( 0.000000000000000000, 0.000000000000000000, -1.000000000000000000 ) ) ;
#36836 = ORIENTED_EDGE ( 'NONE', *, *, #9844, .F. ) ;
#36837 = ORIENTED_EDGE ( 'NONE', *, *, #12276, .F. ) ;
#36838 = DIRECTION ( 'NONE',  ( 1.000000000000000000, 0.000000000000000000, 0.000000000000000000 ) ) ;
#36839 = CARTESIAN_POINT ( 'NONE',  ( 0.000000000000000000, -0.4129979343797593461, 6.800241778083677247 ) ) ;
#36840 = DIRECTION ( 'NONE',  ( 0.000000000000000000, 0.01356324068817998940, -0.9999080150203990547 ) ) ;
#36841 = EDGE_CURVE ( 'NONE', #9063, #65109, #58666, .T. ) ;
#36842 = CARTESIAN_POINT ( 'NONE',  ( -35.04709527796842394, 0.01012471662513447779, 0.007095259204982495849 ) ) ;
#36843 = CARTESIAN_POINT ( 'NONE',  ( -37.00000000000000711, 1.463443770872774774, 12.09831040184924866 ) ) ;
#36844 = ORIENTED_EDGE ( 'NONE', *, *, #53702, .F. ) ;
#36845 = ORIENTED_EDGE ( 'NONE', *, *, #9606, .F. ) ;
#36846 = FACE_OUTER_BOUND ( 'NONE', #45495, .T. ) ;
#36847 = ORIENTED_EDGE ( 'NONE', *, *, #56783, .F. ) ;
#36848 = DIRECTION ( 'NONE',  ( -1.000000000000000000, 0.000000000000000000, 0.000000000000000000 ) ) ;
#36849 = DIRECTION ( 'NONE',  ( 0.000000000000000000, 0.01356324068817998940, -0.9999080150203990547 ) ) ;
#36850 = DIRECTION ( 'NONE',  ( -1.000000000000000000, -0.000000000000000000, 0.000000000000000000 ) ) ;
#36851 = AXIS2_PLACEMENT_3D ( 'NONE', #14700, #49361, #59306 ) ;
#36852 = CARTESIAN_POINT ( 'NONE',  ( -37.00000000000000711, 8.389074212634413996, -8.839356091079956457 ) ) ;
#36853 = CARTESIAN_POINT ( 'NONE',  ( 2.589278595511360415, 7.746633201026548399, -0.2408616556815215415 ) ) ;
#36854 = CARTESIAN_POINT ( 'NONE',  ( 10.48620311856346454, 8.250315036047107142, -8.713914264323181058 ) ) ;
#36855 = CARTESIAN_POINT ( 'NONE',  ( 0.6511581176980835162, 12.23990098761684919, -1.822219471613748087 ) ) ;
#36856 = EDGE_LOOP ( 'NONE', ( #2783, #38508, #37081, #52623 ) ) ;
#36857 = EDGE_CURVE ( 'NONE', #18279, #15981, #61740, .T. ) ;
#36858 = EDGE_CURVE ( 'NONE', #52549, #46634, #60651, .T. ) ;
#36859 = CARTESIAN_POINT ( 'NONE',  ( 1.283627346226608346, -5.810034161408860420, 11.16434663959570273 ) ) ;
#36860 = VERTEX_POINT ( 'NONE', #21375 ) ;
#36861 = AXIS2_PLACEMENT_3D ( 'NONE', #11292, #31561, #11932 ) ;
#36862 = CARTESIAN_POINT ( 'NONE',  ( 35.00000000000000000, 4.705694406421931860E-17, -3.469127814946512892E-15 ) ) ;
#36863 = EDGE_CURVE ( 'NONE', #26729, #2095, #52179, .T. ) ;
#36864 = CARTESIAN_POINT ( 'NONE',  ( 35.00000000000000000, -1.457575200925456560, 12.66641127287626745 ) ) ;
#36865 = DIRECTION ( 'NONE',  ( -1.000000000000000000, -0.000000000000000000, 0.000000000000000000 ) ) ;
#36866 = VECTOR ( 'NONE', #19792, 1000.000000000000000 ) ;
#36867 = CARTESIAN_POINT ( 'NONE',  ( -27.08588607604449550, 1.631236259433597402, 1.616144682268070065 ) ) ;
#36868 = ORIENTED_EDGE ( 'NONE', *, *, #55336, .T. ) ;
#36869 = DIRECTION ( 'NONE',  ( 1.000000000000000000, -0.000000000000000000, -0.000000000000000000 ) ) ;
#36870 = CARTESIAN_POINT ( 'NONE',  ( 47.00000000000000711, 4.705694406421931860E-17, -3.469127814946512892E-15 ) ) ;
#36871 = DIRECTION ( 'NONE',  ( 0.3939253465568944290, 0.6978179301705716986, 0.5982248387291266845 ) ) ;
#36872 = VERTEX_POINT ( 'NONE', #26693 ) ;
#36874 = ORIENTED_EDGE ( 'NONE', *, *, #52021, .T. ) ;
#36873 = B_SPLINE_CURVE_WITH_KNOTS ( 'NONE', 3,
 ( #8529, #22869, #28483, #33792, #58786, #28821, #13205, #33490, #27842, #8869 ),
 .UNSPECIFIED., .F., .F.,
 ( 4, 3, 3, 4 ),
 ( 0.0001763147164361797566, 0.0002097400188389093628, 0.0002811534801551362692, 0.0003526297678872502878 ),
 .UNSPECIFIED. ) ;
#36875 = CARTESIAN_POINT ( 'NONE',  ( -37.00000000000000711, 0.000000000000000000, 0.000000000000000000 ) ) ;
#36876 = ORIENTED_EDGE ( 'NONE', *, *, #947, .T. ) ;
#36877 = ORIENTED_EDGE ( 'NONE', *, *, #57708, .T. ) ;
#36878 = VERTEX_POINT ( 'NONE', #46984 ) ;
#36879 = VERTEX_POINT ( 'NONE', #37315 ) ;
#36880 = CARTESIAN_POINT ( 'NONE',  ( 0.2915757698887274096, 4.392559307431903370, 11.44067056871811161 ) ) ;
#36881 = EDGE_CURVE ( 'NONE', #40269, #53819, #52824, .T. ) ;
#36882 = DIRECTION ( 'NONE',  ( 0.000000000000000000, 0.01356324068817998940, -0.9999080150203990547 ) ) ;
#36883 = CARTESIAN_POINT ( 'NONE',  ( 0.000000000000000000, -2.469490258309472441, 6.482025155313308140 ) ) ;
#36884 = DIRECTION ( 'NONE',  ( -1.000000000000000000, 0.000000000000000000, 0.000000000000000000 ) ) ;
#36885 = DIRECTION ( 'NONE',  ( -1.000000000000000000, 0.000000000000000000, -0.000000000000000000 ) ) ;
#36886 = VERTEX_POINT ( 'NONE', #7062 ) ;
#36887 = EDGE_CURVE ( 'NONE', #20614, #24790, #18373, .T. ) ;
#36888 = DIRECTION ( 'NONE',  ( 0.000000000000000000, -0.2355298848897378061, -0.9718671068226493182 ) ) ;
#36889 =( BOUNDED_CURVE ( )  B_SPLINE_CURVE ( 3, ( #12838, #58760, #49106, #18527 ),
 .UNSPECIFIED., .F., .F. ) 
 B_SPLINE_CURVE_WITH_KNOTS ( ( 4, 4 ),
 ( 1.845784941385602673, 1.860835188181379163 ),
 .UNSPECIFIED. ) 
 CURVE ( )  GEOMETRIC_REPRESENTATION_ITEM ( )  RATIONAL_B_SPLINE_CURVE ( ( 1.000000000000000000, 0.9999811242616895024, 0.9999811242616895024, 1.000000000000000000 ) ) 
 REPRESENTATION_ITEM ( '' )  );
#36890 = VERTEX_POINT ( 'NONE', #27336 ) ;
#36891 = CYLINDRICAL_SURFACE ( 'NONE', #4022, 12.18649999999999878 ) ;
#36892 = CARTESIAN_POINT ( 'NONE',  ( -22.27722015946439171, 2.828901469906485389, -2.356370737780153046 ) ) ;
#36893 = LINE ( 'NONE', #59973, #16119 ) ;
#36894 = FACE_OUTER_BOUND ( 'NONE', #40219, .T. ) ;
#36895 = CARTESIAN_POINT ( 'NONE',  ( 0.3040950598368152291, 11.60568999039894678, 3.956873563689569551 ) ) ;
#36896 = CARTESIAN_POINT ( 'NONE',  ( -32.00000000000000711, 5.510910596163084625E-16, 0.000000000000000000 ) ) ;
#36897 = ORIENTED_EDGE ( 'NONE', *, *, #50082, .F. ) ;
#36898 = CARTESIAN_POINT ( 'NONE',  ( 0.2655924914740778742, 12.05257978623656889, -2.169924872617939648 ) ) ;
#36899 =( BOUNDED_SURFACE ( )  B_SPLINE_SURFACE ( 3, 1, ( 
 ( #29570, #25247 ),
 ( #45212, #8658 ),
 ( #49247, #24266 ),
 ( #28938, #24937 ) ),
 .UNSPECIFIED., .F., .F., .T. ) 
 B_SPLINE_SURFACE_WITH_KNOTS ( ( 4, 4 ),
 ( 2, 2 ),
 ( 0.000000000000000000, 1.000000000000000000 ),
 ( 0.000000000000000000, 1.000000000000000000 ),
 .UNSPECIFIED. ) 
 GEOMETRIC_REPRESENTATION_ITEM ( )  RATIONAL_B_SPLINE_SURFACE ( (
 ( 1.000000000000000000, 1.000000000000000000),
 ( 0.8716676215708681896, 0.8964445200148167814),
 ( 0.8716676215708681896, 0.8964445200148167814),
 ( 1.000000000000000000, 1.000000000000000000) ) ) 
 REPRESENTATION_ITEM ( '' )  SURFACE ( )  );
#36900 = ORIENTED_EDGE ( 'NONE', *, *, #50969, .F. ) ;
#36901 = CARTESIAN_POINT ( 'NONE',  ( 0.3610902822527233269, 10.76187877352513134, 5.910495176556216812 ) ) ;
#36902 = CARTESIAN_POINT ( 'NONE',  ( 18.54281746013980481, -28.86505449477129659, -7.298814700743937678 ) ) ;
#36903 = DIRECTION ( 'NONE',  ( 0.000000000000000000, 0.01356324068817998940, -0.9999080150203990547 ) ) ;
#36904 = DIRECTION ( 'NONE',  ( 0.000000000000000000, 0.6943713148249588407, -0.7196168960969843154 ) ) ;
#36905 = DIRECTION ( 'NONE',  ( 0.9582930651793755139, -0.1596922922278012080, -0.2370079598497647211 ) ) ;
#36906 = ORIENTED_EDGE ( 'NONE', *, *, #50186, .T. ) ;
#36907 = DIRECTION ( 'NONE',  ( 1.000000000000000000, 0.000000000000000000, 0.000000000000000000 ) ) ;
#36908 = LINE ( 'NONE', #51580, #58881 ) ;
#36909 = LINE ( 'NONE', #41233, #60866 ) ;
#36910 = AXIS2_PLACEMENT_3D ( 'NONE', #49101, #2891, #8185 ) ;
#36911 = CARTESIAN_POINT ( 'NONE',  ( 26.34661844826604593, 11.53221627053869369, 3.317828791472333005 ) ) ;
#36912 = CIRCLE ( 'NONE', #56034, 12.18650000000000055 ) ;
#36913 = EDGE_CURVE ( 'NONE', #18433, #57362, #58949, .T. ) ;
#36914 = DIRECTION ( 'NONE',  ( 0.9606638835031803270, -0.1629100154396138922, -0.2249116044183865903 ) ) ;
#36915 = CARTESIAN_POINT ( 'NONE',  ( 2.241352910868909643, -6.569501556381469598, 3.889181972941426313 ) ) ;
#36916 = B_SPLINE_CURVE_WITH_KNOTS ( 'NONE', 3,
 ( #17025, #5857, #10470, #30746, #2415, #17701, #46078 ),
 .UNSPECIFIED., .F., .F.,
 ( 4, 3, 4 ),
 ( 0.000000000000000000, 0.001700533616330544709, 0.005002426799371397989 ),
 .UNSPECIFIED. ) ;
#36917 = EDGE_CURVE ( 'NONE', #9409, #50465, #57952, .T. ) ;
#36918 = EDGE_LOOP ( 'NONE', ( #41994, #24624, #32906, #40553 ) ) ;
#36919 = B_SPLINE_CURVE_WITH_KNOTS ( 'NONE', 3,
 ( #57916, #33282, #53587, #18673, #48923, #23307, #12333 ),
 .UNSPECIFIED., .F., .F.,
 ( 4, 3, 4 ),
 ( 0.000000000000000000, 0.001700533616330576585, 0.005002426799371340743 ),
 .UNSPECIFIED. ) ;
#36920 = ORIENTED_EDGE ( 'NONE', *, *, #21862, .F. ) ;
#36921 = CARTESIAN_POINT ( 'NONE',  ( -22.71097035706202405, 4.510116093748279376, -2.118550233809386896 ) ) ;
#36922 = CARTESIAN_POINT ( 'NONE',  ( 44.06649112733599338, -1.138262461040735474, 14.66001971352460309 ) ) ;
#36923 = CARTESIAN_POINT ( 'NONE',  ( -29.58156646296218995, -2.915657712021824111, 13.18682379069277388 ) ) ;
#36924 = CYLINDRICAL_SURFACE ( 'NONE', #59437, 5.000000000000000888 ) ;
#36925 = ORIENTED_EDGE ( 'NONE', *, *, #17776, .F. ) ;
#36927 = ORIENTED_EDGE ( 'NONE', *, *, #59908, .F. ) ;
#36926 = B_SPLINE_CURVE_WITH_KNOTS ( 'NONE', 3,
 ( #34814, #14537, #9546, #4607, #40139, #14858, #25190, #55456, #9896, #45463, #65730, #40476, #36482, #36126, #21180, #21528 ),
 .UNSPECIFIED., .F., .F.,
 ( 4, 3, 3, 3, 3, 4 ),
 ( 0.000000000000000000, 0.0002999043160757356601, 0.0005998071753051037111, 0.0008997092107374638848, 0.001204458948195666346, 0.001510329163476545160 ),
 .UNSPECIFIED. ) ;
#36928 = EDGE_LOOP ( 'NONE', ( #15623, #6929, #50, #23209 ) ) ;
#36929 = CYLINDRICAL_SURFACE ( 'NONE', #1556, 2.899999999999994582 ) ;
#36930 = CIRCLE ( 'NONE', #8281, 5.000000000000000000 ) ;
#36931 = CARTESIAN_POINT ( 'NONE',  ( 21.90174657591892071, 11.97747433400151884, -0.7349207973210698519 ) ) ;
#36932 = ORIENTED_EDGE ( 'NONE', *, *, #58654, .T. ) ;
#36933 = CARTESIAN_POINT ( 'NONE',  ( 2.000000000000001776, 2.315790869867068835, 7.133520354428100951 ) ) ;
#36934 = DIRECTION ( 'NONE',  ( 0.000000000000000000, 0.01356324068817992175, -0.9999080150203990547 ) ) ;
#36936 = VERTEX_POINT ( 'NONE', #43606 ) ;
#36935 = VECTOR ( 'NONE', #26715, 1000.000000000000114 ) ;
#36937 = DIRECTION ( 'NONE',  ( 1.000000000000000000, 0.000000000000000000, 0.000000000000000000 ) ) ;
#36938 = B_SPLINE_CURVE_WITH_KNOTS ( 'NONE', 3,
 ( #46104, #12141, #51745, #51088, #25809, #62665, #11802 ),
 .UNSPECIFIED., .F., .F.,
 ( 4, 3, 4 ),
 ( 8.157409164538106469E-15, 0.002398160485435165898, 0.005002426799384885464 ),
 .UNSPECIFIED. ) ;
#36939 = CARTESIAN_POINT ( 'NONE',  ( 19.56743653832047869, -29.99999999999999645, -4.999999999999984013 ) ) ;
#36940 = CARTESIAN_POINT ( 'NONE',  ( 23.48109318918174182, 2.900249156073090528, 11.64847700441486467 ) ) ;
#36941 = ORIENTED_EDGE ( 'NONE', *, *, #25509, .T. ) ;
#36942 = DIRECTION ( 'NONE',  ( -0.000000000000000000, -0.000000000000000000, -1.000000000000000000 ) ) ;
#36943 = ORIENTED_EDGE ( 'NONE', *, *, #13601, .T. ) ;
#36944 = CARTESIAN_POINT ( 'NONE',  ( 0.5547464869798228726, 7.697709668896196789, -9.648168635481763289 ) ) ;
#36945 = CARTESIAN_POINT ( 'NONE',  ( -17.81734942214415440, -8.644007148549530228, 10.38604278132294922 ) ) ;
#36946 = CARTESIAN_POINT ( 'NONE',  ( 0.000000000000000000, -6.812627895098285258, 0.04423456934719675882 ) ) ;
#36947 = DIRECTION ( 'NONE',  ( 1.000000000000000000, 0.000000000000000000, 0.000000000000000000 ) ) ;
#36948 = CARTESIAN_POINT ( 'NONE',  ( 5.514970785353741078, -0.004694330894494374434, 0.0005190732562558384843 ) ) ;
#36949 = DIRECTION ( 'NONE',  ( -1.000000000000000000, -0.000000000000000000, -0.000000000000000000 ) ) ;
#36950 = DIRECTION ( 'NONE',  ( 0.000000000000000000, 1.000000000000000000, 0.000000000000000000 ) ) ;
#36951 = CARTESIAN_POINT ( 'NONE',  ( 8.821156950359336335, 6.332123185147309208, -10.20069656434953131 ) ) ;
#36952 = VERTEX_POINT ( 'NONE', #28331 ) ;
#36953 = CARTESIAN_POINT ( 'NONE',  ( 35.00000000000000000, 4.705694406421931860E-17, -3.469127814946512892E-15 ) ) ;
#36954 = EDGE_LOOP ( 'NONE', ( #53705, #40430, #16737, #32221 ) ) ;
#36955 = CARTESIAN_POINT ( 'NONE',  ( -35.00000000000000000, 7.376655759825023750, -9.700295462048581285 ) ) ;
#36956 = DIRECTION ( 'NONE',  ( 0.000000000000000000, -0.6943713148249532896, 0.7196168960969895334 ) ) ;
#36958 = ORIENTED_EDGE ( 'NONE', *, *, #45542, .T. ) ;
#36957 = EDGE_CURVE ( 'NONE', #20446, #52831, #51133, .T. ) ;
#36959 = CARTESIAN_POINT ( 'NONE',  ( 2.844750968616162723, 7.470159816919374585, 2.364925124213946628 ) ) ;
#36960 = CARTESIAN_POINT ( 'NONE',  ( 1.549075743846873632, 12.12370443967657252, -3.694639393663405436 ) ) ;
#36961 = DIRECTION ( 'NONE',  ( -1.000000000000000000, 0.000000000000000000, 0.000000000000000000 ) ) ;
#36962 = CARTESIAN_POINT ( 'NONE',  ( 2.000000000000001776, 6.606214214351110670, -2.114938770769863030 ) ) ;
#36964 = EDGE_CURVE ( 'NONE', #63113, #8767, #18236, .T. ) ;
#36963 = EDGE_LOOP ( 'NONE', ( #19358, #52128, #29403, #44698 ) ) ;
#36965 = ORIENTED_EDGE ( 'NONE', *, *, #44651, .F. ) ;
#36966 = CARTESIAN_POINT ( 'NONE',  ( -10.90165637462999904, -7.508992741355384304, 11.21895841913464587 ) ) ;
#36967 = AXIS2_PLACEMENT_3D ( 'NONE', #19136, #53747, #54066 ) ;
#36968 = EDGE_LOOP ( 'NONE', ( #29505, #25259, #28530, #59742 ) ) ;
#36969 = DIRECTION ( 'NONE',  ( -1.000000000000000000, 0.000000000000000000, 0.000000000000000000 ) ) ;
#36970 = LINE ( 'NONE', #6740, #46267 ) ;
#36971 = DIRECTION ( 'NONE',  ( -1.000000000000000000, -0.000000000000000000, -0.000000000000000000 ) ) ;
#36972 = ORIENTED_EDGE ( 'NONE', *, *, #22692, .T. ) ;
#36973 = CARTESIAN_POINT ( 'NONE',  ( 0.3006302518452046990, -4.404090606399806873, -11.43947177966006556 ) ) ;
#36974 = VECTOR ( 'NONE', #64124, 1000.000000000000000 ) ;
#36975 = EDGE_CURVE ( 'NONE', #21980, #47209, #54328, .T. ) ;
#36976 = CIRCLE ( 'NONE', #48691, 12.75000000000000178 ) ;
#36977 = ADVANCED_FACE ( 'NONE', ( #37967 ), #32631, .T. ) ;
#36978 = CARTESIAN_POINT ( 'NONE',  ( 3.780834652287974773, 8.352030633203074927, 8.616471685210687070 ) ) ;
#36979 = CARTESIAN_POINT ( 'NONE',  ( -35.00000000000000000, 0.000000000000000000, 0.000000000000000000 ) ) ;
#36980 = CARTESIAN_POINT ( 'NONE',  ( -35.00000000000000000, 11.68758509253248334, -1.171570255487489609 ) ) ;
#36982 = CIRCLE ( 'NONE', #34882, 12.75000000000000178 ) ;
#36981 = CARTESIAN_POINT ( 'NONE',  ( 0.2657645697724700939, -5.991637049003168514, -10.68050050043097166 ) ) ;
#36983 = EDGE_CURVE ( 'NONE', #62930, #63438, #35202, .T. ) ;
#36984 = DIRECTION ( 'NONE',  ( 1.000000000000000000, 0.000000000000000000, 0.000000000000000000 ) ) ;
#36985 = CARTESIAN_POINT ( 'NONE',  ( 2.288423627607475197, -5.755330594805005084, 5.039850887180246986 ) ) ;
#36986 = CARTESIAN_POINT ( 'NONE',  ( -27.35552965826137140, -1.773915698030568366, 2.548625910254532112 ) ) ;
#36987 = AXIS2_PLACEMENT_3D ( 'NONE', #22848, #39093, #33470 ) ;
#36988 = EDGE_CURVE ( 'NONE', #25430, #12876, #40472, .T. ) ;
#36989 = ORIENTED_EDGE ( 'NONE', *, *, #45656, .T. ) ;
#36990 = DIRECTION ( 'NONE',  ( -1.000000000000000000, 0.000000000000000000, 0.000000000000000000 ) ) ;
#36991 = CARTESIAN_POINT ( 'NONE',  ( 0.2759803524722223567, -12.24828167798667167, -0.1894460813477297501 ) ) ;
#36992 = ORIENTED_EDGE ( 'NONE', *, *, #55787, .F. ) ;
#36993 = DIRECTION ( 'NONE',  ( 1.000000000000000000, 0.000000000000000000, 0.000000000000000000 ) ) ;
#36994 = ADVANCED_FACE ( 'NONE', ( #38293 ), #59631, .F. ) ;
#36995 = DIRECTION ( 'NONE',  ( 0.000000000000000000, 0.000000000000000000, 1.000000000000000000 ) ) ;
#36996 = VERTEX_POINT ( 'NONE', #8712 ) ;
#36997 = CARTESIAN_POINT ( 'NONE',  ( 2.245754705088791159, 6.556487589644730996, 3.913944702467391679 ) ) ;
#36998 = ORIENTED_EDGE ( 'NONE', *, *, #61568, .T. ) ;
#36999 = DIRECTION ( 'NONE',  ( 0.000000000000000000, 0.000000000000000000, -1.000000000000000000 ) ) ;
#37000 = ORIENTED_EDGE ( 'NONE', *, *, #47801, .F. ) ;
#37001 = ORIENTED_EDGE ( 'NONE', *, *, #25131, .T. ) ;
#37002 = CARTESIAN_POINT ( 'NONE',  ( 24.82652845881425208, -8.390869743685021476, -8.578654028722157321 ) ) ;
#37003 = AXIS2_PLACEMENT_3D ( 'NONE', #38280, #3068, #28979 ) ;
#37004 = ORIENTED_EDGE ( 'NONE', *, *, #13358, .F. ) ;
#37005 = EDGE_CURVE ( 'NONE', #38749, #34574, #44744, .T. ) ;
#37006 = CARTESIAN_POINT ( 'NONE',  ( -26.39842685320601134, -10.43619857301325560, 5.924288189175664243 ) ) ;
#37007 = CARTESIAN_POINT ( 'NONE',  ( 1.375507693219669481, -11.64019206974686327, -4.865932489132057448 ) ) ;
#37008 = CARTESIAN_POINT ( 'NONE',  ( -35.00000000000000000, -7.215058775251326217, 9.821084925794544063 ) ) ;
#37009 = CARTESIAN_POINT ( 'NONE',  ( 1.194176325881337819, -0.5141316333310350650, -12.54527478469375623 ) ) ;
#37010 = ORIENTED_EDGE ( 'NONE', *, *, #25184, .T. ) ;
#37011 = CARTESIAN_POINT ( 'NONE',  ( -4.979813338170842485, -1.249770091004172690, -11.93591655830499931 ) ) ;
#37012 = VECTOR ( 'NONE', #63292, 1000.000000000000000 ) ;
#37013 = CARTESIAN_POINT ( 'NONE',  ( 6.676753782886446942, -28.39896155677633516, 11.13103273143544314 ) ) ;
#37014 = DIRECTION ( 'NONE',  ( -1.000000000000000000, 0.000000000000000000, 0.000000000000000000 ) ) ;
#37016 = EDGE_LOOP ( 'NONE', ( #48089, #56129, #26794, #5713 ) ) ;
#37015 = CARTESIAN_POINT ( 'NONE',  ( 36.00000000000000711, -12.63095688309027764, 1.738225594540123708 ) ) ;
#37017 = CYLINDRICAL_SURFACE ( 'NONE', #52207, 5.000000000000000888 ) ;
#37018 = VERTEX_POINT ( 'NONE', #35522 ) ;
#37019 = DIRECTION ( 'NONE',  ( -1.000000000000000000, 0.000000000000000000, 0.000000000000000000 ) ) ;
#37020 = ORIENTED_EDGE ( 'NONE', *, *, #51864, .F. ) ;
#37021 = CARTESIAN_POINT ( 'NONE',  ( -16.98800322446194855, 2.922502605998049674, 13.17987020110344787 ) ) ;
#37022 = CARTESIAN_POINT ( 'NONE',  ( -35.00000000000000000, 10.28547182238008162, 5.672855678558722303 ) ) ;
#37023 = AXIS2_PLACEMENT_3D ( 'NONE', #41992, #12063, #21397 ) ;
#37024 = CARTESIAN_POINT ( 'NONE',  ( 1.462291587748804300, -4.914320681885039122, 11.65117843858572755 ) ) ;
#37025 = ORIENTED_EDGE ( 'NONE', *, *, #25777, .F. ) ;
#37026 = CARTESIAN_POINT ( 'NONE',  ( 1.719304012338398469, 8.755325027793414705, 9.242227816402090568 ) ) ;
#37027 = DIRECTION ( 'NONE',  ( -1.000000000000000000, -0.000000000000000000, 0.000000000000000000 ) ) ;
#37028 = CARTESIAN_POINT ( 'NONE',  ( 5.515539859299206427, 0.001886660928063779545, -0.005751553894235449972 ) ) ;
#37029 = ORIENTED_EDGE ( 'NONE', *, *, #12002, .F. ) ;
#37030 = AXIS2_PLACEMENT_3D ( 'NONE', #51975, #6419, #1443 ) ;
#37031 = AXIS2_PLACEMENT_3D ( 'NONE', #21681, #41936, #27296 ) ;
#37032 = ORIENTED_EDGE ( 'NONE', *, *, #64670, .F. ) ;
#37033 = CARTESIAN_POINT ( 'NONE',  ( 2.573738926104372826, 7.583190312075771544, 1.575954828885281822 ) ) ;
#37034 = ORIENTED_EDGE ( 'NONE', *, *, #26947, .F. ) ;
#37035 = VECTOR ( 'NONE', #12270, 1000.000000000000000 ) ;
#37036 = VERTEX_POINT ( 'NONE', #36158 ) ;
#37037 = B_SPLINE_CURVE_WITH_KNOTS ( 'NONE', 3,
 ( #1594, #21867, #42112, #1903, #38111, #8512, #33473, #63379, #28800, #59085, #64046, #37799, #58093 ),
 .UNSPECIFIED., .F., .F.,
 ( 4, 3, 3, 3, 4 ),
 ( 3.878959614448864246E-18, 6.607593386745498512E-05, 0.0001321518677373520001, 0.0001982171734706217813, 0.0002642860854759490966 ),
 .UNSPECIFIED. ) ;
#37038 = DIRECTION ( 'NONE',  ( 1.000000000000000000, -0.000000000000000000, 0.000000000000000000 ) ) ;
#37039 = DIRECTION ( 'NONE',  ( -1.000000000000000000, 0.000000000000000000, 0.000000000000000000 ) ) ;
#37040 = DIRECTION ( 'NONE',  ( 1.000000000000000000, 0.000000000000000000, 0.000000000000000000 ) ) ;
#37041 = CARTESIAN_POINT ( 'NONE',  ( 1.937114397841935398, 7.182898292393766759, 10.63710405811936255 ) ) ;
#37042 = CARTESIAN_POINT ( 'NONE',  ( 1.719304012339833099, -9.242227816401946683, 8.755325027794301107 ) ) ;
#37043 = EDGE_CURVE ( 'NONE', #60814, #60039, #12905, .T. ) ;
#37044 = FACE_OUTER_BOUND ( 'NONE', #49395, .T. ) ;
#37045 = FACE_OUTER_BOUND ( 'NONE', #42497, .T. ) ;
#37046 = EDGE_LOOP ( 'NONE', ( #29127, #52186, #8307, #17514 ) ) ;
#37047 = CARTESIAN_POINT ( 'NONE',  ( 2.000000000000001776, 4.570217215903371155, 5.218059682435623792 ) ) ;
#37048 = LINE ( 'NONE', #23676, #44642 ) ;
#37049 = CARTESIAN_POINT ( 'NONE',  ( 0.3053067050349195233, 4.409108891833811938, -11.43920902168902032 ) ) ;
#37050 = AXIS2_PLACEMENT_3D ( 'NONE', #56200, #40586, #10639 ) ;
#37051 = EDGE_CURVE ( 'NONE', #48033, #23557, #5620, .T. ) ;
#37052 = DIRECTION ( 'NONE',  ( 1.000000000000000000, 0.000000000000000000, 0.000000000000000000 ) ) ;
#37053 = CIRCLE ( 'NONE', #12660, 5.000000000000000000 ) ;
#37054 = DIRECTION ( 'NONE',  ( 1.000000000000000000, 0.000000000000000000, 0.000000000000000000 ) ) ;
#37055 = ADVANCED_FACE ( 'NONE', ( #5274 ), #20227, .T. ) ;
#37056 = CARTESIAN_POINT ( 'NONE',  ( 8.437200413559441614, 4.218240606060086328, -11.23760835609581399 ) ) ;
#37057 = EDGE_CURVE ( 'NONE', #8907, #19699, #14155, .T. ) ;
#37058 = ORIENTED_EDGE ( 'NONE', *, *, #49560, .T. ) ;
#37059 = CARTESIAN_POINT ( 'NONE',  ( 2.889800649504073782, 5.728825117897707209, 2.156828754871487064 ) ) ;
#37060 = CARTESIAN_POINT ( 'NONE',  ( 0.2706063244538067791, -1.954041462022338971, -12.09107863371558444 ) ) ;
#37061 = FACE_OUTER_BOUND ( 'NONE', #60962, .T. ) ;
#37062 = CARTESIAN_POINT ( 'NONE',  ( 3.474089039520120270, -31.27092243478756117, 14.18576039181575688 ) ) ;
#37063 = B_SPLINE_CURVE_WITH_KNOTS ( 'NONE', 3,
 ( #35806, #55798, #61107, #10227, #15539, #46157, #7124 ),
 .UNSPECIFIED., .F., .F.,
 ( 4, 3, 4 ),
 ( 0.000000000000000000, 0.001700533616330553600, 0.005002426799371221047 ),
 .UNSPECIFIED. ) ;
#37064 = CIRCLE ( 'NONE', #8420, 12.18650000000000055 ) ;
#37065 = ADVANCED_FACE ( 'NONE', ( #35176 ), #63881, .F. ) ;
#37066 = CARTESIAN_POINT ( 'NONE',  ( -25.68925157440544638, 10.12461928084059259, 6.442855087883957665 ) ) ;
#37067 = DIRECTION ( 'NONE',  ( 1.000000000000000000, 0.000000000000000000, 0.000000000000000000 ) ) ;
#37068 = CIRCLE ( 'NONE', #17963, 7.938172270156617749 ) ;
#37069 =( BOUNDED_SURFACE ( )  B_SPLINE_SURFACE ( 3, 1, ( 
 ( #62663, #1538 ),
 ( #47411, #32412 ),
 ( #58036, #38054 ),
 ( #6508, #12452 ) ),
 .UNSPECIFIED., .F., .F., .F. ) 
 B_SPLINE_SURFACE_WITH_KNOTS ( ( 4, 4 ),
 ( 2, 2 ),
 ( 0.000000000000000000, 1.000000000000000000 ),
 ( 0.000000000000000000, 1.000000000000000000 ),
 .UNSPECIFIED. ) 
 GEOMETRIC_REPRESENTATION_ITEM ( )  RATIONAL_B_SPLINE_SURFACE ( (
 ( 1.000000000000000000, 1.000000000000000000),
 ( 0.9932032654565553509, 0.8386279382598736953),
 ( 0.9932032654565553509, 0.8386279382598736953),
 ( 1.000000000000000000, 1.000000000000000000) ) ) 
 REPRESENTATION_ITEM ( '' )  SURFACE ( )  );
#37070 = EDGE_LOOP ( 'NONE', ( #61804, #60357, #50040, #30348 ) ) ;
#37071 = DIRECTION ( 'NONE',  ( -1.000000000000000000, 0.000000000000000000, 0.000000000000000000 ) ) ;
#37072 = CARTESIAN_POINT ( 'NONE',  ( 0.000000000000000000, -3.224464355699868889, 6.771471746881965181 ) ) ;
#37073 = EDGE_CURVE ( 'NONE', #10498, #4335, #27324, .T. ) ;
#37074 = CARTESIAN_POINT ( 'NONE',  ( 2.253265082352138737, -4.810902415501418616, -5.932955906470167129 ) ) ;
#37075 = PLANE ( 'NONE',  #27537 ) ;
#37076 = ORIENTED_EDGE ( 'NONE', *, *, #13546, .T. ) ;
#37077 = CARTESIAN_POINT ( 'NONE',  ( 0.2671309869109485535, 2.286013846430026142, 12.03155065772886090 ) ) ;
#37078 = DIRECTION ( 'NONE',  ( 0.000000000000000000, 0.01356324068817998940, -0.9999080150203990547 ) ) ;
#37079 = EDGE_CURVE ( 'NONE', #5369, #13777, #57500, .T. ) ;
#37081 = ORIENTED_EDGE ( 'NONE', *, *, #18654, .T. ) ;
#37080 = LINE ( 'NONE', #3765, #30747 ) ;
#37082 = DIRECTION ( 'NONE',  ( 0.000000000000000000, 0.000000000000000000, 1.000000000000000000 ) ) ;
#37083 = EDGE_CURVE ( 'NONE', #55976, #8578, #17216, .T. ) ;
#37084 = FACE_BOUND ( 'NONE', #6575, .T. ) ;
#37085 = ORIENTED_EDGE ( 'NONE', *, *, #37204, .T. ) ;
#37086 = ADVANCED_FACE ( 'NONE', ( #57796 ), #11558, .T. ) ;
#37087 = CARTESIAN_POINT ( 'NONE',  ( 22.00000000000000711, -20.00000000000000000, -1.499999999999998002 ) ) ;
#37088 = DIRECTION ( 'NONE',  ( 1.000000000000000000, 0.000000000000000000, -0.000000000000000000 ) ) ;
#37089 = CYLINDRICAL_SURFACE ( 'NONE', #3557, 12.18650000000000055 ) ;
#37090 = CARTESIAN_POINT ( 'NONE',  ( -3.644870031796809684, -12.49356576308750100, 5.128347001116654980 ) ) ;
#37091 = CARTESIAN_POINT ( 'NONE',  ( -9.600257793028196929, 9.184030621591224630, -7.726472095688762920 ) ) ;
#37092 = EDGE_CURVE ( 'NONE', #50423, #14292, #3341, .T. ) ;
#37093 = DIRECTION ( 'NONE',  ( 0.000000000000000000, -0.1387779952735885280, 0.9903235168508540687 ) ) ;
#37095 = ORIENTED_EDGE ( 'NONE', *, *, #3316, .T. ) ;
#37094 = CARTESIAN_POINT ( 'NONE',  ( -35.00000000000000000, -10.59380114696474884, 7.094637218249319588 ) ) ;
#37096 = ORIENTED_EDGE ( 'NONE', *, *, #49370, .F. ) ;
#37097 = CARTESIAN_POINT ( 'NONE',  ( 2.241352910868909643, -0.08337961031709527349, 7.633946224498472155 ) ) ;
#37098 = VERTEX_POINT ( 'NONE', #51815 ) ;
#37099 = PRODUCT_CONTEXT ( 'NONE', #65029, 'mechanical' ) ;
#37100 = DIRECTION ( 'NONE',  ( -1.000000000000000000, 0.000000000000000000, -0.000000000000000000 ) ) ;
#37101 = DIRECTION ( 'NONE',  ( -0.3939253465568944290, 0.5833358547425184781, -0.7103112711423392733 ) ) ;
#37102 = CIRCLE ( 'NONE', #59418, 12.18650000000000055 ) ;
#37103 = CARTESIAN_POINT ( 'NONE',  ( 35.00000000000000000, 4.705694406421931860E-17, -3.469127814946512892E-15 ) ) ;
#37104 = ORIENTED_EDGE ( 'NONE', *, *, #42650, .T. ) ;
#37105 = CARTESIAN_POINT ( 'NONE',  ( 5.516018279890452902, -0.006286471671801945743, 0.002527316374434286465 ) ) ;
#37106 = AXIS2_PLACEMENT_3D ( 'NONE', #59316, #48693, #4112 ) ;
#37107 = CARTESIAN_POINT ( 'NONE',  ( -22.31328051695926007, -3.633840107626937765, 1.076152733467191869 ) ) ;
#37108 = ORIENTED_EDGE ( 'NONE', *, *, #24767, .T. ) ;
#37109 = VERTEX_POINT ( 'NONE', #1612 ) ;
#37110 = CARTESIAN_POINT ( 'NONE',  ( 2.969415267404512448, 7.680649281077198687, -1.748187016698217411 ) ) ;
#37111 = ORIENTED_EDGE ( 'NONE', *, *, #49601, .T. ) ;
#37112 = DIRECTION ( 'NONE',  ( -1.000000000000000000, 0.000000000000000000, 0.000000000000000000 ) ) ;
#37113 = DIRECTION ( 'NONE',  ( 0.000000000000000000, -0.01356324068817998940, 0.9999080150203990547 ) ) ;
#37114 = CARTESIAN_POINT ( 'NONE',  ( 9.273470328753727898, 2.853023627877379731, 13.19712399426135008 ) ) ;
#37116 = AXIS2_PLACEMENT_3D ( 'NONE', #42902, #23281, #13306 ) ;
#37115 = CARTESIAN_POINT ( 'NONE',  ( -27.09048036756548328, 0.9969423855787405975, -2.083857239072913092 ) ) ;
#37117 = EDGE_CURVE ( 'NONE', #7095, #61909, #32804, .T. ) ;
#37118 = CARTESIAN_POINT ( 'NONE',  ( 0.000000000000000000, -45.00000000000000000, 0.000000000000000000 ) ) ;
#37119 = CARTESIAN_POINT ( 'NONE',  ( 26.17129964821461385, -11.44745868472663197, 3.602463285258928671 ) ) ;
#37120 = DIRECTION ( 'NONE',  ( 0.000000000000000000, 0.01356324068817998940, -0.9999080150203990547 ) ) ;
#37121 = AXIS2_PLACEMENT_3D ( 'NONE', #24090, #59031, #19440 ) ;
#37122 = VERTEX_POINT ( 'NONE', #2254 ) ;
#37123 = DIRECTION ( 'NONE',  ( 0.000000000000000000, -0.2006870767258961963, 0.9796553971857727694 ) ) ;
#37124 = VERTEX_POINT ( 'NONE', #61772 ) ;
#37125 = CYLINDRICAL_SURFACE ( 'NONE', #50215, 5.000000000000000000 ) ;
#37126 = CARTESIAN_POINT ( 'NONE',  ( -22.27218376572352554, -2.577901515391805898, 2.630375585211909506 ) ) ;
#37127 = CYLINDRICAL_SURFACE ( 'NONE', #64720, 4.999999999999999112 ) ;
#37128 = DIRECTION ( 'NONE',  ( 0.000000000000000000, 0.01356324068817991828, -0.9999080150203990547 ) ) ;
#37129 = CARTESIAN_POINT ( 'NONE',  ( 0.2647959493198558945, -10.67808515296906791, -5.995292100780899247 ) ) ;
#37130 = EDGE_CURVE ( 'NONE', #18591, #54727, #41569, .T. ) ;
#37131 = AXIS2_PLACEMENT_3D ( 'NONE', #29270, #14599, #49567 ) ;
#37132 = CARTESIAN_POINT ( 'NONE',  ( 0.3665391374699472626, 4.447929964102847578, 11.44911061034387956 ) ) ;
#37133 = ORIENTED_EDGE ( 'NONE', *, *, #1815, .T. ) ;
#37134 = ORIENTED_EDGE ( 'NONE', *, *, #33383, .T. ) ;
#37135 = EDGE_CURVE ( 'NONE', #4279, #26831, #44739, .T. ) ;
#37136 = CARTESIAN_POINT ( 'NONE',  ( -27.08429572838383947, 0.2296550094123047669, 2.279961732801582208 ) ) ;
#37137 = ORIENTED_EDGE ( 'NONE', *, *, #6162, .T. ) ;
#37138 = FACE_OUTER_BOUND ( 'NONE', #135, .T. ) ;
#37139 = CARTESIAN_POINT ( 'NONE',  ( 0.2655924914740778742, -0.04405032194294832004, -12.24627751708824341 ) ) ;
#37140 = DIRECTION ( 'NONE',  ( 1.000000000000000000, 0.000000000000000000, 0.000000000000000000 ) ) ;
#37141 = CARTESIAN_POINT ( 'NONE',  ( 2.241311220309555985, 1.417008678104584307, -7.501736494813729728 ) ) ;
#37142 = EDGE_CURVE ( 'NONE', #26538, #15657, #52481, .T. ) ;
#37143 = ORIENTED_EDGE ( 'NONE', *, *, #18526, .T. ) ;
#37144 = CARTESIAN_POINT ( 'NONE',  ( 0.2671309869109474988, 12.08782215308012020, 1.966882337881730392 ) ) ;
#37145 = CARTESIAN_POINT ( 'NONE',  ( -35.00000000000000000, 7.146664589318047156, -9.321877890560362090 ) ) ;
#37146 = DIRECTION ( 'NONE',  ( 0.000000000000000000, -0.01356324068817998940, 0.9999080150203990547 ) ) ;
#37147 = CARTESIAN_POINT ( 'NONE',  ( -28.27451930523357149, -3.452175767011101737, 24.83788945613662236 ) ) ;
#37148 = AXIS2_PLACEMENT_3D ( 'NONE', #56900, #31591, #51903 ) ;
#37149 = CARTESIAN_POINT ( 'NONE',  ( 2.000000000000001776, -7.248432822490231686, -1.926193556693109654 ) ) ;
#37150 = CARTESIAN_POINT ( 'NONE',  ( 9.612870878434209843, -11.96650298090370690, -0.9106810471525499384 ) ) ;
#37151 = VERTEX_POINT ( 'NONE', #46812 ) ;
#37152 = CARTESIAN_POINT ( 'NONE',  ( -19.30028080049353179, -29.00000000000000000, -5.863682654924961213 ) ) ;
#37153 = VERTEX_POINT ( 'NONE', #37149 ) ;
#37154 = CARTESIAN_POINT ( 'NONE',  ( -37.00000000000000711, 12.18359334611896472, 0.2661492558803780772 ) ) ;
#37155 = CARTESIAN_POINT ( 'NONE',  ( 35.00000000000000000, 9.700295462048766026, 7.376655759824770620 ) ) ;
#37156 = CARTESIAN_POINT ( 'NONE',  ( 35.00000000000000000, 4.705694406421931860E-17, -3.469127814946512892E-15 ) ) ;
#37157 = DIRECTION ( 'NONE',  ( 1.000000000000000000, 0.000000000000000000, -0.000000000000000000 ) ) ;
#37158 = CARTESIAN_POINT ( 'NONE',  ( 35.00000000000000000, -12.38385022362083632, -3.033604067594535714 ) ) ;
#37159 = EDGE_CURVE ( 'NONE', #57376, #40209, #11793, .T. ) ;
#37160 = AXIS2_PLACEMENT_3D ( 'NONE', #50768, #10508, #10850 ) ;
#37161 = EDGE_LOOP ( 'NONE', ( #36876, #39054, #45879, #55072 ) ) ;
#37162 = ORIENTED_EDGE ( 'NONE', *, *, #8355, .F. ) ;
#37163 = CARTESIAN_POINT ( 'NONE',  ( 0.2956976708475454463, 1.911282699793726669, 12.10637007622313988 ) ) ;
#37164 = EDGE_CURVE ( 'NONE', #32109, #3960, #42796, .T. ) ;
#37165 = ORIENTED_EDGE ( 'NONE', *, *, #535, .F. ) ;
#37166 = VECTOR ( 'NONE', #49144, 1000.000000000000000 ) ;
#37167 = CARTESIAN_POINT ( 'NONE',  ( -27.08429572838383947, -2.279961732801590646, 0.2296550094122822017 ) ) ;
#37168 = DIRECTION ( 'NONE',  ( 0.000000000000000000, 0.01356324068817992175, -0.9999080150203990547 ) ) ;
#37169 = CARTESIAN_POINT ( 'NONE',  ( 2.177405672430401395, 10.89176600225243341, -2.605669267167184167 ) ) ;
#37170 = CYLINDRICAL_SURFACE ( 'NONE', #38577, 6.936499999999988120 ) ;
#37171 = DIRECTION ( 'NONE',  ( -1.000000000000000000, 0.000000000000000000, 0.000000000000000000 ) ) ;
#37172 = EDGE_CURVE ( 'NONE', #26332, #56593, #21557, .T. ) ;
#37173 = CARTESIAN_POINT ( 'NONE',  ( 0.2646305136544065406, 0.1321451301297855152, 12.24595685781654453 ) ) ;
#37174 = CARTESIAN_POINT ( 'NONE',  ( -37.00000000000000711, 12.26766708251996363, -3.473736367725128726 ) ) ;
#37175 = VERTEX_POINT ( 'NONE', #27186 ) ;
#37176 = DIRECTION ( 'NONE',  ( -1.000000000000000000, 0.000000000000000000, 0.000000000000000000 ) ) ;
#37177 = AXIS2_PLACEMENT_3D ( 'NONE', #20359, #20035, #10060 ) ;
#37178 = ORIENTED_EDGE ( 'NONE', *, *, #17329, .F. ) ;
#37179 = CARTESIAN_POINT ( 'NONE',  ( 1.719304012341585475, 10.62216384465587993, -7.017415949613843296 ) ) ;
#37180 = FACE_OUTER_BOUND ( 'NONE', #17174, .T. ) ;
#37181 = CARTESIAN_POINT ( 'NONE',  ( -27.10113028276155234, 1.697941299269287940, 1.613062633976892091 ) ) ;
#37182 = ORIENTED_EDGE ( 'NONE', *, *, #38334, .F. ) ;
#37183 = DIRECTION ( 'NONE',  ( 1.000000000000000000, -0.000000000000000000, 0.000000000000000000 ) ) ;
#37184 = CARTESIAN_POINT ( 'NONE',  ( -14.43403921783542998, -30.05772736394682454, -4.235651140256554648 ) ) ;
#37185 = CARTESIAN_POINT ( 'NONE',  ( 2.430348790457391051, 2.814990071338047350, 7.164221884688230624 ) ) ;
#37186 = VERTEX_POINT ( 'NONE', #47480 ) ;
#37187 = VERTEX_POINT ( 'NONE', #1919 ) ;
#37188 = CYLINDRICAL_SURFACE ( 'NONE', #6680, 5.000000000000000888 ) ;
#37189 = ORIENTED_EDGE ( 'NONE', *, *, #58030, .T. ) ;
#37190 = VERTEX_POINT ( 'NONE', #22189 ) ;
#37191 = ORIENTED_EDGE ( 'NONE', *, *, #358, .F. ) ;
#37192 = B_SPLINE_CURVE_WITH_KNOTS ( 'NONE', 3,
 ( #51638, #62551, #6083, #7044, #5764, #61579, #42946, #37637, #12669, #13343, #3735, #49279, #17693 ),
 .UNSPECIFIED., .F., .F.,
 ( 4, 3, 3, 3, 4 ),
 ( 2.453269466693398698E-18, 6.607593386745292514E-05, 0.0001321518677373508346, 0.0001982171734706214832, 0.0002642860854759498013 ),
 .UNSPECIFIED. ) ;
#37193 = ORIENTED_EDGE ( 'NONE', *, *, #35711, .F. ) ;
#37194 = CARTESIAN_POINT ( 'NONE',  ( -22.27715239060371744, -2.689999469426690215, 2.513478159995840677 ) ) ;
#37195 = CARTESIAN_POINT ( 'NONE',  ( 145.1370849898475797, 3.309064568108273190E-14, 0.000000000000000000 ) ) ;
#37196 = EDGE_CURVE ( 'NONE', #63452, #2298, #9897, .T. ) ;
#37198 = CIRCLE ( 'NONE', #6413, 5.000000000000000000 ) ;
#37197 = CARTESIAN_POINT ( 'NONE',  ( 1.719304012341585253, 9.242227816401774376, -8.755325027795295867 ) ) ;
#37199 = CARTESIAN_POINT ( 'NONE',  ( 9.650000913499871658, 11.97776111335499749, -0.7481793053950375194 ) ) ;
#37200 = DIRECTION ( 'NONE',  ( -0.6151304903148129277, 0.000000000000000000, -0.7884253166185480888 ) ) ;
#37201 = CONICAL_SURFACE ( 'NONE', #55241, 7.938172270156617749, 1.280189991382167047 ) ;
#37202 = EDGE_LOOP ( 'NONE', ( #40510, #22298, #30566, #63411 ) ) ;
#37203 = CARTESIAN_POINT ( 'NONE',  ( 36.00000000000000711, -3.640372113593464576, 12.21925492305365424 ) ) ;
#37204 = EDGE_CURVE ( 'NONE', #16407, #1249, #43789, .T. ) ;
#37205 = ORIENTED_EDGE ( 'NONE', *, *, #50831, .T. ) ;
#37206 = DIRECTION ( 'NONE',  ( 0.000000000000000000, 0.01356324068817992175, -0.9999080150203990547 ) ) ;
#37207 = CARTESIAN_POINT ( 'NONE',  ( -22.27713295444592845, 2.673940016109018103, -2.530364014314298249 ) ) ;
#37208 = CARTESIAN_POINT ( 'NONE',  ( 35.00000000000000000, -11.65554240571056077, 1.456211999474460672 ) ) ;
#37209 = CARTESIAN_POINT ( 'NONE',  ( 0.3164563675027631806, -8.065346584422186993, -9.237806174449842089 ) ) ;
#37210 = FACE_OUTER_BOUND ( 'NONE', #50259, .T. ) ;
#37211 = CYLINDRICAL_SURFACE ( 'NONE', #18565, 2.899999999999994582 ) ;
#37212 = EDGE_CURVE ( 'NONE', #52741, #33343, #5473, .T. ) ;
#37213 = CIRCLE ( 'NONE', #11713, 12.18649999999999878 ) ;
#37214 = ORIENTED_EDGE ( 'NONE', *, *, #61683, .T. ) ;
#37215 = CARTESIAN_POINT ( 'NONE',  ( 35.00000000000000000, 11.65554240571056788, -1.456211999474385843 ) ) ;
#37216 = AXIS2_PLACEMENT_3D ( 'NONE', #52462, #61750, #56802 ) ;
#37217 = VERTEX_POINT ( 'NONE', #63722 ) ;
#37218 = CARTESIAN_POINT ( 'NONE',  ( 2.290907136833250757, 5.963935563308487176, -4.792500160339624671 ) ) ;
#37219 = CARTESIAN_POINT ( 'NONE',  ( 12.54355452190763920, -28.27128177340750526, 13.14909765253697849 ) ) ;
#37220 = CARTESIAN_POINT ( 'NONE',  ( -27.09569413923794201, -0.6513788562879314625, -2.232620870184092610 ) ) ;
#37221 = CARTESIAN_POINT ( 'NONE',  ( 2.259830038564997867, -6.684701880279348529, 3.700395974956117051 ) ) ;
#37222 = EDGE_CURVE ( 'NONE', #26369, #64706, #36873, .T. ) ;
#37223 = ORIENTED_EDGE ( 'NONE', *, *, #15390, .T. ) ;
#37224 = FACE_OUTER_BOUND ( 'NONE', #31092, .T. ) ;
#37226 = CIRCLE ( 'NONE', #53196, 7.499999999999988454 ) ;
#37225 = CARTESIAN_POINT ( 'NONE',  ( -7.181456785175555524, 25.00000000000000000, -10.45493698471458188 ) ) ;
#37227 = DIRECTION ( 'NONE',  ( 0.000000000000000000, -0.01356324068817998940, 0.9999080150203990547 ) ) ;
#37228 = CARTESIAN_POINT ( 'NONE',  ( 26.08439714455133185, 11.40113243194252846, 3.743551691817327942 ) ) ;
#37229 = EDGE_CURVE ( 'NONE', #25053, #36560, #54246, .T. ) ;
#37230 = B_SPLINE_CURVE_WITH_KNOTS ( 'NONE', 3,
 ( #36376, #30402, #51692, #61001, #46361, #41349, #55999, #6134, #5823, #65320 ),
 .UNSPECIFIED., .F., .F.,
 ( 4, 3, 3, 4 ),
 ( 8.673617379884035472E-19, 6.607638129004461778E-05, 9.911389841680439588E-05, 0.0001667630577588628533 ),
 .UNSPECIFIED. ) ;
#37231 = AXIS2_PLACEMENT_3D ( 'NONE', #13718, #4087, #3464 ) ;
#37232 = DIRECTION ( 'NONE',  ( -1.000000000000000000, -0.000000000000000000, 0.000000000000000000 ) ) ;
#37233 = VERTEX_POINT ( 'NONE', #54094 ) ;
#37234 = PRODUCT_DEFINITION_CONTEXT ( 'detailed design', #64631, 'design' ) ;
#37235 = CARTESIAN_POINT ( 'NONE',  ( 5.514624014163232779, -0.003278974416025000511, -0.002529391395134995228 ) ) ;
#37236 = VECTOR ( 'NONE', #28117, 1000.000000000000000 ) ;
#37237 = CARTESIAN_POINT ( 'NONE',  ( 1.020182472823639053, -5.858468047365780862, -11.03967505355413081 ) ) ;
#37238 = EDGE_CURVE ( 'NONE', #57905, #23272, #8634, .T. ) ;
#37239 = ADVANCED_BREP_SHAPE_REPRESENTATION ( '', ( #7045, #24966 ), #2684 ) ;
#37240 = CIRCLE ( 'NONE', #21355, 5.000000000000000888 ) ;
#37241 = CIRCLE ( 'NONE', #12792, 5.000000000000000000 ) ;
#37242 = VECTOR ( 'NONE', #20503, 1000.000000000000000 ) ;
#37243 = ORIENTED_EDGE ( 'NONE', *, *, #60658, .F. ) ;
#37244 = EDGE_CURVE ( 'NONE', #41165, #53863, #38385, .T. ) ;
#37245 = ORIENTED_EDGE ( 'NONE', *, *, #8280, .F. ) ;
#37246 = CARTESIAN_POINT ( 'NONE',  ( 0.2650492433740052056, 2.234874822562896490, 12.04046084639674241 ) ) ;
#37247 = AXIS2_PLACEMENT_3D ( 'NONE', #43755, #64357, #8500 ) ;
#37248 = DIRECTION ( 'NONE',  ( 0.000000000000000000, 1.000000000000000000, 0.000000000000000000 ) ) ;
#37249 = CARTESIAN_POINT ( 'NONE',  ( 0.3675815128205894289, -7.689697408877338880, 9.574637318041938627 ) ) ;
#37250 = CYLINDRICAL_SURFACE ( 'NONE', #50951, 12.75000000000000178 ) ;
#37251 = VERTEX_POINT ( 'NONE', #24155 ) ;
#37252 = ORIENTED_EDGE ( 'NONE', *, *, #14707, .T. ) ;
#37253 = VERTEX_POINT ( 'NONE', #23854 ) ;
#37254 = B_SPLINE_CURVE_WITH_KNOTS ( 'NONE', 3,
 ( #34607, #19004, #24980, #19978, #29306, #9325, #49291, #40246, #54261, #24645, #29611, #43949, #24001, #59905, #24308, #44923, #60534, #44573, #14328, #65202, #39270, #59568, #14969, #28644, #35258, #3746 ),
 .UNSPECIFIED., .F., .F.,
 ( 4, 2, 2, 2, 2, 2, 2, 2, 2, 2, 2, 2, 4 ),
 ( 1.852685484479510593E-18, 0.001358278954194288126, 0.002037418431291433164, 0.002716557908388578853, 0.003395697385485724543, 0.004074836862582869798, 0.005433115816777158574, 0.006112255293874302962, 0.006791394770971447351, 0.007470534248068590871, 0.008149673725165736127, 0.009507952679360023168, 0.01086623163355430847 ),
 .UNSPECIFIED. ) ;
#37255 = CARTESIAN_POINT ( 'NONE',  ( 2.373367633546871414, 7.676289145832773109, 0.1808255748565736620 ) ) ;
#37256 = CONICAL_SURFACE ( 'NONE', #61699, 7.938172270156617749, 1.280189991382167047 ) ;
#37257 = CIRCLE ( 'NONE', #8601, 5.000000000000000888 ) ;
#37258 = CARTESIAN_POINT ( 'NONE',  ( 22.05618987420085020, 11.97361567146972483, -0.7978078888370661037 ) ) ;
#37259 = EDGE_LOOP ( 'NONE', ( #34896, #14282, #4815, #25411 ) ) ;
#37260 = LINE ( 'NONE', #43557, #48560 ) ;
#37261 = CIRCLE ( 'NONE', #26689, 5.000000000000000000 ) ;
#37262 = AXIS2_PLACEMENT_3D ( 'NONE', #11565, #46820, #2263 ) ;
#37263 = CARTESIAN_POINT ( 'NONE',  ( -37.00000000000000711, 4.426194442447240363, 11.35427606708807957 ) ) ;
#37264 = ORIENTED_EDGE ( 'NONE', *, *, #56908, .T. ) ;
#37265 =( BOUNDED_SURFACE ( )  B_SPLINE_SURFACE ( 3, 1, ( 
 ( #64844, #18008 ),
 ( #53602, #28968 ),
 ( #33628, #38269 ),
 ( #28311, #48604 ) ),
 .UNSPECIFIED., .F., .F., .F. ) 
 B_SPLINE_SURFACE_WITH_KNOTS ( ( 4, 4 ),
 ( 2, 2 ),
 ( 0.000000000000000000, 1.000000000000000000 ),
 ( 0.000000000000000000, 1.000000000000000000 ),
 .UNSPECIFIED. ) 
 GEOMETRIC_REPRESENTATION_ITEM ( )  RATIONAL_B_SPLINE_SURFACE ( (
 ( 1.000000000000000000, 1.000000000000000000),
 ( 0.9942764183789327692, 0.8450855930916580938),
 ( 0.9942764183789327692, 0.8450855930916580938),
 ( 1.000000000000000000, 1.000000000000000000) ) ) 
 REPRESENTATION_ITEM ( '' )  SURFACE ( )  );
#37266 = CARTESIAN_POINT ( 'NONE',  ( 37.00000000000000711, 0.8294751490779324055, -12.15823808070322798 ) ) ;
#37267 = CYLINDRICAL_SURFACE ( 'NONE', #6351, 4.999999999999999112 ) ;
#37268 = CARTESIAN_POINT ( 'NONE',  ( 22.88594695219327235, 3.421158645304719137, 11.50198563395281148 ) ) ;
#37269 = ORIENTED_EDGE ( 'NONE', *, *, #25355, .T. ) ;
#37270 = CIRCLE ( 'NONE', #21374, 12.18650000000000055 ) ;
#37271 = CARTESIAN_POINT ( 'NONE',  ( 0.3106921474978520115, 12.11369598333779507, -1.896868624982938289 ) ) ;
#37272 = VERTEX_POINT ( 'NONE', #64699 ) ;
#37273 = CARTESIAN_POINT ( 'NONE',  ( 2.000000000000001776, 2.469490258309515518, -6.482025155313297482 ) ) ;
#37274 = AXIS2_PLACEMENT_3D ( 'NONE', #23568, #28539, #48844 ) ;
#37275 = CARTESIAN_POINT ( 'NONE',  ( -19.18529308429517855, -4.483916446487654639, 12.73508973186750204 ) ) ;
#37276 = CARTESIAN_POINT ( 'NONE',  ( -1.327480008007509151E-11, -31.03649492335491544, -14.44372008463338908 ) ) ;
#37277 = CARTESIAN_POINT ( 'NONE',  ( -35.00000000000000000, 0.000000000000000000, 0.000000000000000000 ) ) ;
#37278 = CARTESIAN_POINT ( 'NONE',  ( 2.241449424704146320, -6.580749518451827207, 3.870245369721799555 ) ) ;
#37279 = DIRECTION ( 'NONE',  ( 1.000000000000000000, -0.000000000000000000, 0.000000000000000000 ) ) ;
#37280 = CARTESIAN_POINT ( 'NONE',  ( 1.375507693220547223, 6.813306181536364470, -10.61839108744984550 ) ) ;
#37281 = DIRECTION ( 'NONE',  ( 1.000000000000000000, -0.000000000000000000, 0.000000000000000000 ) ) ;
#37282 = ORIENTED_EDGE ( 'NONE', *, *, #32803, .T. ) ;
#37283 = DIRECTION ( 'NONE',  ( -1.000000000000000000, 0.000000000000000000, 0.000000000000000000 ) ) ;
#37284 = AXIS2_PLACEMENT_3D ( 'NONE', #36561, #46531, #40897 ) ;
#37285 = EDGE_CURVE ( 'NONE', #39958, #23378, #303, .T. ) ;
#37286 = VERTEX_POINT ( 'NONE', #5536 ) ;
#37287 =( BOUNDED_SURFACE ( )  B_SPLINE_SURFACE ( 3, 1, ( 
 ( #26453, #36436 ),
 ( #31447, #6192 ),
 ( #21478, #17795 ),
 ( #59034, #48401 ) ),
 .UNSPECIFIED., .F., .F., .F. ) 
 B_SPLINE_SURFACE_WITH_KNOTS ( ( 4, 4 ),
 ( 2, 2 ),
 ( 0.000000000000000000, 1.000000000000000000 ),
 ( 0.000000000000000000, 1.000000000000000000 ),
 .UNSPECIFIED. ) 
 GEOMETRIC_REPRESENTATION_ITEM ( )  RATIONAL_B_SPLINE_SURFACE ( (
 ( 1.000000000000000000, 1.000000000000000000),
 ( 0.6933888150995267674, 0.9895912004443193632),
 ( 0.6933888150995267674, 0.9895912004443193632),
 ( 1.000000000000000000, 1.000000000000000000) ) ) 
 REPRESENTATION_ITEM ( '' )  SURFACE ( )  );
#37288 = DIRECTION ( 'NONE',  ( 0.000000000000000000, -0.01356324068817998940, 0.9999080150203990547 ) ) ;
#37289 = CARTESIAN_POINT ( 'NONE',  ( 0.000000000000000000, -7.493043167941613625, 0.3229614270519164942 ) ) ;
#37290 = AXIS2_PLACEMENT_3D ( 'NONE', #51007, #35017, #55329 ) ;
#37291 = EDGE_LOOP ( 'NONE', ( #56545, #43884, #63490, #5653 ) ) ;
#37292 = DIRECTION ( 'NONE',  ( -1.000000000000000000, 0.000000000000000000, 0.000000000000000000 ) ) ;
#37293 = CARTESIAN_POINT ( 'NONE',  ( 0.2834382757448009604, 6.300836243950157289, 10.50792790568170432 ) ) ;
#37294 = DIRECTION ( 'NONE',  ( -1.000000000000000000, 0.000000000000000000, 0.000000000000000000 ) ) ;
#37295 = ORIENTED_EDGE ( 'NONE', *, *, #58672, .F. ) ;
#37296 = AXIS2_PLACEMENT_3D ( 'NONE', #6749, #46983, #61938 ) ;
#37297 = ADVANCED_FACE ( 'NONE', ( #56042 ), #35746, .T. ) ;
#37298 = AXIS2_PLACEMENT_3D ( 'NONE', #34118, #54437, #7553 ) ;
#37299 = ORIENTED_EDGE ( 'NONE', *, *, #24835, .F. ) ;
#37300 = CARTESIAN_POINT ( 'NONE',  ( 0.000000000000000000, 0.08317740279942427428, -7.499538753794372070 ) ) ;
#37301 = ORIENTED_EDGE ( 'NONE', *, *, #31804, .T. ) ;
#37302 = CARTESIAN_POINT ( 'NONE',  ( 2.990245332647882393, 3.377079998295721808, -7.779904630197268744 ) ) ;
#37303 = DIRECTION ( 'NONE',  ( -1.000000000000000000, 0.000000000000000000, 0.000000000000000000 ) ) ;
#37304 = CARTESIAN_POINT ( 'NONE',  ( -3.014567788889948474, -9.061531127596236246, 10.01322194078947447 ) ) ;
#37305 = DIRECTION ( 'NONE',  ( 0.000000000000000000, -0.01356324068817992175, 0.9999080150203990547 ) ) ;
#37306 = DIRECTION ( 'NONE',  ( 0.000000000000000000, -0.7617968321374810614, -0.6478160128812026075 ) ) ;
#37307 = EDGE_CURVE ( 'NONE', #28763, #56470, #44754, .T. ) ;
#37308 = ORIENTED_EDGE ( 'NONE', *, *, #22672, .F. ) ;
#37309 = DIRECTION ( 'NONE',  ( 0.000000000000000000, -0.8369827122275286246, -0.5472293298355360713 ) ) ;
#37310 = VECTOR ( 'NONE', #41041, 1000.000000000000000 ) ;
#37311 = EDGE_CURVE ( 'NONE', #33819, #53510, #36021, .T. ) ;
#37312 = CARTESIAN_POINT ( 'NONE',  ( 27.65241022803075666, 12.51656249166301116, 5.069893477639606516 ) ) ;
#37313 = CARTESIAN_POINT ( 'NONE',  ( 3.152665057735546839, 0.4801242025606423658, 7.923639299008859105 ) ) ;
#37314 = B_SPLINE_CURVE_WITH_KNOTS ( 'NONE', 3,
 ( #50849, #45860, #20246, #24925, #56145, #55168, #40527 ),
 .UNSPECIFIED., .F., .F.,
 ( 4, 3, 4 ),
 ( 0.000000000000000000, 0.001700533616330518905, 0.005002426799371241864 ),
 .UNSPECIFIED. ) ;
#37315 = CARTESIAN_POINT ( 'NONE',  ( -18.04458733766117362, 11.34280559204706584, 3.916728392552376370 ) ) ;
#37316 = DIRECTION ( 'NONE',  ( -1.000000000000000000, 0.000000000000000000, 0.000000000000000000 ) ) ;
#37317 = CARTESIAN_POINT ( 'NONE',  ( -9.044048956294579611, -11.38398270688160530, -3.796001806769629727 ) ) ;
#37318 = DIRECTION ( 'NONE',  ( -0.000000000000000000, -1.000000000000000000, -0.000000000000000000 ) ) ;
#37319 = DIRECTION ( 'NONE',  ( -1.000000000000000000, 0.000000000000000000, 0.000000000000000000 ) ) ;
#37320 = CIRCLE ( 'NONE', #14999, 7.499999999999988454 ) ;
#37321 = ADVANCED_FACE ( 'NONE', ( #55398 ), #9836, .T. ) ;
#37322 = VERTEX_POINT ( 'NONE', #65676 ) ;
#37323 = DIRECTION ( 'NONE',  ( 0.000000000000000000, 0.3554799084908900619, 0.9346839223284566511 ) ) ;
#37324 = CARTESIAN_POINT ( 'NONE',  ( 4.638437190804134858, -10.09537402753981361, 8.963882972395243343 ) ) ;
#37325 = CIRCLE ( 'NONE', #44728, 12.75000000000000178 ) ;
#37326 = ORIENTED_EDGE ( 'NONE', *, *, #6886, .T. ) ;
#37327 = CARTESIAN_POINT ( 'NONE',  ( -37.00000000000000711, -11.01837265713077763, 6.415447294506668285 ) ) ;
#37328 = CARTESIAN_POINT ( 'NONE',  ( 1.000000000000000888, 1.693411908627302509, -7.306323022404582979 ) ) ;
#37329 = ORIENTED_EDGE ( 'NONE', *, *, #83, .T. ) ;
#37330 = VECTOR ( 'NONE', #47497, 1000.000000000000114 ) ;
#37331 = CARTESIAN_POINT ( 'NONE',  ( -35.00000000000000000, 1.791059740004591561, -12.05416472667163674 ) ) ;
#37332 = ORIENTED_EDGE ( 'NONE', *, *, #50277, .T. ) ;
#37333 = LINE ( 'NONE', #62935, #917 ) ;
#37334 = ORIENTED_EDGE ( 'NONE', *, *, #49696, .F. ) ;
#37335 = ORIENTED_EDGE ( 'NONE', *, *, #25679, .F. ) ;
#37336 = EDGE_CURVE ( 'NONE', #37187, #14288, #62782, .T. ) ;
#37337 = AXIS2_PLACEMENT_3D ( 'NONE', #10499, #21134, #26457 ) ;
#37338 = CARTESIAN_POINT ( 'NONE',  ( 37.00000000000000711, -5.865551165830999558, 11.32068061209301213 ) ) ;
#37339 = CIRCLE ( 'NONE', #45850, 4.999999999999999112 ) ;
#37340 = ORIENTED_EDGE ( 'NONE', *, *, #51046, .T. ) ;
#37341 = DIRECTION ( 'NONE',  ( -1.000000000000000000, 0.000000000000000000, -0.000000000000000000 ) ) ;
#37342 = CARTESIAN_POINT ( 'NONE',  ( 5.515539859299206427, 0.006049968793488397570, 0.0001942659352248016788 ) ) ;
#37343 = CARTESIAN_POINT ( 'NONE',  ( 35.00000000000000000, -11.53507381115584529, -2.216820770815045805 ) ) ;
#37344 = CARTESIAN_POINT ( 'NONE',  ( 35.00000000000000000, 4.705694406421931860E-17, -3.469127814946512892E-15 ) ) ;
#37345 = ORIENTED_EDGE ( 'NONE', *, *, #17584, .T. ) ;
#37346 = CARTESIAN_POINT ( 'NONE',  ( 0.2671309869109471657, -7.747281147400610912, 9.484919892054794133 ) ) ;
#37347 = CARTESIAN_POINT ( 'NONE',  ( -4.291397156012838110, -28.05769852054401881, 12.02237517917411047 ) ) ;
#37348 = DIRECTION ( 'NONE',  ( -1.000000000000000000, -0.000000000000000000, 0.000000000000000000 ) ) ;
#37349 = ORIENTED_EDGE ( 'NONE', *, *, #47798, .F. ) ;
#37350 = DIRECTION ( 'NONE',  ( 0.000000000000000000, 0.000000000000000000, 1.000000000000000000 ) ) ;
#37351 = ORIENTED_EDGE ( 'NONE', *, *, #57993, .F. ) ;
#37352 = CARTESIAN_POINT ( 'NONE',  ( 0.2650492433740071485, 9.309907554970086707, -7.955688793815992810 ) ) ;
#37353 = ORIENTED_EDGE ( 'NONE', *, *, #22162, .F. ) ;
#37354 = CARTESIAN_POINT ( 'NONE',  ( 24.17635063625124658, -8.757419633580374452, -8.209409434500527070 ) ) ;
#37355 = AXIS2_PLACEMENT_3D ( 'NONE', #45499, #54190, #34545 ) ;
#37356 = DIRECTION ( 'NONE',  ( -1.000000000000000000, 0.000000000000000000, 0.000000000000000000 ) ) ;
#37357 = CARTESIAN_POINT ( 'NONE',  ( 0.6511581176957849104, -4.541862140119324209, 11.51117493088887045 ) ) ;
#37358 = AXIS2_PLACEMENT_3D ( 'NONE', #58880, #13294, #52874 ) ;
#37359 = ORIENTED_EDGE ( 'NONE', *, *, #35983, .F. ) ;
#37360 = CARTESIAN_POINT ( 'NONE',  ( 0.6473888112830245012, 8.203438694127655140, 9.263269341114806821 ) ) ;
#37361 = DIRECTION ( 'NONE',  ( 0.000000000000000000, -0.6269146997507875074, -0.7790879021242596014 ) ) ;
#37362 = CARTESIAN_POINT ( 'NONE',  ( 12.87841448470966377, 11.26304985228344258, -7.445374560091265081 ) ) ;
#37364 = ORIENTED_EDGE ( 'NONE', *, *, #28357, .T. ) ;
#37363 = VECTOR ( 'NONE', #10400, 1000.000000000000000 ) ;
#37365 = ADVANCED_FACE ( 'NONE', ( #10168 ), #4865, .F. ) ;
#37366 = ORIENTED_EDGE ( 'NONE', *, *, #48857, .F. ) ;
#37367 = LINE ( 'NONE', #17432, #14657 ) ;
#37368 = ORIENTED_EDGE ( 'NONE', *, *, #63187, .T. ) ;
#37369 = ADVANCED_FACE ( 'NONE', ( #21468 ), #62655, .T. ) ;
#37370 = ORIENTED_EDGE ( 'NONE', *, *, #43519, .F. ) ;
#37371 = CIRCLE ( 'NONE', #54347, 12.75000000000000178 ) ;
#37372 = DIRECTION ( 'NONE',  ( -1.000000000000000000, 0.000000000000000000, 0.000000000000000000 ) ) ;
#37373 = CARTESIAN_POINT ( 'NONE',  ( 0.4613984246114880561, -10.51786362586218893, 6.399144685811677391 ) ) ;
#37374 = CARTESIAN_POINT ( 'NONE',  ( -35.00000000000000000, -0.01609748574453131326, 11.74614673114904129 ) ) ;
#37375 = CARTESIAN_POINT ( 'NONE',  ( 37.00000000000000711, 4.705694406421931860E-17, -3.469127814946512892E-15 ) ) ;
#37376 = CARTESIAN_POINT ( 'NONE',  ( 5.530133899448235191, 0.006510401266731621894, -0.01459891979722821240 ) ) ;
#37377 = EDGE_CURVE ( 'NONE', #54727, #26353, #6182, .T. ) ;
#37378 = CARTESIAN_POINT ( 'NONE',  ( 35.00000000000000000, -10.91536515067650903, -4.339012074899918581 ) ) ;
#37379 = ORIENTED_EDGE ( 'NONE', *, *, #42312, .F. ) ;
#37380 = DIRECTION ( 'NONE',  ( 1.000000000000000000, 0.000000000000000000, 0.000000000000000000 ) ) ;
#37381 = FACE_OUTER_BOUND ( 'NONE', #7242, .T. ) ;
#37382 = ADVANCED_FACE ( 'NONE', ( #22108 ), #7143, .T. ) ;
#37383 = AXIS2_PLACEMENT_3D ( 'NONE', #50118, #4574, #566 ) ;
#37384 = VECTOR ( 'NONE', #15235, 1000.000000000000000 ) ;
#37385 = AXIS2_PLACEMENT_3D ( 'NONE', #37626, #32939, #57923 ) ;
#37386 = CARTESIAN_POINT ( 'NONE',  ( -35.04643116707788408, -0.007621814750504232738, -0.009511118309140503824 ) ) ;
#37387 = DIRECTION ( 'NONE',  ( 0.000000000000000000, -0.5987040770935737610, 0.8009703041134120793 ) ) ;
#37388 = CIRCLE ( 'NONE', #3444, 3.999999999999999556 ) ;
#37389 = CARTESIAN_POINT ( 'NONE',  ( -10.95212338237647920, -9.902220863987562183, -9.175839033069911110 ) ) ;
#37390 = EDGE_CURVE ( 'NONE', #42435, #38749, #60660, .T. ) ;
#37391 = LINE ( 'NONE', #31734, #41568 ) ;
#37392 = DIRECTION ( 'NONE',  ( 0.000000000000000000, 0.000000000000000000, 1.000000000000000000 ) ) ;
#37393 = ORIENTED_EDGE ( 'NONE', *, *, #32639, .F. ) ;
#37394 = CARTESIAN_POINT ( 'NONE',  ( -27.08417142187571613, 0.4261087887162147148, 2.251180450989566317 ) ) ;
#37395 = CYLINDRICAL_SURFACE ( 'NONE', #14404, 12.18650000000000055 ) ;
#37396 = CARTESIAN_POINT ( 'NONE',  ( -22.94572469358971034, -2.078200699019439934, -4.424217216616522563 ) ) ;
#37397 = CARTESIAN_POINT ( 'NONE',  ( 2.717984159220127260, -1.631703089060319911, -7.620583877640776826 ) ) ;
#37398 = CIRCLE ( 'NONE', #17245, 5.000000000000000888 ) ;
#37399 = CIRCLE ( 'NONE', #4489, 6.936499999999989896 ) ;
#37400 = DIRECTION ( 'NONE',  ( -0.000000000000000000, -0.000000000000000000, -1.000000000000000000 ) ) ;
#37401 = DIRECTION ( 'NONE',  ( 0.000000000000000000, 0.5472293298355215274, -0.8369827122275381726 ) ) ;
#37402 = CIRCLE ( 'NONE', #8762, 2.899999999999995026 ) ;
#37403 = ORIENTED_EDGE ( 'NONE', *, *, #26485, .F. ) ;
#37404 = CARTESIAN_POINT ( 'NONE',  ( -35.00000000000000000, 12.18359334611896472, 0.2661492558803780772 ) ) ;
#37405 = CARTESIAN_POINT ( 'NONE',  ( 35.00000000000000000, 11.68758509253246558, -1.171570255487653700 ) ) ;
#37406 = CARTESIAN_POINT ( 'NONE',  ( 0.2676618633000477643, 9.277614237849274303, 7.994628339664862082 ) ) ;
#37407 = AXIS2_PLACEMENT_3D ( 'NONE', #21247, #27226, #22232 ) ;
#37408 = CARTESIAN_POINT ( 'NONE',  ( 1.719304012339826659, -12.64775761152879596, -1.452142814149639305 ) ) ;
#37409 = ORIENTED_EDGE ( 'NONE', *, *, #35275, .T. ) ;
#37410 = CARTESIAN_POINT ( 'NONE',  ( 0.000000000000000000, 0.000000000000000000, 0.000000000000000000 ) ) ;
#37411 = DIRECTION ( 'NONE',  ( 1.000000000000000000, 0.000000000000000000, -0.000000000000000000 ) ) ;
#37413 = VERTEX_POINT ( 'NONE', #27418 ) ;
#37412 = CARTESIAN_POINT ( 'NONE',  ( 0.2653519890518162283, -12.24619734961135187, 8.824939080896778643E-06 ) ) ;
#37414 = CARTESIAN_POINT ( 'NONE',  ( 2.000000000000001776, 0.000000000000000000, 0.000000000000000000 ) ) ;
#37415 = ADVANCED_FACE ( 'NONE', ( #42703 ), #1188, .T. ) ;
#37416 = DIRECTION ( 'NONE',  ( 0.000000000000000000, -0.01356324068817991828, 0.9999080150203990547 ) ) ;
#37417 = ORIENTED_EDGE ( 'NONE', *, *, #12796, .T. ) ;
#37418 = CARTESIAN_POINT ( 'NONE',  ( 0.3002738374340819250, -9.533456882268691146, 7.705051734330245594 ) ) ;
#37419 = AXIS2_PLACEMENT_3D ( 'NONE', #4267, #24539, #44817 ) ;
#37420 = CARTESIAN_POINT ( 'NONE',  ( 0.3040950598368152291, -5.912066680610686298, 10.74226959800789594 ) ) ;
#37421 = CARTESIAN_POINT ( 'NONE',  ( 2.241509619876139059, 7.525055189891922680, -1.287997509666494400 ) ) ;
#37422 = DIRECTION ( 'NONE',  ( -0.000000000000000000, -0.000000000000000000, -1.000000000000000000 ) ) ;
#37423 = FACE_OUTER_BOUND ( 'NONE', #3805, .T. ) ;
#37424 = CARTESIAN_POINT ( 'NONE',  ( 0.8320506296491609888, 11.81055997318803996, 3.891425424503343944 ) ) ;
#37426 = ORIENTED_EDGE ( 'NONE', *, *, #36241, .F. ) ;
#37425 = FACE_OUTER_BOUND ( 'NONE', #10962, .T. ) ;
#37427 = CARTESIAN_POINT ( 'NONE',  ( 10.22080531381022972, 7.430815483004926669, 11.27448495604908452 ) ) ;
#37428 = ORIENTED_EDGE ( 'NONE', *, *, #58787, .T. ) ;
#37429 = VECTOR ( 'NONE', #33334, 1000.000000000000000 ) ;
#37430 = FACE_OUTER_BOUND ( 'NONE', #46110, .T. ) ;
#37431 = VERTEX_POINT ( 'NONE', #41394 ) ;
#37432 = VECTOR ( 'NONE', #23290, 1000.000000000000000 ) ;
#37433 = B_SPLINE_CURVE_WITH_KNOTS ( 'NONE', 3,
 ( #42403, #22146, #38427, #12170, #22482, #28444, #23466, #12482, #27795, #48098, #38087, #48747, #64023, #13471, #42745, #17163 ),
 .UNSPECIFIED., .F., .F.,
 ( 4, 3, 3, 3, 3, 4 ),
 ( 7.973125766754336844E-18, 6.991367980366376635E-05, 0.0001398269368981360438, 0.0002097400188389090918, 0.0002811534801551364318, 0.0003526297678872492036 ),
 .UNSPECIFIED. ) ;
#37434 = ITEM_DEFINED_TRANSFORMATION ( 'NONE', 'NONE', #23973,  #24966 ) ;
#37435 = CARTESIAN_POINT ( 'NONE',  ( 1.719304012338199295, 12.70777170743846796, -0.7661785589580241140 ) ) ;
#37437 = CARTESIAN_POINT ( 'NONE',  ( -3.857720864536276828, 10.47202569828348651, 5.863983351155762413 ) ) ;
#37436 = CIRCLE ( 'NONE', #38539, 5.000000000000000888 ) ;
#37438 = EDGE_CURVE ( 'NONE', #1482, #60562, #39426, .T. ) ;
#37439 = CARTESIAN_POINT ( 'NONE',  ( -48.68114316863543678, -0.2655233219083077412, -3.919294168552598379 ) ) ;
#37440 = CARTESIAN_POINT ( 'NONE',  ( -37.00000000000000711, -9.677500615117949678, 6.657191900728284928 ) ) ;
#37441 = ORIENTED_EDGE ( 'NONE', *, *, #51371, .F. ) ;
#37442 = CARTESIAN_POINT ( 'NONE',  ( 0.3665391374699472626, 1.872534962004960724, -12.13918562134716694 ) ) ;
#37443 = EDGE_CURVE ( 'NONE', #10928, #38977, #26776, .T. ) ;
#37444 = CARTESIAN_POINT ( 'NONE',  ( 1.194176325881339595, -3.807610977967000654, 11.96454551582841219 ) ) ;
#37445 = VERTEX_POINT ( 'NONE', #21809 ) ;
#37447 = ORIENTED_EDGE ( 'NONE', *, *, #61380, .T. ) ;
#37446 = B_SPLINE_CURVE_WITH_KNOTS ( 'NONE', 3,
 ( #45671, #20079, #61607, #50678, #35359, #61957, #36679, #15723, #60639, #5123, #46341, #25390, #127, #60981, #11403, #51986, #10414, #20408 ),
 .UNSPECIFIED., .F., .F.,
 ( 4, 2, 2, 2, 2, 2, 2, 2, 4 ),
 ( 2.453269466693398698E-18, 0.002548279257371096305, 0.003185349071713867563, 0.003822418886056638387, 0.005096558514742179601, 0.006370698143427721248, 0.007644837772113261161, 0.008918977400798800206, 0.01019311702948434012 ),
 .UNSPECIFIED. ) ;
#37448 = FACE_OUTER_BOUND ( 'NONE', #41001, .T. ) ;
#37449 = EDGE_CURVE ( 'NONE', #46319, #11584, #3574, .T. ) ;
#37450 = VERTEX_POINT ( 'NONE', #23099 ) ;
#37451 = DIRECTION ( 'NONE',  ( 0.000000000000000000, 0.01356324068817998940, -0.9999080150203990547 ) ) ;
#37452 = CARTESIAN_POINT ( 'NONE',  ( -22.71097035706202405, 4.510116093748279376, -2.118550233809386896 ) ) ;
#37453 = DIRECTION ( 'NONE',  ( 0.000000000000000000, 0.9246979985058736418, 0.3807014730195186769 ) ) ;
#37454 = LINE ( 'NONE', #12182, #23097 ) ;
#37455 = AXIS2_PLACEMENT_3D ( 'NONE', #61531, #11332, #27275 ) ;
#37456 = CARTESIAN_POINT ( 'NONE',  ( -37.25000000000001421, -27.44817602132958356, -3.024649682742615919 ) ) ;
#37457 = CARTESIAN_POINT ( 'NONE',  ( 0.000000000000000000, -1.779948802829750543, -6.576141558201276993 ) ) ;
#37458 = EDGE_CURVE ( 'NONE', #4186, #1369, #13122, .T. ) ;
#37459 = DIRECTION ( 'NONE',  ( 1.000000000000000000, -0.000000000000000000, 0.000000000000000000 ) ) ;
#37460 = ORIENTED_EDGE ( 'NONE', *, *, #53859, .T. ) ;
#37461 = DIRECTION ( 'NONE',  ( 0.000000000000000000, 0.000000000000000000, 1.000000000000000000 ) ) ;
#37462 = EDGE_CURVE ( 'NONE', #9134, #59369, #37736, .T. ) ;
#37463 = VERTEX_POINT ( 'NONE', #38048 ) ;
#37464 = CIRCLE ( 'NONE', #32181, 6.936499999999989896 ) ;
#37465 = DIRECTION ( 'NONE',  ( 1.000000000000000000, 0.000000000000000000, 0.000000000000000000 ) ) ;
#37466 = CARTESIAN_POINT ( 'NONE',  ( -35.04660725145885891, 0.01223081933021788817, -0.001288602543501626970 ) ) ;
#37467 = CARTESIAN_POINT ( 'NONE',  ( 2.430348790457107278, -2.814990071337903910, -7.164221884688188879 ) ) ;
#37468 = LINE ( 'NONE', #52119, #42518 ) ;
#37469 = ORIENTED_EDGE ( 'NONE', *, *, #15510, .T. ) ;
#37470 = VERTEX_POINT ( 'NONE', #58031 ) ;
#37471 = CARTESIAN_POINT ( 'NONE',  ( 0.000000000000000000, -6.812627895098285258, -0.04423456934733380197 ) ) ;
#37472 = ADVANCED_FACE ( 'NONE', ( #12446 ), #28101, .T. ) ;
#37473 =( BOUNDED_CURVE ( )  B_SPLINE_CURVE ( 3, ( #52976, #39309, #43646, #34330 ),
 .UNSPECIFIED., .F., .F. ) 
 B_SPLINE_CURVE_WITH_KNOTS ( ( 4, 4 ),
 ( 1.737343023833860078, 1.756906829757061361 ),
 .UNSPECIFIED. ) 
 CURVE ( )  GEOMETRIC_REPRESENTATION_ITEM ( )  RATIONAL_B_SPLINE_CURVE ( ( 1.000000000000000000, 0.9999681050458084641, 0.9999681050458084641, 1.000000000000000000 ) ) 
 REPRESENTATION_ITEM ( '' )  );
#37474 = VERTEX_POINT ( 'NONE', #8796 ) ;
#37475 = CARTESIAN_POINT ( 'NONE',  ( 0.3474126878361824544, 7.689340002166858312, -9.566300984424323417 ) ) ;
#37476 = DIRECTION ( 'NONE',  ( -1.000000000000000000, 0.000000000000000000, 0.000000000000000000 ) ) ;
#37477 = ADVANCED_FACE ( 'NONE', ( #53371 ), #48708, .T. ) ;
#37478 = CARTESIAN_POINT ( 'NONE',  ( 0.8320506296491597675, -9.767350172724373891, -7.696193170530718497 ) ) ;
#37479 = CARTESIAN_POINT ( 'NONE',  ( 2.242819959140644581, 1.426511055719408283, -7.500446639314762187 ) ) ;
#37480 = ORIENTED_EDGE ( 'NONE', *, *, #16399, .F. ) ;
#37481 = AXIS2_PLACEMENT_3D ( 'NONE', #34937, #64881, #39625 ) ;
#37482 = CARTESIAN_POINT ( 'NONE',  ( 0.2872850955227749803, 12.10187515377843326, 1.921748909352199775 ) ) ;
#37483 = CARTESIAN_POINT ( 'NONE',  ( 2.241352910868908310, -0.08337961031698915004, -7.633946224498474820 ) ) ;
#37484 = AXIS2_PLACEMENT_3D ( 'NONE', #34792, #40119, #50776 ) ;
#37485 = CARTESIAN_POINT ( 'NONE',  ( 35.00000000000000000, -5.428340790341627198, 10.91072401419415883 ) ) ;
#37486 = CARTESIAN_POINT ( 'NONE',  ( -47.41189015808931373, -0.5144011408980343480, 11.10762064040664221 ) ) ;
#37487 = AXIS2_PLACEMENT_3D ( 'NONE', #3086, #23347, #63904 ) ;
#37488 = AXIS2_PLACEMENT_3D ( 'NONE', #57153, #37171, #47819 ) ;
#37489 = CARTESIAN_POINT ( 'NONE',  ( 2.305787727787084407, -0.1666591538752151269, -7.654065630109508689 ) ) ;
#37490 = DIRECTION ( 'NONE',  ( 0.000000000000000000, -0.01356324068817998940, 0.9999080150203990547 ) ) ;
#37491 = ORIENTED_EDGE ( 'NONE', *, *, #63581, .T. ) ;
#37492 = CIRCLE ( 'NONE', #34309, 5.000000000000000000 ) ;
#37493 = CARTESIAN_POINT ( 'NONE',  ( -18.91767133624980701, -28.94173879345719058, -6.680047468371234309 ) ) ;
#37494 = VERTEX_POINT ( 'NONE', #54017 ) ;
#37495 = CARTESIAN_POINT ( 'NONE',  ( -5.871534791385524699, -0.9854293836816523378, -13.46435699085508908 ) ) ;
#37496 = DIRECTION ( 'NONE',  ( 0.000000000000000000, 0.000000000000000000, 1.000000000000000000 ) ) ;
#37497 = CARTESIAN_POINT ( 'NONE',  ( 5.514624014163232779, -0.004045310349816146414, 0.0008859786816847309548 ) ) ;
#37498 = CIRCLE ( 'NONE', #38601, 12.75000000000000178 ) ;
#37499 = DIRECTION ( 'NONE',  ( 1.000000000000000000, -0.000000000000000000, 0.000000000000000000 ) ) ;
#37500 = CARTESIAN_POINT ( 'NONE',  ( 37.00000000000000711, 12.15823808070323508, 0.8294751490777961811 ) ) ;
#37501 = CIRCLE ( 'NONE', #12009, 2.899999999999994582 ) ;
#37502 = EDGE_CURVE ( 'NONE', #17695, #16904, #1291, .T. ) ;
#37503 = EDGE_CURVE ( 'NONE', #23892, #54738, #57546, .T. ) ;
#37504 = ORIENTED_EDGE ( 'NONE', *, *, #39789, .F. ) ;
#37505 = VERTEX_POINT ( 'NONE', #44346 ) ;
#37506 = CARTESIAN_POINT ( 'NONE',  ( 0.3160775863651129614, 1.892533050396167260, 12.11619190710938732 ) ) ;
#37507 = ORIENTED_EDGE ( 'NONE', *, *, #29695, .F. ) ;
#37508 = LINE ( 'NONE', #42816, #61684 ) ;
#37509 = CARTESIAN_POINT ( 'NONE',  ( 3.423954070241203240, 5.768012864559385555, -12.21298188730038881 ) ) ;
#37510 = CARTESIAN_POINT ( 'NONE',  ( 35.00000000000000000, 6.950793414699941941, 10.68873102412834797 ) ) ;
#37511 = DIRECTION ( 'NONE',  ( 0.000000000000000000, 0.9987865678893279586, -0.04924826701374244303 ) ) ;
#37512 = CARTESIAN_POINT ( 'NONE',  ( 1.719304012340734378, -7.581471372739226666, -10.22720798541506682 ) ) ;
#37513 = VECTOR ( 'NONE', #11937, 1000.000000000000000 ) ;
#37514 = CARTESIAN_POINT ( 'NONE',  ( 2.256373768223411069, -1.195444820369733430, 7.545294827890043798 ) ) ;
#37515 = CARTESIAN_POINT ( 'NONE',  ( 5.514970785353741078, -0.004532877335078721974, -0.001326349372336278450 ) ) ;
#37516 = VERTEX_POINT ( 'NONE', #8457 ) ;
#37517 = ORIENTED_EDGE ( 'NONE', *, *, #3391, .T. ) ;
#37518 = ADVANCED_FACE ( 'NONE', ( #43042 ), #59330, .T. ) ;
#37519 = CARTESIAN_POINT ( 'NONE',  ( -35.00000000000000000, 0.000000000000000000, 0.000000000000000000 ) ) ;
#37520 = ORIENTED_EDGE ( 'NONE', *, *, #46770, .T. ) ;
#37521 = CARTESIAN_POINT ( 'NONE',  ( 23.30204873196431237, -11.22993834942661273, -7.499434092014816144 ) ) ;
#37522 = DIRECTION ( 'NONE',  ( 1.000000000000000000, 0.000000000000000000, 0.000000000000000000 ) ) ;
#37523 = AXIS2_PLACEMENT_3D ( 'NONE', #37926, #37608, #17331 ) ;
#37524 = ADVANCED_FACE ( 'NONE', ( #18777 ), #58703, .T. ) ;
#37525 = DIRECTION ( 'NONE',  ( -1.000000000000000000, 0.000000000000000000, 0.000000000000000000 ) ) ;
#37526 = ORIENTED_EDGE ( 'NONE', *, *, #4717, .F. ) ;
#37527 = PLANE ( 'NONE',  #65135 ) ;
#37528 = CARTESIAN_POINT ( 'NONE',  ( -14.21898193534930144, -33.70038524408754910, -9.575031237889035651 ) ) ;
#37529 = CARTESIAN_POINT ( 'NONE',  ( 2.639814597422740050, -1.600543348184864545, 7.600559958731741617 ) ) ;
#37530 = ORIENTED_EDGE ( 'NONE', *, *, #63274, .F. ) ;
#37531 = ORIENTED_EDGE ( 'NONE', *, *, #41500, .T. ) ;
#37532 = CARTESIAN_POINT ( 'NONE',  ( 3.291290029914074378, 8.250315036047103590, 10.68561190601527855 ) ) ;
#37533 = EDGE_CURVE ( 'NONE', #37217, #8268, #35249, .T. ) ;
#37534 = ORIENTED_EDGE ( 'NONE', *, *, #41512, .F. ) ;
#37535 = ORIENTED_EDGE ( 'NONE', *, *, #13468, .F. ) ;
#37537 = CARTESIAN_POINT ( 'NONE',  ( 2.297017764050091948, 3.968300849026757948, 6.543724852214691801 ) ) ;
#37536 = VECTOR ( 'NONE', #46254, 1000.000000000000000 ) ;
#37538 = AXIS2_PLACEMENT_3D ( 'NONE', #8422, #28695, #23733 ) ;
#37539 = EDGE_LOOP ( 'NONE', ( #12508, #27351, #43357, #29273 ) ) ;
#37540 = ORIENTED_EDGE ( 'NONE', *, *, #16395, .T. ) ;
#37541 = CARTESIAN_POINT ( 'NONE',  ( -22.27716857039623477, -2.705892286796401702, 2.496432241075906333 ) ) ;
#37542 = DIRECTION ( 'NONE',  ( -1.000000000000000000, -1.836970198721029688E-16, 0.000000000000000000 ) ) ;
#37543 = AXIS2_PLACEMENT_3D ( 'NONE', #6507, #5877, #47079 ) ;
#37544 = AXIS2_PLACEMENT_3D ( 'NONE', #29182, #23877, #28507 ) ;
#37545 = CYLINDRICAL_SURFACE ( 'NONE', #29883, 3.309571291727934295 ) ;
#37546 = DIRECTION ( 'NONE',  ( -1.000000000000000000, 0.000000000000000000, 0.000000000000000000 ) ) ;
#37547 = DIRECTION ( 'NONE',  ( -1.000000000000000000, 0.000000000000000000, 0.000000000000000000 ) ) ;
#37548 = DIRECTION ( 'NONE',  ( -1.000000000000000000, 0.000000000000000000, -0.000000000000000000 ) ) ;
#37549 = ORIENTED_EDGE ( 'NONE', *, *, #21634, .T. ) ;
#37550 = CARTESIAN_POINT ( 'NONE',  ( -36.00000000000000711, -9.733281772932221187, 8.235637554476612721 ) ) ;
#37551 = EDGE_CURVE ( 'NONE', #48302, #12489, #25677, .T. ) ;
#37553 = CARTESIAN_POINT ( 'NONE',  ( 2.373367633546855426, 4.795703124519890892, 5.996611082971977424 ) ) ;
#37552 = CIRCLE ( 'NONE', #8874, 2.899999999999995026 ) ;
#37554 = DIRECTION ( 'NONE',  ( 0.000000000000000000, 0.000000000000000000, 1.000000000000000000 ) ) ;
#37555 = EDGE_CURVE ( 'NONE', #33347, #37684, #56679, .T. ) ;
#37556 = CARTESIAN_POINT ( 'NONE',  ( 0.2956976708475454463, -2.344604179391494458, 12.02996380804952814 ) ) ;
#37557 = VECTOR ( 'NONE', #434, 1000.000000000000000 ) ;
#37558 = CYLINDRICAL_SURFACE ( 'NONE', #40327, 5.000000000000000000 ) ;
#37559 = CARTESIAN_POINT ( 'NONE',  ( 2.000000000000001776, 5.450255447309811707, -4.087611905901392007 ) ) ;
#37560 = B_SPLINE_CURVE_WITH_KNOTS ( 'NONE', 3,
 ( #14686, #50314, #44079, #63043, #23139, #30003, #43403, #22825, #39979, #33448, #18511, #59064, #63680 ),
 .UNSPECIFIED., .F., .F.,
 ( 4, 3, 3, 3, 4 ),
 ( 0.0002792983885906414167, 0.0002796382307041358844, 0.0003495477861619811287, 0.0004194573423310287916, 0.0005586102576333146046 ),
 .UNSPECIFIED. ) ;
#37561 = EDGE_CURVE ( 'NONE', #22141, #55015, #38724, .T. ) ;
#37562 = AXIS2_PLACEMENT_3D ( 'NONE', #47738, #17805, #32737 ) ;
#37563 = VERTEX_POINT ( 'NONE', #33721 ) ;
#37564 = CARTESIAN_POINT ( 'NONE',  ( -14.37650451283982100, 8.347980080371831590, -8.621445213188774659 ) ) ;
#37565 = ADVANCED_FACE ( 'NONE', ( #28736 ), #49052, .T. ) ;
#37566 = AXIS2_PLACEMENT_3D ( 'NONE', #29987, #35625, #14034 ) ;
#37567 = ORIENTED_EDGE ( 'NONE', *, *, #21930, .T. ) ;
#37568 = CARTESIAN_POINT ( 'NONE',  ( 2.655192694324000069, 3.822392723567352490, 8.807900729499975157 ) ) ;
#37569 = CARTESIAN_POINT ( 'NONE',  ( 2.000000000000001776, 1.956810415765277922, -6.654767106875532967 ) ) ;
#37570 = CIRCLE ( 'NONE', #63047, 5.000000000000000888 ) ;
#37571 = CARTESIAN_POINT ( 'NONE',  ( 11.49573924273014391, -13.34169095181821341, -2.066154205673190969 ) ) ;
#37572 = EDGE_CURVE ( 'NONE', #57134, #35533, #62837, .T. ) ;
#37573 = CARTESIAN_POINT ( 'NONE',  ( -27.09125059358653331, -0.6356863790372184742, -2.223272438024536779 ) ) ;
#37574 = CARTESIAN_POINT ( 'NONE',  ( 2.290907136833251645, -6.705538900522852508, 3.684064771923238002 ) ) ;
#37575 = ORIENTED_EDGE ( 'NONE', *, *, #27493, .F. ) ;
#37576 = CARTESIAN_POINT ( 'NONE',  ( 0.5547464869798224285, 10.53334899235179734, -6.433541106624982575 ) ) ;
#37577 = CARTESIAN_POINT ( 'NONE',  ( 0.000000000000000000, -6.750946897830710114, 1.593658756657014397 ) ) ;
#37578 = DIRECTION ( 'NONE',  ( 0.000000000000000000, 0.01356324068817998940, -0.9999080150203990547 ) ) ;
#37579 = CARTESIAN_POINT ( 'NONE',  ( -2.952869152607111136, 7.581333670610111319, 11.17020052527586138 ) ) ;
#37580 = CIRCLE ( 'NONE', #1467, 12.18650000000000055 ) ;
#37581 = CARTESIAN_POINT ( 'NONE',  ( 37.00000000000000711, 6.547236723514018308, -9.752226076388918585 ) ) ;
#37582 = ORIENTED_EDGE ( 'NONE', *, *, #4032, .T. ) ;
#37583 = CARTESIAN_POINT ( 'NONE',  ( 5.516018279890452902, 0.005331956019561467572, 0.004180585980734550546 ) ) ;
#37584 = CIRCLE ( 'NONE', #53554, 5.000000000000001776 ) ;
#37585 = AXIS2_PLACEMENT_3D ( 'NONE', #34169, #18247, #64740 ) ;
#37586 = CIRCLE ( 'NONE', #54606, 7.499999999999988454 ) ;
#37587 = EDGE_CURVE ( 'NONE', #217, #52756, #3398, .T. ) ;
#37588 = ORIENTED_EDGE ( 'NONE', *, *, #42555, .T. ) ;
#37589 = VERTEX_POINT ( 'NONE', #19433 ) ;
#37590 = CARTESIAN_POINT ( 'NONE',  ( 2.269879328256733775, -6.544400685875852552, 3.949706986712179013 ) ) ;
#37592 = AXIS2_PLACEMENT_3D ( 'NONE', #46106, #54772, #40097 ) ;
#37591 = CARTESIAN_POINT ( 'NONE',  ( 2.781367136452546962, -6.608147481822088665, 4.171010984503177532 ) ) ;
#37593 = CARTESIAN_POINT ( 'NONE',  ( 35.00000000000000000, 2.021542716731571154, 12.01765980939839196 ) ) ;
#37594 = CARTESIAN_POINT ( 'NONE',  ( -37.00000000000000711, 4.309077947445652867, 10.92721691015457708 ) ) ;
#37595 = CARTESIAN_POINT ( 'NONE',  ( 0.9232058338315058954, -9.791640253608095534, -7.723624854284817154 ) ) ;
#37596 = ORIENTED_EDGE ( 'NONE', *, *, #5870, .F. ) ;
#37597 = AXIS2_PLACEMENT_3D ( 'NONE', #4266, #4609, #44815 ) ;
#37598 = EDGE_CURVE ( 'NONE', #49577, #61311, #49686, .T. ) ;
#37599 = VERTEX_POINT ( 'NONE', #122 ) ;
#37600 = ORIENTED_EDGE ( 'NONE', *, *, #57727, .F. ) ;
#37601 = DIRECTION ( 'NONE',  ( -1.000000000000000000, 0.000000000000000000, 0.000000000000000000 ) ) ;
#37602 = CIRCLE ( 'NONE', #38645, 2.899999999999993694 ) ;
#37603 = CARTESIAN_POINT ( 'NONE',  ( -27.16196273015727058, 13.32896842526023207, -2.143521441892688895 ) ) ;
#37604 = ORIENTED_EDGE ( 'NONE', *, *, #54266, .F. ) ;
#37605 = FACE_OUTER_BOUND ( 'NONE', #10256, .T. ) ;
#37606 = CARTESIAN_POINT ( 'NONE',  ( 1.719304012339844867, -11.38834240361479644, 5.690355757826019989 ) ) ;
#37607 = ORIENTED_EDGE ( 'NONE', *, *, #6400, .F. ) ;
#37608 = DIRECTION ( 'NONE',  ( -1.000000000000000000, 0.000000000000000000, 0.000000000000000000 ) ) ;
#37609 = VECTOR ( 'NONE', #42658, 1000.000000000000000 ) ;
#37610 = CARTESIAN_POINT ( 'NONE',  ( 36.00000000000000711, 11.73555825188276280, -4.983891302653623789 ) ) ;
#37611 = CARTESIAN_POINT ( 'NONE',  ( 2.255723233589907117, 7.132203433012072935, 2.736592204238131210 ) ) ;
#37612 = ORIENTED_EDGE ( 'NONE', *, *, #54116, .F. ) ;
#37613 = ORIENTED_EDGE ( 'NONE', *, *, #23425, .T. ) ;
#37614 = DIRECTION ( 'NONE',  ( 0.000000000000000000, 0.07632122047555796318, -0.9970832820307045097 ) ) ;
#37615 = EDGE_CURVE ( 'NONE', #43482, #42026, #4131, .T. ) ;
#37616 = VERTEX_POINT ( 'NONE', #19762 ) ;
#37617 = DIRECTION ( 'NONE',  ( -1.000000000000000000, 0.000000000000000000, -0.000000000000000000 ) ) ;
#37618 = DIRECTION ( 'NONE',  ( -0.9582930651793755139, 0.2067888154783164567, 0.1972632429577085844 ) ) ;
#37619 = EDGE_CURVE ( 'NONE', #34726, #44597, #35007, .T. ) ;
#37620 = CARTESIAN_POINT ( 'NONE',  ( 2.350038591456828474, -3.024612895786653599, -10.18214835920313455 ) ) ;
#37621 = DIRECTION ( 'NONE',  ( 0.000000000000000000, -0.6269146997508042718, -0.7790879021242460567 ) ) ;
#37622 = AXIS2_PLACEMENT_3D ( 'NONE', #34275, #19324, #39917 ) ;
#37623 = DIRECTION ( 'NONE',  ( 0.000000000000000000, -0.1118654143051685257, -0.9937233664769752339 ) ) ;
#37624 = CARTESIAN_POINT ( 'NONE',  ( 24.97632970311352452, -10.66122974065905282, -8.283959357202887119 ) ) ;
#37625 = CARTESIAN_POINT ( 'NONE',  ( 35.00000000000000000, -6.891188680298889757, -9.512294188640879611 ) ) ;
#37626 = CARTESIAN_POINT ( 'NONE',  ( 37.00000000000000711, -0.7214809346829402781, -11.72397916322012179 ) ) ;
#37628 = EDGE_LOOP ( 'NONE', ( #49974, #50961, #64991, #47958 ) ) ;
#37627 = B_SPLINE_CURVE_WITH_KNOTS ( 'NONE', 3,
 ( #16960, #12954, #53547, #52564, #12608, #32887, #53198, #48549, #41902, #62188, #16640, #63808, #9254, #9573, #19593, #49532, #49215, #3329, #29537, #8953, #44843, #3970, #29236, #3000, #34207, #24234 ),
 .UNSPECIFIED., .F., .F.,
 ( 4, 2, 2, 2, 2, 2, 2, 2, 2, 2, 2, 2, 4 ),
 ( 0.02207550202482942009, 0.02483637361899842730, 0.02621680941608292917, 0.02759724521316743451, 0.03035811680733644519, 0.03173855260442095400, 0.03311898840150546280, 0.03587985999567448736, 0.03864073158984350498, 0.04002116738692802073, 0.04140160318401252953, 0.04278203898109704528, 0.04416247477818155409 ),
 .UNSPECIFIED. ) ;
#37629 = FACE_OUTER_BOUND ( 'NONE', #48915, .T. ) ;
#37630 = ORIENTED_EDGE ( 'NONE', *, *, #64014, .T. ) ;
#37631 = CARTESIAN_POINT ( 'NONE',  ( 5.536195898058073439, 0.007230647766619090894, 0.004468797463753810574 ) ) ;
#37632 = CARTESIAN_POINT ( 'NONE',  ( 1.000000000000000888, -7.414200355365264450, 1.131208685655129775 ) ) ;
#37633 = AXIS2_PLACEMENT_3D ( 'NONE', #26075, #16077, #65312 ) ;
#37634 = ORIENTED_EDGE ( 'NONE', *, *, #40315, .T. ) ;
#37635 = DIRECTION ( 'NONE',  ( 0.000000000000000000, 0.01356324068817998593, -0.9999080150203990547 ) ) ;
#37636 = CARTESIAN_POINT ( 'NONE',  ( 0.3109076770648994126, 6.333869442011780926, 10.49874397806408410 ) ) ;
#37637 = CARTESIAN_POINT ( 'NONE',  ( 0.2653519789438769649, -9.395292406847872257, -7.854827495960904571 ) ) ;
#37638 = EDGE_CURVE ( 'NONE', #64575, #43456, #60976, .T. ) ;
#37639 = VERTEX_POINT ( 'NONE', #45666 ) ;
#37640 = ORIENTED_EDGE ( 'NONE', *, *, #42221, .F. ) ;
#37641 = DIRECTION ( 'NONE',  ( -1.000000000000000000, -0.000000000000000000, 0.000000000000000000 ) ) ;
#37642 = EDGE_CURVE ( 'NONE', #4063, #50233, #24637, .T. ) ;
#37643 = ORIENTED_EDGE ( 'NONE', *, *, #45621, .F. ) ;
#37644 = CYLINDRICAL_SURFACE ( 'NONE', #30743, 5.000000000000000888 ) ;
#37645 = DIRECTION ( 'NONE',  ( 0.000000000000000000, -0.01356324068817998940, 0.9999080150203990547 ) ) ;
#37646 = EDGE_CURVE ( 'NONE', #17686, #8949, #26766, .T. ) ;
#37647 = DIRECTION ( 'NONE',  ( 1.000000000000000000, 0.000000000000000000, 0.000000000000000000 ) ) ;
#37648 = CARTESIAN_POINT ( 'NONE',  ( -17.81810384895137389, -6.313241100106963266, 10.20918272949938554 ) ) ;
#37649 = VERTEX_POINT ( 'NONE', #55318 ) ;
#37650 = CARTESIAN_POINT ( 'NONE',  ( 0.3665391374699464300, 12.04754782681757241, 2.392238720110500427 ) ) ;
#37651 = CIRCLE ( 'NONE', #11124, 5.000000000000000888 ) ;
#37652 = EDGE_CURVE ( 'NONE', #19174, #54245, #44666, .T. ) ;
#37653 = CARTESIAN_POINT ( 'NONE',  ( -35.04709527796842394, 0.01232256164996302361, 0.001003525937966209813 ) ) ;
#37654 = DIRECTION ( 'NONE',  ( 1.000000000000000000, 0.000000000000000000, -0.000000000000000000 ) ) ;
#37655 = DIRECTION ( 'NONE',  ( 1.000000000000000000, -0.000000000000000000, -0.000000000000000000 ) ) ;
#37656 = CARTESIAN_POINT ( 'NONE',  ( -27.08416813689868263, -0.7899859999124457799, 2.150738950797705940 ) ) ;
#37657 = DIRECTION ( 'NONE',  ( 0.4622435816439406930, 0.000000000000000000, -0.8867529933577791290 ) ) ;
#37658 = CARTESIAN_POINT ( 'NONE',  ( -35.00000000000000000, 0.000000000000000000, 0.000000000000000000 ) ) ;
#37659 = CARTESIAN_POINT ( 'NONE',  ( -22.29978294495153435, -2.710748743830170060, -2.590262069787990562 ) ) ;
#37660 = AXIS2_PLACEMENT_3D ( 'NONE', #7444, #37721, #51488 ) ;
#37661 = VERTEX_POINT ( 'NONE', #9110 ) ;
#37662 = CARTESIAN_POINT ( 'NONE',  ( 2.247206125382828379, -0.1157489416152055195, 7.635476611656038415 ) ) ;
#37663 = CARTESIAN_POINT ( 'NONE',  ( 0.3401186441510248848, -12.26845925752607158, -0.2556125181571129446 ) ) ;
#37664 = EDGE_CURVE ( 'NONE', #14001, #44564, #13992, .T. ) ;
#37665 =( BOUNDED_SURFACE ( )  B_SPLINE_SURFACE ( 3, 1, ( 
 ( #54867, #9289 ),
 ( #44227, #29575 ),
 ( #49882, #4333 ),
 ( #25251, #35558 ) ),
 .UNSPECIFIED., .F., .F., .F. ) 
 B_SPLINE_SURFACE_WITH_KNOTS ( ( 4, 4 ),
 ( 2, 2 ),
 ( 0.000000000000000000, 1.000000000000000000 ),
 ( 0.000000000000000000, 1.000000000000000000 ),
 .UNSPECIFIED. ) 
 GEOMETRIC_REPRESENTATION_ITEM ( )  RATIONAL_B_SPLINE_SURFACE ( (
 ( 1.000000000000000000, 1.000000000000000000),
 ( 0.9856612449720755231, 0.9999558406602322425),
 ( 0.9856612449720755231, 0.9999558406602322425),
 ( 1.000000000000000000, 1.000000000000000000) ) ) 
 REPRESENTATION_ITEM ( '' )  SURFACE ( )  );
#37666 = ORIENTED_EDGE ( 'NONE', *, *, #63620, .F. ) ;
#37667 = CARTESIAN_POINT ( 'NONE',  ( -22.28236030719477512, 3.683993210674375351, -0.3108070568283785584 ) ) ;
#37668 = LINE ( 'NONE', #57965, #30035 ) ;
#37669 = ORIENTED_EDGE ( 'NONE', *, *, #56243, .F. ) ;
#37670 = B_SPLINE_CURVE_WITH_KNOTS ( 'NONE', 3,
 ( #48768, #13186, #4187, #54419, #28157, #64677 ),
 .UNSPECIFIED., .F., .F.,
 ( 4, 2, 4 ),
 ( 0.0001654224980408386077, 0.0006219428995476521897, 0.001078463301054465853 ),
 .UNSPECIFIED. ) ;
#37671 = UNCERTAINTY_MEASURE_WITH_UNIT (LENGTH_MEASURE( 1.000000000000000082E-05 ), #18881, 'distance_accuracy_value', 'NONE');
#37672 = CARTESIAN_POINT ( 'NONE',  ( 2.305787727787084407, 6.545285700970527643, 3.971363876083986888 ) ) ;
#37673 = ORIENTED_EDGE ( 'NONE', *, *, #38061, .F. ) ;
#37674 = AXIS2_PLACEMENT_3D ( 'NONE', #36862, #26892, #9358 ) ;
#37675 = CARTESIAN_POINT ( 'NONE',  ( 0.2647959493198558945, -5.995292100780861944, 10.67808515296908922 ) ) ;
#37676 = ORIENTED_EDGE ( 'NONE', *, *, #39070, .F. ) ;
#37677 = VERTEX_POINT ( 'NONE', #10099 ) ;
#37678 = CARTESIAN_POINT ( 'NONE',  ( 0.2956976708475479443, -12.02996380804952459, -2.344604179391541088 ) ) ;
#37679 = ORIENTED_EDGE ( 'NONE', *, *, #63637, .F. ) ;
#37680 = CARTESIAN_POINT ( 'NONE',  ( 25.00000000000000355, -9.999999999999998224, 5.000000000000000888 ) ) ;
#37681 = DIRECTION ( 'NONE',  ( 0.3939253465568944290, 0.9190910618577644575, 0.009718094113442748289 ) ) ;
#37682 = FACE_OUTER_BOUND ( 'NONE', #5838, .T. ) ;
#37683 = DIRECTION ( 'NONE',  ( 0.000000000000000000, 0.01356324068817991828, -0.9999080150203990547 ) ) ;
#37684 = VERTEX_POINT ( 'NONE', #65295 ) ;
#37685 = AXIS2_PLACEMENT_3D ( 'NONE', #17774, #46714, #1828 ) ;
#37686 = DIRECTION ( 'NONE',  ( -1.000000000000000000, 0.000000000000000000, 0.000000000000000000 ) ) ;
#37687 = CARTESIAN_POINT ( 'NONE',  ( -5.261125060311115931, -26.02247534669140094, 15.21511059005040423 ) ) ;
#37688 = CARTESIAN_POINT ( 'NONE',  ( 2.000000000000001776, -6.539067737394505642, 2.314222412769772586 ) ) ;
#37690 = EDGE_LOOP ( 'NONE', ( #18819, #18285, #13298, #10526 ) ) ;
#37689 = CARTESIAN_POINT ( 'NONE',  ( 36.00000000000000711, -5.556331110570486231, -11.47561260193575272 ) ) ;
#37691 = CARTESIAN_POINT ( 'NONE',  ( -35.00000000000000000, 11.38112321385055026, -2.905556151562505462 ) ) ;
#37692 = EDGE_CURVE ( 'NONE', #59870, #8677, #24744, .T. ) ;
#37693 = ORIENTED_EDGE ( 'NONE', *, *, #64943, .T. ) ;
#37694 = AXIS2_PLACEMENT_3D ( 'NONE', #49897, #54882, #19955 ) ;
#37695 = CARTESIAN_POINT ( 'NONE',  ( 0.2655924914740778742, 6.161287456391684181, 10.58356227062111543 ) ) ;
#37696 = ORIENTED_EDGE ( 'NONE', *, *, #38318, .F. ) ;
#37697 = CARTESIAN_POINT ( 'NONE',  ( -35.00000000000000000, 10.93004082984018410, 6.564808257521808521 ) ) ;
#37698 = CARTESIAN_POINT ( 'NONE',  ( -37.00000000000000711, -12.74068829017553561, -0.4871980014162809458 ) ) ;
#37699 = EDGE_CURVE ( 'NONE', #7316, #7009, #17182, .T. ) ;
#37700 = AXIS2_PLACEMENT_3D ( 'NONE', #33356, #8745, #3782 ) ;
#37701 = CARTESIAN_POINT ( 'NONE',  ( 2.241352910868908310, -7.633946224498473043, -0.08337961031712197435 ) ) ;
#37702 = ORIENTED_EDGE ( 'NONE', *, *, #7609, .F. ) ;
#37703 = DIRECTION ( 'NONE',  ( -1.000000000000000000, -0.000000000000000000, 0.000000000000000000 ) ) ;
#37704 = CARTESIAN_POINT ( 'NONE',  ( -22.27384469013076185, -2.581192766446256837, -2.625926801827886070 ) ) ;
#37705 = CARTESIAN_POINT ( 'NONE',  ( 12.37428322565249417, 10.69553198490500989, -8.245447885329925342 ) ) ;
#37706 = EDGE_LOOP ( 'NONE', ( #8391, #38457, #57306, #36932 ) ) ;
#37707 = ORIENTED_EDGE ( 'NONE', *, *, #39255, .F. ) ;
#37708 = LINE ( 'NONE', #1153, #23187 ) ;
#37709 = ORIENTED_EDGE ( 'NONE', *, *, #24387, .F. ) ;
#37710 = EDGE_LOOP ( 'NONE', ( #52827, #64193, #62450, #16215 ) ) ;
#37711 = DIRECTION ( 'NONE',  ( 0.000000000000000000, 0.01356324068817991828, -0.9999080150203990547 ) ) ;
#37712 = CARTESIAN_POINT ( 'NONE',  ( -17.95869421093891916, -11.89647782150295541, 1.606523818316730301 ) ) ;
#37713 = DIRECTION ( 'NONE',  ( -1.000000000000000000, 0.000000000000000000, 0.000000000000000000 ) ) ;
#37714 = DIRECTION ( 'NONE',  ( 0.000000000000000000, -0.01356324068817998940, 0.9999080150203990547 ) ) ;
#37715 = CARTESIAN_POINT ( 'NONE',  ( -36.00000000000000711, -12.26766708251994409, 3.473736367725209551 ) ) ;
#37716 = EDGE_CURVE ( 'NONE', #3284, #52011, #60306, .T. ) ;
#37717 = CARTESIAN_POINT ( 'NONE',  ( -1.734723475976807094E-15, -3.469446951953614189E-15, 25.00000000000000000 ) ) ;
#37718 = CIRCLE ( 'NONE', #13275, 5.000000000000001776 ) ;
#37719 = CARTESIAN_POINT ( 'NONE',  ( 37.00000000000000711, 4.237620530777969741, 11.42599468261424356 ) ) ;
#37720 = ORIENTED_EDGE ( 'NONE', *, *, #33995, .F. ) ;
#37721 = DIRECTION ( 'NONE',  ( 1.000000000000000000, 0.000000000000000000, 0.000000000000000000 ) ) ;
#37722 = DIRECTION ( 'NONE',  ( 1.000000000000000000, -0.000000000000000000, 0.000000000000000000 ) ) ;
#37723 = AXIS2_PLACEMENT_3D ( 'NONE', #62064, #5903, #65705 ) ;
#37724 = ADVANCED_FACE ( 'NONE', ( #54688 ), #9415, .T. ) ;
#37725 = CARTESIAN_POINT ( 'NONE',  ( 2.288423627607481414, -4.792733268640415822, 5.962686897379188444 ) ) ;
#37726 = CYLINDRICAL_SURFACE ( 'NONE', #56685, 12.74999999999999822 ) ;
#37727 = DIRECTION ( 'NONE',  ( 0.000000000000000000, 0.01356324068817998940, -0.9999080150203989437 ) ) ;
#37728 = CARTESIAN_POINT ( 'NONE',  ( 17.27839441901508621, -12.20388373500082224, 5.771933972472480967 ) ) ;
#37729 = DIRECTION ( 'NONE',  ( 0.000000000000000000, 0.000000000000000000, -1.000000000000000000 ) ) ;
#37730 = ORIENTED_EDGE ( 'NONE', *, *, #10269, .T. ) ;
#37731 = DIRECTION ( 'NONE',  ( 0.000000000000000000, 0.01356324068817998940, -0.9999080150203990547 ) ) ;
#37732 = CARTESIAN_POINT ( 'NONE',  ( 0.3675815128205894289, -1.872154644482002528, -12.13672785388552100 ) ) ;
#37733 = CARTESIAN_POINT ( 'NONE',  ( -35.04582288351658548, 0.004274985098064986062, 0.01196488372920834035 ) ) ;
#37734 = CARTESIAN_POINT ( 'NONE',  ( -17.61481692485065054, -13.12896122980146529, 3.215558237703250111 ) ) ;
#37735 = CIRCLE ( 'NONE', #21853, 6.936499999999993449 ) ;
#37736 = LINE ( 'NONE', #24084, #36250 ) ;
#37737 = FACE_OUTER_BOUND ( 'NONE', #60904, .T. ) ;
#37738 = ADVANCED_FACE ( 'NONE', ( #4805 ), #25072, .T. ) ;
#37739 = ORIENTED_EDGE ( 'NONE', *, *, #20716, .F. ) ;
#37740 = CARTESIAN_POINT ( 'NONE',  ( 18.23350676702760609, -7.210796396001341257, 9.602820039526596574 ) ) ;
#37741 = DIRECTION ( 'NONE',  ( -1.000000000000000000, 0.000000000000000000, 0.000000000000000000 ) ) ;
#37742 = CARTESIAN_POINT ( 'NONE',  ( -35.00000000000000000, -6.307491713049102167, 9.908974237959624176 ) ) ;
#37743 = CARTESIAN_POINT ( 'NONE',  ( -35.05175862995318425, 0.008949502803489231550, 0.008837625261040246705 ) ) ;
#37744 = VERTEX_POINT ( 'NONE', #40337 ) ;
#37745 = EDGE_CURVE ( 'NONE', #16416, #65638, #39475, .T. ) ;
#37746 = DIRECTION ( 'NONE',  ( 1.000000000000000000, -0.000000000000000000, -0.000000000000000000 ) ) ;
#37747 = DIRECTION ( 'NONE',  ( 1.000000000000000000, 0.000000000000000000, 0.000000000000000000 ) ) ;
#37748 = ORIENTED_EDGE ( 'NONE', *, *, #4837, .T. ) ;
#37749 = VERTEX_POINT ( 'NONE', #21041 ) ;
#37750 = CYLINDRICAL_SURFACE ( 'NONE', #15071, 6.936499999999988120 ) ;
#37751 = AXIS2_PLACEMENT_3D ( 'NONE', #44492, #14875, #64770 ) ;
#37752 = ADVANCED_FACE ( 'NONE', ( #46012 ), #20959, .F. ) ;
#37753 = CARTESIAN_POINT ( 'NONE',  ( 0.2767916011545379917, -4.367596755337373793, -11.44495079483528777 ) ) ;
#37754 = ORIENTED_EDGE ( 'NONE', *, *, #45956, .T. ) ;
#37755 = CARTESIAN_POINT ( 'NONE',  ( 0.3160775863651076878, -9.546663463486092738, 7.697077652699416461 ) ) ;
#37756 = CARTESIAN_POINT ( 'NONE',  ( 0.000000000000000000, 3.786546189469266466, -5.663561025469129540 ) ) ;
#37757 = CARTESIAN_POINT ( 'NONE',  ( 2.241449424704145876, 7.507583637787367259, -1.386092121067129757 ) ) ;
#37758 = CYLINDRICAL_SURFACE ( 'NONE', #43598, 7.499999999999988454 ) ;
#37759 = DIRECTION ( 'NONE',  ( -1.000000000000000000, 0.000000000000000000, 0.000000000000000000 ) ) ;
#37760 = CARTESIAN_POINT ( 'NONE',  ( 0.2648321136542699517, 5.999882851577475584, 10.67551415837652051 ) ) ;
#37762 = EDGE_LOOP ( 'NONE', ( #5068, #38550, #28532, #21877 ) ) ;
#37761 = DIRECTION ( 'NONE',  ( -0.9582930651793755139, -0.2777159889015697880, -0.06744057189511687422 ) ) ;
#37763 = CARTESIAN_POINT ( 'NONE',  ( 1.549075743846799025, 4.962709020481401723, -11.66216484053774138 ) ) ;
#37764 = EDGE_CURVE ( 'NONE', #13349, #48023, #31031, .T. ) ;
#37765 = ORIENTED_EDGE ( 'NONE', *, *, #7322, .F. ) ;
#37766 = LINE ( 'NONE', #1220, #34220 ) ;
#37767 = ORIENTED_EDGE ( 'NONE', *, *, #5941, .F. ) ;
#37768 = ORIENTED_EDGE ( 'NONE', *, *, #708, .F. ) ;
#37769 = PRODUCT_CONTEXT ( 'NONE', #13670, 'mechanical' ) ;
#37770 = CARTESIAN_POINT ( 'NONE',  ( 1.547277799338547588, -11.66196709685588573, 4.961646058323668562 ) ) ;
#37771 = CARTESIAN_POINT ( 'NONE',  ( -19.56743653832047158, -30.00000000000000355, 5.000000000000000888 ) ) ;
#37772 = CARTESIAN_POINT ( 'NONE',  ( -4.045856953771468589, 9.480858417917106706, 7.359659509255599197 ) ) ;
#37773 = CARTESIAN_POINT ( 'NONE',  ( -35.62304844322794395, -2.500997609376294228, -21.53526926371173289 ) ) ;
#37774 = DIRECTION ( 'NONE',  ( -1.000000000000000000, 0.000000000000000000, 0.000000000000000000 ) ) ;
#37775 = ORIENTED_EDGE ( 'NONE', *, *, #31166, .F. ) ;
#37776 = VECTOR ( 'NONE', #51810, 999.9999999999998863 ) ;
#37777 = CARTESIAN_POINT ( 'NONE',  ( -22.27719412087655471, -0.5341638063191807007, -3.642699606241637245 ) ) ;
#37778 = CARTESIAN_POINT ( 'NONE',  ( 3.924671233276515458, 7.659762911315605827, -11.15143203671860306 ) ) ;
#37780 = ORIENTED_EDGE ( 'NONE', *, *, #40752, .T. ) ;
#37779 = CARTESIAN_POINT ( 'NONE',  ( 0.2657645697724709821, 11.55867655367626945, -4.045961170622892844 ) ) ;
#37781 = VERTEX_POINT ( 'NONE', #10743 ) ;
#37782 = CARTESIAN_POINT ( 'NONE',  ( 1.937114397841932290, -5.226660192101668656, 11.72279974487461907 ) ) ;
#37783 = VERTEX_POINT ( 'NONE', #41006 ) ;
#37784 = CARTESIAN_POINT ( 'NONE',  ( 2.241506898688417238, 1.286963596520092956, -7.525229609709728429 ) ) ;
#37785 = CARTESIAN_POINT ( 'NONE',  ( 5.514970785353741078, 0.003805873180274313254, -0.002796696073589883310 ) ) ;
#37786 = DIRECTION ( 'NONE',  ( 1.000000000000000000, 0.000000000000000000, 0.000000000000000000 ) ) ;
#37787 = AXIS2_PLACEMENT_3D ( 'NONE', #52681, #27073, #37361 ) ;
#37788 = CARTESIAN_POINT ( 'NONE',  ( 0.8320506296491576581, 12.30686996250300247, 1.781423711749617889 ) ) ;
#37789 = LINE ( 'NONE', #27470, #63852 ) ;
#37790 = CARTESIAN_POINT ( 'NONE',  ( -27.09048036756592026, -1.905306051559101155, 1.306202114107285039 ) ) ;
#37791 = CARTESIAN_POINT ( 'NONE',  ( 35.00000000000000000, -10.14408668126217350, -5.921969905510321652 ) ) ;
#37792 = ORIENTED_EDGE ( 'NONE', *, *, #12684, .T. ) ;
#37793 = DIRECTION ( 'NONE',  ( -1.000000000000000000, 0.000000000000000000, -0.000000000000000000 ) ) ;
#37794 = EDGE_LOOP ( 'NONE', ( #62611, #41210, #13711, #37861 ) ) ;
#37795 = CARTESIAN_POINT ( 'NONE',  ( 0.2653141334712566524, -6.084912053827412848, 10.62748186152495578 ) ) ;
#37796 = CARTESIAN_POINT ( 'NONE',  ( -8.504635283918430488, -10.07629646921066779, -8.990051544619507951 ) ) ;
#37797 = EDGE_CURVE ( 'NONE', #29943, #28034, #34388, .T. ) ;
#37798 = CARTESIAN_POINT ( 'NONE',  ( -35.00000000000000000, 1.030638227056741574, -12.14284015767849034 ) ) ;
#37799 = CARTESIAN_POINT ( 'NONE',  ( 0.2650492433740059828, -11.54478237753289172, -4.084772052580713186 ) ) ;
#37800 = ORIENTED_EDGE ( 'NONE', *, *, #11573, .F. ) ;
#37801 = ADVANCED_FACE ( 'NONE', ( #41660 ), #31998, .T. ) ;
#37802 = ORIENTED_EDGE ( 'NONE', *, *, #5435, .T. ) ;
#37803 = CARTESIAN_POINT ( 'NONE',  ( -27.09483304420799143, 0.1669215111592837197, 2.317106154747420987 ) ) ;
#37804 = ORIENTED_EDGE ( 'NONE', *, *, #33814, .F. ) ;
#37805 = DIRECTION ( 'NONE',  ( -1.000000000000000000, 0.000000000000000000, 0.000000000000000000 ) ) ;
#37806 = CARTESIAN_POINT ( 'NONE',  ( 9.176090415275556467, 6.974186229596638142, 9.772926367110217782 ) ) ;
#37807 = DIRECTION ( 'NONE',  ( 1.000000000000000000, 0.000000000000000000, 0.000000000000000000 ) ) ;
#37808 = CARTESIAN_POINT ( 'NONE',  ( -37.00000000000000711, 10.59380114696480391, -7.094637218249240540 ) ) ;
#37809 = ORIENTED_EDGE ( 'NONE', *, *, #29193, .F. ) ;
#37810 = CARTESIAN_POINT ( 'NONE',  ( 2.931247277082670966, 2.338794445044995118, 7.508560300462408854 ) ) ;
#37811 = CARTESIAN_POINT ( 'NONE',  ( 18.03946127237285069, 10.01571122672373093, 9.058849096994427086 ) ) ;
#37812 = CARTESIAN_POINT ( 'NONE',  ( 0.2653141617321010948, -10.58343467791291737, -6.161204121352803931 ) ) ;
#37813 = DIRECTION ( 'NONE',  ( 1.000000000000000000, 0.000000000000000000, 0.000000000000000000 ) ) ;
#37814 = EDGE_CURVE ( 'NONE', #61800, #59191, #46948, .T. ) ;
#37815 = AXIS2_PLACEMENT_3D ( 'NONE', #34263, #38605, #43247 ) ;
#37816 = CARTESIAN_POINT ( 'NONE',  ( 0.3106921474978460718, 6.333448016104198608, -10.49891314301079071 ) ) ;
#37817 = DIRECTION ( 'NONE',  ( -1.000000000000000000, 0.000000000000000000, -0.000000000000000000 ) ) ;
#37818 = AXIS2_PLACEMENT_3D ( 'NONE', #43359, #28733, #39036 ) ;
#37819 = EDGE_CURVE ( 'NONE', #44068, #40994, #37339, .T. ) ;
#37820 = ORIENTED_EDGE ( 'NONE', *, *, #57741, .T. ) ;
#37821 = EDGE_CURVE ( 'NONE', #37661, #33997, #11087, .T. ) ;
#37822 = CARTESIAN_POINT ( 'NONE',  ( -27.08423805673873019, 1.665498649074246496, -1.573803011992711109 ) ) ;
#37823 = DIRECTION ( 'NONE',  ( 0.000000000000000000, 0.8515178078024849828, -0.5243256840888592674 ) ) ;
#37824 = FACE_OUTER_BOUND ( 'NONE', #52574, .T. ) ;
#37825 = ORIENTED_EDGE ( 'NONE', *, *, #54188, .T. ) ;
#37826 = EDGE_CURVE ( 'NONE', #4245, #32821, #51180, .T. ) ;
#37827 = CARTESIAN_POINT ( 'NONE',  ( 1.000000000000000888, -0.7281529553922420073, 7.464569195442772198 ) ) ;
#37828 = CARTESIAN_POINT ( 'NONE',  ( 1.020182472822681374, -8.370187102469690998, 9.280950437305071077 ) ) ;
#37829 = DIRECTION ( 'NONE',  ( 0.000000000000000000, -0.9551603052523510717, 0.2960891610144412156 ) ) ;
#37830 = DIRECTION ( 'NONE',  ( 0.000000000000000000, -0.9937233664769749009, 0.1118654143051720229 ) ) ;
#37831 = CARTESIAN_POINT ( 'NONE',  ( 37.00000000000000711, -2.544412758415763420, 11.91791701451268537 ) ) ;
#37832 = ORIENTED_EDGE ( 'NONE', *, *, #32560, .F. ) ;
#37834 = ORIENTED_EDGE ( 'NONE', *, *, #18112, .T. ) ;
#37833 = ADVANCED_FACE ( 'NONE', ( #41983 ), #62264, .T. ) ;
#37835 = DIRECTION ( 'NONE',  ( -1.000000000000000000, -0.000000000000000000, -0.000000000000000000 ) ) ;
#37836 = VERTEX_POINT ( 'NONE', #47329 ) ;
#37837 = DIRECTION ( 'NONE',  ( -0.000000000000000000, -0.000000000000000000, -1.000000000000000000 ) ) ;
#37838 = DIRECTION ( 'NONE',  ( 0.000000000000000000, 0.000000000000000000, 1.000000000000000000 ) ) ;
#37839 = FACE_OUTER_BOUND ( 'NONE', #1232, .T. ) ;
#37840 = FACE_OUTER_BOUND ( 'NONE', #23031, .T. ) ;
#37841 = CARTESIAN_POINT ( 'NONE',  ( 3.031336079627524605, 7.886784934834240701, -0.4165536638483573473 ) ) ;
#37842 = EDGE_CURVE ( 'NONE', #4753, #807, #52646, .T. ) ;
#37843 = CARTESIAN_POINT ( 'NONE',  ( 2.242418902651940549, -1.227462051872194815, 7.535443599794969138 ) ) ;
#37844 = DIRECTION ( 'NONE',  ( 0.000000000000000000, 0.7196168960969817618, 0.6943713148249616163 ) ) ;
#37845 = ORIENTED_EDGE ( 'NONE', *, *, #55196, .T. ) ;
#37846 = ORIENTED_EDGE ( 'NONE', *, *, #6747, .F. ) ;
#37847 = CARTESIAN_POINT ( 'NONE',  ( 1.633930747251779225, -5.718685543473577049, 11.34237452761324505 ) ) ;
#37848 = VERTEX_POINT ( 'NONE', #57636 ) ;
#37849 = CARTESIAN_POINT ( 'NONE',  ( -22.30861784526115699, 2.600591904828422507, -2.737516124790391636 ) ) ;
#37850 = CARTESIAN_POINT ( 'NONE',  ( 0.7446945582532709107, 8.243982823409844229, -9.270687147117392612 ) ) ;
#37851 = EDGE_CURVE ( 'NONE', #61730, #57422, #64957, .T. ) ;
#37852 = DIRECTION ( 'NONE',  ( -1.000000000000000000, 0.000000000000000000, 0.000000000000000000 ) ) ;
#37853 = ORIENTED_EDGE ( 'NONE', *, *, #14457, .T. ) ;
#37854 = FACE_OUTER_BOUND ( 'NONE', #35884, .T. ) ;
#37855 = LINE ( 'NONE', #21242, #46683 ) ;
#37856 = CARTESIAN_POINT ( 'NONE',  ( -35.04660725145885891, 0.008800808525126678494, -0.008590646501141869715 ) ) ;
#37857 = VERTEX_POINT ( 'NONE', #12371 ) ;
#37858 = ORIENTED_EDGE ( 'NONE', *, *, #37964, .T. ) ;
#37859 = DIRECTION ( 'NONE',  ( 0.000000000000000000, 0.000000000000000000, 1.000000000000000000 ) ) ;
#37860 = ORIENTED_EDGE ( 'NONE', *, *, #39939, .F. ) ;
#37861 = ORIENTED_EDGE ( 'NONE', *, *, #17689, .T. ) ;
#37862 = DIRECTION ( 'NONE',  ( 0.000000000000000000, -0.7196168960969719919, -0.6943713148249717193 ) ) ;
#37863 = ORIENTED_EDGE ( 'NONE', *, *, #59559, .T. ) ;
#37864 = AXIS2_PLACEMENT_3D ( 'NONE', #12616, #2697, #13603 ) ;
#37865 = VERTEX_POINT ( 'NONE', #32978 ) ;
#37866 = CARTESIAN_POINT ( 'NONE',  ( -22.27719443589224113, -2.737335337013107051, 2.462030382548431984 ) ) ;
#37867 = DIRECTION ( 'NONE',  ( 0.000000000000000000, -0.7617968321374811724, -0.6478160128812026075 ) ) ;
#37868 = DIRECTION ( 'NONE',  ( 0.000000000000000000, 0.000000000000000000, -1.000000000000000000 ) ) ;
#37869 = FACE_OUTER_BOUND ( 'NONE', #23456, .T. ) ;
#37870 = CYLINDRICAL_SURFACE ( 'NONE', #12522, 5.000000000000000888 ) ;
#37871 = AXIS2_PLACEMENT_3D ( 'NONE', #43059, #63338, #13141 ) ;
#37872 = DIRECTION ( 'NONE',  ( -1.000000000000000000, 0.000000000000000000, 0.000000000000000000 ) ) ;
#37873 = ORIENTED_EDGE ( 'NONE', *, *, #59615, .F. ) ;
#37874 =( BOUNDED_SURFACE ( )  B_SPLINE_SURFACE ( 3, 1, ( 
 ( #36535, #50836 ),
 ( #26218, #30533 ),
 ( #16574, #11566 ),
 ( #25554, #45846 ) ),
 .UNSPECIFIED., .F., .F., .F. ) 
 B_SPLINE_SURFACE_WITH_KNOTS ( ( 4, 4 ),
 ( 2, 2 ),
 ( 0.000000000000000000, 1.000000000000000000 ),
 ( 0.000000000000000000, 1.000000000000000000 ),
 .UNSPECIFIED. ) 
 GEOMETRIC_REPRESENTATION_ITEM ( )  RATIONAL_B_SPLINE_SURFACE ( (
 ( 1.000000000000000000, 1.000000000000000000),
 ( 0.9932032654565553509, 0.8386279382598740284),
 ( 0.9932032654565553509, 0.8386279382598740284),
 ( 1.000000000000000000, 1.000000000000000000) ) ) 
 REPRESENTATION_ITEM ( '' )  SURFACE ( )  );
#37875 = FACE_OUTER_BOUND ( 'NONE', #36928, .T. ) ;
#37876 = CARTESIAN_POINT ( 'NONE',  ( 2.000000000000001776, -6.883677378339461583, 0.8544109087185534079 ) ) ;
#37877 = CARTESIAN_POINT ( 'NONE',  ( -35.00000000000000000, 1.791059740004591561, -12.05416472667163674 ) ) ;
#37878 = CARTESIAN_POINT ( 'NONE',  ( 47.00000000000000711, 4.705694406421931860E-17, -3.469127814946512892E-15 ) ) ;
#37879 = DIRECTION ( 'NONE',  ( 1.000000000000000000, 0.000000000000000000, 0.000000000000000000 ) ) ;
#37880 = CARTESIAN_POINT ( 'NONE',  ( 2.305787727787084407, -3.971363876083918498, -6.545285700970570275 ) ) ;
#37881 = CARTESIAN_POINT ( 'NONE',  ( 0.3006302518452078631, -11.59403866275563821, -3.979421585299229402 ) ) ;
#37882 = DIRECTION ( 'NONE',  ( -0.000000000000000000, -1.000000000000000000, -0.000000000000000000 ) ) ;
#37883 = EDGE_CURVE ( 'NONE', #14515, #22753, #38970, .T. ) ;
#37884 = ORIENTED_EDGE ( 'NONE', *, *, #29284, .T. ) ;
#37885 = DIRECTION ( 'NONE',  ( -1.000000000000000000, -0.000000000000000000, -0.000000000000000000 ) ) ;
#37886 = EDGE_LOOP ( 'NONE', ( #65761, #41412, #65511, #15847 ) ) ;
#37887 = CARTESIAN_POINT ( 'NONE',  ( 0.3223008802179254118, 10.74209118105756744, 5.919638939520617704 ) ) ;
#37888 = DIRECTION ( 'NONE',  ( -1.000000000000000000, 0.000000000000000000, 0.000000000000000000 ) ) ;
#37889 = CARTESIAN_POINT ( 'NONE',  ( 0.2851083653049530375, -0.4107471485392680810, -13.49374991542258151 ) ) ;
#37890 = CARTESIAN_POINT ( 'NONE',  ( 1.719304012341583476, 7.581471372739232883, -10.22720798541541498 ) ) ;
#37891 = CARTESIAN_POINT ( 'NONE',  ( 2.430348790456736019, 7.611893186157221436, 1.144258029164500368 ) ) ;
#37892 = ORIENTED_EDGE ( 'NONE', *, *, #63979, .T. ) ;
#37893 = DIRECTION ( 'NONE',  ( 1.000000000000000000, -0.000000000000000000, -0.000000000000000000 ) ) ;
#37894 = DIRECTION ( 'NONE',  ( 1.000000000000000000, 0.000000000000000000, 0.000000000000000000 ) ) ;
#37895 = CARTESIAN_POINT ( 'NONE',  ( -28.85619398320021745, 3.750539801530000439, 25.00000000000000000 ) ) ;
#37896 = CARTESIAN_POINT ( 'NONE',  ( -4.049878455451396242, 11.39499819594600183, 7.250431408498958952 ) ) ;
#37897 = EDGE_CURVE ( 'NONE', #52157, #27171, #55435, .T. ) ;
#37898 = ORIENTED_EDGE ( 'NONE', *, *, #39980, .F. ) ;
#37899 = EDGE_CURVE ( 'NONE', #39860, #8191, #23696, .T. ) ;
#37900 = CARTESIAN_POINT ( 'NONE',  ( 25.00000000000000711, -3.797884998337192286, -24.00000000000000000 ) ) ;
#37901 = EDGE_CURVE ( 'NONE', #3390, #38662, #16129, .T. ) ;
#37902 = CARTESIAN_POINT ( 'NONE',  ( 2.260457164927185847, -3.939659644572505393, -6.546788723198600835 ) ) ;
#37903 = CIRCLE ( 'NONE', #28325, 4.999999999999999112 ) ;
#37904 = AXIS2_PLACEMENT_3D ( 'NONE', #42912, #23292, #53887 ) ;
#37905 = ORIENTED_EDGE ( 'NONE', *, *, #21227, .T. ) ;
#37906 = CARTESIAN_POINT ( 'NONE',  ( -9.615673917211060129, 12.77468887473842685, -4.382797285550743105 ) ) ;
#37907 = ORIENTED_EDGE ( 'NONE', *, *, #31359, .T. ) ;
#37908 = CARTESIAN_POINT ( 'NONE',  ( 2.244591118396559448, -6.558116599718194273, 3.910457279126699159 ) ) ;
#37909 = LINE ( 'NONE', #32902, #4582 ) ;
#37910 = DIRECTION ( 'NONE',  ( 1.000000000000000000, 0.000000000000000000, -0.000000000000000000 ) ) ;
#37911 = FACE_OUTER_BOUND ( 'NONE', #42008, .T. ) ;
#37912 = EDGE_CURVE ( 'NONE', #31042, #33111, #40754, .T. ) ;
#37913 = CARTESIAN_POINT ( 'NONE',  ( -22.27218376572352554, -2.099017427146257386, -3.026314224080938864 ) ) ;
#37914 = ORIENTED_EDGE ( 'NONE', *, *, #59465, .T. ) ;
#37915 = EDGE_CURVE ( 'NONE', #22476, #50940, #12959, .T. ) ;
#37916 = ORIENTED_EDGE ( 'NONE', *, *, #9327, .T. ) ;
#37917 = ORIENTED_EDGE ( 'NONE', *, *, #49161, .T. ) ;
#37918 = CARTESIAN_POINT ( 'NONE',  ( 2.284126774967663032, 7.240052432235682289, -2.466502196988892059 ) ) ;
#37919 = EDGE_CURVE ( 'NONE', #34795, #58896, #24863, .T. ) ;
#37920 = CARTESIAN_POINT ( 'NONE',  ( 5.514970785353741078, 0.003262412238248228995, -0.003415090918276198536 ) ) ;
#37921 = ORIENTED_EDGE ( 'NONE', *, *, #43712, .F. ) ;
#37922 = CARTESIAN_POINT ( 'NONE',  ( 1.719304012338199517, 0.000000000000000000, 0.000000000000000000 ) ) ;
#37923 = EDGE_CURVE ( 'NONE', #63668, #43107, #4250, .T. ) ;
#37924 = CARTESIAN_POINT ( 'NONE',  ( -35.00000000000000000, -7.971186206369537786, 9.217970097227697224 ) ) ;
#37925 = VERTEX_POINT ( 'NONE', #9040 ) ;
#37926 = CARTESIAN_POINT ( 'NONE',  ( 2.000000000000001776, 6.662861565602072211, 1.421313227905651289 ) ) ;
#37927 = CARTESIAN_POINT ( 'NONE',  ( 2.288423627607478750, -2.767471693622750362, -7.131972212895032470 ) ) ;
#37928 = CARTESIAN_POINT ( 'NONE',  ( -35.00000000000000000, -10.43555801961479190, 5.391785509270926369 ) ) ;
#37929 = ORIENTED_EDGE ( 'NONE', *, *, #21963, .F. ) ;
#37931 = EDGE_CURVE ( 'NONE', #46064, #50432, #32063, .T. ) ;
#37930 = VERTEX_POINT ( 'NONE', #14016 ) ;
#37932 = CARTESIAN_POINT ( 'NONE',  ( 2.259830038564998311, 2.483392345594764183, 7.225713255971552229 ) ) ;
#37933 = ORIENTED_EDGE ( 'NONE', *, *, #4853, .F. ) ;
#37934 =( NAMED_UNIT ( * ) PLANE_ANGLE_UNIT ( ) SI_UNIT ( $, .RADIAN. ) );
#37935 = EDGE_LOOP ( 'NONE', ( #24042, #13387, #37329, #35627 ) ) ;
#37936 = CARTESIAN_POINT ( 'NONE',  ( 2.241352910868908754, 3.744764251556992996, 6.652881166698525028 ) ) ;
#37937 = DIRECTION ( 'NONE',  ( 0.000000000000000000, 0.01356324068817998940, -0.9999080150203989437 ) ) ;
#37938 = CARTESIAN_POINT ( 'NONE',  ( -37.00000000000000711, -4.339012074900030491, 10.91536515067646818 ) ) ;
#37939 = CARTESIAN_POINT ( 'NONE',  ( -22.28856623400852399, 3.603818606161810045, 0.9049353338066237207 ) ) ;
#37940 = CARTESIAN_POINT ( 'NONE',  ( -35.00000000000000000, -6.265926637539413591, -11.10408318471066380 ) ) ;
#37941 = CARTESIAN_POINT ( 'NONE',  ( -37.00000000000000711, 12.16632754454237997, -0.7008968033237440443 ) ) ;
#37942 = CARTESIAN_POINT ( 'NONE',  ( -27.01437459610461644, -8.723448335974111956, -8.240233560378637634 ) ) ;
#37943 = ORIENTED_EDGE ( 'NONE', *, *, #57878, .F. ) ;
#37944 = CARTESIAN_POINT ( 'NONE',  ( -22.51237073810381162, -3.933875531624977828, -2.023441661740719155 ) ) ;
#37945 = VERTEX_POINT ( 'NONE', #64547 ) ;
#37946 = DIRECTION ( 'NONE',  ( -1.000000000000000000, -0.000000000000000000, 0.000000000000000000 ) ) ;
#37947 = FACE_OUTER_BOUND ( 'NONE', #46511, .T. ) ;
#37948 = ORIENTED_EDGE ( 'NONE', *, *, #14814, .T. ) ;
#37949 = CARTESIAN_POINT ( 'NONE',  ( -14.37660149302730694, 8.348016424126690538, 8.621410803000902234 ) ) ;
#37950 = CARTESIAN_POINT ( 'NONE',  ( 0.2872850955227766456, 12.02931961709053255, -2.333231805482862242 ) ) ;
#37951 = CARTESIAN_POINT ( 'NONE',  ( 2.781367136451758260, -7.636197200465718815, 1.659348694504308552 ) ) ;
#37952 = CIRCLE ( 'NONE', #14525, 12.73084802173761787 ) ;
#37953 = VERTEX_POINT ( 'NONE', #59923 ) ;
#37954 = EDGE_CURVE ( 'NONE', #22894, #30390, #41658, .T. ) ;
#37955 = ORIENTED_EDGE ( 'NONE', *, *, #6392, .F. ) ;
#37956 = AXIS2_PLACEMENT_3D ( 'NONE', #22387, #62957, #31396 ) ;
#37957 = CARTESIAN_POINT ( 'NONE',  ( 2.653899356900423001, -6.857477569908684956, -3.657605971842797565 ) ) ;
#37958 = ORIENTED_EDGE ( 'NONE', *, *, #51801, .F. ) ;
#37959 = DIRECTION ( 'NONE',  ( -1.000000000000000000, 0.000000000000000000, 0.000000000000000000 ) ) ;
#37960 = CARTESIAN_POINT ( 'NONE',  ( -27.08419642509983305, 2.181485315953908266, 0.7009209357102503812 ) ) ;
#37961 = CARTESIAN_POINT ( 'NONE',  ( -3.276654955009157710, -12.28508903930122997, 5.608921276358484143 ) ) ;
#37962 = CYLINDRICAL_SURFACE ( 'NONE', #55483, 4.999999999999999112 ) ;
#37963 = ORIENTED_EDGE ( 'NONE', *, *, #8018, .T. ) ;
#37964 = EDGE_CURVE ( 'NONE', #10268, #3168, #50181, .T. ) ;
#37965 = CARTESIAN_POINT ( 'NONE',  ( 35.00000000000000000, 11.26103545359850955, -3.340853584269734000 ) ) ;
#37966 = DIRECTION ( 'NONE',  ( 0.000000000000000000, 0.01356324068817998940, -0.9999080150203990547 ) ) ;
#37967 = FACE_OUTER_BOUND ( 'NONE', #49659, .T. ) ;
#37968 = CARTESIAN_POINT ( 'NONE',  ( -27.08419642509983305, -0.7009209357102701432, 2.181485315953912707 ) ) ;
#37969 = EDGE_CURVE ( 'NONE', #7715, #55405, #7408, .T. ) ;
#37970 = CARTESIAN_POINT ( 'NONE',  ( -27.01437459610461644, 25.00000000000000000, -8.240233560378637634 ) ) ;
#37971 = CARTESIAN_POINT ( 'NONE',  ( 0.8320506296491548826, 4.610676791972340816, 11.54877388447406616 ) ) ;
#37972 = CARTESIAN_POINT ( 'NONE',  ( 2.705197763288554214, 5.217779042888522234, -5.783040721897881653 ) ) ;
#37973 = AXIS2_PLACEMENT_3D ( 'NONE', #39407, #8177, #28449 ) ;
#37974 = ORIENTED_EDGE ( 'NONE', *, *, #9479, .T. ) ;
#37975 = CARTESIAN_POINT ( 'NONE',  ( 2.276198483117258586, -0.1540629821338843908, 7.644465698238557039 ) ) ;
#37976 = CIRCLE ( 'NONE', #19958, 5.000000000000001776 ) ;
#37977 = EDGE_LOOP ( 'NONE', ( #50054, #9048, #56915, #20973 ) ) ;
#37978 = CARTESIAN_POINT ( 'NONE',  ( -15.95899433880837748, 7.887743777454596206, -9.043566668317041035 ) ) ;
#37979 = CARTESIAN_POINT ( 'NONE',  ( -22.27786964138239867, 3.667590411552012597, -0.3434379038477686774 ) ) ;
#37980 = CARTESIAN_POINT ( 'NONE',  ( -35.00000000000000000, 0.000000000000000000, 0.000000000000000000 ) ) ;
#37981 = EDGE_LOOP ( 'NONE', ( #59503, #38273, #46135, #42452 ) ) ;
#37982 = CARTESIAN_POINT ( 'NONE',  ( 2.259830038566064125, 6.546987858512988367, 3.938923657570771564 ) ) ;
#37983 = ORIENTED_EDGE ( 'NONE', *, *, #30256, .T. ) ;
#37984 = CARTESIAN_POINT ( 'NONE',  ( 0.000000000000000000, -30.50000000000000000, -14.13397459621556251 ) ) ;
#37985 = ORIENTED_EDGE ( 'NONE', *, *, #1136, .F. ) ;
#37986 = AXIS2_PLACEMENT_3D ( 'NONE', #23150, #49434, #39413 ) ;
#37987 = ORIENTED_EDGE ( 'NONE', *, *, #18793, .F. ) ;
#37988 = DIRECTION ( 'NONE',  ( 0.000000000000000000, 0.000000000000000000, 1.000000000000000000 ) ) ;
#37989 = EDGE_CURVE ( 'NONE', #44595, #1539, #50279, .T. ) ;
#37990 = CARTESIAN_POINT ( 'NONE',  ( 0.2911222467163573913, -12.02952766044174027, -2.338869407810991063 ) ) ;
#37991 = AXIS2_PLACEMENT_3D ( 'NONE', #9710, #4766, #54944 ) ;
#37992 = VERTEX_POINT ( 'NONE', #29628 ) ;
#37993 = EDGE_CURVE ( 'NONE', #25258, #63926, #13004, .T. ) ;
#37994 = CARTESIAN_POINT ( 'NONE',  ( -25.86628395826706850, -5.139808748864358456, 10.84354029019568522 ) ) ;
#37995 = CARTESIAN_POINT ( 'NONE',  ( 2.440552418640495436, -2.818488640081624474, 7.166505277347720693 ) ) ;
#37996 = DIRECTION ( 'NONE',  ( 0.2475719085175094591, 0.000000000000000000, -0.9688695217174487784 ) ) ;
#37997 = ORIENTED_EDGE ( 'NONE', *, *, #26536, .T. ) ;
#37998 = CYLINDRICAL_SURFACE ( 'NONE', #50072, 5.000000000000000888 ) ;
#37999 = CARTESIAN_POINT ( 'NONE',  ( 16.03117610287102579, -28.25087052915268870, 10.32844618003480619 ) ) ;
#38000 = CARTESIAN_POINT ( 'NONE',  ( 1.452237505248552996, -6.833827325205392711, 10.65201107290465288 ) ) ;
#38001 = ORIENTED_EDGE ( 'NONE', *, *, #32366, .F. ) ;
#38002 = EDGE_CURVE ( 'NONE', #55842, #35253, #57591, .T. ) ;
#38003 = CYLINDRICAL_SURFACE ( 'NONE', #36268, 7.499999999999988454 ) ;
#38004 = ORIENTED_EDGE ( 'NONE', *, *, #43330, .F. ) ;
#38005 = CARTESIAN_POINT ( 'NONE',  ( -4.975205859172452172, -1.416020129149132778, 25.00000000000000000 ) ) ;
#38006 = ORIENTED_EDGE ( 'NONE', *, *, #55697, .T. ) ;
#38007 = CARTESIAN_POINT ( 'NONE',  ( 35.00000000000000000, 4.705694406421931860E-17, -3.469127814946512892E-15 ) ) ;
#38008 = DIRECTION ( 'NONE',  ( 1.000000000000000000, -0.000000000000000000, 0.000000000000000000 ) ) ;
#38009 = CARTESIAN_POINT ( 'NONE',  ( -35.00000000000000000, -10.91536515067645041, -4.339012074900068683 ) ) ;
#38010 = CARTESIAN_POINT ( 'NONE',  ( 0.3474126878361877835, -3.953748424960721319, 11.61929161290145451 ) ) ;
#38011 = CARTESIAN_POINT ( 'NONE',  ( 0.2653141617321038703, -11.52265685897332048, 4.147035654172678498 ) ) ;
#38012 = CARTESIAN_POINT ( 'NONE',  ( -35.04582288351658548, 0.009684687560339159604, 0.008224400713780126784 ) ) ;
#38013 = CARTESIAN_POINT ( 'NONE',  ( 13.00153132360262020, 13.08923778586748732, -3.311356634985274994 ) ) ;
#38014 = ORIENTED_EDGE ( 'NONE', *, *, #10978, .F. ) ;
#38015 = ORIENTED_EDGE ( 'NONE', *, *, #7520, .F. ) ;
#38016 = DIRECTION ( 'NONE',  ( -0.000000000000000000, -0.000000000000000000, -1.000000000000000000 ) ) ;
#38017 = ORIENTED_EDGE ( 'NONE', *, *, #28091, .F. ) ;
#38018 = ORIENTED_EDGE ( 'NONE', *, *, #3501, .F. ) ;
#38019 = CARTESIAN_POINT ( 'NONE',  ( -22.29290468048228036, 3.357740900108103776, 1.621390503294450225 ) ) ;
#38020 = FACE_OUTER_BOUND ( 'NONE', #986, .T. ) ;
#38021 = CARTESIAN_POINT ( 'NONE',  ( 0.3006302518452010353, -10.50091819089219847, 6.323626002161042869 ) ) ;
#38022 = FACE_OUTER_BOUND ( 'NONE', #34952, .T. ) ;
#38023 = AXIS2_PLACEMENT_3D ( 'NONE', #51132, #39494, #39827 ) ;
#38024 = DIRECTION ( 'NONE',  ( 0.000000000000000000, -0.6269146997507876184, -0.7790879021242596014 ) ) ;
#38025 = EDGE_CURVE ( 'NONE', #31754, #57595, #22508, .T. ) ;
#38026 = CARTESIAN_POINT ( 'NONE',  ( 0.4613984246114875565, -10.80075367333618352, -5.909164750631147989 ) ) ;
#38027 = EDGE_CURVE ( 'NONE', #21899, #58914, #26813, .T. ) ;
#38028 = VERTEX_POINT ( 'NONE', #17619 ) ;
#38029 = CARTESIAN_POINT ( 'NONE',  ( -27.08416781016246588, -1.485424708116789061, -1.744495588874931169 ) ) ;
#38030 = CIRCLE ( 'NONE', #8292, 2.899999999999995026 ) ;
#38031 = CARTESIAN_POINT ( 'NONE',  ( 35.00000000000000000, 9.752226076388984310, 6.547236723513913503 ) ) ;
#38032 = ADVANCED_FACE ( 'NONE', ( #23245 ), #23585, .T. ) ;
#38033 = VECTOR ( 'NONE', #42035, 1000.000000000000000 ) ;
#38034 = DIRECTION ( 'NONE',  ( -1.000000000000000000, -0.000000000000000000, -0.000000000000000000 ) ) ;
#38035 = DIRECTION ( 'NONE',  ( 1.000000000000000000, 0.000000000000000000, -0.000000000000000000 ) ) ;
#38036 =( BOUNDED_CURVE ( )  B_SPLINE_CURVE ( 3, ( #23873, #38147, #27864, #23199 ),
 .UNSPECIFIED., .F., .F. ) 
 B_SPLINE_CURVE_WITH_KNOTS ( ( 4, 4 ),
 ( 5.214177674634521864, 5.220361350322005656 ),
 .UNSPECIFIED. ) 
 CURVE ( )  GEOMETRIC_REPRESENTATION_ITEM ( )  RATIONAL_B_SPLINE_CURVE ( ( 1.000000000000000000, 0.9999968135154544413, 0.9999968135154544413, 1.000000000000000000 ) ) 
 REPRESENTATION_ITEM ( '' )  );
#38037 = DIRECTION ( 'NONE',  ( 1.000000000000000000, -0.000000000000000000, -0.000000000000000000 ) ) ;
#38038 = CARTESIAN_POINT ( 'NONE',  ( 1.452237505248555660, 12.34692280296795985, -2.778494755358929424 ) ) ;
#38039 = EDGE_CURVE ( 'NONE', #24268, #34288, #8598, .T. ) ;
#38041 = EDGE_LOOP ( 'NONE', ( #25418, #16148, #49109, #59787 ) ) ;
#38040 = EDGE_CURVE ( 'NONE', #39632, #23832, #55484, .T. ) ;
#38042 = CARTESIAN_POINT ( 'NONE',  ( 0.2651627923886305527, 2.213220384814432951, -12.04449855907066436 ) ) ;
#38043 = CARTESIAN_POINT ( 'NONE',  ( 0.3218525148189829710, -1.888670068297569449, -12.11874253990391637 ) ) ;
#38044 = DIRECTION ( 'NONE',  ( -1.000000000000000000, 0.000000000000000000, 0.000000000000000000 ) ) ;
#38045 = DIRECTION ( 'NONE',  ( 0.000000000000000000, 0.000000000000000000, -1.000000000000000000 ) ) ;
#38046 = EDGE_CURVE ( 'NONE', #52497, #31515, #18469, .T. ) ;
#38047 = CIRCLE ( 'NONE', #11525, 5.000000000000000000 ) ;
#38048 = CARTESIAN_POINT ( 'NONE',  ( -35.00000000000000000, 6.018036132182325026, -11.24036214326513949 ) ) ;
#38049 = ORIENTED_EDGE ( 'NONE', *, *, #37135, .T. ) ;
#38050 = AXIS2_PLACEMENT_3D ( 'NONE', #16191, #5919, #26175 ) ;
#38051 = DIRECTION ( 'NONE',  ( 0.000000000000000000, 0.01356324068817991828, -0.9999080150203990547 ) ) ;
#38052 = CARTESIAN_POINT ( 'NONE',  ( 5.530133899448235191, 0.01550764871776275436, -0.003876417824003384680 ) ) ;
#38053 = DIRECTION ( 'NONE',  ( -1.000000000000000000, 0.000000000000000000, 0.000000000000000000 ) ) ;
#38054 = CARTESIAN_POINT ( 'NONE',  ( -22.27218376572352554, 3.670373711461416111, -0.3046453028544185981 ) ) ;
#38055 = ORIENTED_EDGE ( 'NONE', *, *, #37642, .T. ) ;
#38056 = CARTESIAN_POINT ( 'NONE',  ( 0.000000000000000000, -0.3246585432985730213, -6.805031400696120336 ) ) ;
#38057 = CARTESIAN_POINT ( 'NONE',  ( -19.02967556479663713, 11.99999999999999645, 1.585036030062028271E-15 ) ) ;
#38058 = ORIENTED_EDGE ( 'NONE', *, *, #17751, .T. ) ;
#38059 = ORIENTED_EDGE ( 'NONE', *, *, #27608, .T. ) ;
#38060 = DIRECTION ( 'NONE',  ( 0.000000000000000000, 0.01356324068818000848, -0.9999080150203990547 ) ) ;
#38061 = EDGE_CURVE ( 'NONE', #12842, #52828, #16179, .T. ) ;
#38062 = AXIS2_PLACEMENT_3D ( 'NONE', #53083, #8505, #3214 ) ;
#38063 = CARTESIAN_POINT ( 'NONE',  ( -35.00000000000000000, -6.946017217729864690, -10.01317267707894310 ) ) ;
#38064 = ORIENTED_EDGE ( 'NONE', *, *, #35915, .T. ) ;
#38065 = EDGE_CURVE ( 'NONE', #42754, #39718, #27755, .T. ) ;
#38066 = DIRECTION ( 'NONE',  ( 1.000000000000000000, 0.000000000000000000, 0.000000000000000000 ) ) ;
#38067 = CARTESIAN_POINT ( 'NONE',  ( 0.2638984909335716500, -9.508791614589247487, 7.718810690099029870 ) ) ;
#38068 = CIRCLE ( 'NONE', #44473, 12.18650000000000055 ) ;
#38069 = DIRECTION ( 'NONE',  ( -1.000000000000000000, 0.000000000000000000, 0.000000000000000000 ) ) ;
#38070 = AXIS2_PLACEMENT_3D ( 'NONE', #1138, #21417, #61983 ) ;
#38071 = CARTESIAN_POINT ( 'NONE',  ( 2.257661810676419911, -7.546014018371154819, -1.193649218120667044 ) ) ;
#38072 = DIRECTION ( 'NONE',  ( -1.000000000000000000, -0.000000000000000000, 0.000000000000000000 ) ) ;
#38073 = DIRECTION ( 'NONE',  ( 1.000000000000000000, 0.000000000000000000, 0.000000000000000000 ) ) ;
#38075 = VERTEX_POINT ( 'NONE', #12939 ) ;
#38074 = FACE_OUTER_BOUND ( 'NONE', #14298, .T. ) ;
#38076 = VECTOR ( 'NONE', #62235, 1000.000000000000000 ) ;
#38077 = DIRECTION ( 'NONE',  ( -1.000000000000000000, 0.000000000000000000, 0.000000000000000000 ) ) ;
#38078 = ORIENTED_EDGE ( 'NONE', *, *, #35288, .F. ) ;
#38079 = LINE ( 'NONE', #43732, #53998 ) ;
#38080 = ORIENTED_EDGE ( 'NONE', *, *, #51423, .F. ) ;
#38081 = AXIS2_PLACEMENT_3D ( 'NONE', #23833, #49440, #24139 ) ;
#38082 = VERTEX_POINT ( 'NONE', #48532 ) ;
#38083 = CARTESIAN_POINT ( 'NONE',  ( -26.18480416658880117, 12.06940664534210939, 6.048772596418739766 ) ) ;
#38084 = CARTESIAN_POINT ( 'NONE',  ( 3.168054457075969665, -30.71813892570239801, 15.09231838820068106 ) ) ;
#38085 = DIRECTION ( 'NONE',  ( -1.000000000000000000, -0.000000000000000000, 0.000000000000000000 ) ) ;
#38086 = CARTESIAN_POINT ( 'NONE',  ( -25.00000000000000355, -3.797884998337192286, -23.99999999999999289 ) ) ;
#38087 = CARTESIAN_POINT ( 'NONE',  ( -27.08418179957658367, 0.7235373421492767854, -2.174042548349540471 ) ) ;
#38088 = EDGE_LOOP ( 'NONE', ( #41332, #47272, #14768, #60126 ) ) ;
#38089 = CARTESIAN_POINT ( 'NONE',  ( -24.91103398156301907, -10.02593217122324987, 6.596658411782785336 ) ) ;
#38090 = CARTESIAN_POINT ( 'NONE',  ( -37.00000000000000711, 2.185196060783882288, 11.54110654723649709 ) ) ;
#38092 = EDGE_LOOP ( 'NONE', ( #53505, #46039, #31921, #62872 ) ) ;
#38091 = DIRECTION ( 'NONE',  ( -1.000000000000000000, 0.000000000000000000, 0.000000000000000000 ) ) ;
#38093 = ORIENTED_EDGE ( 'NONE', *, *, #140, .T. ) ;
#38094 = LINE ( 'NONE', #7866, #52385 ) ;
#38095 = VERTEX_POINT ( 'NONE', #22934 ) ;
#38096 = CARTESIAN_POINT ( 'NONE',  ( -35.00000000000000000, 5.865551165831237590, -11.32068061209289134 ) ) ;
#38097 = CARTESIAN_POINT ( 'NONE',  ( 0.2869720083484389450, 0.2084396331388363444, -12.25163264065380453 ) ) ;
#38098 = CARTESIAN_POINT ( 'NONE',  ( 0.3040950598368152291, 12.25911170648142701, -0.2511348647276077650 ) ) ;
#38099 = CARTESIAN_POINT ( 'NONE',  ( 0.000000000000000000, -0.7281529553922420073, 7.464569195442772198 ) ) ;
#38100 = LINE ( 'NONE', #58409, #26697 ) ;
#38101 = CARTESIAN_POINT ( 'NONE',  ( -27.08506889328344158, -1.872884652028457220, 1.324351020478543806 ) ) ;
#38102 = VECTOR ( 'NONE', #25285, 1000.000000000000000 ) ;
#38103 = CARTESIAN_POINT ( 'NONE',  ( 2.245754705088396364, 3.913944702466356063, -6.556487589645189296 ) ) ;
#38104 = EDGE_CURVE ( 'NONE', #23316, #22231, #9765, .T. ) ;
#38105 = ORIENTED_EDGE ( 'NONE', *, *, #4611, .F. ) ;
#38106 = DIRECTION ( 'NONE',  ( 0.000000000000000000, 0.7617968321374899432, 0.6478160128811920604 ) ) ;
#38107 = CIRCLE ( 'NONE', #50848, 12.18650000000000055 ) ;
#38108 = ORIENTED_EDGE ( 'NONE', *, *, #4016, .T. ) ;
#38109 = CARTESIAN_POINT ( 'NONE',  ( -22.66110217412718342, 3.914841338650350444, 3.020638270782502133 ) ) ;
#38110 = CARTESIAN_POINT ( 'NONE',  ( 2.251139882113958990, -3.925854078924265966, 6.551456272498888289 ) ) ;
#38111 = CARTESIAN_POINT ( 'NONE',  ( 0.2653141617321018164, -11.49253039221379957, -4.229807441322429362 ) ) ;
#38112 = AXIS2_PLACEMENT_3D ( 'NONE', #20779, #46700, #5845 ) ;
#38113 = ORIENTED_EDGE ( 'NONE', *, *, #22270, .T. ) ;
#38114 = EDGE_CURVE ( 'NONE', #17397, #10044, #33556, .T. ) ;
#38115 = CARTESIAN_POINT ( 'NONE',  ( -27.08954555554413446, 0.1819824474943435577, 2.300063521504146724 ) ) ;
#38116 = VERTEX_POINT ( 'NONE', #8279 ) ;
#38117 = CARTESIAN_POINT ( 'NONE',  ( 35.00000000000000000, 9.733281772932159015, -8.235637554476680222 ) ) ;
#38118 = CARTESIAN_POINT ( 'NONE',  ( 2.000000000000001776, 1.225832621831950187, -6.827324998361564923 ) ) ;
#38119 = CARTESIAN_POINT ( 'NONE',  ( 2.276905613633648962, 1.479235344773160987, 7.501802783089481785 ) ) ;
#38120 = DIRECTION ( 'NONE',  ( 1.000000000000000000, 0.000000000000000000, 0.000000000000000000 ) ) ;
#38121 = ADVANCED_FACE ( 'NONE', ( #28556 ), #48856, .T. ) ;
#38122 = VERTEX_POINT ( 'NONE', #13576 ) ;
#38123 = CARTESIAN_POINT ( 'NONE',  ( 0.2653141334712582067, -6.161213243425185837, -10.58342934917118328 ) ) ;
#38124 = CARTESIAN_POINT ( 'NONE',  ( 36.00000000000000711, 2.527899948230813987, 12.49688848680881037 ) ) ;
#38125 = CYLINDRICAL_SURFACE ( 'NONE', #1503, 6.342778212674966554 ) ;
#38126 = VECTOR ( 'NONE', #20130, 1000.000000000000000 ) ;
#38127 = FACE_OUTER_BOUND ( 'NONE', #24303, .T. ) ;
#38128 = EDGE_CURVE ( 'NONE', #15694, #54998, #33865, .T. ) ;
#38129 = CARTESIAN_POINT ( 'NONE',  ( 2.907497136250526637, -3.613027414876720300, 6.976431712756427928 ) ) ;
#38130 = DIRECTION ( 'NONE',  ( -1.000000000000000000, -0.000000000000000000, -0.000000000000000000 ) ) ;
#38131 = ORIENTED_EDGE ( 'NONE', *, *, #24242, .F. ) ;
#38132 = CARTESIAN_POINT ( 'NONE',  ( 35.00000000000000000, 12.15823808070323508, 0.8294751490777961811 ) ) ;
#38133 = DIRECTION ( 'NONE',  ( 1.000000000000000000, 0.000000000000000000, 0.000000000000000000 ) ) ;
#38134 = B_SPLINE_CURVE_WITH_KNOTS ( 'NONE', 3,
 ( #12548, #22558, #37841, #26546, #1301, #58132, #21581, #41844, #16587, #36853, #11580, #31850, #16901, #52164, #6616, #26884 ),
 .UNSPECIFIED., .F., .F.,
 ( 4, 3, 3, 3, 3, 4 ),
 ( 3.325020220743593725E-17, 0.0002126834539179991046, 0.0004253519300366846289, 0.0006380165497225060529, 0.0007442707582429298162, 0.0009453531351393624962 ),
 .UNSPECIFIED. ) ;
#38135 = CARTESIAN_POINT ( 'NONE',  ( -12.50548042261300097, -29.27747730776674118, -5.013933227252968194 ) ) ;
#38136 = ORIENTED_EDGE ( 'NONE', *, *, #19617, .T. ) ;
#38137 = CARTESIAN_POINT ( 'NONE',  ( -17.16501208148281066, 3.058370451741322604, -13.14974288367183597 ) ) ;
#38138 = CARTESIAN_POINT ( 'NONE',  ( 2.000000000000001776, 1.865193240757095916, 6.552473556515182374 ) ) ;
#38139 = DIRECTION ( 'NONE',  ( 0.000000000000000000, -0.8369827122275401710, -0.5472293298355185298 ) ) ;
#38140 = CARTESIAN_POINT ( 'NONE',  ( 5.520433897694421610, 0.005630909886752951364, 0.01397038704729916363 ) ) ;
#38141 = CARTESIAN_POINT ( 'NONE',  ( 0.2872850955227749803, -11.44140577127595648, 4.386654201695106003 ) ) ;
#38142 = EDGE_CURVE ( 'NONE', #39511, #18880, #37388, .T. ) ;
#38143 = CIRCLE ( 'NONE', #55097, 6.936499999999987232 ) ;
#38144 = ORIENTED_EDGE ( 'NONE', *, *, #5585, .F. ) ;
#38145 = FACE_OUTER_BOUND ( 'NONE', #27145, .T. ) ;
#38146 = ORIENTED_EDGE ( 'NONE', *, *, #39680, .T. ) ;
#38147 = CARTESIAN_POINT ( 'NONE',  ( 17.11285760380283705, -10.50878607827770317, 5.793619504978386736 ) ) ;
#38148 = DIRECTION ( 'NONE',  ( -1.000000000000000000, 0.000000000000000000, 0.000000000000000000 ) ) ;
#38149 = DIRECTION ( 'NONE',  ( 1.000000000000000000, 0.000000000000000000, 0.000000000000000000 ) ) ;
#38150 = CARTESIAN_POINT ( 'NONE',  ( -16.98800322446194855, 2.922502605998049674, 25.00000000000000000 ) ) ;
#38152 = CARTESIAN_POINT ( 'NONE',  ( 35.00000000000000000, -11.81949347079744506, 2.968224442958526943 ) ) ;
#38151 = CIRCLE ( 'NONE', #18002, 7.499999999999988454 ) ;
#38153 = CARTESIAN_POINT ( 'NONE',  ( 0.2638984909335720941, 0.1991813963113996944, 12.24571285024409129 ) ) ;
#38154 = ORIENTED_EDGE ( 'NONE', *, *, #24533, .F. ) ;
#38155 = ORIENTED_EDGE ( 'NONE', *, *, #29457, .F. ) ;
#38156 = CARTESIAN_POINT ( 'NONE',  ( 0.2655924914740778742, -10.58356227062113675, 6.161287456391646877 ) ) ;
#38157 = ORIENTED_EDGE ( 'NONE', *, *, #15959, .T. ) ;
#38158 = CARTESIAN_POINT ( 'NONE',  ( 35.00000000000000000, 4.705694406421931860E-17, -3.469127814946512892E-15 ) ) ;
#38159 = CIRCLE ( 'NONE', #48824, 5.000000000000000000 ) ;
#38160 = EDGE_CURVE ( 'NONE', #34180, #31078, #60752, .T. ) ;
#38161 = LINE ( 'NONE', #51845, #61933 ) ;
#38162 = CARTESIAN_POINT ( 'NONE',  ( -35.00000000000000000, 0.000000000000000000, 0.000000000000000000 ) ) ;
#38164 = ORIENTED_EDGE ( 'NONE', *, *, #52964, .F. ) ;
#38163 = CIRCLE ( 'NONE', #59394, 12.18649999999999878 ) ;
#38165 = DIRECTION ( 'NONE',  ( -1.000000000000000000, -0.000000000000000000, -0.000000000000000000 ) ) ;
#38166 = CARTESIAN_POINT ( 'NONE',  ( 3.047904605210427942, 1.788881754552641867, -7.698174516567096504 ) ) ;
#38167 = DIRECTION ( 'NONE',  ( -1.000000000000000000, 0.000000000000000000, 0.000000000000000000 ) ) ;
#38168 = EDGE_LOOP ( 'NONE', ( #43156, #48820, #42594, #57380 ) ) ;
#38169 = EDGE_LOOP ( 'NONE', ( #52098, #17014, #9417, #47978 ) ) ;
#38170 = CARTESIAN_POINT ( 'NONE',  ( 2.000000000000001776, 0.000000000000000000, 0.000000000000000000 ) ) ;
#38171 = ORIENTED_EDGE ( 'NONE', *, *, #28283, .T. ) ;
#38172 = DIRECTION ( 'NONE',  ( -1.000000000000000000, -0.000000000000000000, 0.000000000000000000 ) ) ;
#38173 = VERTEX_POINT ( 'NONE', #24217 ) ;
#38174 = CIRCLE ( 'NONE', #11604, 2.899999999999995026 ) ;
#38175 = EDGE_LOOP ( 'NONE', ( #41958, #5149, #22035, #26898 ) ) ;
#38176 = CARTESIAN_POINT ( 'NONE',  ( -22.27718112499583469, -2.901898111564438221, 2.265557025479510322 ) ) ;
#38177 = CARTESIAN_POINT ( 'NONE',  ( -27.10512513516319899, -1.618446180706342163, 1.709353012333651112 ) ) ;
#38178 = CARTESIAN_POINT ( 'NONE',  ( 2.000000000000001776, 7.484036900328565167, 0.4890722589969472844 ) ) ;
#38179 = CARTESIAN_POINT ( 'NONE',  ( 0.2676618633000460434, 7.994628339664956229, -9.277614237849192591 ) ) ;
#38180 = CARTESIAN_POINT ( 'NONE',  ( 5.520433897694421610, 0.01397038704729859290, 0.005630909886752917537 ) ) ;
#38181 = CARTESIAN_POINT ( 'NONE',  ( 35.00000000000000000, 0.3025107581131208367, -11.74226168163341555 ) ) ;
#38182 = EDGE_CURVE ( 'NONE', #27902, #29107, #8734, .T. ) ;
#38183 = ORIENTED_EDGE ( 'NONE', *, *, #48857, .T. ) ;
#38184 = CARTESIAN_POINT ( 'NONE',  ( -37.00000000000000711, -12.70128625845193859, 1.113475361586445000 ) ) ;
#38185 = ADVANCED_FACE ( 'NONE', ( #55130 ), #35502, .T. ) ;
#38186 = CARTESIAN_POINT ( 'NONE',  ( -22.27721701579900682, 2.783642043008654809, -2.409654355488377586 ) ) ;
#38187 = EDGE_CURVE ( 'NONE', #33435, #3297, #54415, .T. ) ;
#38188 = CARTESIAN_POINT ( 'NONE',  ( -10.00000000000000178, 0.000000000000000000, 0.000000000000000000 ) ) ;
#38189 = CARTESIAN_POINT ( 'NONE',  ( -22.30625920655495165, 2.610366806364701642, -2.750410778797873323 ) ) ;
#38190 = CARTESIAN_POINT ( 'NONE',  ( 28.69468230381643892, 10.59444862976622304, 5.650893053773811125 ) ) ;
#38191 = DIRECTION ( 'NONE',  ( -1.000000000000000000, 0.000000000000000000, -0.000000000000000000 ) ) ;
#38192 = CARTESIAN_POINT ( 'NONE',  ( 37.00000000000000711, -12.74921544981110877, 0.1414404973753431438 ) ) ;
#38193 = CARTESIAN_POINT ( 'NONE',  ( 3.347841273039249721, -10.61118957148187825, -5.603807266321158664 ) ) ;
#38194 = CARTESIAN_POINT ( 'NONE',  ( 2.655192694323949443, -9.584054627287619255, 0.5793947661801162052 ) ) ;
#38195 = AXIS2_PLACEMENT_3D ( 'NONE', #8209, #34755, #18843 ) ;
#38196 = CIRCLE ( 'NONE', #9509, 7.499999999999988454 ) ;
#38197 = ORIENTED_EDGE ( 'NONE', *, *, #61031, .T. ) ;
#38198 = EDGE_CURVE ( 'NONE', #42734, #52495, #9240, .T. ) ;
#38199 = CARTESIAN_POINT ( 'NONE',  ( 2.305787727787083519, -7.135468203929965725, -2.774453000917220802 ) ) ;
#38200 = AXIS2_PLACEMENT_3D ( 'NONE', #10082, #55960, #5101 ) ;
#38201 = ORIENTED_EDGE ( 'NONE', *, *, #32300, .T. ) ;
#38202 = CARTESIAN_POINT ( 'NONE',  ( 3.152665057733995191, 6.622010822086684456, 4.377619405892240856 ) ) ;
#38203 = CARTESIAN_POINT ( 'NONE',  ( 35.00000000000000000, 11.99999999999999822, 1.469576158976822172E-15 ) ) ;
#38204 = CARTESIAN_POINT ( 'NONE',  ( -36.00000000000000711, -0.3137578094508294280, -12.74613886779085625 ) ) ;
#38205 = CARTESIAN_POINT ( 'NONE',  ( 3.152665057734040488, 0.000000000000000000, 0.000000000000000000 ) ) ;
#38206 = CARTESIAN_POINT ( 'NONE',  ( 2.524535260911636936, 7.646662375930073807, 1.123794384999134754 ) ) ;
#38207 = ORIENTED_EDGE ( 'NONE', *, *, #20194, .F. ) ;
#38208 = CYLINDRICAL_SURFACE ( 'NONE', #16473, 6.936499999999988120 ) ;
#38209 = DIRECTION ( 'NONE',  ( 0.000000000000000000, 0.6876994588534192099, 0.7259954919231347281 ) ) ;
#38210 = CARTESIAN_POINT ( 'NONE',  ( -36.00000000000000711, -8.366449238204298311, -9.621072037177086145 ) ) ;
#38211 = CARTESIAN_POINT ( 'NONE',  ( -35.00000000000000000, 0.000000000000000000, 0.000000000000000000 ) ) ;
#38212 = EDGE_CURVE ( 'NONE', #53630, #31059, #60125, .T. ) ;
#38213 = VECTOR ( 'NONE', #36528, 1000.000000000000000 ) ;
#38214 = DIRECTION ( 'NONE',  ( 0.000000000000000000, 0.2618041379715635442, -0.9651210252299794456 ) ) ;
#38215 = VERTEX_POINT ( 'NONE', #15540 ) ;
#38216 = FACE_OUTER_BOUND ( 'NONE', #41503, .T. ) ;
#38217 = CARTESIAN_POINT ( 'NONE',  ( -22.27834755396593991, -1.338300169228702430, 3.434702243602647975 ) ) ;
#38218 = CARTESIAN_POINT ( 'NONE',  ( -5.894163417175557029, -31.16155000483562176, 14.52685451768251923 ) ) ;
#38219 = AXIS2_PLACEMENT_3D ( 'NONE', #34878, #55185, #9617 ) ;
#38220 = VERTEX_POINT ( 'NONE', #35807 ) ;
#38221 = CARTESIAN_POINT ( 'NONE',  ( 10.47216603063722395, 7.645002999120487530, -9.252792978029043880 ) ) ;
#38222 = EDGE_LOOP ( 'NONE', ( #710, #45534, #25387, #17814 ) ) ;
#38223 = CARTESIAN_POINT ( 'NONE',  ( 2.257661810676204972, 5.013319178750904825, 5.764872664104674804 ) ) ;
#38224 = DIRECTION ( 'NONE',  ( 0.000000000000000000, 0.01356324068817998940, -0.9999080150203990547 ) ) ;
#38225 = CARTESIAN_POINT ( 'NONE',  ( 34.90603985575356205, -2.603248520265782684, 21.87429913450488428 ) ) ;
#38226 = CARTESIAN_POINT ( 'NONE',  ( 35.00000000000000000, 10.92721691015455754, -4.309077947445693724 ) ) ;
#38227 = CARTESIAN_POINT ( 'NONE',  ( -22.28236030719477512, -2.111163412226044311, -3.035028179399218207 ) ) ;
#38228 = VERTEX_POINT ( 'NONE', #39510 ) ;
#38229 = ORIENTED_EDGE ( 'NONE', *, *, #38160, .F. ) ;
#38230 = ORIENTED_EDGE ( 'NONE', *, *, #13316, .T. ) ;
#38231 = DIRECTION ( 'NONE',  ( -1.000000000000000000, 0.000000000000000000, 0.000000000000000000 ) ) ;
#38232 = EDGE_CURVE ( 'NONE', #53881, #42115, #43804, .T. ) ;
#38234 = DIRECTION ( 'NONE',  ( 0.000000000000000000, 0.000000000000000000, 1.000000000000000000 ) ) ;
#38233 = CIRCLE ( 'NONE', #60510, 12.18650000000000055 ) ;
#38235 = AXIS2_PLACEMENT_3D ( 'NONE', #44918, #9652, #29947 ) ;
#38236 = AXIS2_PLACEMENT_3D ( 'NONE', #23781, #48066, #2524 ) ;
#38237 = EDGE_LOOP ( 'NONE', ( #52872, #31186, #24091, #53304 ) ) ;
#38238 = DIRECTION ( 'NONE',  ( -0.000000000000000000, -1.000000000000000000, -0.000000000000000000 ) ) ;
#38239 = CARTESIAN_POINT ( 'NONE',  ( -22.28629837673888048, -0.2936941584814351525, -3.697248502489090427 ) ) ;
#38240 = EDGE_LOOP ( 'NONE', ( #27139, #61062, #17980, #4809 ) ) ;
#38241 = DIRECTION ( 'NONE',  ( 0.000000000000000000, -0.01356324068817991481, 0.9999080150203990547 ) ) ;
#38242 =( BOUNDED_SURFACE ( )  B_SPLINE_SURFACE ( 3, 1, ( 
 ( #17516, #36799 ),
 ( #47765, #48109 ),
 ( #62708, #11207 ),
 ( #37785, #57096 ) ),
 .UNSPECIFIED., .F., .F., .F. ) 
 B_SPLINE_SURFACE_WITH_KNOTS ( ( 4, 4 ),
 ( 2, 2 ),
 ( 0.000000000000000000, 1.000000000000000000 ),
 ( 0.000000000000000000, 1.000000000000000000 ),
 .UNSPECIFIED. ) 
 GEOMETRIC_REPRESENTATION_ITEM ( )  RATIONAL_B_SPLINE_SURFACE ( (
 ( 1.000000000000000000, 1.000000000000000000),
 ( 0.9942764183789327692, 0.8450855930916585379),
 ( 0.9942764183789327692, 0.8450855930916585379),
 ( 1.000000000000000000, 1.000000000000000000) ) ) 
 REPRESENTATION_ITEM ( '' )  SURFACE ( )  );
#38243 = CARTESIAN_POINT ( 'NONE',  ( 2.244591118396556784, -2.712243649838657067, -7.137527852925281913 ) ) ;
#38244 = CARTESIAN_POINT ( 'NONE',  ( 37.00000000000000711, 4.705694406421931860E-17, -3.469127814946512892E-15 ) ) ;
#38245 = VERTEX_POINT ( 'NONE', #4274 ) ;
#38246 = VERTEX_POINT ( 'NONE', #50493 ) ;
#38247 = CARTESIAN_POINT ( 'NONE',  ( 0.09505933169495142665, -0.1369491540312669231, 11.99999999999999112 ) ) ;
#38248 = EDGE_LOOP ( 'NONE', ( #9894, #35091, #51858, #18626 ) ) ;
#38249 = CARTESIAN_POINT ( 'NONE',  ( 9.753977307252423401, 1.283513182606664360, -13.44047255910775185 ) ) ;
#38250 = EDGE_LOOP ( 'NONE', ( #51551, #38414 ) ) ;
#38251 = CARTESIAN_POINT ( 'NONE',  ( 2.284126774967666584, 3.686252397487125965, 6.701756155761956713 ) ) ;
#38252 = AXIS2_PLACEMENT_3D ( 'NONE', #51190, #61797, #25911 ) ;
#38253 = CARTESIAN_POINT ( 'NONE',  ( 14.06742311316907212, -34.40796758970419233, -8.422011900746815272 ) ) ;
#38254 = CARTESIAN_POINT ( 'NONE',  ( -9.351388602708162523, 25.00000000000000000, -3.665735721005252135 ) ) ;
#38255 = CARTESIAN_POINT ( 'NONE',  ( -22.29978294495153790, 3.642708310327678056, 0.8878583829805118954 ) ) ;
#38256 = EDGE_CURVE ( 'NONE', #2532, #55405, #30506, .T. ) ;
#38257 = CARTESIAN_POINT ( 'NONE',  ( 37.00000000000000711, 12.08216339958902630, 1.591260454995109930 ) ) ;
#38258 = CARTESIAN_POINT ( 'NONE',  ( -22.31328051695926007, -0.2528478350593797996, -3.781397440874599614 ) ) ;
#38259 = CARTESIAN_POINT ( 'NONE',  ( -27.74980211595206114, -10.95110850461715657, -4.915186702031700605 ) ) ;
#38260 = ORIENTED_EDGE ( 'NONE', *, *, #60422, .T. ) ;
#38261 = AXIS2_PLACEMENT_3D ( 'NONE', #50110, #24492, #54108 ) ;
#38262 = CARTESIAN_POINT ( 'NONE',  ( 2.241311220309554653, -7.141707286456110637, -2.698144003944865865 ) ) ;
#38263 = VERTEX_POINT ( 'NONE', #4619 ) ;
#38264 = CARTESIAN_POINT ( 'NONE',  ( 37.00000000000000711, -11.95840593935202811, -2.346765782874394635 ) ) ;
#38265 = ADVANCED_FACE ( 'NONE', ( #60781 ), #24885, .F. ) ;
#38266 = CARTESIAN_POINT ( 'NONE',  ( 1.452237505248555660, -12.34692280296793676, 2.778494755359015134 ) ) ;
#38267 = EDGE_CURVE ( 'NONE', #10044, #11257, #46991, .T. ) ;
#38268 = ORIENTED_EDGE ( 'NONE', *, *, #33545, .F. ) ;
#38269 = CARTESIAN_POINT ( 'NONE',  ( 0.3040950598368144520, -5.912066680610537972, -10.74226959800797587 ) ) ;
#38270 = CARTESIAN_POINT ( 'NONE',  ( -10.00000000000000178, 0.000000000000000000, 0.000000000000000000 ) ) ;
#38271 = VECTOR ( 'NONE', #11044, 1000.000000000000000 ) ;
#38272 = CARTESIAN_POINT ( 'NONE',  ( 0.2717059086739019858, -2.300075171420154163, -12.03041489115254414 ) ) ;
#38273 = ORIENTED_EDGE ( 'NONE', *, *, #62470, .F. ) ;
#38274 = ORIENTED_EDGE ( 'NONE', *, *, #6684, .F. ) ;
#38275 = EDGE_CURVE ( 'NONE', #25175, #60806, #49105, .T. ) ;
#38276 = CARTESIAN_POINT ( 'NONE',  ( -28.85619398320021745, 3.750539801530000439, 25.00000000000000000 ) ) ;
#38277 = AXIS2_PLACEMENT_3D ( 'NONE', #38999, #59622, #59293 ) ;
#38278 = ORIENTED_EDGE ( 'NONE', *, *, #29417, .T. ) ;
#38279 = EDGE_CURVE ( 'NONE', #29827, #37187, #35291, .T. ) ;
#38280 = CARTESIAN_POINT ( 'NONE',  ( -21.24030193723618609, 25.00000000000000000, -5.230344621181295395 ) ) ;
#38281 = DIRECTION ( 'NONE',  ( 0.000000000000000000, 0.000000000000000000, 1.000000000000000000 ) ) ;
#38282 = CARTESIAN_POINT ( 'NONE',  ( 0.2655924914740778742, -9.409507842005970346, -7.838010948425144342 ) ) ;
#38283 = CARTESIAN_POINT ( 'NONE',  ( 2.241352910868908310, 4.970878533273838329, -5.794346703933798359 ) ) ;
#38284 = CARTESIAN_POINT ( 'NONE',  ( -18.16590544919054295, -5.562395585315481839, 10.63608869936934376 ) ) ;
#38285 = ORIENTED_EDGE ( 'NONE', *, *, #558, .T. ) ;
#38286 = CARTESIAN_POINT ( 'NONE',  ( 36.00000000000000711, -5.143145423404195782, 11.66664283989685202 ) ) ;
#38287 = EDGE_CURVE ( 'NONE', #51860, #40629, #25197, .T. ) ;
#38288 = AXIS2_PLACEMENT_3D ( 'NONE', #39528, #59827, #60142 ) ;
#38289 = VECTOR ( 'NONE', #15948, 1000.000000000000000 ) ;
#38290 = ADVANCED_FACE ( 'NONE', ( #3957 ), #40831, .T. ) ;
#38291 = FACE_OUTER_BOUND ( 'NONE', #15273, .T. ) ;
#38292 = EDGE_CURVE ( 'NONE', #37098, #8838, #60402, .T. ) ;
#38293 = FACE_OUTER_BOUND ( 'NONE', #20530, .T. ) ;
#38294 = CARTESIAN_POINT ( 'NONE',  ( -36.00000000000000711, -11.01837265713077763, 6.415447294506668285 ) ) ;
#38295 = CARTESIAN_POINT ( 'NONE',  ( 0.2651627923886329397, 7.803990550466305187, 9.437479615842670810 ) ) ;
#38296 = DIRECTION ( 'NONE',  ( 0.000000000000000000, 0.000000000000000000, 1.000000000000000000 ) ) ;
#38297 = CARTESIAN_POINT ( 'NONE',  ( -22.59969328935897437, -0.7214993884004085034, 4.594269189967448597 ) ) ;
#38298 = AXIS2_PLACEMENT_3D ( 'NONE', #18139, #53724, #1865 ) ;
#38299 = AXIS2_PLACEMENT_3D ( 'NONE', #28094, #13433, #44341 ) ;
#38300 = ORIENTED_EDGE ( 'NONE', *, *, #13658, .T. ) ;
#38301 = CARTESIAN_POINT ( 'NONE',  ( 12.68972104065789530, -10.01785652089451695, -6.609210272055840996 ) ) ;
#38302 = AXIS2_PLACEMENT_3D ( 'NONE', #16209, #11224, #46464 ) ;
#38303 = AXIS2_PLACEMENT_3D ( 'NONE', #21891, #26532, #51822 ) ;
#38304 = ORIENTED_EDGE ( 'NONE', *, *, #11209, .F. ) ;
#38305 = CARTESIAN_POINT ( 'NONE',  ( -37.00000000000000711, -3.093009498344009955, 11.78745411414838884 ) ) ;
#38306 = CARTESIAN_POINT ( 'NONE',  ( -22.30986928587821794, 3.771068405887398889, -0.2539257557460580794 ) ) ;
#38307 = CARTESIAN_POINT ( 'NONE',  ( -29.92777678363736626, -3.750539801530011985, -11.39883551934752681 ) ) ;
#38308 = ORIENTED_EDGE ( 'NONE', *, *, #17950, .F. ) ;
#38309 = CIRCLE ( 'NONE', #25709, 5.000000000000001776 ) ;
#38310 = DIRECTION ( 'NONE',  ( -1.000000000000000000, 0.000000000000000000, 0.000000000000000000 ) ) ;
#38311 = ORIENTED_EDGE ( 'NONE', *, *, #9330, .T. ) ;
#38312 = FACE_OUTER_BOUND ( 'NONE', #58832, .T. ) ;
#38313 = ORIENTED_EDGE ( 'NONE', *, *, #24013, .F. ) ;
#38314 = ORIENTED_EDGE ( 'NONE', *, *, #9241, .F. ) ;
#38315 = LINE ( 'NONE', #28036, #16398 ) ;
#38317 = EDGE_CURVE ( 'NONE', #65390, #20627, #32081, .T. ) ;
#38316 = CARTESIAN_POINT ( 'NONE',  ( -22.28776923226071105, -3.350304995653716755, -1.601293944844131678 ) ) ;
#38318 = EDGE_CURVE ( 'NONE', #46103, #62889, #111, .T. ) ;
#38319 = EDGE_LOOP ( 'NONE', ( #58635, #27991 ) ) ;
#38320 = DIRECTION ( 'NONE',  ( 0.000000000000000000, 0.7196168960969767658, 0.6943713148249667233 ) ) ;
#38321 = CARTESIAN_POINT ( 'NONE',  ( 3.308621013519160492, 3.312703205413596308, 13.09392454462600952 ) ) ;
#38322 = CYLINDRICAL_SURFACE ( 'NONE', #3656, 5.225920239717171789 ) ;
#38323 = CARTESIAN_POINT ( 'NONE',  ( -22.27706485742869091, -2.580541389029911148, -2.625261754997698205 ) ) ;
#38324 = VERTEX_POINT ( 'NONE', #48063 ) ;
#38325 = DIRECTION ( 'NONE',  ( 0.000000000000000000, -0.01356324068817991828, 0.9999080150203990547 ) ) ;
#38326 = CARTESIAN_POINT ( 'NONE',  ( 18.66975156949834513, -28.88996333714986875, 7.079161351701957372 ) ) ;
#38327 = DIRECTION ( 'NONE',  ( 0.000000000000000000, -0.6478160128812002760, 0.7617968321374830598 ) ) ;
#38329 = ORIENTED_EDGE ( 'NONE', *, *, #39361, .T. ) ;
#38328 = FACE_OUTER_BOUND ( 'NONE', #62399, .T. ) ;
#38331 = AXIS2_PLACEMENT_3D ( 'NONE', #17473, #37747, #22796 ) ;
#38330 = CARTESIAN_POINT ( 'NONE',  ( 0.2646305136544065406, 6.008537389229564596, -10.67138229758223211 ) ) ;
#38332 = VERTEX_POINT ( 'NONE', #32411 ) ;
#38333 = CARTESIAN_POINT ( 'NONE',  ( 37.00000000000000711, -11.07407352312215387, -3.916263239775311433 ) ) ;
#38334 = EDGE_CURVE ( 'NONE', #42662, #60382, #42370, .T. ) ;
#38335 = VERTEX_POINT ( 'NONE', #17133 ) ;
#38336 = DIRECTION ( 'NONE',  ( -1.000000000000000000, 0.000000000000000000, 0.000000000000000000 ) ) ;
#38337 = CARTESIAN_POINT ( 'NONE',  ( 0.3341166715381294616, 3.958014133396767775, -11.61315925169690821 ) ) ;
#38338 = CARTESIAN_POINT ( 'NONE',  ( 15.69195845145067736, -33.00000000000000000, 4.009712365929969380 ) ) ;
#38339 = CARTESIAN_POINT ( 'NONE',  ( 0.2958664285830416851, -3.984029505266645454, 11.59077733151254996 ) ) ;
#38340 = AXIS2_PLACEMENT_3D ( 'NONE', #10100, #35008, #41320 ) ;
#38341 = CIRCLE ( 'NONE', #59625, 12.18649999999999878 ) ;
#38343 = CIRCLE ( 'NONE', #1187, 12.18650000000000233 ) ;
#38342 = CYLINDRICAL_SURFACE ( 'NONE', #47381, 4.999999999999999112 ) ;
#38344 = ADVANCED_FACE ( 'NONE', ( #7148 ), #33070, .T. ) ;
#38345 = CARTESIAN_POINT ( 'NONE',  ( -6.388056983029618330, -1.618957853436955308, -13.40265429600850311 ) ) ;
#38346 = CARTESIAN_POINT ( 'NONE',  ( -35.00000000000000000, -9.493370459201647904, -6.917234959366931335 ) ) ;
#38347 = VERTEX_POINT ( 'NONE', #17469 ) ;
#38348 = CIRCLE ( 'NONE', #60614, 2.899999999999995026 ) ;
#38349 = CYLINDRICAL_SURFACE ( 'NONE', #50769, 12.18649999999999878 ) ;
#38350 = ORIENTED_EDGE ( 'NONE', *, *, #9606, .T. ) ;
#38351 = EDGE_CURVE ( 'NONE', #52499, #53854, #43762, .T. ) ;
#38352 = ORIENTED_EDGE ( 'NONE', *, *, #5105, .F. ) ;
#38353 = CARTESIAN_POINT ( 'NONE',  ( 2.000000000000001776, -3.805198749487460841, 5.799611601383201531 ) ) ;
#38354 = CARTESIAN_POINT ( 'NONE',  ( -22.30986928587821794, 3.392803916780413598, 1.665628047792409472 ) ) ;
#38355 = CARTESIAN_POINT ( 'NONE',  ( -27.15525204139122550, 2.394850816831299856, -0.7327319213109826368 ) ) ;
#38356 = CARTESIAN_POINT ( 'NONE',  ( -22.31099767395441091, 2.106713667647955202, 3.142100240805162592 ) ) ;
#38358 = AXIS2_PLACEMENT_3D ( 'NONE', #34794, #19858, #55769 ) ;
#38357 = CARTESIAN_POINT ( 'NONE',  ( 5.514970785353741078, 0.004532877335078711566, 0.001326349372336311627 ) ) ;
#38359 = AXIS2_PLACEMENT_3D ( 'NONE', #17712, #13038, #43609 ) ;
#38360 = CARTESIAN_POINT ( 'NONE',  ( -35.00000000000000000, 11.17622378668011685, -3.614449339633368119 ) ) ;
#38361 = DIRECTION ( 'NONE',  ( 1.000000000000000000, -0.000000000000000000, 0.000000000000000000 ) ) ;
#38362 = AXIS2_PLACEMENT_3D ( 'NONE', #45567, #39928, #692 ) ;
#38363 = VERTEX_POINT ( 'NONE', #27759 ) ;
#38364 = EDGE_CURVE ( 'NONE', #4569, #14095, #19370, .T. ) ;
#38365 = CYLINDRICAL_SURFACE ( 'NONE', #7387, 12.18649999999999878 ) ;
#38366 = CIRCLE ( 'NONE', #60624, 12.74999999999999822 ) ;
#38367 = CARTESIAN_POINT ( 'NONE',  ( -10.00000000000000178, 0.000000000000000000, 0.000000000000000000 ) ) ;
#38368 = DIRECTION ( 'NONE',  ( -0.000000000000000000, -1.000000000000000000, -0.000000000000000000 ) ) ;
#38369 = EDGE_CURVE ( 'NONE', #63832, #22351, #27859, .T. ) ;
#38370 = AXIS2_PLACEMENT_3D ( 'NONE', #64123, #18603, #59151 ) ;
#38371 = EDGE_CURVE ( 'NONE', #54954, #19174, #53359, .T. ) ;
#38372 = DIRECTION ( 'NONE',  ( 0.000000000000000000, 0.000000000000000000, 1.000000000000000000 ) ) ;
#38373 = DIRECTION ( 'NONE',  ( -1.000000000000000000, 0.000000000000000000, 0.000000000000000000 ) ) ;
#38374 = EDGE_CURVE ( 'NONE', #20925, #22914, #61840, .T. ) ;
#38375 = CARTESIAN_POINT ( 'NONE',  ( 2.241451721903214178, -2.553895636571891004, -7.194631024842671252 ) ) ;
#38376 = EDGE_CURVE ( 'NONE', #41890, #52499, #19098, .T. ) ;
#38377 = LINE ( 'NONE', #8133, #11868 ) ;
#38378 = CIRCLE ( 'NONE', #9705, 5.000000000000001776 ) ;
#38379 = AXIS2_PLACEMENT_3D ( 'NONE', #12061, #36003, #31039 ) ;
#38380 = VERTEX_POINT ( 'NONE', #18472 ) ;
#38381 = CARTESIAN_POINT ( 'NONE',  ( 1.719304012339869514, -10.22720798541492471, 7.581471372739622794 ) ) ;
#38382 = LINE ( 'NONE', #23095, #65424 ) ;
#38383 = CARTESIAN_POINT ( 'NONE',  ( -23.41523303002442091, -1.997501275420740630, -4.252418708693360472 ) ) ;
#38384 = CIRCLE ( 'NONE', #51128, 12.74999999999999822 ) ;
#38385 = CIRCLE ( 'NONE', #9718, 2.899999999999995914 ) ;
#38386 = CARTESIAN_POINT ( 'NONE',  ( -24.90268129027903399, 7.525069038327800719, 9.354736030227490673 ) ) ;
#38387 = DIRECTION ( 'NONE',  ( 0.000000000000000000, 0.01356324068817998940, -0.9999080150203989437 ) ) ;
#38388 = VERTEX_POINT ( 'NONE', #28741 ) ;
#38389 = CARTESIAN_POINT ( 'NONE',  ( -15.27729454824424948, 5.151216734910788908, 25.00000000000000000 ) ) ;
#38390 = CARTESIAN_POINT ( 'NONE',  ( 0.2657645697724705380, 9.283243433323075777, 7.987126944299666853 ) ) ;
#38391 = CARTESIAN_POINT ( 'NONE',  ( -35.04643116707788408, 0.01193867652720184691, -0.002453861112635541408 ) ) ;
#38392 = ORIENTED_EDGE ( 'NONE', *, *, #41941, .F. ) ;
#38393 = CARTESIAN_POINT ( 'NONE',  ( -36.00000000000000711, 2.527899948230635907, 12.49688848680885300 ) ) ;
#38394 = DIRECTION ( 'NONE',  ( -0.000000000000000000, -0.000000000000000000, -1.000000000000000000 ) ) ;
#38395 = ORIENTED_EDGE ( 'NONE', *, *, #31577, .F. ) ;
#38396 = ORIENTED_EDGE ( 'NONE', *, *, #43212, .F. ) ;
#38397 = B_SPLINE_CURVE_WITH_KNOTS ( 'NONE', 3,
 ( #19255, #29864, #19589, #14558, #55142, #9569, #617, #10905 ),
 .UNSPECIFIED., .F., .F.,
 ( 4, 2, 2, 4 ),
 ( 0.01054950296625598721, 0.01134544828840661213, 0.01214139361055723877, 0.01373328425485848513 ),
 .UNSPECIFIED. ) ;
#38398 = CARTESIAN_POINT ( 'NONE',  ( -35.00000000000000000, 0.000000000000000000, 0.000000000000000000 ) ) ;
#38399 = VECTOR ( 'NONE', #2205, 1000.000000000000000 ) ;
#38400 = AXIS2_PLACEMENT_3D ( 'NONE', #42137, #46182, #10919 ) ;
#38401 = EDGE_CURVE ( 'NONE', #40447, #28337, #27915, .T. ) ;
#38402 = ORIENTED_EDGE ( 'NONE', *, *, #63949, .F. ) ;
#38403 = AXIS2_PLACEMENT_3D ( 'NONE', #6584, #27178, #47790 ) ;
#38404 = CARTESIAN_POINT ( 'NONE',  ( -35.00000000000000000, -0.9416912585473466990, -12.71517666308949046 ) ) ;
#38405 = EDGE_CURVE ( 'NONE', #64117, #44435, #26859, .T. ) ;
#38406 = CARTESIAN_POINT ( 'NONE',  ( -47.00000000000000711, 0.000000000000000000, 0.000000000000000000 ) ) ;
#38407 = DIRECTION ( 'NONE',  ( 0.000000000000000000, 0.01356324068817992175, -0.9999080150203990547 ) ) ;
#38408 = CARTESIAN_POINT ( 'NONE',  ( -37.25000000000000711, -27.21021009056489603, 4.499999999999997335 ) ) ;
#38409 = CARTESIAN_POINT ( 'NONE',  ( -37.00000000000000711, 11.50504120060943158, 4.018060380616439886 ) ) ;
#38410 = DIRECTION ( 'NONE',  ( -1.000000000000000000, -0.000000000000000000, 0.000000000000000000 ) ) ;
#38412 = ORIENTED_EDGE ( 'NONE', *, *, #41878, .T. ) ;
#38411 = DIRECTION ( 'NONE',  ( -1.000000000000000000, -0.000000000000000000, 0.000000000000000000 ) ) ;
#38413 = CYLINDRICAL_SURFACE ( 'NONE', #26748, 12.75000000000000178 ) ;
#38414 = ORIENTED_EDGE ( 'NONE', *, *, #48633, .T. ) ;
#38415 = CARTESIAN_POINT ( 'NONE',  ( -37.00000000000000711, 0.000000000000000000, 0.000000000000000000 ) ) ;
#38416 = VECTOR ( 'NONE', #63617, 1000.000000000000000 ) ;
#38417 = ORIENTED_EDGE ( 'NONE', *, *, #21341, .T. ) ;
#38418 = EDGE_CURVE ( 'NONE', #38861, #28445, #33451, .T. ) ;
#38419 = ORIENTED_EDGE ( 'NONE', *, *, #7894, .T. ) ;
#38420 = ITEM_DEFINED_TRANSFORMATION ( 'NONE', 'NONE', #37723,  #24966 ) ;
#38421 = CARTESIAN_POINT ( 'NONE',  ( -25.68170654058536329, 11.85933282897061503, 6.451667499124866367 ) ) ;
#38422 = CARTESIAN_POINT ( 'NONE',  ( -13.91099446267133999, -33.59051099066034851, 9.908177736482725706 ) ) ;
#38423 = CARTESIAN_POINT ( 'NONE',  ( -27.45775109278351067, 25.00000000000000000, -8.471355351200609007 ) ) ;
#38424 = B_SPLINE_CURVE_WITH_KNOTS ( 'NONE', 3,
 ( #63352, #34074, #48093, #43736, #64017, #54392, #2549, #23130, #17816, #18504, #43395, #3535, #63670, #23809, #13157, #53731, #38756, #8825, #59056, #29114 ),
 .UNSPECIFIED., .F., .F.,
 ( 4, 2, 2, 2, 2, 2, 2, 2, 2, 4 ),
 ( 0.000000000000000000, 0.0008473511760410093376, 0.001694702352082018675, 0.002118377940102530825, 0.002542053528123043842, 0.003389404704164079418, 0.004236755880205114559, 0.005084107056246151002, 0.005931458232287185710, 0.006778809408328222152 ),
 .UNSPECIFIED. ) ;
#38425 = DIRECTION ( 'NONE',  ( 0.000000000000000000, -0.9105187689795999351, 0.4134677391718417638 ) ) ;
#38426 = CARTESIAN_POINT ( 'NONE',  ( -28.15855999187489189, -3.461419147680624864, -23.80441447217193485 ) ) ;
#38427 = CARTESIAN_POINT ( 'NONE',  ( -27.08423923533013777, 0.8983804370399791628, -2.107995711831551322 ) ) ;
#38428 = ORIENTED_EDGE ( 'NONE', *, *, #11953, .T. ) ;
#38429 = DIRECTION ( 'NONE',  ( -1.000000000000000000, -1.836970198721029688E-16, 0.000000000000000000 ) ) ;
#38430 = CARTESIAN_POINT ( 'NONE',  ( 2.288423627607479194, 5.755330594805035282, -5.039850887180206129 ) ) ;
#38431 = DIRECTION ( 'NONE',  ( -1.000000000000000000, 0.000000000000000000, 0.000000000000000000 ) ) ;
#38432 = EDGE_LOOP ( 'NONE', ( #14890, #10361, #23226, #4160 ) ) ;
#38433 = DIRECTION ( 'NONE',  ( 1.000000000000000000, 0.000000000000000000, 0.000000000000000000 ) ) ;
#38434 = EDGE_CURVE ( 'NONE', #16649, #54027, #15180, .T. ) ;
#38435 = EDGE_LOOP ( 'NONE', ( #27849, #59382, #60424, #8287 ) ) ;
#38436 = CARTESIAN_POINT ( 'NONE',  ( -18.25006854224444908, -9.443202773001939221, 25.00000000000000000 ) ) ;
#38437 = CARTESIAN_POINT ( 'NONE',  ( 2.406456491625949656, -8.704497555693093247, 5.751891873091646623 ) ) ;
#38438 = CARTESIAN_POINT ( 'NONE',  ( 3.152665057734040488, 0.000000000000000000, 0.000000000000000000 ) ) ;
#38439 = EDGE_CURVE ( 'NONE', #27786, #44289, #3508, .T. ) ;
#38440 = VECTOR ( 'NONE', #31451, 1000.000000000000000 ) ;
#38441 = DIRECTION ( 'NONE',  ( 0.000000000000000000, 0.8169148498130295311, -0.5767582926624942319 ) ) ;
#38442 = DIRECTION ( 'NONE',  ( 1.000000000000000000, 0.000000000000000000, 0.000000000000000000 ) ) ;
#38443 = VECTOR ( 'NONE', #50013, 1000.000000000000000 ) ;
#38444 = DIRECTION ( 'NONE',  ( -1.000000000000000000, -0.000000000000000000, -0.000000000000000000 ) ) ;
#38445 = ORIENTED_EDGE ( 'NONE', *, *, #20716, .T. ) ;
#38446 =( BOUNDED_SURFACE ( )  B_SPLINE_SURFACE ( 3, 1, ( 
 ( #2136, #5848 ),
 ( #47379, #21099 ),
 ( #17098, #12106 ),
 ( #26108, #11448 ) ),
 .UNSPECIFIED., .F., .F., .F. ) 
 B_SPLINE_SURFACE_WITH_KNOTS ( ( 4, 4 ),
 ( 2, 2 ),
 ( 0.000000000000000000, 1.000000000000000000 ),
 ( 0.000000000000000000, 1.000000000000000000 ),
 .UNSPECIFIED. ) 
 GEOMETRIC_REPRESENTATION_ITEM ( )  RATIONAL_B_SPLINE_SURFACE ( (
 ( 1.000000000000000000, 1.000000000000000000),
 ( 0.9942764183789327692, 0.8450855930916585379),
 ( 0.9942764183789327692, 0.8450855930916585379),
 ( 1.000000000000000000, 1.000000000000000000) ) ) 
 REPRESENTATION_ITEM ( '' )  SURFACE ( )  );
#38447 = DIRECTION ( 'NONE',  ( -1.000000000000000000, 0.000000000000000000, 0.000000000000000000 ) ) ;
#38448 = ORIENTED_EDGE ( 'NONE', *, *, #45956, .F. ) ;
#38449 = CARTESIAN_POINT ( 'NONE',  ( 0.6511581176957895734, 3.919972364658811603, 11.73752429815098886 ) ) ;
#38450 = CARTESIAN_POINT ( 'NONE',  ( 2.969415267404872161, 4.760005747566406598, -6.276215141898866534 ) ) ;
#38451 = DIRECTION ( 'NONE',  ( 0.000000000000000000, -0.01356324068817991828, 0.9999080150203990547 ) ) ;
#38452 = VECTOR ( 'NONE', #10063, 1000.000000000000000 ) ;
#38453 = ADVANCED_FACE ( 'NONE', ( #44044 ), #54022, .T. ) ;
#38454 = VERTEX_POINT ( 'NONE', #64315 ) ;
#38455 = FACE_OUTER_BOUND ( 'NONE', #61911, .T. ) ;
#38456 = EDGE_CURVE ( 'NONE', #32332, #62269, #23650, .T. ) ;
#38457 = ORIENTED_EDGE ( 'NONE', *, *, #64368, .F. ) ;
#38458 = CARTESIAN_POINT ( 'NONE',  ( 0.3654063281920739148, 7.689576266239796176, -9.573804659448589049 ) ) ;
#38459 = CARTESIAN_POINT ( 'NONE',  ( 5.515188684475870851, -0.002355816063606842176, 0.004804816249379301012 ) ) ;
#38460 = AXIS2_PLACEMENT_3D ( 'NONE', #11671, #21327, #32593 ) ;
#38461 = EDGE_CURVE ( 'NONE', #65063, #64384, #23205, .T. ) ;
#38462 = CARTESIAN_POINT ( 'NONE',  ( -27.08704841010922948, -2.081152044925736355, -0.9786466045375251666 ) ) ;
#38463 = CARTESIAN_POINT ( 'NONE',  ( 3.152665057736163678, 7.923639299009212600, -0.4801242025614006481 ) ) ;
#38464 = ORIENTED_EDGE ( 'NONE', *, *, #38746, .F. ) ;
#38465 = CARTESIAN_POINT ( 'NONE',  ( 0.2653519991613825790, -6.104031847944945355, -10.61652626436034730 ) ) ;
#38466 = CARTESIAN_POINT ( 'NONE',  ( -22.28284753389937478, -2.590196335759710422, 2.640101649307533105 ) ) ;
#38467 = CARTESIAN_POINT ( 'NONE',  ( 2.524535260912932344, -1.123794384998863416, 7.646662375930550759 ) ) ;
#38468 = LINE ( 'NONE', #55310, #45523 ) ;
#38469 = CARTESIAN_POINT ( 'NONE',  ( 2.251152103363648127, -0.1252683866804617796, -7.636644423939539905 ) ) ;
#38470 = AXIS2_PLACEMENT_3D ( 'NONE', #62720, #6893, #1250 ) ;
#38471 = DIRECTION ( 'NONE',  ( 1.000000000000000000, 0.000000000000000000, -0.000000000000000000 ) ) ;
#38472 = ORIENTED_EDGE ( 'NONE', *, *, #8248, .T. ) ;
#38473 = LINE ( 'NONE', #28488, #28013 ) ;
#38474 = CARTESIAN_POINT ( 'NONE',  ( 5.514624014163232779, -0.001574979445069392804, -0.003830004412313170285 ) ) ;
#38475 = CARTESIAN_POINT ( 'NONE',  ( -1.046707184715866212, -25.73493584727765082, -15.64955084339668012 ) ) ;
#38476 = VERTEX_POINT ( 'NONE', #6430 ) ;
#38477 = LINE ( 'NONE', #59110, #40812 ) ;
#38478 = DIRECTION ( 'NONE',  ( 0.000000000000000000, -0.01356324068817998940, 0.9999080150203990547 ) ) ;
#38479 = CARTESIAN_POINT ( 'NONE',  ( 18.46655499260420541, -7.261936723394225801, 11.40458322575580752 ) ) ;
#38480 = AXIS2_PLACEMENT_3D ( 'NONE', #56232, #10674, #26309 ) ;
#38481 = DIRECTION ( 'NONE',  ( -1.000000000000000000, 0.000000000000000000, 0.000000000000000000 ) ) ;
#38482 = CARTESIAN_POINT ( 'NONE',  ( 0.3109076770649024657, -11.43910935267335383, 4.414555973477779283 ) ) ;
#38483 = AXIS2_PLACEMENT_3D ( 'NONE', #34702, #9430, #3842 ) ;
#38484 = AXIS2_PLACEMENT_3D ( 'NONE', #39622, #29319, #44278 ) ;
#38485 = ORIENTED_EDGE ( 'NONE', *, *, #38722, .F. ) ;
#38486 = PLANE ( 'NONE',  #19144 ) ;
#38487 = EDGE_LOOP ( 'NONE', ( #34874, #3207, #28032, #26318 ) ) ;
#38488 = CARTESIAN_POINT ( 'NONE',  ( -22.65999102136916221, 0.5917351393135550364, -4.797155153747068468 ) ) ;
#38489 = EDGE_CURVE ( 'NONE', #54691, #4335, #30691, .T. ) ;
#38490 = DIRECTION ( 'NONE',  ( 0.000000000000000000, -0.01356324068817998940, 0.9999080150203990547 ) ) ;
#38491 = CARTESIAN_POINT ( 'NONE',  ( -35.00000000000000000, 11.72397916322013600, -0.7214809346827312231 ) ) ;
#38492 = CARTESIAN_POINT ( 'NONE',  ( -27.32337605527165891, 0.3676050637290936285, -2.988381643048341196 ) ) ;
#38493 = CARTESIAN_POINT ( 'NONE',  ( 35.00000000000000000, -2.772148766916200380, -11.86701198550355585 ) ) ;
#38494 = DIRECTION ( 'NONE',  ( 0.000000000000000000, -0.8835120444460178302, -0.4684084406997996997 ) ) ;
#38495 = CARTESIAN_POINT ( 'NONE',  ( 2.247112776671466250, -1.211104213045427258, 7.539676020705981863 ) ) ;
#38496 = FACE_OUTER_BOUND ( 'NONE', #53766, .T. ) ;
#38497 = VERTEX_POINT ( 'NONE', #55979 ) ;
#38498 = ORIENTED_EDGE ( 'NONE', *, *, #35820, .T. ) ;
#38499 = ORIENTED_EDGE ( 'NONE', *, *, #16749, .F. ) ;
#38500 = CARTESIAN_POINT ( 'NONE',  ( 2.941278708680199916, 2.952340773940184349, -5.383216837018909295 ) ) ;
#38501 = CARTESIAN_POINT ( 'NONE',  ( -27.28563798457901513, 0.04047623855284777222, -2.896153581097040242 ) ) ;
#38502 = CARTESIAN_POINT ( 'NONE',  ( -22.28939870658739864, -1.608176106660549554, 3.352428181135941987 ) ) ;
#38503 = ORIENTED_EDGE ( 'NONE', *, *, #61127, .F. ) ;
#38504 = CARTESIAN_POINT ( 'NONE',  ( 36.00000000000000711, 12.73293890771483916, 0.6593684648219062527 ) ) ;
#38505 = AXIS2_PLACEMENT_3D ( 'NONE', #47030, #21075, #1489 ) ;
#38506 = CARTESIAN_POINT ( 'NONE',  ( 0.000000000000000000, -30.00000000000000000, -15.00000000000000000 ) ) ;
#38507 = LINE ( 'NONE', #52826, #12730 ) ;
#38508 = ORIENTED_EDGE ( 'NONE', *, *, #14457, .F. ) ;
#38509 = AXIS2_PLACEMENT_3D ( 'NONE', #11840, #6549, #5917 ) ;
#38510 = VERTEX_POINT ( 'NONE', #41664 ) ;
#38511 = DIRECTION ( 'NONE',  ( -1.000000000000000000, 0.000000000000000000, 0.000000000000000000 ) ) ;
#38512 = EDGE_CURVE ( 'NONE', #56181, #59691, #43857, .T. ) ;
#38513 = ORIENTED_EDGE ( 'NONE', *, *, #9583, .F. ) ;
#38514 = CARTESIAN_POINT ( 'NONE',  ( 1.000000000000000888, 5.662015959325264802, -4.918493191653922736 ) ) ;
#38515 = ORIENTED_EDGE ( 'NONE', *, *, #63802, .T. ) ;
#38516 = VERTEX_POINT ( 'NONE', #41325 ) ;
#38517 = LINE ( 'NONE', #63767, #39457 ) ;
#38518 = EDGE_CURVE ( 'NONE', #33298, #53158, #37446, .T. ) ;
#38519 = DIRECTION ( 'NONE',  ( -1.000000000000000000, 0.000000000000000000, -0.000000000000000000 ) ) ;
#38520 = CARTESIAN_POINT ( 'NONE',  ( -27.10128162969864007, -2.337214317750536008, 0.1566844438592054634 ) ) ;
#38521 = DIRECTION ( 'NONE',  ( 0.000000000000000000, 0.01356324068817991828, -0.9999080150203990547 ) ) ;
#38522 = DIRECTION ( 'NONE',  ( -0.000000000000000000, 1.000000000000000000, -0.000000000000000000 ) ) ;
#38523 = B_SPLINE_CURVE_WITH_KNOTS ( 'NONE', 3,
 ( #13696, #33981, #44288, #59274, #54633, #24029, #3440, #59599, #43976, #63577, #64559, #39296, #53643, #3101, #8081, #28670, #14027, #54295, #7751 ),
 .UNSPECIFIED., .F., .F.,
 ( 4, 3, 3, 3, 3, 3, 4 ),
 ( 1.029150036413375294E-17, 4.457896483014832405E-05, 6.639290541541954295E-05, 8.820687556478702977E-05, 0.0001100173248778896191, 0.0001545671401658089039, 0.0001830328308068576552 ),
 .UNSPECIFIED. ) ;
#38524 = CARTESIAN_POINT ( 'NONE',  ( 0.2801149460245108691, 11.57793225195137055, 4.005169813315148097 ) ) ;
#38525 = AXIS2_PLACEMENT_3D ( 'NONE', #55994, #26725, #51018 ) ;
#38526 = ORIENTED_EDGE ( 'NONE', *, *, #63145, .T. ) ;
#38527 = LINE ( 'NONE', #63453, #37035 ) ;
#38528 = CYLINDRICAL_SURFACE ( 'NONE', #16391, 4.999999999999999112 ) ;
#38529 = CARTESIAN_POINT ( 'NONE',  ( 0.2652384529303155047, -9.338494547402444113, 7.922180393770638318 ) ) ;
#38530 = DIRECTION ( 'NONE',  ( -1.000000000000000000, 0.000000000000000000, 0.000000000000000000 ) ) ;
#38532 = DIRECTION ( 'NONE',  ( 0.000000000000000000, -0.4134677391718386552, -0.9105187689796012673 ) ) ;
#38531 = VECTOR ( 'NONE', #10747, 999.9999999999998863 ) ;
#38533 = FACE_OUTER_BOUND ( 'NONE', #7111, .T. ) ;
#38534 = CARTESIAN_POINT ( 'NONE',  ( -27.08421723179412410, 1.556274442127719704, 1.681635392574617693 ) ) ;
#38535 = DIRECTION ( 'NONE',  ( 0.000000000000000000, 0.01356324068817998940, -0.9999080150203990547 ) ) ;
#38536 = VECTOR ( 'NONE', #49792, 1000.000000000000114 ) ;
#38537 = CARTESIAN_POINT ( 'NONE',  ( -27.16343335735464137, -10.63351257863160626, -8.317934404008965998 ) ) ;
#38538 = EDGE_CURVE ( 'NONE', #44248, #49332, #51002, .T. ) ;
#38539 = AXIS2_PLACEMENT_3D ( 'NONE', #62651, #15790, #539 ) ;
#38540 = VECTOR ( 'NONE', #16334, 1000.000000000000000 ) ;
#38541 = VERTEX_POINT ( 'NONE', #46018 ) ;
#38542 = CARTESIAN_POINT ( 'NONE',  ( -37.00000000000000711, 11.74226168163341555, 0.3025107581131598611 ) ) ;
#38543 = ORIENTED_EDGE ( 'NONE', *, *, #26026, .F. ) ;
#38544 = DIRECTION ( 'NONE',  ( 0.000000000000000000, 0.6745969609292663538, 0.7381862504171949890 ) ) ;
#38545 = CARTESIAN_POINT ( 'NONE',  ( -16.02919692786944239, -28.24921752684737086, -10.30002093107130356 ) ) ;
#38546 = CARTESIAN_POINT ( 'NONE',  ( 12.52917170697542737, -11.52224091069466638, -7.043940186100077661 ) ) ;
#38547 = VECTOR ( 'NONE', #51402, 1000.000000000000000 ) ;
#38548 = FACE_OUTER_BOUND ( 'NONE', #18369, .T. ) ;
#38549 = CARTESIAN_POINT ( 'NONE',  ( 0.000000000000000000, -45.00000000000000000, 0.000000000000000000 ) ) ;
#38550 = ORIENTED_EDGE ( 'NONE', *, *, #37819, .T. ) ;
#38551 = AXIS2_PLACEMENT_3D ( 'NONE', #29955, #14331, #5031 ) ;
#38552 = CARTESIAN_POINT ( 'NONE',  ( 2.000000000000001776, 1.693411908627200146, 7.306323022404582979 ) ) ;
#38553 = DIRECTION ( 'NONE',  ( -1.000000000000000000, -0.000000000000000000, 0.000000000000000000 ) ) ;
#38554 = DIRECTION ( 'NONE',  ( -1.000000000000000000, 0.000000000000000000, -0.000000000000000000 ) ) ;
#38555 = FACE_OUTER_BOUND ( 'NONE', #50747, .T. ) ;
#38556 = ADVANCED_FACE ( 'NONE', ( #56299 ), #474, .T. ) ;
#38557 = AXIS2_PLACEMENT_3D ( 'NONE', #38491, #59423, #48171 ) ;
#38558 = DIRECTION ( 'NONE',  ( 0.000000000000000000, 0.000000000000000000, 1.000000000000000000 ) ) ;
#38559 = EDGE_LOOP ( 'NONE', ( #45934, #65169, #51933, #33274 ) ) ;
#38560 = VECTOR ( 'NONE', #63363, 1000.000000000000000 ) ;
#38561 = CYLINDRICAL_SURFACE ( 'NONE', #58355, 2.899999999999994582 ) ;
#38562 = CARTESIAN_POINT ( 'NONE',  ( -37.00000000000000711, -8.534258022646161734, 8.699265615722952205 ) ) ;
#38563 = LINE ( 'NONE', #53867, #31985 ) ;
#38564 = AXIS2_PLACEMENT_3D ( 'NONE', #26640, #2030, #22651 ) ;
#38565 = ORIENTED_EDGE ( 'NONE', *, *, #58200, .F. ) ;
#38566 = ORIENTED_EDGE ( 'NONE', *, *, #61493, .T. ) ;
#38567 = DIRECTION ( 'NONE',  ( -1.000000000000000000, 0.000000000000000000, 0.000000000000000000 ) ) ;
#38569 = ORIENTED_EDGE ( 'NONE', *, *, #25038, .F. ) ;
#38568 = EDGE_CURVE ( 'NONE', #37953, #36795, #32114, .T. ) ;
#38570 = CARTESIAN_POINT ( 'NONE',  ( 2.251152103363437185, 5.004701566804899748, 5.769488058190947122 ) ) ;
#38571 = CARTESIAN_POINT ( 'NONE',  ( 2.507146904658099196, -3.672650549645619211, -6.793847219607487276 ) ) ;
#38572 = CARTESIAN_POINT ( 'NONE',  ( -25.00000000000000355, -30.00000000000000000, 24.00000000000000000 ) ) ;
#38573 = CARTESIAN_POINT ( 'NONE',  ( 0.3006302518452059758, 9.243299516615135047, -8.051021221755679136 ) ) ;
#38574 = CARTESIAN_POINT ( 'NONE',  ( 5.530133899448235191, -0.01111090067015095897, 0.01149180883054541115 ) ) ;
#38575 = ADVANCED_FACE ( 'NONE', ( #31035 ), #51346, .T. ) ;
#38576 = ORIENTED_EDGE ( 'NONE', *, *, #47300, .T. ) ;
#38577 = AXIS2_PLACEMENT_3D ( 'NONE', #63108, #22208, #48487 ) ;
#38578 = VECTOR ( 'NONE', #41037, 1000.000000000000000 ) ;
#38579 = EDGE_LOOP ( 'NONE', ( #8533, #21237, #25100, #9117 ) ) ;
#38580 = ORIENTED_EDGE ( 'NONE', *, *, #45484, .T. ) ;
#38581 = CARTESIAN_POINT ( 'NONE',  ( 5.516018279890452902, -0.005331956019561440684, -0.004180585980734585240 ) ) ;
#38582 = AXIS2_PLACEMENT_3D ( 'NONE', #10096, #25381, #24395 ) ;
#38584 = AXIS2_PLACEMENT_3D ( 'NONE', #41251, #36267, #6045 ) ;
#38583 = DIRECTION ( 'NONE',  ( -1.000000000000000000, 0.000000000000000000, 0.000000000000000000 ) ) ;
#38585 = EDGE_CURVE ( 'NONE', #31676, #56666, #31090, .T. ) ;
#38586 = ORIENTED_EDGE ( 'NONE', *, *, #41270, .F. ) ;
#38587 = DIRECTION ( 'NONE',  ( 0.000000000000000000, -0.01356324068817999808, 0.9999080150203990547 ) ) ;
#38588 = CARTESIAN_POINT ( 'NONE',  ( 2.827825597296802496, -8.073505504738395899, 4.031992772938967740 ) ) ;
#38589 = ORIENTED_EDGE ( 'NONE', *, *, #37638, .T. ) ;
#38590 = CARTESIAN_POINT ( 'NONE',  ( 2.931247277082684288, 7.255238984871627217, 3.034789039497215679 ) ) ;
#38591 = CARTESIAN_POINT ( 'NONE',  ( 22.05618987420085020, -11.97361567146970529, -0.7978078888370666588 ) ) ;
#38592 = DIRECTION ( 'NONE',  ( 0.000000000000000000, -0.01356324068817998940, 0.9999080150203990547 ) ) ;
#38593 = VERTEX_POINT ( 'NONE', #7743 ) ;
#38594 = AXIS2_PLACEMENT_3D ( 'NONE', #445, #20715, #40989 ) ;
#38595 = VERTEX_POINT ( 'NONE', #52956 ) ;
#38596 = CARTESIAN_POINT ( 'NONE',  ( 2.262775599886257538, 2.480428346600533906, 7.227769107232051127 ) ) ;
#38597 = ORIENTED_EDGE ( 'NONE', *, *, #36510, .F. ) ;
#38598 = ADVANCED_FACE ( 'NONE', ( #28028 ), #23037, .T. ) ;
#38599 = CARTESIAN_POINT ( 'NONE',  ( 8.938435699493556541, 2.394065638922180828, -13.28818146251820309 ) ) ;
#38600 = VERTEX_POINT ( 'NONE', #43293 ) ;
#38601 = AXIS2_PLACEMENT_3D ( 'NONE', #61206, #1690, #37227 ) ;
#38602 = CARTESIAN_POINT ( 'NONE',  ( 0.2653519890518156177, -4.188437879978335054, 11.50766430042468080 ) ) ;
#38603 = CARTESIAN_POINT ( 'NONE',  ( 0.2653519789438770204, 11.51519617080780655, 4.167744179923950298 ) ) ;
#38604 = CARTESIAN_POINT ( 'NONE',  ( -15.60798173055017912, -34.17470894020297578, -7.727686298000182141 ) ) ;
#38605 = DIRECTION ( 'NONE',  ( 1.000000000000000000, 0.000000000000000000, 0.000000000000000000 ) ) ;
#38606 = CARTESIAN_POINT ( 'NONE',  ( 35.00000000000000000, -3.640372113593464576, 12.21925492305365246 ) ) ;
#38607 = CARTESIAN_POINT ( 'NONE',  ( -22.49803948133826736, -4.343047530463636896, 0.1132714802761758260 ) ) ;
#38608 = ORIENTED_EDGE ( 'NONE', *, *, #15156, .T. ) ;
#38609 = CARTESIAN_POINT ( 'NONE',  ( 35.00000000000000000, 4.705694406421931860E-17, -3.469127814946512892E-15 ) ) ;
#38610 = CIRCLE ( 'NONE', #9932, 12.18650000000000055 ) ;
#38611 = VERTEX_POINT ( 'NONE', #38307 ) ;
#38612 = CARTESIAN_POINT ( 'NONE',  ( 2.276198483117258142, -2.759333101207195327, 7.130755363255154577 ) ) ;
#38613 = CIRCLE ( 'NONE', #15242, 12.18650000000000055 ) ;
#38614 = FACE_OUTER_BOUND ( 'NONE', #27504, .T. ) ;
#38615 = ORIENTED_EDGE ( 'NONE', *, *, #54431, .F. ) ;
#38616 = CARTESIAN_POINT ( 'NONE',  ( -16.08885787060327033, 8.362789014594929071, 8.606209290561983138 ) ) ;
#38617 = CARTESIAN_POINT ( 'NONE',  ( 0.3675815128205912052, 12.04510820461662668, -2.391755495700480516 ) ) ;
#38618 = CARTESIAN_POINT ( 'NONE',  ( 0.3223008802179305743, -2.370176598416255054, -12.03398982086836355 ) ) ;
#38619 = B_SPLINE_CURVE_WITH_KNOTS ( 'NONE', 3,
 ( #15949, #62823, #691, #46891, #31581, #56549, #36238, #6333, #31273, #6024, #1351, #51244, #21632, #41894, #26279, #32239 ),
 .UNSPECIFIED., .F., .F.,
 ( 4, 3, 3, 3, 3, 4 ),
 ( 8.673617379884034509E-19, 0.0002176109881720231839, 0.0004352086762394586066, 0.0006528017811446851226, 0.0007615147961451692411, 0.0009453342004947268718 ),
 .UNSPECIFIED. ) ;
#38620 = ORIENTED_EDGE ( 'NONE', *, *, #60275, .F. ) ;
#38621 = VECTOR ( 'NONE', #65158, 1000.000000000000000 ) ;
#38622 = ORIENTED_EDGE ( 'NONE', *, *, #8788, .F. ) ;
#38623 = CARTESIAN_POINT ( 'NONE',  ( 2.969415267404955650, -7.007431655063692588, -3.597837242549690284 ) ) ;
#38624 = ORIENTED_EDGE ( 'NONE', *, *, #61590, .T. ) ;
#38625 = DIRECTION ( 'NONE',  ( 0.000000000000000000, 0.000000000000000000, 1.000000000000000000 ) ) ;
#38626 = DIRECTION ( 'NONE',  ( 0.000000000000000000, 0.2618041379715563277, -0.9651210252299813330 ) ) ;
#38627 = DIRECTION ( 'NONE',  ( 0.000000000000000000, 1.000000000000000000, 0.000000000000000000 ) ) ;
#38628 = CARTESIAN_POINT ( 'NONE',  ( -2.532614230583026593, 5.020478806276888584, 10.89930238848911337 ) ) ;
#38629 = LINE ( 'NONE', #58942, #42685 ) ;
#38630 = ORIENTED_EDGE ( 'NONE', *, *, #63463, .T. ) ;
#38631 = VECTOR ( 'NONE', #53014, 1000.000000000000000 ) ;
#38632 = AXIS2_PLACEMENT_3D ( 'NONE', #17911, #39155, #54140 ) ;
#38633 = CARTESIAN_POINT ( 'NONE',  ( -35.00000000000000000, 0.000000000000000000, 0.000000000000000000 ) ) ;
#38634 = AXIS2_PLACEMENT_3D ( 'NONE', #16795, #21472, #46732 ) ;
#38635 = EDGE_CURVE ( 'NONE', #918, #46346, #2431, .T. ) ;
#38636 =( BOUNDED_SURFACE ( )  B_SPLINE_SURFACE ( 3, 1, ( 
 ( #3901, #19172 ),
 ( #23518, #33798 ),
 ( #13210, #54442 ),
 ( #13516, #28825 ) ),
 .UNSPECIFIED., .F., .F., .F. ) 
 B_SPLINE_SURFACE_WITH_KNOTS ( ( 4, 4 ),
 ( 2, 2 ),
 ( 0.000000000000000000, 1.000000000000000000 ),
 ( 0.000000000000000000, 1.000000000000000000 ),
 .UNSPECIFIED. ) 
 GEOMETRIC_REPRESENTATION_ITEM ( )  RATIONAL_B_SPLINE_SURFACE ( (
 ( 1.000000000000000000, 1.000000000000000000),
 ( 0.6933888150995267674, 0.9895912004443193632),
 ( 0.6933888150995267674, 0.9895912004443193632),
 ( 1.000000000000000000, 1.000000000000000000) ) ) 
 REPRESENTATION_ITEM ( '' )  SURFACE ( )  );
#38637 = CARTESIAN_POINT ( 'NONE',  ( -28.66013792860432119, -1.490739498621027836, 1.071635578228282482 ) ) ;
#38638 = AXIS2_PLACEMENT_3D ( 'NONE', #36496, #45819, #57117 ) ;
#38639 = DIRECTION ( 'NONE',  ( -1.000000000000000000, 0.000000000000000000, 0.000000000000000000 ) ) ;
#38640 = CARTESIAN_POINT ( 'NONE',  ( 35.00000000000000000, -2.936739658819788712, 11.37311665002366290 ) ) ;
#38641 = CARTESIAN_POINT ( 'NONE',  ( 35.00000000000000000, -11.96656215839371917, -4.400442035670902641 ) ) ;
#38642 = CARTESIAN_POINT ( 'NONE',  ( 0.000000000000000000, -6.586971819220345026, 3.586335490831356054 ) ) ;
#38643 = CARTESIAN_POINT ( 'NONE',  ( -22.30861784526116054, -2.737516124790392080, -2.600591904828418954 ) ) ;
#38644 = AXIS2_PLACEMENT_3D ( 'NONE', #59098, #9177, #24471 ) ;
#38645 = AXIS2_PLACEMENT_3D ( 'NONE', #46512, #7248, #41852 ) ;
#38646 = EDGE_CURVE ( 'NONE', #27477, #19993, #54454, .T. ) ;
#38647 = VERTEX_POINT ( 'NONE', #13051 ) ;
#38648 = CARTESIAN_POINT ( 'NONE',  ( 12.56381792447365164, -11.46152505571988556, -3.559530320152763938 ) ) ;
#38649 = VERTEX_POINT ( 'NONE', #12702 ) ;
#38651 =( BOUNDED_CURVE ( )  B_SPLINE_CURVE ( 3, ( #42692, #36743, #62993, #37728 ),
 .UNSPECIFIED., .F., .F. ) 
 B_SPLINE_CURVE_WITH_KNOTS ( ( 4, 4 ),
 ( 1.123686293514793100, 1.129014759054202566 ),
 .UNSPECIFIED. ) 
 CURVE ( )  GEOMETRIC_REPRESENTATION_ITEM ( )  RATIONAL_B_SPLINE_CURVE ( ( 1.000000000000000000, 0.9999976339559824012, 0.9999976339559824012, 1.000000000000000000 ) ) 
 REPRESENTATION_ITEM ( '' )  );
#38650 = CARTESIAN_POINT ( 'NONE',  ( 35.00000000000000000, 4.705694406421931860E-17, -3.469127814946512892E-15 ) ) ;
#38652 = EDGE_CURVE ( 'NONE', #7920, #3473, #28729, .T. ) ;
#38653 = DIRECTION ( 'NONE',  ( 1.000000000000000000, 0.000000000000000000, 0.000000000000000000 ) ) ;
#38654 = CARTESIAN_POINT ( 'NONE',  ( 22.00000000000000711, -20.00000000000000000, -1.499999999999998002 ) ) ;
#38655 = AXIS2_PLACEMENT_3D ( 'NONE', #37791, #17522, #7521 ) ;
#38656 = ORIENTED_EDGE ( 'NONE', *, *, #39099, .T. ) ;
#38657 = CARTESIAN_POINT ( 'NONE',  ( 0.2650492594609234476, -12.24562116224018382, -0.1101156276918037469 ) ) ;
#38658 = FACE_OUTER_BOUND ( 'NONE', #9136, .T. ) ;
#38659 = ADVANCED_FACE ( 'NONE', ( #57300 ), #62929, .T. ) ;
#38660 = ORIENTED_EDGE ( 'NONE', *, *, #40026, .F. ) ;
#38661 = ORIENTED_EDGE ( 'NONE', *, *, #37615, .T. ) ;
#38662 = VERTEX_POINT ( 'NONE', #32003 ) ;
#38663 = DIRECTION ( 'NONE',  ( 0.000000000000000000, -0.01356324068817999114, 0.9999080150203989437 ) ) ;
#38664 = CARTESIAN_POINT ( 'NONE',  ( -22.28939870658739864, -3.352428181135935326, -1.608176106660559768 ) ) ;
#38665 = VECTOR ( 'NONE', #58245, 1000.000000000000000 ) ;
#38666 = EDGE_CURVE ( 'NONE', #14988, #21432, #62075, .T. ) ;
#38667 = ORIENTED_EDGE ( 'NONE', *, *, #38876, .T. ) ;
#38668 = CARTESIAN_POINT ( 'NONE',  ( -35.00000000000000000, -10.92721691015459307, 4.309077947445612899 ) ) ;
#38669 = CARTESIAN_POINT ( 'NONE',  ( -35.00000000000000000, 6.036400161834567513, 10.07641281632180075 ) ) ;
#38670 = LINE ( 'NONE', #58974, #34419 ) ;
#38671 = DIRECTION ( 'NONE',  ( 0.000000000000000000, 0.000000000000000000, 1.000000000000000000 ) ) ;
#38672 = ORIENTED_EDGE ( 'NONE', *, *, #35330, .F. ) ;
#38673 = FACE_OUTER_BOUND ( 'NONE', #34235, .T. ) ;
#38674 = EDGE_CURVE ( 'NONE', #19282, #50607, #22038, .T. ) ;
#38675 = CARTESIAN_POINT ( 'NONE',  ( 18.18435566811206527, -28.78814669831782780, 7.856426167042674713 ) ) ;
#38676 = CARTESIAN_POINT ( 'NONE',  ( 2.251152103363647683, -1.449454666117681256, -7.498874008626772003 ) ) ;
#38678 = ORIENTED_EDGE ( 'NONE', *, *, #49379, .T. ) ;
#38677 = LINE ( 'NONE', #58981, #14883 ) ;
#38679 = CARTESIAN_POINT ( 'NONE',  ( 5.515188684475870851, -0.005140903460551146317, 0.001485678338381694451 ) ) ;
#38680 = VERTEX_POINT ( 'NONE', #52650 ) ;
#38681 = AXIS2_PLACEMENT_3D ( 'NONE', #40104, #562, #10843 ) ;
#38682 = DIRECTION ( 'NONE',  ( 0.000000000000000000, 0.9467777615094560284, 0.3218879778916007850 ) ) ;
#38683 = CIRCLE ( 'NONE', #37585, 4.999999999999998224 ) ;
#38684 = ORIENTED_EDGE ( 'NONE', *, *, #50955, .T. ) ;
#38685 = CARTESIAN_POINT ( 'NONE',  ( 2.241451721903216399, 7.194631024842675693, -2.553895636571864802 ) ) ;
#38686 = CARTESIAN_POINT ( 'NONE',  ( -35.04709527796842394, 0.005292201869334239861, 0.01117341439754379606 ) ) ;
#38687 = DIRECTION ( 'NONE',  ( 0.000000000000000000, -0.01356324068817998940, 0.9999080150203990547 ) ) ;
#38688 = DIRECTION ( 'NONE',  ( 1.000000000000000000, 0.000000000000000000, 0.000000000000000000 ) ) ;
#38689 = DIRECTION ( 'NONE',  ( 0.000000000000000000, 0.000000000000000000, 1.000000000000000000 ) ) ;
#38690 = CARTESIAN_POINT ( 'NONE',  ( -10.90165637462999548, -7.167514722546433070, -11.44751403622255026 ) ) ;
#38691 = CARTESIAN_POINT ( 'NONE',  ( 1.719304012341585253, 11.38834240361577521, -5.690355757825364513 ) ) ;
#38692 = EDGE_CURVE ( 'NONE', #21953, #21123, #7075, .T. ) ;
#38693 = ORIENTED_EDGE ( 'NONE', *, *, #45680, .F. ) ;
#38694 = CARTESIAN_POINT ( 'NONE',  ( -27.10719052120871098, -1.622102031466687189, 1.714424047991066846 ) ) ;
#38695 = EDGE_LOOP ( 'NONE', ( #3282, #7048, #57783, #39542 ) ) ;
#38696 = EDGE_CURVE ( 'NONE', #22365, #44, #37668, .T. ) ;
#38697 = ORIENTED_EDGE ( 'NONE', *, *, #12239, .F. ) ;
#38698 = CARTESIAN_POINT ( 'NONE',  ( 1.283627346226881683, 1.641214790177954352, -12.47820286973621506 ) ) ;
#38699 = CARTESIAN_POINT ( 'NONE',  ( 5.515188684475870851, -0.003154373509839927467, -0.004322737127823468931 ) ) ;
#38700 = FACE_OUTER_BOUND ( 'NONE', #34559, .T. ) ;
#38701 = CARTESIAN_POINT ( 'NONE',  ( 0.3632410797595190810, -10.49990774419906181, 6.365652464380866959 ) ) ;
#38702 = CARTESIAN_POINT ( 'NONE',  ( 0.2655924914740778742, -7.905499957109173970, -9.352877839710680874 ) ) ;
#38703 = VECTOR ( 'NONE', #16258, 1000.000000000000000 ) ;
#38704 = CARTESIAN_POINT ( 'NONE',  ( 2.241451721903216399, -7.507681056655368224, -1.385577012535832875 ) ) ;
#38705 = DIRECTION ( 'NONE',  ( 1.000000000000000000, -0.000000000000000000, -0.000000000000000000 ) ) ;
#38706 = EDGE_LOOP ( 'NONE', ( #37447, #41478, #39240, #60485 ) ) ;
#38707 = AXIS2_PLACEMENT_3D ( 'NONE', #26631, #37601, #12312 ) ;
#38708 = LINE ( 'NONE', #59009, #4232 ) ;
#38709 = CARTESIAN_POINT ( 'NONE',  ( 2.253265082352433168, -5.768060979107497488, -5.007416537586576233 ) ) ;
#38710 = CARTESIAN_POINT ( 'NONE',  ( -35.04660725145885891, -0.01184012236745385360, -0.003326400506043277784 ) ) ;
#38711 = EDGE_CURVE ( 'NONE', #29549, #59063, #24734, .T. ) ;
#38712 = CARTESIAN_POINT ( 'NONE',  ( 37.00000000000000711, -10.68873102412837639, 6.950793414699901085 ) ) ;
#38713 = DIRECTION ( 'NONE',  ( 0.000000000000000000, 0.2149704402110178270, 0.9766205557100881007 ) ) ;
#38714 = CIRCLE ( 'NONE', #10037, 6.936499999999988120 ) ;
#38715 = CARTESIAN_POINT ( 'NONE',  ( 2.241536586108912488, -2.617055111126402878, -7.171901127201320669 ) ) ;
#38716 = CARTESIAN_POINT ( 'NONE',  ( -9.572767838435238374, -3.704540188508917087, 12.98284452592227289 ) ) ;
#38717 = ORIENTED_EDGE ( 'NONE', *, *, #58437, .T. ) ;
#38718 = DIRECTION ( 'NONE',  ( -1.000000000000000000, 0.000000000000000000, -0.000000000000000000 ) ) ;
#38719 = AXIS2_PLACEMENT_3D ( 'NONE', #23445, #64975, #29099 ) ;
#38720 = DIRECTION ( 'NONE',  ( -1.000000000000000000, 0.000000000000000000, -0.000000000000000000 ) ) ;
#38721 = DIRECTION ( 'NONE',  ( 1.000000000000000000, -0.000000000000000000, 0.000000000000000000 ) ) ;
#38722 = EDGE_CURVE ( 'NONE', #13729, #18751, #63252, .T. ) ;
#38723 = ADVANCED_FACE ( 'NONE', ( #23355 ), #19693, .T. ) ;
#38724 = LINE ( 'NONE', #59025, #32015 ) ;
#38725 = FACE_OUTER_BOUND ( 'NONE', #35478, .T. ) ;
#38726 = AXIS2_PLACEMENT_3D ( 'NONE', #9166, #13496, #59726 ) ;
#38727 = ORIENTED_EDGE ( 'NONE', *, *, #7823, .T. ) ;
#38728 = CARTESIAN_POINT ( 'NONE',  ( -17.59845147210442917, 3.553096750747292809, 13.02522436870010303 ) ) ;
#38729 = B_SPLINE_CURVE_WITH_KNOTS ( 'NONE', 3,
 ( #39473, #58472, #59134, #8565, #28852, #49163, #59774 ),
 .UNSPECIFIED., .F., .F.,
 ( 4, 3, 4 ),
 ( 0.000000000000000000, 0.001700533616330544926, 0.005002426799371471715 ),
 .UNSPECIFIED. ) ;
#38730 = CARTESIAN_POINT ( 'NONE',  ( 0.2676618633000449332, -12.08777609394271657, 1.968216791520453368 ) ) ;
#38731 = CARTESIAN_POINT ( 'NONE',  ( -18.15462106490041094, 3.496563557764767793, -11.48178370015430083 ) ) ;
#38732 = VERTEX_POINT ( 'NONE', #24328 ) ;
#38733 = CARTESIAN_POINT ( 'NONE',  ( 0.2872850955227745917, 2.333231805482987475, 12.02931961709051834 ) ) ;
#38734 = CARTESIAN_POINT ( 'NONE',  ( 35.00000000000000000, -11.26103545359853264, 3.340853584269647847 ) ) ;
#38735 = ADVANCED_FACE ( 'NONE', ( #29325 ), #14350, .T. ) ;
#38736 = VERTEX_POINT ( 'NONE', #38654 ) ;
#38737 = AXIS2_PLACEMENT_3D ( 'NONE', #20931, #50563, #29929 ) ;
#38738 = ORIENTED_EDGE ( 'NONE', *, *, #45464, .T. ) ;
#38739 = CARTESIAN_POINT ( 'NONE',  ( 35.00000000000000000, 4.705694406421931860E-17, -3.469127814946512892E-15 ) ) ;
#38740 = AXIS2_PLACEMENT_3D ( 'NONE', #55759, #10191, #50767 ) ;
#38741 = ORIENTED_EDGE ( 'NONE', *, *, #4217, .F. ) ;
#38742 = CARTESIAN_POINT ( 'NONE',  ( -37.00000000000000711, 0.000000000000000000, 0.000000000000000000 ) ) ;
#38743 = CARTESIAN_POINT ( 'NONE',  ( -20.79170840334646542, -12.91784323155722269, -3.921648409140116698 ) ) ;
#38744 = FACE_OUTER_BOUND ( 'NONE', #8803, .T. ) ;
#38745 = FACE_OUTER_BOUND ( 'NONE', #20706, .T. ) ;
#38746 = EDGE_CURVE ( 'NONE', #1560, #10110, #49316, .T. ) ;
#38747 = DIRECTION ( 'NONE',  ( 1.000000000000000000, 0.000000000000000000, -0.000000000000000000 ) ) ;
#38749 = VERTEX_POINT ( 'NONE', #58961 ) ;
#38748 = PLANE ( 'NONE',  #22349 ) ;
#38750 = CARTESIAN_POINT ( 'NONE',  ( -35.00000000000000000, 0.7536123767500182424, -11.72195762423409171 ) ) ;
#38751 = EDGE_CURVE ( 'NONE', #65741, #19944, #65224, .T. ) ;
#38752 = VERTEX_POINT ( 'NONE', #28343 ) ;
#38753 = FACE_OUTER_BOUND ( 'NONE', #21148, .T. ) ;
#38754 = ORIENTED_EDGE ( 'NONE', *, *, #31472, .F. ) ;
#38755 = EDGE_LOOP ( 'NONE', ( #31047, #29581, #32900, #17555 ) ) ;
#38756 = CARTESIAN_POINT ( 'NONE',  ( -18.43690493633051730, 6.168852665516345368, 12.01132493851507377 ) ) ;
#38757 = EDGE_CURVE ( 'NONE', #46798, #4318, #33658, .T. ) ;
#38758 = CARTESIAN_POINT ( 'NONE',  ( -15.30016555129190792, -29.00876116002328686, 11.22753712088974964 ) ) ;
#38759 = CARTESIAN_POINT ( 'NONE',  ( -3.161182887995629187, 5.208071662170946858, 10.84703524381376383 ) ) ;
#38760 = AXIS2_PLACEMENT_3D ( 'NONE', #59982, #40662, #5102 ) ;
#38761 = DIRECTION ( 'NONE',  ( -1.000000000000000000, -0.000000000000000000, -0.000000000000000000 ) ) ;
#38762 = DIRECTION ( 'NONE',  ( 1.000000000000000000, 0.000000000000000000, 0.000000000000000000 ) ) ;
#38763 = EDGE_CURVE ( 'NONE', #53630, #59129, #49381, .T. ) ;
#38764 = LINE ( 'NONE', #17504, #22454 ) ;
#38766 = ORIENTED_EDGE ( 'NONE', *, *, #55500, .T. ) ;
#38765 = EDGE_CURVE ( 'NONE', #56420, #38541, #5619, .T. ) ;
#38767 = CYLINDRICAL_SURFACE ( 'NONE', #41073, 4.999999999999999112 ) ;
#38768 = CARTESIAN_POINT ( 'NONE',  ( 35.00000000000000000, 4.705694406421931860E-17, -3.469127814946512892E-15 ) ) ;
#38769 = FACE_OUTER_BOUND ( 'NONE', #10139, .T. ) ;
#38770 = VERTEX_POINT ( 'NONE', #54626 ) ;
#38771 = EDGE_CURVE ( 'NONE', #15788, #3402, #14656, .T. ) ;
#38772 = CARTESIAN_POINT ( 'NONE',  ( -10.00000000000000178, 0.000000000000000000, 0.000000000000000000 ) ) ;
#38773 = MECHANICAL_DESIGN_GEOMETRIC_PRESENTATION_REPRESENTATION (  '', ( #48331 ), #56878 ) ;
#38774 = ORIENTED_EDGE ( 'NONE', *, *, #34808, .F. ) ;
#38775 = FACE_OUTER_BOUND ( 'NONE', #16849, .T. ) ;
#38776 = CARTESIAN_POINT ( 'NONE',  ( 35.00000000000000000, 4.237620530777968852, 11.42599468261424178 ) ) ;
#38777 = DIRECTION ( 'NONE',  ( 0.000000000000000000, -0.01356324068817992175, 0.9999080150203990547 ) ) ;
#38778 = CARTESIAN_POINT ( 'NONE',  ( -22.27704833740210333, 2.993786163585794746, -2.142029987820960102 ) ) ;
#38779 = DIRECTION ( 'NONE',  ( 0.000000000000000000, 0.000000000000000000, 1.000000000000000000 ) ) ;
#38780 = CARTESIAN_POINT ( 'NONE',  ( -35.00000000000000000, -10.14408668126209001, -5.921969905510467314 ) ) ;
#38781 = LINE ( 'NONE', #63371, #12059 ) ;
#38782 = VERTEX_POINT ( 'NONE', #38974 ) ;
#38783 = AXIS2_PLACEMENT_3D ( 'NONE', #14637, #48698, #65512 ) ;
#38784 = ORIENTED_EDGE ( 'NONE', *, *, #8928, .F. ) ;
#38785 = CARTESIAN_POINT ( 'NONE',  ( 0.000000000000000000, 0.000000000000000000, 0.000000000000000000 ) ) ;
#38786 = CARTESIAN_POINT ( 'NONE',  ( -35.00000000000000000, -10.01317267707891467, 6.946017217729903770 ) ) ;
#38787 = DIRECTION ( 'NONE',  ( 0.000000000000000000, 0.6051742151937610226, 0.7960930657056468629 ) ) ;
#38788 = AXIS2_PLACEMENT_3D ( 'NONE', #30633, #50944, #65548 ) ;
#38789 = ADVANCED_FACE ( 'NONE', ( #9346 ), #13691, .T. ) ;
#38790 = CARTESIAN_POINT ( 'NONE',  ( 2.350038591457881409, -1.210550722321041217, -10.55267716396152444 ) ) ;
#38791 = DIRECTION ( 'NONE',  ( 0.000000000000000000, 0.01356324068817998940, -0.9999080150203990547 ) ) ;
#38792 = CARTESIAN_POINT ( 'NONE',  ( -9.620557803072061986, -3.748754942421991920, -11.40376018319986606 ) ) ;
#38793 = CARTESIAN_POINT ( 'NONE',  ( 35.00000000000000000, 0.4353888892050056802, 11.73808581813437080 ) ) ;
#38794 = DIRECTION ( 'NONE',  ( -1.000000000000000000, 0.000000000000000000, 0.000000000000000000 ) ) ;
#38795 = CARTESIAN_POINT ( 'NONE',  ( 2.589278595513779813, -5.163950571302539316, -5.779442428606855309 ) ) ;
#38796 = VERTEX_POINT ( 'NONE', #54286 ) ;
#38797 = CARTESIAN_POINT ( 'NONE',  ( 35.00000000000000000, 4.705694406421931860E-17, -3.469127814946512892E-15 ) ) ;
#38798 = CARTESIAN_POINT ( 'NONE',  ( 19.28625800530496903, 6.413918128308424116, 11.87904264843580471 ) ) ;
#38799 = EDGE_CURVE ( 'NONE', #65794, #29543, #47000, .T. ) ;
#38800 = CARTESIAN_POINT ( 'NONE',  ( 5.530133899448235191, 0.001124651387254987358, -0.01594518557925582447 ) ) ;
#38801 = CARTESIAN_POINT ( 'NONE',  ( 35.00000000000000000, 1.591260454995240714, -12.08216339958901564 ) ) ;
#38802 = B_SPLINE_CURVE_WITH_KNOTS ( 'NONE', 3,
 ( #57548, #17637, #48242, #47885, #58529, #12293, #11967, #62498 ),
 .UNSPECIFIED., .F., .F.,
 ( 4, 2, 2, 4 ),
 ( 0.000000000000000000, 0.0003639104015149990413, 0.0007278208030299984080, 0.001455641606060001370 ),
 .UNSPECIFIED. ) ;
#38803 = AXIS2_PLACEMENT_3D ( 'NONE', #27015, #57276, #17023 ) ;
#38804 = CARTESIAN_POINT ( 'NONE',  ( 0.000000000000000000, -4.376687952327356079, 5.220963330856582374 ) ) ;
#38805 = CARTESIAN_POINT ( 'NONE',  ( 1.000000000000000888, 5.097042323172460421, 5.501832381651443171 ) ) ;
#38806 = ORIENTED_EDGE ( 'NONE', *, *, #9383, .T. ) ;
#38807 = CARTESIAN_POINT ( 'NONE',  ( 0.2655924914740778742, -7.838010948425109703, 9.409507842005998768 ) ) ;
#38808 = CARTESIAN_POINT ( 'NONE',  ( 1.937114397841935398, 11.53912442307255404, 5.620553190833015300 ) ) ;
#38809 = CARTESIAN_POINT ( 'NONE',  ( -8.761386526127953545, -26.55543068763903491, -14.32493309394703829 ) ) ;
#38810 = VERTEX_POINT ( 'NONE', #4741 ) ;
#38811 = CARTESIAN_POINT ( 'NONE',  ( 5.514970785353741078, -0.004324946436530291601, 0.001897634820904994845 ) ) ;
#38812 = DIRECTION ( 'NONE',  ( -1.000000000000000000, 0.000000000000000000, -0.000000000000000000 ) ) ;
#38813 = FACE_OUTER_BOUND ( 'NONE', #39051, .T. ) ;
#38814 = EDGE_CURVE ( 'NONE', #42534, #10290, #46582, .T. ) ;
#38815 = PRESENTATION_LAYER_ASSIGNMENT (  '', '', ( #63205 ) ) ;
#38816 = DIRECTION ( 'NONE',  ( -1.000000000000000000, 0.000000000000000000, -0.000000000000000000 ) ) ;
#38817 = CYLINDRICAL_SURFACE ( 'NONE', #45848, 5.000000000000000888 ) ;
#38818 = LINE ( 'NONE', #59117, #24450 ) ;
#38819 = EDGE_LOOP ( 'NONE', ( #44504, #4020, #45514, #48268 ) ) ;
#38820 = DIRECTION ( 'NONE',  ( -1.000000000000000000, 0.000000000000000000, 0.000000000000000000 ) ) ;
#38821 = CARTESIAN_POINT ( 'NONE',  ( -37.00000000000000711, 0.000000000000000000, 0.000000000000000000 ) ) ;
#38823 = CIRCLE ( 'NONE', #8070, 6.936499999999987232 ) ;
#38822 = CARTESIAN_POINT ( 'NONE',  ( -37.00000000000000711, -8.366449238204298311, -9.621072037177086145 ) ) ;
#38824 = CARTESIAN_POINT ( 'NONE',  ( 2.368238019615414025, -4.795442552788031776, 5.994627685103054660 ) ) ;
#38825 = CARTESIAN_POINT ( 'NONE',  ( -28.67667724226168602, -1.299025457479350054, 1.375746547601627956 ) ) ;
#38826 = LINE ( 'NONE', #38152, #49098 ) ;
#38827 = DIRECTION ( 'NONE',  ( 0.000000000000000000, -0.01356324068817999114, 0.9999080150203989437 ) ) ;
#38828 = FACE_OUTER_BOUND ( 'NONE', #50581, .T. ) ;
#38829 = ORIENTED_EDGE ( 'NONE', *, *, #46369, .F. ) ;
#38830 = ORIENTED_EDGE ( 'NONE', *, *, #42398, .F. ) ;
#38831 = CARTESIAN_POINT ( 'NONE',  ( 0.3665391374699464300, 12.13918562134721491, -1.872534962004675174 ) ) ;
#38833 = ORIENTED_EDGE ( 'NONE', *, *, #58159, .T. ) ;
#38832 = B_SPLINE_CURVE_WITH_KNOTS ( 'NONE', 3,
 ( #12296, #32562, #52873, #58196, #12615, #32892, #7995 ),
 .UNSPECIFIED., .F., .F.,
 ( 4, 3, 4 ),
 ( 7.997016289651561525E-15, 0.002398160485435674606, 0.005002426799388316747 ),
 .UNSPECIFIED. ) ;
#38834 = EDGE_CURVE ( 'NONE', #43665, #6221, #65050, .T. ) ;
#38835 = SHAPE_REPRESENTATION_RELATIONSHIP ( 'NONE' , 'NONE' ,  #29683, #4012 ) ;
#38836 = ADVANCED_FACE ( 'NONE', ( #40266 ), #10339, .T. ) ;
#38838 = DIRECTION ( 'NONE',  ( 1.000000000000000000, -0.000000000000000000, 0.000000000000000000 ) ) ;
#38837 = CIRCLE ( 'NONE', #10156, 4.999999999999999112 ) ;
#38839 = FACE_OUTER_BOUND ( 'NONE', #60408, .T. ) ;
#38840 = EDGE_CURVE ( 'NONE', #6120, #46319, #41585, .T. ) ;
#38841 = CARTESIAN_POINT ( 'NONE',  ( -22.29677679919927868, -1.633785040807699707, 3.364642266483119482 ) ) ;
#38842 = ORIENTED_EDGE ( 'NONE', *, *, #40611, .F. ) ;
#38843 = CARTESIAN_POINT ( 'NONE',  ( -35.00000000000000000, 7.474872387601008583, 9.060822531526074641 ) ) ;
#38844 =( BOUNDED_CURVE ( )  B_SPLINE_CURVE ( 3, ( #24842, #61071, #35767, #10506 ),
 .UNSPECIFIED., .F., .F. ) 
 B_SPLINE_CURVE_WITH_KNOTS ( ( 4, 4 ),
 ( 4.681958569418493532, 4.712388980384689674 ),
 .UNSPECIFIED. ) 
 CURVE ( )  GEOMETRIC_REPRESENTATION_ITEM ( )  RATIONAL_B_SPLINE_CURVE ( ( 1.000000000000000000, 0.9999228339960630763, 0.9999228339960630763, 1.000000000000000000 ) ) 
 REPRESENTATION_ITEM ( '' )  );
#38845 = DIRECTION ( 'NONE',  ( -1.000000000000000000, 0.000000000000000000, 0.000000000000000000 ) ) ;
#38846 = DIRECTION ( 'NONE',  ( 1.000000000000000000, -0.000000000000000000, -0.000000000000000000 ) ) ;
#38847 = ORIENTED_EDGE ( 'NONE', *, *, #21607, .F. ) ;
#38848 = EDGE_LOOP ( 'NONE', ( #48301, #51214, #57022, #50504 ) ) ;
#38849 = EDGE_CURVE ( 'NONE', #4057, #21447, #24731, .T. ) ;
#38850 = DIRECTION ( 'NONE',  ( 0.000000000000000000, 0.8835120444460240474, -0.4684084406997880423 ) ) ;
#38851 = DIRECTION ( 'NONE',  ( 0.000000000000000000, 0.000000000000000000, -1.000000000000000000 ) ) ;
#38852 = ORIENTED_EDGE ( 'NONE', *, *, #3057, .T. ) ;
#38853 = ORIENTED_EDGE ( 'NONE', *, *, #46090, .F. ) ;
#38854 = DIRECTION ( 'NONE',  ( -1.000000000000000000, 0.000000000000000000, 0.000000000000000000 ) ) ;
#38855 = DIRECTION ( 'NONE',  ( 0.000000000000000000, -0.01356324068817998940, 0.9999080150203990547 ) ) ;
#38856 = AXIS2_PLACEMENT_3D ( 'NONE', #10900, #31505, #23501 ) ;
#38857 = CARTESIAN_POINT ( 'NONE',  ( 0.3057689695767508153, 10.49983108339468707, -6.328747727191083250 ) ) ;
#38858 = CARTESIAN_POINT ( 'NONE',  ( 0.2759803524722234669, 8.018167820447629879, -9.260954523383658099 ) ) ;
#38859 = LINE ( 'NONE', #63774, #60336 ) ;
#38860 = LINE ( 'NONE', #44168, #61958 ) ;
#38861 = VERTEX_POINT ( 'NONE', #30615 ) ;
#38862 = CARTESIAN_POINT ( 'NONE',  ( 2.249013661412228249, -1.444210756221599556, 7.499157010299432713 ) ) ;
#38863 = CARTESIAN_POINT ( 'NONE',  ( -16.29237361052064870, 7.773568625800320042, 9.141951862542200047 ) ) ;
#38864 = CARTESIAN_POINT ( 'NONE',  ( 37.00000000000000711, -11.96656215839371917, -4.400442035670902641 ) ) ;
#38865 = CARTESIAN_POINT ( 'NONE',  ( -35.00000000000000000, -7.817610399097453922, -8.766823244862070652 ) ) ;
#38866 = CYLINDRICAL_SURFACE ( 'NONE', #22209, 12.74999999999999822 ) ;
#38867 = FACE_OUTER_BOUND ( 'NONE', #24951, .T. ) ;
#38868 = LINE ( 'NONE', #53179, #50004 ) ;
#38869 = DIRECTION ( 'NONE',  ( 1.000000000000000000, 0.000000000000000000, 0.000000000000000000 ) ) ;
#38870 = DIRECTION ( 'NONE',  ( -1.000000000000000000, 0.000000000000000000, -0.000000000000000000 ) ) ;
#38871 = PRODUCT_RELATED_PRODUCT_CATEGORY ( 'part', '', ( #19015 ) ) ;
#38872 = EDGE_CURVE ( 'NONE', #10229, #53826, #4567, .T. ) ;
#38873 = ORIENTED_EDGE ( 'NONE', *, *, #16502, .T. ) ;
#38874 = CARTESIAN_POINT ( 'NONE',  ( -35.00000000000000000, -8.830544224262881770, -9.196955404009390378 ) ) ;
#38875 = AXIS2_PLACEMENT_3D ( 'NONE', #16362, #1727, #12336 ) ;
#38876 = EDGE_CURVE ( 'NONE', #4358, #16416, #61875, .T. ) ;
#38877 = CIRCLE ( 'NONE', #49521, 12.74999999999999822 ) ;
#38878 = VERTEX_POINT ( 'NONE', #21307 ) ;
#38879 = DIRECTION ( 'NONE',  ( -1.000000000000000000, 0.000000000000000000, 0.000000000000000000 ) ) ;
#38880 = DIRECTION ( 'NONE',  ( 1.000000000000000000, 0.000000000000000000, 0.000000000000000000 ) ) ;
#38881 = CARTESIAN_POINT ( 'NONE',  ( 12.84947240711940530, -12.08188435868343902, -6.035714449063213749 ) ) ;
#38882 = DIRECTION ( 'NONE',  ( 1.000000000000000000, -0.000000000000000000, 0.000000000000000000 ) ) ;
#38883 = DIRECTION ( 'NONE',  ( -1.000000000000000000, 0.000000000000000000, 0.000000000000000000 ) ) ;
#38884 = EDGE_LOOP ( 'NONE', ( #10152, #47906, #59104, #50240 ) ) ;
#38885 = CYLINDRICAL_SURFACE ( 'NONE', #27146, 13.50000000000000178 ) ;
#38886 = CARTESIAN_POINT ( 'NONE',  ( 2.288423627607476529, -3.684511167348244243, 6.704349683466405807 ) ) ;
#38887 = ADVANCED_FACE ( 'NONE', ( #35281 ), #45937, .T. ) ;
#38888 = DIRECTION ( 'NONE',  ( -1.000000000000000000, -0.000000000000000000, -0.000000000000000000 ) ) ;
#38889 = CARTESIAN_POINT ( 'NONE',  ( -22.29195009621226831, 2.682867222693523956, 2.585382421603408698 ) ) ;
#38890 = AXIS2_PLACEMENT_3D ( 'NONE', #53980, #19056, #3469 ) ;
#38891 = DIRECTION ( 'NONE',  ( 1.000000000000000000, -0.000000000000000000, 0.000000000000000000 ) ) ;
#38892 = ORIENTED_EDGE ( 'NONE', *, *, #12685, .T. ) ;
#38893 = CARTESIAN_POINT ( 'NONE',  ( -18.76908574728738088, 11.99999999999999289, 0.6354707926302536336 ) ) ;
#38894 = ORIENTED_EDGE ( 'NONE', *, *, #22840, .T. ) ;
#38895 = CARTESIAN_POINT ( 'NONE',  ( 2.491965175173491698, 5.773748672881994892, -5.121563073453221371 ) ) ;
#38897 = EDGE_CURVE ( 'NONE', #60806, #28767, #10030, .T. ) ;
#38896 = CARTESIAN_POINT ( 'NONE',  ( -35.00000000000000000, 12.08216339958900676, 1.591260454995285789 ) ) ;
#38898 = ADVANCED_FACE ( 'NONE', ( #56222 ), #51265, .T. ) ;
#38899 = EDGE_CURVE ( 'NONE', #38611, #47989, #25314, .T. ) ;
#38900 = CARTESIAN_POINT ( 'NONE',  ( 6.623202313640009997, -7.527612111493656499, 11.20804235361907253 ) ) ;
#38901 = ORIENTED_EDGE ( 'NONE', *, *, #47328, .T. ) ;
#38902 = ORIENTED_EDGE ( 'NONE', *, *, #11536, .F. ) ;
#38903 = CARTESIAN_POINT ( 'NONE',  ( -27.22222364661110916, 10.76538614228702606, 5.304738902579495097 ) ) ;
#38904 = DIRECTION ( 'NONE',  ( 0.000000000000000000, -0.6745969609292717939, -0.7381862504171901040 ) ) ;
#38905 = DIRECTION ( 'NONE',  ( 0.000000000000000000, 0.01356324068817998940, -0.9999080150203989437 ) ) ;
#38906 = DIRECTION ( 'NONE',  ( 0.000000000000000000, 0.000000000000000000, 1.000000000000000000 ) ) ;
#38907 = CARTESIAN_POINT ( 'NONE',  ( 1.452237505248552996, -11.67686475128076573, -4.880303821311127166 ) ) ;
#38908 = CARTESIAN_POINT ( 'NONE',  ( -22.28629837673887693, -2.102970853432566845, -3.055064048018814482 ) ) ;
#38909 = ORIENTED_EDGE ( 'NONE', *, *, #11269, .T. ) ;
#38910 = ORIENTED_EDGE ( 'NONE', *, *, #7328, .T. ) ;
#38911 = VERTEX_POINT ( 'NONE', #40608 ) ;
#38912 = CARTESIAN_POINT ( 'NONE',  ( -35.00000000000000000, 0.000000000000000000, 0.000000000000000000 ) ) ;
#38913 = EDGE_CURVE ( 'NONE', #20840, #48378, #60901, .T. ) ;
#38914 = CARTESIAN_POINT ( 'NONE',  ( -28.85619398320021745, 3.750539801530000439, 11.39883551934754280 ) ) ;
#38915 = ORIENTED_EDGE ( 'NONE', *, *, #46453, .F. ) ;
#38916 = AXIS2_PLACEMENT_3D ( 'NONE', #15427, #35693, #25089 ) ;
#38917 = DIRECTION ( 'NONE',  ( -1.000000000000000000, 0.000000000000000000, -0.000000000000000000 ) ) ;
#38918 = EDGE_CURVE ( 'NONE', #27953, #54227, #20668, .T. ) ;
#38919 = CARTESIAN_POINT ( 'NONE',  ( 2.290907136833256530, -7.561169784528411597, 1.168459104840908314 ) ) ;
#38920 = ORIENTED_EDGE ( 'NONE', *, *, #62585, .F. ) ;
#38921 = AXIS2_PLACEMENT_3D ( 'NONE', #50596, #60891, #14339 ) ;
#38922 = CARTESIAN_POINT ( 'NONE',  ( 2.241506898688417682, 6.591904579673283138, -3.851253041557037182 ) ) ;
#38923 = CARTESIAN_POINT ( 'NONE',  ( 21.90174657591892071, -11.97747433400148864, -0.7349207973210698519 ) ) ;
#38924 = DIRECTION ( 'NONE',  ( -1.000000000000000000, 0.000000000000000000, 0.000000000000000000 ) ) ;
#38925 = ORIENTED_EDGE ( 'NONE', *, *, #33784, .F. ) ;
#38926 = ORIENTED_EDGE ( 'NONE', *, *, #24232, .F. ) ;
#38927 = CARTESIAN_POINT ( 'NONE',  ( 1.719304012341460908, 3.626341562669523011, -12.20344780066162649 ) ) ;
#38928 = UNCERTAINTY_MEASURE_WITH_UNIT (LENGTH_MEASURE( 1.000000000000000082E-05 ), #44450, 'distance_accuracy_value', 'NONE');
#38929 = EDGE_LOOP ( 'NONE', ( #49725, #58966, #56745, #38448 ) ) ;
#38930 = CARTESIAN_POINT ( 'NONE',  ( 35.00000000000000000, 4.705694406421931860E-17, -3.469127814946512892E-15 ) ) ;
#38931 = ORIENTED_EDGE ( 'NONE', *, *, #59047, .T. ) ;
#38932 = ORIENTED_EDGE ( 'NONE', *, *, #62229, .T. ) ;
#38933 = CARTESIAN_POINT ( 'NONE',  ( 2.261269890822074746, 3.699080366006695098, 6.685978463722140219 ) ) ;
#38934 = DIRECTION ( 'NONE',  ( 0.000000000000000000, -0.01356324068817992001, 0.9999080150203990547 ) ) ;
#38935 = CARTESIAN_POINT ( 'NONE',  ( -14.24371601685413502, -33.70914924250542555, -9.547107017903027071 ) ) ;
#38936 = LINE ( 'NONE', #33929, #46569 ) ;
#38937 = DIRECTION ( 'NONE',  ( -1.000000000000000000, 0.000000000000000000, 0.000000000000000000 ) ) ;
#38938 = CARTESIAN_POINT ( 'NONE',  ( 0.5572780756284594350, -0.3055340344620345872, 12.33974848088638687 ) ) ;
#38939 = VERTEX_POINT ( 'NONE', #15648 ) ;
#38940 = DIRECTION ( 'NONE',  ( -1.000000000000000000, 0.000000000000000000, 0.000000000000000000 ) ) ;
#38941 = VERTEX_POINT ( 'NONE', #35923 ) ;
#38942 = CYLINDRICAL_SURFACE ( 'NONE', #42280, 12.18649999999999878 ) ;
#38943 = DIRECTION ( 'NONE',  ( -1.000000000000000000, 0.000000000000000000, 0.000000000000000000 ) ) ;
#38944 = EDGE_LOOP ( 'NONE', ( #20685, #4650, #7683, #64990 ) ) ;
#38945 = CARTESIAN_POINT ( 'NONE',  ( -17.08212596820160556, 7.928502486991608755, 9.008165934404118502 ) ) ;
#38946 = DIRECTION ( 'NONE',  ( -1.000000000000000000, 0.000000000000000000, -0.000000000000000000 ) ) ;
#38947 = CARTESIAN_POINT ( 'NONE',  ( 2.844750968615431752, -7.651810733888697591, 1.686994672841962029 ) ) ;
#38948 = ORIENTED_EDGE ( 'NONE', *, *, #33472, .F. ) ;
#38949 = ORIENTED_EDGE ( 'NONE', *, *, #49379, .F. ) ;
#38950 = CARTESIAN_POINT ( 'NONE',  ( 2.263328370261528999, -7.640407877530317471, 0.1420109704215539170 ) ) ;
#38951 = ADVANCED_FACE ( 'NONE', ( #30953 ), #5716, .T. ) ;
#38952 = ORIENTED_EDGE ( 'NONE', *, *, #22426, .T. ) ;
#38953 = CYLINDRICAL_SURFACE ( 'NONE', #61443, 2.899999999999994582 ) ;
#38954 = PRESENTATION_STYLE_ASSIGNMENT (( #63545 ) ) ;
#38955 = CARTESIAN_POINT ( 'NONE',  ( -29.28424789664604333, 2.973701217869066049, 13.19321996469480318 ) ) ;
#38956 = DIRECTION ( 'NONE',  ( 0.1024315404614497965, 0.9947400562552481951, 0.000000000000000000 ) ) ;
#38957 = CARTESIAN_POINT ( 'NONE',  ( 1.372161826076366165, -9.274145586376226547, 8.551811013234654979 ) ) ;
#38958 = EDGE_LOOP ( 'NONE', ( #51919, #59840, #115, #22720 ) ) ;
#38959 = DIRECTION ( 'NONE',  ( -1.000000000000000000, -0.000000000000000000, 0.000000000000000000 ) ) ;
#38960 = CIRCLE ( 'NONE', #27272, 12.18650000000000055 ) ;
#38961 = CARTESIAN_POINT ( 'NONE',  ( 1.634816307075101838, 1.494046826342973588, 12.61459884933128350 ) ) ;
#38962 = EDGE_CURVE ( 'NONE', #19382, #53566, #33266, .T. ) ;
#38963 = CARTESIAN_POINT ( 'NONE',  ( 2.507146904658100528, -7.565123178000297877, -1.553587269793135217 ) ) ;
#38964 = CARTESIAN_POINT ( 'NONE',  ( 5.536195898058073439, 0.003145317580921152666, 0.007896796515810895062 ) ) ;
#38965 = CYLINDRICAL_SURFACE ( 'NONE', #59349, 2.899999999999994582 ) ;
#38966 = DIRECTION ( 'NONE',  ( -1.000000000000000000, 0.000000000000000000, 0.000000000000000000 ) ) ;
#38967 = CARTESIAN_POINT ( 'NONE',  ( 35.00000000000000000, 9.063649021438955344, -8.146229107149434157 ) ) ;
#38968 = CARTESIAN_POINT ( 'NONE',  ( 0.000000000000000000, 0.000000000000000000, 0.000000000000000000 ) ) ;
#38969 = ORIENTED_EDGE ( 'NONE', *, *, #13250, .T. ) ;
#38970 = LINE ( 'NONE', #47637, #36299 ) ;
#38971 = ORIENTED_EDGE ( 'NONE', *, *, #44921, .F. ) ;
#38972 = CARTESIAN_POINT ( 'NONE',  ( 37.00000000000000711, -10.32377448871663006, 6.475373545682407972 ) ) ;
#38973 = CARTESIAN_POINT ( 'NONE',  ( -22.27713295444592845, -3.580881989303324353, 0.8543895091636493078 ) ) ;
#38974 = CARTESIAN_POINT ( 'NONE',  ( 35.00000000000000000, 9.063649021438955344, -8.146229107149434157 ) ) ;
#38975 = DIRECTION ( 'NONE',  ( 0.000000000000000000, 0.01356324068817992175, -0.9999080150203990547 ) ) ;
#38976 = ORIENTED_EDGE ( 'NONE', *, *, #19020, .F. ) ;
#38977 = VERTEX_POINT ( 'NONE', #26302 ) ;
#38978 = EDGE_LOOP ( 'NONE', ( #27579, #16058, #59634, #43991 ) ) ;
#38979 = CARTESIAN_POINT ( 'NONE',  ( 36.00000000000000711, 12.74613886779084737, -0.3137578094509725357 ) ) ;
#38980 = ORIENTED_EDGE ( 'NONE', *, *, #1424, .F. ) ;
#38981 = CARTESIAN_POINT ( 'NONE',  ( -22.27721688985630522, -2.338410344701250310, -2.843753050855878151 ) ) ;
#38982 = CARTESIAN_POINT ( 'NONE',  ( 2.507146904658097863, -2.843654641958937912, 7.180414359940946234 ) ) ;
#38983 = CARTESIAN_POINT ( 'NONE',  ( 0.3341166715381306274, -9.234320413907852299, 8.078283863465467007 ) ) ;
#38984 = CARTESIAN_POINT ( 'NONE',  ( 47.00000000000000711, 4.705694406421931860E-17, -3.469127814946512892E-15 ) ) ;
#38985 = EDGE_LOOP ( 'NONE', ( #43017, #27744, #37182, #38576 ) ) ;
#38986 = CARTESIAN_POINT ( 'NONE',  ( -14.47334165536099881, 0.000000000000000000, 0.000000000000000000 ) ) ;
#38987 = AXIS2_PLACEMENT_3D ( 'NONE', #19068, #64592, #55287 ) ;
#38988 = LINE ( 'NONE', #12392, #25608 ) ;
#38989 = CARTESIAN_POINT ( 'NONE',  ( 2.273267844204867938, -1.476347988307422199, -7.501135923490795498 ) ) ;
#38991 = ORIENTED_EDGE ( 'NONE', *, *, #947, .F. ) ;
#38990 = DIRECTION ( 'NONE',  ( 0.000000000000000000, -6.883382752675980017E-15, 1.000000000000000000 ) ) ;
#38992 = CARTESIAN_POINT ( 'NONE',  ( 5.515188684475870851, -0.004804816249378844779, 0.002355816063606914167 ) ) ;
#38993 = ORIENTED_EDGE ( 'NONE', *, *, #22358, .F. ) ;
#38994 = DIRECTION ( 'NONE',  ( -1.000000000000000000, 0.000000000000000000, -0.000000000000000000 ) ) ;
#38995 = VERTEX_POINT ( 'NONE', #17649 ) ;
#38996 = CIRCLE ( 'NONE', #47507, 4.999999999999999112 ) ;
#38997 = DIRECTION ( 'NONE',  ( 1.000000000000000000, 0.000000000000000000, 0.000000000000000000 ) ) ;
#38998 = DIRECTION ( 'NONE',  ( 0.000000000000000000, 0.01356324068817998940, -0.9999080150203990547 ) ) ;
#38999 = CARTESIAN_POINT ( 'NONE',  ( 35.00000000000000000, 4.705694406421931860E-17, -3.469127814946512892E-15 ) ) ;
#39000 = CARTESIAN_POINT ( 'NONE',  ( 0.2915757698887279648, -3.989025639548713809, 11.58754481235185985 ) ) ;
#39001 = EDGE_CURVE ( 'NONE', #7923, #50600, #23694, .T. ) ;
#39002 = CARTESIAN_POINT ( 'NONE',  ( 3.152665057734040488, 0.000000000000000000, 0.000000000000000000 ) ) ;
#39003 = AXIS2_PLACEMENT_3D ( 'NONE', #242, #20515, #40800 ) ;
#39004 = CARTESIAN_POINT ( 'NONE',  ( -36.00000000000000711, 4.824807283154123105, 11.80185301892982608 ) ) ;
#39005 = DIRECTION ( 'NONE',  ( -1.000000000000000000, -1.836970198721029688E-16, -0.000000000000000000 ) ) ;
#39006 = ORIENTED_EDGE ( 'NONE', *, *, #27301, .T. ) ;
#39007 = CARTESIAN_POINT ( 'NONE',  ( -4.984433189575353751, -1.083073623696802379, 13.45752292036589637 ) ) ;
#39008 = ORIENTED_EDGE ( 'NONE', *, *, #23283, .T. ) ;
#39009 = ORIENTED_EDGE ( 'NONE', *, *, #36734, .F. ) ;
#39010 = CARTESIAN_POINT ( 'NONE',  ( 1.719304012341412724, 1.452142814149018690, -12.64775761152637301 ) ) ;
#39011 = CARTESIAN_POINT ( 'NONE',  ( -22.31213670151049300, 3.398324501467296699, 1.669817926839889388 ) ) ;
#39012 = DIRECTION ( 'NONE',  ( 0.000000000000000000, 0.000000000000000000, 1.000000000000000000 ) ) ;
#39013 = CARTESIAN_POINT ( 'NONE',  ( 0.3654063281920718609, -10.50027211615251588, 6.366443614636645876 ) ) ;
#39014 = DIRECTION ( 'NONE',  ( -1.000000000000000000, -0.000000000000000000, -0.000000000000000000 ) ) ;
#39015 = CARTESIAN_POINT ( 'NONE',  ( 0.3106921474978457942, 10.73438344699978764, -5.925601485921557554 ) ) ;
#39016 = EDGE_CURVE ( 'NONE', #33099, #61338, #56638, .T. ) ;
#39017 = CARTESIAN_POINT ( 'NONE',  ( 35.00000000000000000, -11.56998259273180274, -3.827046518385039064 ) ) ;
#39018 = SHAPE_REPRESENTATION ( 'straight bevel gear_iso_ISO - Straight bevel gear 0.7M 36GT 12PT 20PA 5FW ---36O12H20MD8.0S1', ( #24966 ), #48383 ) ;
#39019 = EDGE_CURVE ( 'NONE', #29583, #20925, #22646, .T. ) ;
#39020 = ADVANCED_FACE ( 'NONE', ( #21659 ), #63494, .T. ) ;
#39021 = ORIENTED_EDGE ( 'NONE', *, *, #23826, .F. ) ;
#39022 = CARTESIAN_POINT ( 'NONE',  ( 37.00000000000000711, -3.287724142101330571, 11.73463472867579149 ) ) ;
#39023 = CARTESIAN_POINT ( 'NONE',  ( 2.261269890822074302, -5.762737836065078056, -5.017604628138454537 ) ) ;
#39024 = EDGE_CURVE ( 'NONE', #58596, #5514, #26961, .T. ) ;
#39025 = CARTESIAN_POINT ( 'NONE',  ( -35.00000000000000000, 10.42955799785328708, -6.303578524886837009 ) ) ;
#39026 = VERTEX_POINT ( 'NONE', #32904 ) ;
#39027 = AXIS2_PLACEMENT_3D ( 'NONE', #4421, #55268, #50626 ) ;
#39028 = ADVANCED_FACE ( 'NONE', ( #37911 ), #62199, .T. ) ;
#39029 = AXIS2_PLACEMENT_3D ( 'NONE', #906, #16202, #31491 ) ;
#39030 =( BOUNDED_CURVE ( )  B_SPLINE_CURVE ( 3, ( #19152, #59086, #55050, #59391 ),
 .UNSPECIFIED., .F., .F. ) 
 B_SPLINE_CURVE_WITH_KNOTS ( ( 4, 4 ),
 ( 2.476619846412093651, 2.515060261699084254 ),
 .UNSPECIFIED. ) 
 CURVE ( )  GEOMETRIC_REPRESENTATION_ITEM ( )  RATIONAL_B_SPLINE_CURVE ( ( 1.000000000000000000, 0.9998768649967908484, 0.9998768649967908484, 1.000000000000000000 ) ) 
 REPRESENTATION_ITEM ( '' )  );
#39031 = CARTESIAN_POINT ( 'NONE',  ( 2.241509619876138171, -2.575142053947820031, -7.187074272457178559 ) ) ;
#39032 = EDGE_CURVE ( 'NONE', #20284, #44987, #51597, .T. ) ;
#39033 = CARTESIAN_POINT ( 'NONE',  ( 37.00000000000000711, -0.3137578094510115045, -12.74613886779085092 ) ) ;
#39034 = ORIENTED_EDGE ( 'NONE', *, *, #39948, .F. ) ;
#39035 = FACE_BOUND ( 'NONE', #46529, .T. ) ;
#39036 = DIRECTION ( 'NONE',  ( 0.000000000000000000, 0.5243256840888503856, 0.8515178078024905339 ) ) ;
#39037 = CARTESIAN_POINT ( 'NONE',  ( 2.000000000000001776, 1.530946385938479093, -7.342084388195354805 ) ) ;
#39038 = AXIS2_PLACEMENT_3D ( 'NONE', #50789, #5240, #9542 ) ;
#39039 = B_SPLINE_CURVE_WITH_KNOTS ( 'NONE', 3,
 ( #57109, #52459, #25867, #20862, #36130, #21184, #56441, #26838, #10888, #31805, #6570, #911, #57429, #41453, #47139, #1591 ),
 .UNSPECIFIED., .F., .F.,
 ( 4, 2, 2, 2, 2, 2, 2, 4 ),
 ( 3.496446946337351263E-18, 0.001151362128401672283, 0.001727043192602508099, 0.002302724256803344131, 0.003454086385205015763, 0.004605448513606687395, 0.006908172770410029792, 0.009210897027213369587 ),
 .UNSPECIFIED. ) ;
#39040 = AXIS2_PLACEMENT_3D ( 'NONE', #3279, #38845, #49491 ) ;
#39041 = ADVANCED_FACE ( 'NONE', ( #6357 ), #11654, .T. ) ;
#39042 = DIRECTION ( 'NONE',  ( -1.000000000000000000, 0.000000000000000000, 0.000000000000000000 ) ) ;
#39043 = DIRECTION ( 'NONE',  ( -1.000000000000000000, 0.000000000000000000, 0.000000000000000000 ) ) ;
#39044 = ORIENTED_EDGE ( 'NONE', *, *, #19413, .F. ) ;
#39045 = DIRECTION ( 'NONE',  ( -0.000000000000000000, -0.000000000000000000, -1.000000000000000000 ) ) ;
#39046 = CARTESIAN_POINT ( 'NONE',  ( -36.00000000000000711, -2.080187960898653543, 12.57916205664480636 ) ) ;
#39047 = CARTESIAN_POINT ( 'NONE',  ( -16.98800322446194855, 2.922502605998049674, -11.63868456991314027 ) ) ;
#39048 = ORIENTED_EDGE ( 'NONE', *, *, #56137, .F. ) ;
#39049 = CARTESIAN_POINT ( 'NONE',  ( 0.000000000000000000, -1.734723475976807094E-15, -13.50000000000000178 ) ) ;
#39050 = CARTESIAN_POINT ( 'NONE',  ( 0.2650492433740077036, -4.291726136518470902, -11.46945725111971193 ) ) ;
#39051 = EDGE_LOOP ( 'NONE', ( #52621, #37085, #32476, #255 ) ) ;
#39052 = ORIENTED_EDGE ( 'NONE', *, *, #42208, .T. ) ;
#39053 = CARTESIAN_POINT ( 'NONE',  ( -35.04709527796842394, 0.01016988845958452514, 0.007030359780618375409 ) ) ;
#39054 = ORIENTED_EDGE ( 'NONE', *, *, #11396, .T. ) ;
#39055 = CARTESIAN_POINT ( 'NONE',  ( 2.000000000000001776, 3.152010634611773110, -6.039758645301250617 ) ) ;
#39056 = DIRECTION ( 'NONE',  ( 0.000000000000000000, 0.000000000000000000, 1.000000000000000000 ) ) ;
#39057 = DIRECTION ( 'NONE',  ( -1.000000000000000000, 0.000000000000000000, 0.000000000000000000 ) ) ;
#39058 = LINE ( 'NONE', #13775, #1595 ) ;
#39060 = EDGE_LOOP ( 'NONE', ( #57329, #16950, #44496, #20978 ) ) ;
#39059 = CARTESIAN_POINT ( 'NONE',  ( 1.719304012338398246, 7.581471372739840398, 10.22720798541364395 ) ) ;
#39061 = CARTESIAN_POINT ( 'NONE',  ( 25.00000000000000355, -9.999999999999998224, -5.000000000000000888 ) ) ;
#39062 = EDGE_LOOP ( 'NONE', ( #18597, #26041, #29934, #25831 ) ) ;
#39063 = DIRECTION ( 'NONE',  ( -1.000000000000000000, 0.000000000000000000, 0.000000000000000000 ) ) ;
#39064 = ORIENTED_EDGE ( 'NONE', *, *, #19608, .T. ) ;
#39065 = VERTEX_POINT ( 'NONE', #47902 ) ;
#39066 = LINE ( 'NONE', #59362, #64477 ) ;
#39067 = CARTESIAN_POINT ( 'NONE',  ( -13.26547918569768569, -33.36007533429819460, 10.54465099870296996 ) ) ;
#39068 = AXIS2_PLACEMENT_3D ( 'NONE', #34254, #24279, #40552 ) ;
#39069 = CARTESIAN_POINT ( 'NONE',  ( -24.35620976915924984, 10.90526090019620398, 7.960195681111406962 ) ) ;
#39070 = EDGE_CURVE ( 'NONE', #7420, #64126, #6745, .T. ) ;
#39071 = CARTESIAN_POINT ( 'NONE',  ( 37.00000000000000711, 4.705694406421931860E-17, -3.469127814946512892E-15 ) ) ;
#39072 = DIRECTION ( 'NONE',  ( 0.000000000000000000, -0.9970832820307047317, -0.07632122047555413291 ) ) ;
#39073 = CARTESIAN_POINT ( 'NONE',  ( 35.00000000000000000, 12.54989509947654014, 2.250029553613615452 ) ) ;
#39074 = ORIENTED_EDGE ( 'NONE', *, *, #34192, .F. ) ;
#39075 = AXIS2_PLACEMENT_3D ( 'NONE', #7372, #63237, #19983 ) ;
#39076 = ORIENTED_EDGE ( 'NONE', *, *, #34753, .F. ) ;
#39077 = DIRECTION ( 'NONE',  ( -1.000000000000000000, 0.000000000000000000, 0.000000000000000000 ) ) ;
#39078 = CARTESIAN_POINT ( 'NONE',  ( 2.655192694324496561, 9.204230091440560813, 2.733486750963942225 ) ) ;
#39079 = AXIS2_PLACEMENT_3D ( 'NONE', #35962, #59967, #5757 ) ;
#39080 = ORIENTED_EDGE ( 'NONE', *, *, #26896, .T. ) ;
#39081 = CARTESIAN_POINT ( 'NONE',  ( 2.297017764050092836, -7.506328781223015945, 1.490897313050660644 ) ) ;
#39082 = CIRCLE ( 'NONE', #35893, 4.999999999999999112 ) ;
#39083 = CARTESIAN_POINT ( 'NONE',  ( -35.00000000000000000, 0.000000000000000000, 0.000000000000000000 ) ) ;
#39084 = DIRECTION ( 'NONE',  ( -0.000000000000000000, -0.000000000000000000, -1.000000000000000000 ) ) ;
#39085 = CARTESIAN_POINT ( 'NONE',  ( -22.28350523959501217, 3.041489826385515904, -2.107889123925570818 ) ) ;
#39086 = LINE ( 'NONE', #44393, #61768 ) ;
#39087 = EDGE_CURVE ( 'NONE', #65435, #27379, #61936, .T. ) ;
#39088 = CARTESIAN_POINT ( 'NONE',  ( 2.298277635560276977, 3.968740875991644934, -6.543949079923893741 ) ) ;
#39089 = ORIENTED_EDGE ( 'NONE', *, *, #59384, .T. ) ;
#39090 = ADVANCED_FACE ( 'NONE', ( #16974 ), #52410, .T. ) ;
#39091 = ORIENTED_EDGE ( 'NONE', *, *, #6848, .T. ) ;
#39092 = EDGE_CURVE ( 'NONE', #48895, #51071, #54499, .T. ) ;
#39093 = DIRECTION ( 'NONE',  ( 1.000000000000000000, -0.000000000000000000, 0.000000000000000000 ) ) ;
#39094 = DIRECTION ( 'NONE',  ( 0.000000000000000000, -0.01356324068817999114, 0.9999080150203989437 ) ) ;
#39095 = CARTESIAN_POINT ( 'NONE',  ( 29.03457606387295087, 4.854210015632069997, 10.97436308512422265 ) ) ;
#39096 = B_SPLINE_CURVE_WITH_KNOTS ( 'NONE', 3,
 ( #16555, #55808, #20871, #61114, #30512, #56113, #41140 ),
 .UNSPECIFIED., .F., .F.,
 ( 4, 3, 4 ),
 ( 0.0001321430428584417424, 0.0001982171734706201821, 0.0002642860854759487171 ),
 .UNSPECIFIED. ) ;
#39097 = FACE_OUTER_BOUND ( 'NONE', #13233, .T. ) ;
#39098 = CARTESIAN_POINT ( 'NONE',  ( -28.25671366997987732, 12.49082151344278735, -5.130654606202838863 ) ) ;
#39099 = EDGE_CURVE ( 'NONE', #32743, #60603, #5679, .T. ) ;
#39100 = AXIS2_PLACEMENT_3D ( 'NONE', #40814, #41783, #587 ) ;
#39101 = CARTESIAN_POINT ( 'NONE',  ( -10.87579916591577778, -6.848527916712992436, -9.862315760539463128 ) ) ;
#39102 = EDGE_CURVE ( 'NONE', #39990, #62542, #47093, .T. ) ;
#39103 = CARTESIAN_POINT ( 'NONE',  ( -25.86628395826706850, 5.139808748864376220, 10.84354029019568522 ) ) ;
#39104 = CARTESIAN_POINT ( 'NONE',  ( -27.09483304420799143, -2.090133548856194068, -1.013994808271696746 ) ) ;
#39105 = FACE_OUTER_BOUND ( 'NONE', #28470, .T. ) ;
#39106 = EDGE_CURVE ( 'NONE', #60850, #14900, #60854, .T. ) ;
#39107 = ORIENTED_EDGE ( 'NONE', *, *, #63883, .F. ) ;
#39108 = CARTESIAN_POINT ( 'NONE',  ( 35.00000000000000000, -11.81949347079744506, 2.968224442958526943 ) ) ;
#39109 = DIRECTION ( 'NONE',  ( -1.000000000000000000, 0.000000000000000000, -0.000000000000000000 ) ) ;
#39110 = ADVANCED_FACE ( 'NONE', ( #3989 ), #13305, .T. ) ;
#39111 = AXIS2_PLACEMENT_3D ( 'NONE', #56524, #51559, #57183 ) ;
#39112 = EDGE_CURVE ( 'NONE', #36091, #53066, #24779, .T. ) ;
#39113 = CARTESIAN_POINT ( 'NONE',  ( 2.266490820343228574, -0.1453321357832227656, -7.641399530653803396 ) ) ;
#39114 = CARTESIAN_POINT ( 'NONE',  ( 2.259830038564998311, -5.940579220577209441, 4.804964945109168717 ) ) ;
#39115 = AXIS2_PLACEMENT_3D ( 'NONE', #61636, #1484, #22385 ) ;
#39116 = VERTEX_POINT ( 'NONE', #4314 ) ;
#39117 = CARTESIAN_POINT ( 'NONE',  ( 35.00000000000000000, 9.926225166347027340, -6.280308599560179061 ) ) ;
#39118 = CARTESIAN_POINT ( 'NONE',  ( 25.00000000000000355, -30.00000000000000000, 5.000000000000000888 ) ) ;
#39120 = ADVANCED_FACE ( 'NONE', ( #48568 ), #13758, .F. ) ;
#39119 = CARTESIAN_POINT ( 'NONE',  ( -5.901743774574147672, -31.73659747722650692, -13.63115424678022158 ) ) ;
#39121 = ORIENTED_EDGE ( 'NONE', *, *, #46126, .T. ) ;
#39122 = CIRCLE ( 'NONE', #15765, 12.18650000000000233 ) ;
#39123 = CARTESIAN_POINT ( 'NONE',  ( -10.84711731306251714, -4.830322288942776154, -12.61315300571293108 ) ) ;
#39124 = CYLINDRICAL_SURFACE ( 'NONE', #5587, 5.000000000000000888 ) ;
#39125 = LINE ( 'NONE', #2926, #5239 ) ;
#39126 = VECTOR ( 'NONE', #10540, 1000.000000000000000 ) ;
#39127 = DIRECTION ( 'NONE',  ( -1.000000000000000000, 0.000000000000000000, -0.000000000000000000 ) ) ;
#39128 = CARTESIAN_POINT ( 'NONE',  ( -35.00000000000000000, 10.92721691015462149, -4.309077947445535628 ) ) ;
#39129 = DIRECTION ( 'NONE',  ( 0.000000000000000000, 0.000000000000000000, 1.000000000000000000 ) ) ;
#39130 = ORIENTED_EDGE ( 'NONE', *, *, #25753, .T. ) ;
#39131 = DIRECTION ( 'NONE',  ( 1.000000000000000000, -0.000000000000000000, 0.000000000000000000 ) ) ;
#39132 = FACE_OUTER_BOUND ( 'NONE', #12810, .T. ) ;
#39133 = DIRECTION ( 'NONE',  ( -1.000000000000000000, 0.000000000000000000, 0.000000000000000000 ) ) ;
#39134 = CARTESIAN_POINT ( 'NONE',  ( 2.290907136833256974, 7.561169784528423143, -1.168459104840855911 ) ) ;
#39135 = CARTESIAN_POINT ( 'NONE',  ( -35.00000000000000000, -5.672855678558757830, 10.28547182238005853 ) ) ;
#39136 = CARTESIAN_POINT ( 'NONE',  ( -29.61291272822813170, 2.156105836073342275, -11.83797064166018664 ) ) ;
#39137 = CARTESIAN_POINT ( 'NONE',  ( 2.276905613632196790, 1.175741125185098213, -7.555317002491444889 ) ) ;
#39138 = ORIENTED_EDGE ( 'NONE', *, *, #44975, .T. ) ;
#39139 = ORIENTED_EDGE ( 'NONE', *, *, #36398, .T. ) ;
#39140 = CARTESIAN_POINT ( 'NONE',  ( -18.17105223446473872, -5.570524445111396439, -10.62960849765157789 ) ) ;
#39141 = ORIENTED_EDGE ( 'NONE', *, *, #56234, .T. ) ;
#39142 = SURFACE_SIDE_STYLE ('',( #54125 ) ) ;
#39143 = CARTESIAN_POINT ( 'NONE',  ( -27.10719052120871098, -2.295785794152564563, -0.5475695427849640584 ) ) ;
#39144 = EDGE_CURVE ( 'NONE', #9770, #27200, #42794, .T. ) ;
#39145 = VECTOR ( 'NONE', #32958, 1000.000000000000000 ) ;
#39146 = CARTESIAN_POINT ( 'NONE',  ( 3.152665057734040488, 0.000000000000000000, 0.000000000000000000 ) ) ;
#39147 = VERTEX_POINT ( 'NONE', #64799 ) ;
#39148 = CARTESIAN_POINT ( 'NONE',  ( -35.00000000000000000, 0.000000000000000000, 0.000000000000000000 ) ) ;
#39149 = CARTESIAN_POINT ( 'NONE',  ( 2.373367633546870969, 1.511052049480019255, -7.528269033630142104 ) ) ;
#39150 = AXIS2_PLACEMENT_3D ( 'NONE', #54666, #34014, #53988 ) ;
#39151 = CARTESIAN_POINT ( 'NONE',  ( 24.90165730046861370, -0.3389098318347745220, 13.50162224760967256 ) ) ;
#39152 = VERTEX_POINT ( 'NONE', #8009 ) ;
#39153 = EDGE_LOOP ( 'NONE', ( #7811, #39666, #61159, #34497 ) ) ;
#39154 = DIRECTION ( 'NONE',  ( 0.000000000000000000, -1.000000000000000000, 0.000000000000000000 ) ) ;
#39155 = DIRECTION ( 'NONE',  ( -1.000000000000000000, 0.000000000000000000, 0.000000000000000000 ) ) ;
#39156 = EDGE_CURVE ( 'NONE', #39116, #38647, #43680, .T. ) ;
#39157 = ORIENTED_EDGE ( 'NONE', *, *, #60598, .T. ) ;
#39158 = ORIENTED_EDGE ( 'NONE', *, *, #15811, .T. ) ;
#39159 = CARTESIAN_POINT ( 'NONE',  ( 12.52750123246316072, 0.4973700281276248192, 13.49083477977253764 ) ) ;
#39161 = AXIS2_PLACEMENT_3D ( 'NONE', #29255, #18049, #39879 ) ;
#39160 = CARTESIAN_POINT ( 'NONE',  ( -37.00000000000000711, 0.000000000000000000, 0.000000000000000000 ) ) ;
#39162 = DIRECTION ( 'NONE',  ( 0.000000000000000000, 0.01356324068817998940, -0.9999080150203989437 ) ) ;
#39163 = DIRECTION ( 'NONE',  ( 0.000000000000000000, -0.9467777615094536969, -0.3218879778916073908 ) ) ;
#39164 = CYLINDRICAL_SURFACE ( 'NONE', #28481, 2.899999999999994582 ) ;
#39165 = EDGE_CURVE ( 'NONE', #2995, #48281, #26267, .T. ) ;
#39166 = CARTESIAN_POINT ( 'NONE',  ( 3.152665057734086229, 4.725420687650732532, 6.378477742800449768 ) ) ;
#39167 = VECTOR ( 'NONE', #26292, 1000.000000000000000 ) ;
#39168 = VERTEX_POINT ( 'NONE', #61454 ) ;
#39169 = CARTESIAN_POINT ( 'NONE',  ( 2.990245332647879284, -1.974808303407750154, 8.248134185053356049 ) ) ;
#39170 = CARTESIAN_POINT ( 'NONE',  ( -17.69949227665007641, 6.590587637064748705, 10.03069147607176426 ) ) ;
#39171 = CIRCLE ( 'NONE', #45532, 3.999999999999999112 ) ;
#39172 = PRODUCT_DEFINITION_SHAPE ( 'NONE', 'NONE',  #31126 ) ;
#39173 = CARTESIAN_POINT ( 'NONE',  ( 0.2653141617321057577, -9.409385893408552803, 7.837919552760688191 ) ) ;
#39174 = ADVANCED_FACE ( 'NONE', ( #19924 ), #9597, .T. ) ;
#39175 = CARTESIAN_POINT ( 'NONE',  ( -22.27218376572352554, -3.026314224080924209, 2.099017427146280479 ) ) ;
#39176 = DIRECTION ( 'NONE',  ( 0.000000000000000000, 0.000000000000000000, -1.000000000000000000 ) ) ;
#39177 = CARTESIAN_POINT ( 'NONE',  ( -27.08429572838383947, 1.632445743623435197, -1.608131779585709076 ) ) ;
#39178 = CARTESIAN_POINT ( 'NONE',  ( 35.00000000000000000, -10.80631716521670427, -4.603882218679513194 ) ) ;
#39179 = FACE_OUTER_BOUND ( 'NONE', #52679, .T. ) ;
#39180 = AXIS2_PLACEMENT_3D ( 'NONE', #45725, #20791, #15777 ) ;
#39181 = CARTESIAN_POINT ( 'NONE',  ( 1.719304012338401133, 5.690355757826538685, 11.38834240361399885 ) ) ;
#39182 = VERTEX_POINT ( 'NONE', #14582 ) ;
#39183 = DIRECTION ( 'NONE',  ( 0.000000000000000000, 0.000000000000000000, 1.000000000000000000 ) ) ;
#39184 = VERTEX_POINT ( 'NONE', #60480 ) ;
#39185 = FACE_OUTER_BOUND ( 'NONE', #43225, .T. ) ;
#39186 = DIRECTION ( 'NONE',  ( 0.000000000000000000, 0.000000000000000000, -1.000000000000000000 ) ) ;
#39187 = CARTESIAN_POINT ( 'NONE',  ( -10.86097166128075386, -8.305831640360002766, 10.65335268811077896 ) ) ;
#39188 = CARTESIAN_POINT ( 'NONE',  ( 2.589278595513879733, 5.163950571302623693, 5.779442428606822446 ) ) ;
#39189 = VERTEX_POINT ( 'NONE', #35201 ) ;
#39190 = CARTESIAN_POINT ( 'NONE',  ( 35.00000000000000000, -12.68495603654572434, -1.286231064351273101 ) ) ;
#39191 = CARTESIAN_POINT ( 'NONE',  ( -35.00000000000000000, -0.8294751490780184477, 12.15823808070322443 ) ) ;
#39192 = CARTESIAN_POINT ( 'NONE',  ( 9.627852802940182642, 2.216197012197528071, 11.79553571166074555 ) ) ;
#39193 = CARTESIAN_POINT ( 'NONE',  ( 0.6473888112830247232, 2.472751636945372145, 12.12394591856679860 ) ) ;
#39194 = EDGE_CURVE ( 'NONE', #24707, #50839, #26915, .T. ) ;
#39195 = AXIS2_PLACEMENT_3D ( 'NONE', #34527, #54826, #14873 ) ;
#39196 = EDGE_CURVE ( 'NONE', #26844, #20926, #37314, .T. ) ;
#39197 = FACE_OUTER_BOUND ( 'NONE', #63736, .T. ) ;
#39198 = ORIENTED_EDGE ( 'NONE', *, *, #11944, .F. ) ;
#39199 = AXIS2_PLACEMENT_3D ( 'NONE', #8353, #3392, #59551 ) ;
#39201 = ADVANCED_FACE ( 'NONE', ( #36181 ), #30234, .T. ) ;
#39200 = PLANE ( 'NONE',  #7363 ) ;
#39202 = EDGE_LOOP ( 'NONE', ( #21316, #61985, #27349, #38931 ) ) ;
#39203 = CARTESIAN_POINT ( 'NONE',  ( 2.368238019615013012, 5.763545178420172554, -5.070835960312829016 ) ) ;
#39204 = DIRECTION ( 'NONE',  ( -0.3865475372811021382, 0.6938894834606125217, -0.6075346789811091330 ) ) ;
#39205 = CARTESIAN_POINT ( 'NONE',  ( 2.000000000000001776, 6.935703035393450122, 0.1051458740707594125 ) ) ;
#39206 = DIRECTION ( 'NONE',  ( 1.000000000000000000, 0.000000000000000000, 0.000000000000000000 ) ) ;
#39207 = AXIS2_PLACEMENT_3D ( 'NONE', #42809, #33162, #28497 ) ;
#39208 = ORIENTED_EDGE ( 'NONE', *, *, #16835, .F. ) ;
#39209 = EDGE_LOOP ( 'NONE', ( #22955, #2898, #19947, #14521 ) ) ;
#39210 = B_SPLINE_CURVE_WITH_KNOTS ( 'NONE', 3,
 ( #16999, #37278, #27300, #57590, #41616, #62227, #31631, #57920, #51624, #26326 ),
 .UNSPECIFIED., .F., .F.,
 ( 4, 3, 3, 4 ),
 ( 4.336808689942017736E-19, 6.607638129004444159E-05, 9.911389841680550718E-05, 0.0001667630577588612270 ),
 .UNSPECIFIED. ) ;
#39211 = CARTESIAN_POINT ( 'NONE',  ( -27.27855387000350262, 10.59660315834921640, 5.631341004100471892 ) ) ;
#39212 = CARTESIAN_POINT ( 'NONE',  ( 0.2638984909335716500, 4.375449752477288179, -11.43908195192325294 ) ) ;
#39214 = CARTESIAN_POINT ( 'NONE',  ( -35.00000000000000000, 8.258652103341553641, -8.352657516904583801 ) ) ;
#39213 =( BOUNDED_SURFACE ( )  B_SPLINE_SURFACE ( 3, 1, ( 
 ( #24148, #44406 ),
 ( #65026, #35078 ),
 ( #65357, #25134 ),
 ( #19820, #50422 ) ),
 .UNSPECIFIED., .F., .F., .F. ) 
 B_SPLINE_SURFACE_WITH_KNOTS ( ( 4, 4 ),
 ( 2, 2 ),
 ( 0.000000000000000000, 1.000000000000000000 ),
 ( 0.000000000000000000, 1.000000000000000000 ),
 .UNSPECIFIED. ) 
 GEOMETRIC_REPRESENTATION_ITEM ( )  RATIONAL_B_SPLINE_SURFACE ( (
 ( 1.000000000000000000, 1.000000000000000000),
 ( 0.6933888150995267674, 0.9895912004443193632),
 ( 0.6933888150995267674, 0.9895912004443193632),
 ( 1.000000000000000000, 1.000000000000000000) ) ) 
 REPRESENTATION_ITEM ( '' )  SURFACE ( )  );
#39215 = CARTESIAN_POINT ( 'NONE',  ( 2.889800649504073782, -4.732281052280337796, 3.882893708502031860 ) ) ;
#39216 = CARTESIAN_POINT ( 'NONE',  ( 0.3654063281920751916, 9.235228056824031029, -8.093076148785947055 ) ) ;
#39217 = CARTESIAN_POINT ( 'NONE',  ( 0.5572780756284481107, -12.33974848088638687, -0.3055340344620752768 ) ) ;
#39218 = EDGE_LOOP ( 'NONE', ( #44634, #13743, #13553, #14659 ) ) ;
#39219 = ORIENTED_EDGE ( 'NONE', *, *, #27374, .F. ) ;
#39220 = VECTOR ( 'NONE', #26351, 1000.000000000000000 ) ;
#39221 = VERTEX_POINT ( 'NONE', #15578 ) ;
#39222 = CARTESIAN_POINT ( 'NONE',  ( 5.514970785353741078, -0.004588761610584819045, -0.001117786416802158496 ) ) ;
#39223 = DIRECTION ( 'NONE',  ( 0.000000000000000000, 0.2960891610144510966, 0.9551603052523478521 ) ) ;
#39224 = EDGE_CURVE ( 'NONE', #42915, #61990, #32158, .T. ) ;
#39225 = ORIENTED_EDGE ( 'NONE', *, *, #525, .T. ) ;
#39226 = FACE_OUTER_BOUND ( 'NONE', #51404, .T. ) ;
#39227 = DIRECTION ( 'NONE',  ( 0.000000000000000000, -0.1081190184239279872, -0.9941379571543611515 ) ) ;
#39228 = ADVANCED_FACE ( 'NONE', ( #50531 ), #9951, .T. ) ;
#39229 = VERTEX_POINT ( 'NONE', #41174 ) ;
#39230 = CARTESIAN_POINT ( 'NONE',  ( 2.241528039335008327, 6.619488482362989146, -3.803597072146465585 ) ) ;
#39231 = CARTESIAN_POINT ( 'NONE',  ( -35.00000000000000000, 0.000000000000000000, 0.000000000000000000 ) ) ;
#39232 = CARTESIAN_POINT ( 'NONE',  ( 35.00000000000000000, 6.657191900728455458, 9.677500615117825333 ) ) ;
#39233 = ORIENTED_EDGE ( 'NONE', *, *, #5438, .F. ) ;
#39234 = ORIENTED_EDGE ( 'NONE', *, *, #39224, .F. ) ;
#39235 = DIRECTION ( 'NONE',  ( 0.000000000000000000, 0.000000000000000000, -1.000000000000000000 ) ) ;
#39236 = ORIENTED_EDGE ( 'NONE', *, *, #8736, .F. ) ;
#39237 = LINE ( 'NONE', #44890, #6157 ) ;
#39238 = ORIENTED_EDGE ( 'NONE', *, *, #3539, .T. ) ;
#39239 = EDGE_CURVE ( 'NONE', #45342, #27199, #34552, .T. ) ;
#39240 = ORIENTED_EDGE ( 'NONE', *, *, #5963, .F. ) ;
#39241 = EDGE_LOOP ( 'NONE', ( #27316, #62143, #51593, #58124 ) ) ;
#39242 = CARTESIAN_POINT ( 'NONE',  ( 0.2652384529303126182, 11.53005674806963121, 4.126283314267611857 ) ) ;
#39243 = CARTESIAN_POINT ( 'NONE',  ( -35.04683013664716640, 0.006090538653970694813, -0.01075274318002154145 ) ) ;
#39245 = CARTESIAN_POINT ( 'NONE',  ( -22.31328051695926007, 3.685074213229321494, 0.8849444482787824917 ) ) ;
#39244 = VECTOR ( 'NONE', #36149, 1000.000000000000000 ) ;
#39247 = B_SPLINE_CURVE_WITH_KNOTS ( 'NONE', 3,
 ( #26976, #47273, #25998, #36278, #41599, #61888, #16347, #36618 ),
 .UNSPECIFIED., .F., .F.,
 ( 4, 2, 2, 4 ),
 ( 0.01093700429183111500, 0.01319343274642247738, 0.01544986120101383975, 0.01996271811019656450 ),
 .UNSPECIFIED. ) ;
#39246 = CARTESIAN_POINT ( 'NONE',  ( -35.00000000000000000, -2.627174906296831480, -11.44858830469743083 ) ) ;
#39248 = CARTESIAN_POINT ( 'NONE',  ( -22.59983133926799326, 0.06110861519533868080, -4.650609684383240960 ) ) ;
#39249 = ORIENTED_EDGE ( 'NONE', *, *, #13564, .F. ) ;
#39250 = CARTESIAN_POINT ( 'NONE',  ( 41.00000000000000711, -25.03188948156373783, 4.499999999999997335 ) ) ;
#39251 = ORIENTED_EDGE ( 'NONE', *, *, #279, .F. ) ;
#39252 = CIRCLE ( 'NONE', #10569, 12.75000000000000178 ) ;
#39253 = FACE_OUTER_BOUND ( 'NONE', #46231, .T. ) ;
#39254 = DIRECTION ( 'NONE',  ( 1.000000000000000000, -0.000000000000000000, 0.000000000000000000 ) ) ;
#39255 = EDGE_CURVE ( 'NONE', #38647, #8430, #12687, .T. ) ;
#39256 = ORIENTED_EDGE ( 'NONE', *, *, #16789, .T. ) ;
#39257 = CARTESIAN_POINT ( 'NONE',  ( 37.00000000000000711, 10.12742074351896449, -7.745827850123049529 ) ) ;
#39258 = FACE_OUTER_BOUND ( 'NONE', #8217, .T. ) ;
#39259 = CARTESIAN_POINT ( 'NONE',  ( 2.241352910868908754, -6.652881166698485949, -3.744764251557062718 ) ) ;
#39260 = EDGE_CURVE ( 'NONE', #42105, #53879, #40870, .T. ) ;
#39261 = AXIS2_PLACEMENT_3D ( 'NONE', #52406, #43629, #48978 ) ;
#39262 = EDGE_LOOP ( 'NONE', ( #3438, #39747, #7425, #21513 ) ) ;
#39263 = ORIENTED_EDGE ( 'NONE', *, *, #9295, .F. ) ;
#39264 = PLANE ( 'NONE',  #48153 ) ;
#39265 = ORIENTED_EDGE ( 'NONE', *, *, #28893, .F. ) ;
#39266 = CARTESIAN_POINT ( 'NONE',  ( -27.19357181888462094, -12.48377454417556542, 5.138615876886901468 ) ) ;
#39267 = LINE ( 'NONE', #30285, #39341 ) ;
#39268 = CARTESIAN_POINT ( 'NONE',  ( -30.07167209738885560, 0.1566904097641563520, 13.50094810325072814 ) ) ;
#39269 = CARTESIAN_POINT ( 'NONE',  ( 2.969415267404248215, 4.269695207293191075, 6.619534278261581584 ) ) ;
#39270 = CARTESIAN_POINT ( 'NONE',  ( 13.26561344960581934, 10.13979182165873993, -6.421342877150610917 ) ) ;
#39271 = ORIENTED_EDGE ( 'NONE', *, *, #14777, .T. ) ;
#39272 = CIRCLE ( 'NONE', #2115, 12.75000000000000178 ) ;
#39273 = CARTESIAN_POINT ( 'NONE',  ( -22.66110217412718342, -3.914841338650320246, -3.020638270782546542 ) ) ;
#39274 = CARTESIAN_POINT ( 'NONE',  ( 2.406456491626281835, -9.333533259764168477, -4.662370073863471909 ) ) ;
#39275 = ADVANCED_FACE ( 'NONE', ( #25909 ), #46834, .T. ) ;
#39276 = B_SPLINE_CURVE_WITH_KNOTS ( 'NONE', 3,
 ( #37936, #7339, #48590, #3044, #48282, #3377, #52906, #32931, #33614, #58228, #27623, #38933, #17674, #22662, #47926, #38251, #12648, #2386, #2731 ),
 .UNSPECIFIED., .F., .F.,
 ( 4, 3, 3, 3, 3, 3, 4 ),
 ( 0.000000000000000000, 2.831840207499890458E-05, 4.217266859840865451E-05, 5.602024318396426049E-05, 6.290810167969416620E-05, 9.120440630945709744E-05, 0.0001153103026479752088 ),
 .UNSPECIFIED. ) ;
#39277 = EDGE_CURVE ( 'NONE', #39221, #52020, #27523, .T. ) ;
#39278 = CARTESIAN_POINT ( 'NONE',  ( -1.009501604528854735, -26.56249173023641319, -16.21092882686939163 ) ) ;
#39280 = EDGE_CURVE ( 'NONE', #19066, #24709, #57687, .T. ) ;
#39279 = CARTESIAN_POINT ( 'NONE',  ( 2.373367633546870525, -5.072743978105275886, 5.764146204907447668 ) ) ;
#39281 = DIRECTION ( 'NONE',  ( -0.9029087107030919768, 0.4298323628305345534, 0.000000000000000000 ) ) ;
#39282 = CARTESIAN_POINT ( 'NONE',  ( -37.00000000000000711, -3.614449339633411196, -11.17622378668010441 ) ) ;
#39283 = DIRECTION ( 'NONE',  ( -1.000000000000000000, 0.000000000000000000, 0.000000000000000000 ) ) ;
#39284 = CIRCLE ( 'NONE', #64763, 4.999999999999999112 ) ;
#39285 = EDGE_CURVE ( 'NONE', #14592, #28690, #48146, .T. ) ;
#39286 = ORIENTED_EDGE ( 'NONE', *, *, #54731, .T. ) ;
#39287 = CARTESIAN_POINT ( 'NONE',  ( 10.35765492805355592, -11.92981863842239498, -1.311496141409351335 ) ) ;
#39288 = ORIENTED_EDGE ( 'NONE', *, *, #54622, .T. ) ;
#39289 = CARTESIAN_POINT ( 'NONE',  ( -4.989057617119011745, -0.9162120371760335003, 25.00000000000000000 ) ) ;
#39290 = LINE ( 'NONE', #3763, #34399 ) ;
#39291 = B_SPLINE_CURVE_WITH_KNOTS ( 'NONE', 3,
 ( #31038, #41668, #51350, #2703, #62849, #52878, #60984, #55982, #10417, #25731 ),
 .UNSPECIFIED., .F., .F.,
 ( 4, 2, 2, 2, 4 ),
 ( 4.336808689942017736E-19, 0.0007897640485358541377, 0.001579528097071707842, 0.002369292145607561437, 0.003159056194143415250 ),
 .UNSPECIFIED. ) ;
#39292 = CARTESIAN_POINT ( 'NONE',  ( 2.639814597422737386, -7.382549681340928593, 2.414168779979558810 ) ) ;
#39293 = ORIENTED_EDGE ( 'NONE', *, *, #44789, .F. ) ;
#39294 = ORIENTED_EDGE ( 'NONE', *, *, #41219, .T. ) ;
#39295 = VERTEX_POINT ( 'NONE', #2278 ) ;
#39296 = CARTESIAN_POINT ( 'NONE',  ( 0.2869720083484356143, -7.715523637151703973, -9.519277517057183502 ) ) ;
#39297 = CIRCLE ( 'NONE', #35062, 1.500000000000000222 ) ;
#39298 = VERTEX_POINT ( 'NONE', #61795 ) ;
#39299 = CARTESIAN_POINT ( 'NONE',  ( -22.27715526084302056, -2.228953214080623635, -2.930376837866850437 ) ) ;
#39300 = CARTESIAN_POINT ( 'NONE',  ( -37.00000000000000711, 0.000000000000000000, 0.000000000000000000 ) ) ;
#39301 = AXIS2_PLACEMENT_3D ( 'NONE', #15171, #5552, #30146 ) ;
#39302 = CARTESIAN_POINT ( 'NONE',  ( 0.3675815128205894289, -9.235491948680062180, 8.093875121226046687 ) ) ;
#39303 = CARTESIAN_POINT ( 'NONE',  ( 36.00000000000000711, 7.608228585767871976, 10.23119532541064203 ) ) ;
#39304 = ADVANCED_FACE ( 'NONE', ( #32827 ), #42820, .T. ) ;
#39305 = ORIENTED_EDGE ( 'NONE', *, *, #50179, .T. ) ;
#39306 = DIRECTION ( 'NONE',  ( 1.000000000000000000, 0.000000000000000000, 0.000000000000000000 ) ) ;
#39307 = DIRECTION ( 'NONE',  ( 0.000000000000000000, 0.01356324068817998940, -0.9999080150203989437 ) ) ;
#39308 = DIRECTION ( 'NONE',  ( 0.000000000000000000, -0.01356324068818000328, 0.9999080150203990547 ) ) ;
#39310 = ORIENTED_EDGE ( 'NONE', *, *, #35423, .T. ) ;
#39309 = CARTESIAN_POINT ( 'NONE',  ( -27.30970368864378273, -11.82098433594888753, -2.066507538000776467 ) ) ;
#39311 = CYLINDRICAL_SURFACE ( 'NONE', #64938, 10.70557198542813815 ) ;
#39312 = ORIENTED_EDGE ( 'NONE', *, *, #2130, .F. ) ;
#39313 = DIRECTION ( 'NONE',  ( -1.000000000000000000, 0.000000000000000000, 0.000000000000000000 ) ) ;
#39314 = CIRCLE ( 'NONE', #47827, 12.18650000000000055 ) ;
#39315 = VERTEX_POINT ( 'NONE', #56841 ) ;
#39316 = CARTESIAN_POINT ( 'NONE',  ( -29.41315789147035886, 0.9355746134413824855, -11.96533147116139162 ) ) ;
#39317 = DIRECTION ( 'NONE',  ( -1.000000000000000000, 0.000000000000000000, -0.000000000000000000 ) ) ;
#39318 = CARTESIAN_POINT ( 'NONE',  ( -35.00000000000000000, -10.93004082984014147, -6.564808257521884904 ) ) ;
#39319 = LINE ( 'NONE', #32673, #60894 ) ;
#39320 = EDGE_CURVE ( 'NONE', #31123, #52583, #54767, .T. ) ;
#39321 = DIRECTION ( 'NONE',  ( 0.000000000000000000, 0.01356324068817992175, -0.9999080150203990547 ) ) ;
#39322 = CARTESIAN_POINT ( 'NONE',  ( 2.889800649504073782, 0.06738247734050435700, 6.121013568931506832 ) ) ;
#39323 = CARTESIAN_POINT ( 'NONE',  ( 0.3106921474978455167, -3.971572160646677840, -11.60027394202202444 ) ) ;
#39325 = ORIENTED_EDGE ( 'NONE', *, *, #49049, .T. ) ;
#39324 = CARTESIAN_POINT ( 'NONE',  ( 2.000000000000001776, -4.444115772890066651, -5.163689623839394116 ) ) ;
#39326 = CIRCLE ( 'NONE', #10648, 12.18649999999999878 ) ;
#39327 = ORIENTED_EDGE ( 'NONE', *, *, #35520, .T. ) ;
#39328 = FACE_OUTER_BOUND ( 'NONE', #45328, .T. ) ;
#39329 = ORIENTED_EDGE ( 'NONE', *, *, #31910, .F. ) ;
#39330 = AXIS2_PLACEMENT_3D ( 'NONE', #54781, #7926, #23201 ) ;
#39331 = EDGE_CURVE ( 'NONE', #58956, #47135, #38134, .T. ) ;
#39332 = ORIENTED_EDGE ( 'NONE', *, *, #16777, .F. ) ;
#39333 = DIRECTION ( 'NONE',  ( 1.000000000000000000, -0.000000000000000000, 0.000000000000000000 ) ) ;
#39334 = CARTESIAN_POINT ( 'NONE',  ( -35.00000000000000000, 8.389074212634412220, -8.839356091079954680 ) ) ;
#39335 = CARTESIAN_POINT ( 'NONE',  ( 1.452237505248555660, -2.778494755358972057, -12.34692280296794742 ) ) ;
#39336 = CARTESIAN_POINT ( 'NONE',  ( -22.27786964138239867, 2.131221155130671452, 3.004507515156356501 ) ) ;
#39337 = CARTESIAN_POINT ( 'NONE',  ( -22.28629837673888048, 1.594277649056540902, -3.348758206500249468 ) ) ;
#39338 = ADVANCED_FACE ( 'NONE', ( #57480 ), #11905, .T. ) ;
#39339 = CARTESIAN_POINT ( 'NONE',  ( 0.3675815128205894289, 10.76447900494948584, -5.910255304480332761 ) ) ;
#39340 = AXIS2_PLACEMENT_3D ( 'NONE', #23179, #43120, #32484 ) ;
#39341 = VECTOR ( 'NONE', #49917, 1000.000000000000000 ) ;
#39342 = AXIS2_PLACEMENT_3D ( 'NONE', #27944, #22963, #36355 ) ;
#39343 = CARTESIAN_POINT ( 'NONE',  ( -36.00000000000000711, 12.54989509947650994, 2.250029553613800637 ) ) ;
#39344 = VERTEX_POINT ( 'NONE', #6938 ) ;
#39345 = FACE_OUTER_BOUND ( 'NONE', #46828, .T. ) ;
#39346 = CARTESIAN_POINT ( 'NONE',  ( 2.298277635560276533, -5.755367168477967255, -5.044791616846986848 ) ) ;
#39347 = CARTESIAN_POINT ( 'NONE',  ( -22.27384469013076185, 2.154627400808035276, 2.985904959940879344 ) ) ;
#39348 = ORIENTED_EDGE ( 'NONE', *, *, #10200, .T. ) ;
#39349 = AXIS2_PLACEMENT_3D ( 'NONE', #35032, #44062, #65318 ) ;
#39350 = EDGE_CURVE ( 'NONE', #63989, #34225, #36443, .T. ) ;
#39351 = CIRCLE ( 'NONE', #63794, 5.000000000000000000 ) ;
#39352 = VECTOR ( 'NONE', #36291, 1000.000000000000000 ) ;
#39353 = CARTESIAN_POINT ( 'NONE',  ( 33.80171706282990840, -2.756546641835186495, -23.41361577495085200 ) ) ;
#39354 = VECTOR ( 'NONE', #54819, 1000.000000000000000 ) ;
#39355 = CARTESIAN_POINT ( 'NONE',  ( 0.000000000000000000, -6.470132594555779271, -2.133363481234176628 ) ) ;
#39356 = ORIENTED_EDGE ( 'NONE', *, *, #57670, .F. ) ;
#39357 = DIRECTION ( 'NONE',  ( 1.000000000000000000, -0.000000000000000000, 0.000000000000000000 ) ) ;
#39358 = DIRECTION ( 'NONE',  ( 0.000000000000000000, 0.8827602140260332186, -0.4698238015817333135 ) ) ;
#39359 = CARTESIAN_POINT ( 'NONE',  ( 0.6599377198674351019, -0.1505700908830693296, 12.00187902586435840 ) ) ;
#39360 = AXIS2_PLACEMENT_3D ( 'NONE', #33930, #3049, #63858 ) ;
#39361 = EDGE_CURVE ( 'NONE', #11586, #42316, #16281, .T. ) ;
#39362 = DIRECTION ( 'NONE',  ( -0.3865475372811021937, 0.1791957239473662700, 0.9046932595863054205 ) ) ;
#39363 = CARTESIAN_POINT ( 'NONE',  ( 37.00000000000000711, 8.766823244861988940, -7.817610399097547180 ) ) ;
#39364 = CIRCLE ( 'NONE', #11783, 12.18649999999999878 ) ;
#39365 = VERTEX_POINT ( 'NONE', #59428 ) ;
#39366 = CARTESIAN_POINT ( 'NONE',  ( -22.27218376572352554, 3.566922835983793227, 0.9173404081777183361 ) ) ;
#39367 = DIRECTION ( 'NONE',  ( 1.000000000000000000, 0.000000000000000000, 0.000000000000000000 ) ) ;
#39368 = CARTESIAN_POINT ( 'NONE',  ( -17.50299937445415566, 2.687489394990541847, -11.69635546961540129 ) ) ;
#39369 = ORIENTED_EDGE ( 'NONE', *, *, #36627, .T. ) ;
#39370 = CARTESIAN_POINT ( 'NONE',  ( -2.952869152607106251, 25.00000000000000000, 3.755417052241485365 ) ) ;
#39371 = CARTESIAN_POINT ( 'NONE',  ( 35.00000000000000000, -2.185196060783960892, -11.54110654723648466 ) ) ;
#39372 = VERTEX_POINT ( 'NONE', #64093 ) ;
#39373 = ORIENTED_EDGE ( 'NONE', *, *, #3045, .F. ) ;
#39374 = CARTESIAN_POINT ( 'NONE',  ( -36.00000000000000711, -12.54989509947649573, -2.250029553613892563 ) ) ;
#39375 = AXIS2_PLACEMENT_3D ( 'NONE', #5456, #19763, #31032 ) ;
#39376 = CIRCLE ( 'NONE', #10716, 12.18650000000000233 ) ;
#39377 = AXIS2_PLACEMENT_3D ( 'NONE', #6199, #31764, #1552 ) ;
#39378 = VERTEX_POINT ( 'NONE', #58810 ) ;
#39379 = CARTESIAN_POINT ( 'NONE',  ( 2.000000000000001776, 6.906413915731199005, -0.6453518998146886565 ) ) ;
#39380 = DIRECTION ( 'NONE',  ( 0.000000000000000000, 0.9985334138511237079, 0.05413890858542116241 ) ) ;
#39381 = CARTESIAN_POINT ( 'NONE',  ( 0.3401186441510199443, -6.355596563012379185, 10.49699112323340877 ) ) ;
#39382 = CARTESIAN_POINT ( 'NONE',  ( -36.00000000000000711, 3.033604067594749765, -12.38385022362078836 ) ) ;
#39383 = ADVANCED_FACE ( 'NONE', ( #23538 ), #44136, .T. ) ;
#39384 = VECTOR ( 'NONE', #29433, 1000.000000000000000 ) ;
#39385 = CARTESIAN_POINT ( 'NONE',  ( -22.27384469013076185, -3.358914544760241316, -1.508555848190779702 ) ) ;
#39387 = ORIENTED_EDGE ( 'NONE', *, *, #58082, .T. ) ;
#39386 = CARTESIAN_POINT ( 'NONE',  ( 0.3675815128205912052, 7.689697408877274931, 9.574637318041988365 ) ) ;
#39388 = EDGE_CURVE ( 'NONE', #61571, #63912, #21608, .T. ) ;
#39389 = CYLINDRICAL_SURFACE ( 'NONE', #42611, 12.75000000000000178 ) ;
#39390 = VERTEX_POINT ( 'NONE', #8555 ) ;
#39391 = CARTESIAN_POINT ( 'NONE',  ( 0.2650492594609234476, 10.66007682546625546, -6.027447650185258077 ) ) ;
#39392 = ORIENTED_EDGE ( 'NONE', *, *, #2763, .F. ) ;
#39393 = VERTEX_POINT ( 'NONE', #43812 ) ;
#39394 = CARTESIAN_POINT ( 'NONE',  ( -26.04781212229947229, 12.02259665859258675, 6.141663214695094020 ) ) ;
#39395 = AXIS2_PLACEMENT_3D ( 'NONE', #52181, #25019, #65549 ) ;
#39396 = CARTESIAN_POINT ( 'NONE',  ( 1.819964709949660975, -30.58339181399214723, 15.25524951094025639 ) ) ;
#39397 = DIRECTION ( 'NONE',  ( 0.000000000000000000, 0.01356324068817998940, -0.9999080150203990547 ) ) ;
#39398 = CIRCLE ( 'NONE', #60622, 6.936499999999989896 ) ;
#39399 = EDGE_CURVE ( 'NONE', #29699, #45790, #48815, .T. ) ;
#39400 = CARTESIAN_POINT ( 'NONE',  ( 23.11218445469129890, -3.961089654181102482, 11.33103279473652591 ) ) ;
#39401 = DIRECTION ( 'NONE',  ( 0.000000000000000000, 0.6943713148249588407, -0.7196168960969843154 ) ) ;
#39402 = LINE ( 'NONE', #49723, #24595 ) ;
#39403 = ORIENTED_EDGE ( 'NONE', *, *, #13601, .F. ) ;
#39404 = AXIS2_PLACEMENT_3D ( 'NONE', #16095, #12403, #2118 ) ;
#39405 =( BOUNDED_CURVE ( )  B_SPLINE_CURVE ( 3, ( #1439, #16396, #46328, #22022 ),
 .UNSPECIFIED., .F., .F. ) 
 B_SPLINE_CURVE_WITH_KNOTS ( ( 4, 4 ),
 ( 5.457079895576344875, 5.508852664714265046 ),
 .UNSPECIFIED. ) 
 CURVE ( )  GEOMETRIC_REPRESENTATION_ITEM ( )  RATIONAL_B_SPLINE_CURVE ( ( 1.000000000000000000, 0.9997766441710536078, 0.9997766441710536078, 1.000000000000000000 ) ) 
 REPRESENTATION_ITEM ( '' )  );
#39406 = ORIENTED_EDGE ( 'NONE', *, *, #44096, .T. ) ;
#39407 = CARTESIAN_POINT ( 'NONE',  ( 35.00000000000000000, 4.705694406421931860E-17, -3.469127814946512892E-15 ) ) ;
#39408 = ORIENTED_EDGE ( 'NONE', *, *, #44921, .T. ) ;
#39409 = VECTOR ( 'NONE', #13179, 1000.000000000000000 ) ;
#39410 = DIRECTION ( 'NONE',  ( -1.000000000000000000, 0.000000000000000000, 0.000000000000000000 ) ) ;
#39411 = CARTESIAN_POINT ( 'NONE',  ( 0.2869720083484326167, -10.50600528807143164, -6.306330337780625683 ) ) ;
#39412 = CARTESIAN_POINT ( 'NONE',  ( 5.515188684475870851, -0.003857086913166417504, -0.003709313826049733063 ) ) ;
#39413 = DIRECTION ( 'NONE',  ( 0.000000000000000000, 0.8835120444460240474, -0.4684084406997882088 ) ) ;
#39414 = CYLINDRICAL_SURFACE ( 'NONE', #28884, 7.499999999999988454 ) ;
#39415 = DIRECTION ( 'NONE',  ( 1.000000000000000000, 0.000000000000000000, 0.000000000000000000 ) ) ;
#39416 = ORIENTED_EDGE ( 'NONE', *, *, #10879, .T. ) ;
#39417 = B_SPLINE_CURVE_WITH_KNOTS ( 'NONE', 3,
 ( #27193, #17223, #37495, #57801, #12222, #34128, #29169, #63406, #49465, #28187, #53120, #59412, #48475, #18857, #43797, #7911, #39123, #3596, #8540, #48156, #2614, #18209 ),
 .UNSPECIFIED., .F., .F.,
 ( 4, 2, 2, 2, 2, 2, 2, 2, 2, 2, 4 ),
 ( 0.000000000000000000, 0.001318687870781999920, 0.001978031806173001072, 0.002637375741564002007, 0.003956063612346002144, 0.004615407547737001778, 0.005274751483128001413, 0.006593439353909998080, 0.007912127224691993879, 0.009230815095473991413, 0.01054950296625598721 ),
 .UNSPECIFIED. ) ;
#39418 = ORIENTED_EDGE ( 'NONE', *, *, #23067, .F. ) ;
#39419 = FACE_OUTER_BOUND ( 'NONE', #43521, .T. ) ;
#39420 = CARTESIAN_POINT ( 'NONE',  ( -35.00000000000000000, 6.547236723514155976, -9.752226076388824438 ) ) ;
#39421 = B_SPLINE_CURVE_WITH_KNOTS ( 'NONE', 3,
 ( #55222, #44571, #19976, #9323, #35256, #30593, #55564, #64854, #49918, #10005, #30286, #50900, #19336, #5024, #18, #60876, #15316, #25621, #35592, #24643, #55886, #35900, #4370, #40920, #9022, #44920, #19669, #29304, #46249, #10991, #51889, #10636, #36586, #16310, #20948, #37219, #51575, #41226, #47548, #26599, #56889, #22260, #11314, #11957, #41556, #30928, #61510, #62181 ),
 .UNSPECIFIED., .F., .F.,
 ( 4, 2, 2, 2, 2, 2, 2, 2, 2, 2, 2, 2, 2, 2, 2, 2, 2, 2, 2, 2, 2, 2, 2, 4 ),
 ( 8.673617379884035472E-19, 0.003028155528123375149, 0.004542233292185064893, 0.006056311056246753768, 0.007570388820308435705, 0.009084466584370117642, 0.01211262211249347978, 0.01514077764061684192, 0.01816893316874019712, 0.02119708869686355926, 0.02271116646092524380, 0.02422524422498692487, 0.02725339975311028701, 0.02876747751717196808, 0.03028155528123365262, 0.03330971080935701129, 0.03482378857341869582, 0.03633786633748037342, 0.03936602186560374944, 0.04239417739372711852, 0.04390825515778881000, 0.04542233292185050147, 0.04693641068591217907, 0.04845048844997387055 ),
 .UNSPECIFIED. ) ;
#39422 = LINE ( 'NONE', #30434, #24494 ) ;
#39423 = CIRCLE ( 'NONE', #12903, 6.936499999999989008 ) ;
#39424 = CIRCLE ( 'NONE', #1186, 6.936499999999988120 ) ;
#39425 = ORIENTED_EDGE ( 'NONE', *, *, #44633, .F. ) ;
#39426 = CIRCLE ( 'NONE', #47949, 6.936499999999987232 ) ;
#39427 = CARTESIAN_POINT ( 'NONE',  ( -27.45775109278351067, 10.51123867646838583, -8.471355351200609007 ) ) ;
#39428 = CARTESIAN_POINT ( 'NONE',  ( 7.266099666122742384, -5.675241298374717580, -12.25103963726659906 ) ) ;
#39429 = CARTESIAN_POINT ( 'NONE',  ( 35.00000000000000000, 3.614449339633649227, 11.17622378668002092 ) ) ;
#39430 = CARTESIAN_POINT ( 'NONE',  ( 2.000000000000001776, -7.414200355365243134, -1.131208685655240798 ) ) ;
#39431 = CARTESIAN_POINT ( 'NONE',  ( 2.907497136251069314, -5.319973245618573543, -5.781215374755531933 ) ) ;
#39432 = ORIENTED_EDGE ( 'NONE', *, *, #20320, .T. ) ;
#39433 = DIRECTION ( 'NONE',  ( -1.000000000000000000, 0.000000000000000000, 0.000000000000000000 ) ) ;
#39434 = DIRECTION ( 'NONE',  ( 0.000000000000000000, 0.01356324068818000848, -0.9999080150203990547 ) ) ;
#39435 = CARTESIAN_POINT ( 'NONE',  ( 5.520433897694421610, -0.002108682515300382403, -0.01491416502703810272 ) ) ;
#39436 = AXIS2_PLACEMENT_3D ( 'NONE', #16755, #26407, #30415 ) ;
#39437 = EDGE_CURVE ( 'NONE', #10755, #7525, #26762, .T. ) ;
#39438 = AXIS2_PLACEMENT_3D ( 'NONE', #40160, #46167, #51156 ) ;
#39439 = CARTESIAN_POINT ( 'NONE',  ( 2.440552418640497656, -6.568204543009798613, -4.020120046181113516 ) ) ;
#39440 = CARTESIAN_POINT ( 'NONE',  ( 0.8320506296491623210, -4.610676791972267985, -11.54877388447409814 ) ) ;
#39441 = ORIENTED_EDGE ( 'NONE', *, *, #41482, .T. ) ;
#39442 = CARTESIAN_POINT ( 'NONE',  ( 2.297017764050091948, -2.462009443075658943, 7.246120070222751508 ) ) ;
#39443 = CARTESIAN_POINT ( 'NONE',  ( 6.361445718264521432, -4.355102044641763648, 11.18181944858514498 ) ) ;
#39444 = CIRCLE ( 'NONE', #1267, 7.499999999999988454 ) ;
#39445 = CARTESIAN_POINT ( 'NONE',  ( 1.074417311476293158, -25.72614907888524982, -15.66246854766675156 ) ) ;
#39446 = ORIENTED_EDGE ( 'NONE', *, *, #30941, .F. ) ;
#39447 = DIRECTION ( 'NONE',  ( -1.000000000000000000, 0.000000000000000000, 0.000000000000000000 ) ) ;
#39448 = CARTESIAN_POINT ( 'NONE',  ( -28.19089594411849475, -12.81260937809825862, -4.263902777033699465 ) ) ;
#39449 = CARTESIAN_POINT ( 'NONE',  ( 17.86634709757764838, -9.034895380895633821, 10.05927542744126946 ) ) ;
#39450 = CIRCLE ( 'NONE', #25649, 2.899999999999995914 ) ;
#39451 = CARTESIAN_POINT ( 'NONE',  ( -21.23983773598477498, -7.447593303288433830, 25.00000000000000000 ) ) ;
#39452 = CARTESIAN_POINT ( 'NONE',  ( -8.384530407289302545, -9.055240063205157952, -10.03793618941832655 ) ) ;
#39453 = EDGE_CURVE ( 'NONE', #48767, #48483, #40720, .T. ) ;
#39454 = CARTESIAN_POINT ( 'NONE',  ( 1.283627346227448118, 12.28700367512568725, -2.725559306499256262 ) ) ;
#39455 = EDGE_LOOP ( 'NONE', ( #24073, #29396, #1739, #61419 ) ) ;
#39456 = CARTESIAN_POINT ( 'NONE',  ( 2.298277635560276089, -7.246601281227238900, 2.461898367585356961 ) ) ;
#39457 = VECTOR ( 'NONE', #58837, 1000.000000000000000 ) ;
#39458 = CARTESIAN_POINT ( 'NONE',  ( 0.2638984909335716500, 10.70468911391672684, -5.950360275954944989 ) ) ;
#39459 = CARTESIAN_POINT ( 'NONE',  ( 0.3654063281920759687, -9.573804659448610366, -7.689576266239762425 ) ) ;
#39460 = CARTESIAN_POINT ( 'NONE',  ( 3.152665057736233845, -4.725420687649230622, 6.378477742801980988 ) ) ;
#39461 = CYLINDRICAL_SURFACE ( 'NONE', #32206, 2.899999999999994582 ) ;
#39462 = CARTESIAN_POINT ( 'NONE',  ( -35.00000000000000000, -14.99999999999998757, 0.000000000000000000 ) ) ;
#39463 = EDGE_CURVE ( 'NONE', #65264, #41230, #63916, .T. ) ;
#39464 = CARTESIAN_POINT ( 'NONE',  ( -27.04788180060269553, 2.650714769830310846, 1.844972430941732355 ) ) ;
#39465 = CARTESIAN_POINT ( 'NONE',  ( -27.31188777422505609, -8.574970748528183861, -8.395320217058435119 ) ) ;
#39466 = AXIS2_PLACEMENT_3D ( 'NONE', #17274, #6653, #1980 ) ;
#39467 = EDGE_LOOP ( 'NONE', ( #29279, #26412, #58748, #2153 ) ) ;
#39468 = ADVANCED_FACE ( 'NONE', ( #12892 ), #53802, .T. ) ;
#39469 = ORIENTED_EDGE ( 'NONE', *, *, #3001, .T. ) ;
#39470 = CARTESIAN_POINT ( 'NONE',  ( 5.514970785353741078, -0.003415090918276162107, 0.003262412238248703009 ) ) ;
#39471 = ORIENTED_EDGE ( 'NONE', *, *, #13403, .F. ) ;
#39473 = CARTESIAN_POINT ( 'NONE',  ( 3.152665057734062248, -7.609997527621111146, 2.258875078502258216 ) ) ;
#39472 = VECTOR ( 'NONE', #1854, 1000.000000000000000 ) ;
#39474 = AXIS2_PLACEMENT_3D ( 'NONE', #5168, #60690, #18255 ) ;
#39475 = CIRCLE ( 'NONE', #21453, 2.899999999999994582 ) ;
#39476 = EDGE_CURVE ( 'NONE', #54467, #7370, #3611, .T. ) ;
#39477 = DIRECTION ( 'NONE',  ( 0.000000000000000000, 0.000000000000000000, 1.000000000000000000 ) ) ;
#39478 = ORIENTED_EDGE ( 'NONE', *, *, #57273, .F. ) ;
#39479 = DIRECTION ( 'NONE',  ( -1.000000000000000000, 0.000000000000000000, 0.000000000000000000 ) ) ;
#39480 = CARTESIAN_POINT ( 'NONE',  ( 2.835339799623981971, 1.682641786445544296, -7.649567297875980998 ) ) ;
#39482 = EDGE_CURVE ( 'NONE', #58379, #21179, #53483, .T. ) ;
#39481 = CARTESIAN_POINT ( 'NONE',  ( 24.68094058364964027, 0.8458801819018304524, 13.47910264936496105 ) ) ;
#39483 = ORIENTED_EDGE ( 'NONE', *, *, #29801, .T. ) ;
#39484 = ORIENTED_EDGE ( 'NONE', *, *, #41490, .F. ) ;
#39485 = CARTESIAN_POINT ( 'NONE',  ( 2.266490820343224577, -7.230273269342692544, -2.476945027124343390 ) ) ;
#39486 = CARTESIAN_POINT ( 'NONE',  ( -35.00000000000000000, -11.47758908105692655, -2.497432891016966749 ) ) ;
#39487 = ORIENTED_EDGE ( 'NONE', *, *, #56007, .T. ) ;
#39488 = CARTESIAN_POINT ( 'NONE',  ( 6.722269201495262081, -7.162924562234429970, -9.635873505962649688 ) ) ;
#39489 = VERTEX_POINT ( 'NONE', #19191 ) ;
#39490 = CIRCLE ( 'NONE', #36316, 4.000000000000000000 ) ;
#39491 = CARTESIAN_POINT ( 'NONE',  ( -19.47984447937493613, -3.750539801530005768, -11.39883551934754102 ) ) ;
#39492 = FACE_OUTER_BOUND ( 'NONE', #14878, .T. ) ;
#39493 = CARTESIAN_POINT ( 'NONE',  ( -7.181456785175555524, 8.540743096806467705, -10.45493698471458188 ) ) ;
#39494 = DIRECTION ( 'NONE',  ( 1.000000000000000000, -0.000000000000000000, 0.000000000000000000 ) ) ;
#39496 = EDGE_CURVE ( 'NONE', #62930, #52024, #28843, .T. ) ;
#39495 = VECTOR ( 'NONE', #55309, 1000.000000000000000 ) ;
#39497 = DIRECTION ( 'NONE',  ( -1.000000000000000000, 0.000000000000000000, 0.000000000000000000 ) ) ;
#39498 = ORIENTED_EDGE ( 'NONE', *, *, #16135, .F. ) ;
#39499 = CARTESIAN_POINT ( 'NONE',  ( 1.719304012339893051, -12.70777170743898310, 0.7661785589588769874 ) ) ;
#39500 = CARTESIAN_POINT ( 'NONE',  ( -18.06060982367787204, 5.590226830146772130, 10.62101905373911315 ) ) ;
#39501 = AXIS2_PLACEMENT_3D ( 'NONE', #51934, #46601, #47921 ) ;
#39502 = EDGE_CURVE ( 'NONE', #14915, #5644, #62874, .T. ) ;
#39503 = DIRECTION ( 'NONE',  ( 0.000000000000000000, -0.5155538571770286183, 0.8568571761675850551 ) ) ;
#39504 = CARTESIAN_POINT ( 'NONE',  ( 37.00000000000000711, 11.59605747147793942, 5.300372733891518529 ) ) ;
#39505 = LINE ( 'NONE', #59799, #12557 ) ;
#39506 = CARTESIAN_POINT ( 'NONE',  ( 24.06471749115019776, -2.481826756221663821, 13.27386424782494601 ) ) ;
#39507 = AXIS2_PLACEMENT_3D ( 'NONE', #60951, #16381, #36653 ) ;
#39508 = CARTESIAN_POINT ( 'NONE',  ( -22.27706485742869091, -2.154081322712202873, -2.985151051101508468 ) ) ;
#39509 = CARTESIAN_POINT ( 'NONE',  ( -35.00000000000000000, -11.54110654723650420, 2.185196060783841432 ) ) ;
#39510 = CARTESIAN_POINT ( 'NONE',  ( 0.2648978790185584908, -9.295532325666394868, -7.972372351883127095 ) ) ;
#39511 = VERTEX_POINT ( 'NONE', #18573 ) ;
#39512 = CARTESIAN_POINT ( 'NONE',  ( 35.00000000000000000, -2.220215194441986561, -11.98254675519227597 ) ) ;
#39513 = CIRCLE ( 'NONE', #54400, 5.000000000000000888 ) ;
#39514 = EDGE_LOOP ( 'NONE', ( #351, #38513, #41967, #57395 ) ) ;
#39515 = DIRECTION ( 'NONE',  ( 0.000000000000000000, -0.01356324068817991828, 0.9999080150203990547 ) ) ;
#39516 = CARTESIAN_POINT ( 'NONE',  ( 2.261269890822071194, -7.499479675451350857, -1.464004156081723185 ) ) ;
#39517 = CARTESIAN_POINT ( 'NONE',  ( 5.514970785353741078, -0.004588761610585018538, 0.001117786416802603452 ) ) ;
#39518 = CARTESIAN_POINT ( 'NONE',  ( 0.2648978790185619880, 9.465406350830608773, 7.769924372105235122 ) ) ;
#39519 = DIRECTION ( 'NONE',  ( 0.000000000000000000, -0.7790879021242442803, 0.6269146997508066033 ) ) ;
#39520 = ORIENTED_EDGE ( 'NONE', *, *, #56934, .F. ) ;
#39521 = CARTESIAN_POINT ( 'NONE',  ( 2.827825597296806048, 0.5449445831288285413, -9.007857251166427659 ) ) ;
#39522 = CARTESIAN_POINT ( 'NONE',  ( 2.305787727787084407, 2.461236246751170142, -7.249469779319884566 ) ) ;
#39523 = VECTOR ( 'NONE', #22890, 1000.000000000000000 ) ;
#39524 = DIRECTION ( 'NONE',  ( -1.000000000000000000, 0.000000000000000000, 0.000000000000000000 ) ) ;
#39525 = FACE_OUTER_BOUND ( 'NONE', #22293, .T. ) ;
#39526 = EDGE_CURVE ( 'NONE', #1051, #40174, #63744, .T. ) ;
#39527 = VECTOR ( 'NONE', #9339, 1000.000000000000000 ) ;
#39528 = CARTESIAN_POINT ( 'NONE',  ( 0.000000000000000000, -34.50000000000000000, 0.000000000000000000 ) ) ;
#39529 = EDGE_CURVE ( 'NONE', #1056, #3801, #38826, .T. ) ;
#39530 = ORIENTED_EDGE ( 'NONE', *, *, #30546, .F. ) ;
#39531 = CARTESIAN_POINT ( 'NONE',  ( -42.50000000000000000, -2.710505431213761085E-17, 1.201363017033314212E-18 ) ) ;
#39532 = ORIENTED_EDGE ( 'NONE', *, *, #3489, .F. ) ;
#39533 = CARTESIAN_POINT ( 'NONE',  ( 2.288423627607474753, 6.543055113184276017, -3.963881558061893351 ) ) ;
#39534 = CARTESIAN_POINT ( 'NONE',  ( -25.42680463514451361, -3.516354806213008111, 1.651747791411765753 ) ) ;
#39535 = EDGE_CURVE ( 'NONE', #29592, #64891, #12042, .T. ) ;
#39536 = CARTESIAN_POINT ( 'NONE',  ( -10.00000000000000178, 0.000000000000000000, 0.000000000000000000 ) ) ;
#39537 = AXIS2_PLACEMENT_3D ( 'NONE', #58137, #12553, #32832 ) ;
#39538 = DIRECTION ( 'NONE',  ( 0.000000000000000000, 0.01356324068818000328, -0.9999080150203990547 ) ) ;
#39539 = AXIS2_PLACEMENT_3D ( 'NONE', #10494, #63250, #30457 ) ;
#39540 = EDGE_CURVE ( 'NONE', #20729, #16846, #61939, .T. ) ;
#39541 = VERTEX_POINT ( 'NONE', #30470 ) ;
#39542 = ORIENTED_EDGE ( 'NONE', *, *, #53734, .F. ) ;
#39543 = CARTESIAN_POINT ( 'NONE',  ( -35.00000000000000000, -11.68758509253249223, 1.171570255487406786 ) ) ;
#39544 = CARTESIAN_POINT ( 'NONE',  ( -36.00000000000000711, 11.90598845858533750, 4.561791185930457182 ) ) ;
#39546 = CIRCLE ( 'NONE', #36369, 7.499999999999988454 ) ;
#39545 = CARTESIAN_POINT ( 'NONE',  ( 2.000000000000001776, 6.441884263200846839, -2.217201541069800275 ) ) ;
#39547 = CARTESIAN_POINT ( 'NONE',  ( 0.3106921474978470155, 12.25904950202577659, 0.2354703039888528804 ) ) ;
#39548 = CARTESIAN_POINT ( 'NONE',  ( 2.781367136452733924, 6.608147481822127745, -4.171010984503221053 ) ) ;
#39549 = AXIS2_PLACEMENT_3D ( 'NONE', #34883, #9974, #40550 ) ;
#39550 = DIRECTION ( 'NONE',  ( 0.000000000000000000, 0.7381862504171974315, -0.6745969609292639113 ) ) ;
#39551 = DIRECTION ( 'NONE',  ( -1.000000000000000000, 0.000000000000000000, 0.000000000000000000 ) ) ;
#39552 = ORIENTED_EDGE ( 'NONE', *, *, #30666, .F. ) ;
#39553 = EDGE_CURVE ( 'NONE', #1479, #40758, #8728, .T. ) ;
#39554 = ORIENTED_EDGE ( 'NONE', *, *, #32185, .T. ) ;
#39555 = ORIENTED_EDGE ( 'NONE', *, *, #44421, .T. ) ;
#39556 = CARTESIAN_POINT ( 'NONE',  ( 35.00000000000000000, -6.564808257521689505, 10.93004082984025160 ) ) ;
#39557 = CARTESIAN_POINT ( 'NONE',  ( 5.514970785353741078, -0.001897634820904980750, -0.004324946436530298539 ) ) ;
#39558 = VERTEX_POINT ( 'NONE', #19848 ) ;
#39559 = DIRECTION ( 'NONE',  ( 0.000000000000000000, 0.01356324068817992175, -0.9999080150203990547 ) ) ;
#39560 = FACE_BOUND ( 'NONE', #41708, .T. ) ;
#39561 = ORIENTED_EDGE ( 'NONE', *, *, #42927, .T. ) ;
#39562 = CARTESIAN_POINT ( 'NONE',  ( 37.00000000000000711, 4.561791185930414549, -11.90598845858535704 ) ) ;
#39564 = EDGE_CURVE ( 'NONE', #40351, #40103, #25483, .T. ) ;
#39563 = CARTESIAN_POINT ( 'NONE',  ( 37.00000000000000711, -4.339012074899872395, 10.91536515067652324 ) ) ;
#39565 = CARTESIAN_POINT ( 'NONE',  ( 3.663040366865097486, -11.05188025280430786, 4.676643728192003913 ) ) ;
#39566 = EDGE_LOOP ( 'NONE', ( #53127, #52852, #30563, #55948 ) ) ;
#39567 = VERTEX_POINT ( 'NONE', #50452 ) ;
#39568 = CARTESIAN_POINT ( 'NONE',  ( -35.00000000000000000, 0.000000000000000000, 0.000000000000000000 ) ) ;
#39570 = ORIENTED_EDGE ( 'NONE', *, *, #46028, .T. ) ;
#39569 = EDGE_CURVE ( 'NONE', #17690, #24391, #386, .T. ) ;
#39571 = CARTESIAN_POINT ( 'NONE',  ( 10.66646312117316420, 7.972760762573107840, 10.89565866104123515 ) ) ;
#39572 = ORIENTED_EDGE ( 'NONE', *, *, #42402, .T. ) ;
#39573 = AXIS2_PLACEMENT_3D ( 'NONE', #34048, #29085, #43366 ) ;
#39574 = AXIS2_PLACEMENT_3D ( 'NONE', #30244, #50540, #65784 ) ;
#39575 = VERTEX_POINT ( 'NONE', #56067 ) ;
#39577 = EDGE_CURVE ( 'NONE', #1393, #20343, #51236, .T. ) ;
#39576 = VERTEX_POINT ( 'NONE', #49783 ) ;
#39578 = CARTESIAN_POINT ( 'NONE',  ( 37.00000000000000711, 4.705694406421931860E-17, -3.469127814946512892E-15 ) ) ;
#39579 = CARTESIAN_POINT ( 'NONE',  ( -16.81801275797669604, -34.49999999999998579, -5.265606433705287692 ) ) ;
#39580 = CIRCLE ( 'NONE', #14082, 7.938172270156617749 ) ;
#39581 = VECTOR ( 'NONE', #13372, 1000.000000000000000 ) ;
#39582 = DIRECTION ( 'NONE',  ( -1.000000000000000000, 0.000000000000000000, 0.000000000000000000 ) ) ;
#39583 = CYLINDRICAL_SURFACE ( 'NONE', #537, 4.999999999999999112 ) ;
#39584 = ORIENTED_EDGE ( 'NONE', *, *, #44146, .T. ) ;
#39585 = ADVANCED_FACE ( 'NONE', ( #60401 ), #5216, .T. ) ;
#39586 = CARTESIAN_POINT ( 'NONE',  ( 2.259830038564998311, -7.131511317046838272, -2.742210045659254192 ) ) ;
#39587 = VERTEX_POINT ( 'NONE', #9201 ) ;
#39588 = DIRECTION ( 'NONE',  ( 0.000000000000000000, -0.01356324068818000328, 0.9999080150203990547 ) ) ;
#39589 = CARTESIAN_POINT ( 'NONE',  ( -18.25006854224444908, -9.443202773001939221, -9.647586298549935435 ) ) ;
#39590 = EDGE_CURVE ( 'NONE', #32821, #45493, #20506, .T. ) ;
#39591 = EDGE_LOOP ( 'NONE', ( #63654, #40813, #30283, #7113 ) ) ;
#39592 = CARTESIAN_POINT ( 'NONE',  ( 1.287602823388473983, 9.987902848014591939, -7.659913635101546880 ) ) ;
#39593 = CIRCLE ( 'NONE', #32166, 12.18649999999999878 ) ;
#39594 = CARTESIAN_POINT ( 'NONE',  ( 0.2648321136542700627, 4.054947570138896396, 11.55519783395229005 ) ) ;
#39595 = CARTESIAN_POINT ( 'NONE',  ( 2.251152103363641022, -6.676162264140654834, -3.709836606813393445 ) ) ;
#39596 = ORIENTED_EDGE ( 'NONE', *, *, #4983, .F. ) ;
#39597 = CIRCLE ( 'NONE', #19432, 4.999999999999999112 ) ;
#39598 = ORIENTED_EDGE ( 'NONE', *, *, #26930, .F. ) ;
#39599 = CARTESIAN_POINT ( 'NONE',  ( 0.5547464869798215403, 6.433541106625093597, 10.53334899235172983 ) ) ;
#39600 = ORIENTED_EDGE ( 'NONE', *, *, #33501, .F. ) ;
#39601 = DIRECTION ( 'NONE',  ( 0.000000000000000000, -0.4198891015602717602, 0.9075754196709537869 ) ) ;
#39602 = CARTESIAN_POINT ( 'NONE',  ( -19.12534438730314434, -13.43125637399242756, -1.404165056817866297 ) ) ;
#39603 = CARTESIAN_POINT ( 'NONE',  ( 3.047904605210433271, 7.047014837597106229, -3.577928268981992233 ) ) ;
#39604 = CARTESIAN_POINT ( 'NONE',  ( 0.2759803524722224677, -9.260954523383681192, -8.018167820447592575 ) ) ;
#39605 = CARTESIAN_POINT ( 'NONE',  ( 1.547277799338546700, -9.261681528764437843, 8.651049845884134726 ) ) ;
#39606 = VERTEX_POINT ( 'NONE', #55087 ) ;
#39607 = CARTESIAN_POINT ( 'NONE',  ( -27.32337605527166957, -1.812546145273346010, 2.404211887218381527 ) ) ;
#39608 = CARTESIAN_POINT ( 'NONE',  ( 35.00000000000000000, -2.696588552979144460, -12.46157735505188313 ) ) ;
#39609 = ADVANCED_FACE ( 'NONE', ( #25161 ), #4233, .T. ) ;
#39610 = VECTOR ( 'NONE', #60368, 1000.000000000000000 ) ;
#39611 = DIRECTION ( 'NONE',  ( 0.000000000000000000, 0.01356324068817998940, -0.9999080150203990547 ) ) ;
#39612 =( BOUNDED_CURVE ( )  B_SPLINE_CURVE ( 3, ( #8489, #64344, #18812, #13791 ),
 .UNSPECIFIED., .F., .F. ) 
 B_SPLINE_CURVE_WITH_KNOTS ( ( 4, 4 ),
 ( 2.655715767958479745, 2.751510998045912704 ),
 .UNSPECIFIED. ) 
 CURVE ( )  GEOMETRIC_REPRESENTATION_ITEM ( )  RATIONAL_B_SPLINE_CURVE ( ( 1.000000000000000000, 0.9992354190151078175, 0.9992354190151078175, 1.000000000000000000 ) ) 
 REPRESENTATION_ITEM ( '' )  );
#39613 = DIRECTION ( 'NONE',  ( 1.000000000000000000, 0.000000000000000000, 0.000000000000000000 ) ) ;
#39614 = CARTESIAN_POINT ( 'NONE',  ( 2.241317068080776131, -5.906676463196257387, -4.836852665784649119 ) ) ;
#39615 = DIRECTION ( 'NONE',  ( 0.000000000000000000, -0.01356324068817999114, 0.9999080150203989437 ) ) ;
#39616 = FACE_OUTER_BOUND ( 'NONE', #39218, .T. ) ;
#39617 = ADVANCED_FACE ( 'NONE', ( #15501 ), #9112, .F. ) ;
#39618 = VECTOR ( 'NONE', #11829, 1000.000000000000000 ) ;
#39619 = CIRCLE ( 'NONE', #10965, 12.18650000000000055 ) ;
#39620 = AXIS2_PLACEMENT_3D ( 'NONE', #50203, #45511, #45198 ) ;
#39621 = ORIENTED_EDGE ( 'NONE', *, *, #34488, .T. ) ;
#39622 = CARTESIAN_POINT ( 'NONE',  ( -35.00000000000000000, 0.000000000000000000, 0.000000000000000000 ) ) ;
#39623 = ORIENTED_EDGE ( 'NONE', *, *, #43704, .T. ) ;
#39624 = CARTESIAN_POINT ( 'NONE',  ( 0.3164563675027610712, 1.892265234253275530, -12.11636128244742494 ) ) ;
#39625 = DIRECTION ( 'NONE',  ( 0.000000000000000000, -0.5243256840888622650, -0.8515178078024832065 ) ) ;
#39626 = CARTESIAN_POINT ( 'NONE',  ( 2.963017218115625351, -7.522800244854591867, 2.328652339224321022 ) ) ;
#39627 = CIRCLE ( 'NONE', #16292, 12.18650000000000055 ) ;
#39628 = CARTESIAN_POINT ( 'NONE',  ( -37.00000000000000711, -6.946017217729864690, -10.01317267707894310 ) ) ;
#39629 = ORIENTED_EDGE ( 'NONE', *, *, #55988, .F. ) ;
#39630 = EDGE_CURVE ( 'NONE', #11130, #42300, #38844, .T. ) ;
#39631 = AXIS2_PLACEMENT_3D ( 'NONE', #60457, #9925, #14881 ) ;
#39632 = VERTEX_POINT ( 'NONE', #34783 ) ;
#39633 = ORIENTED_EDGE ( 'NONE', *, *, #24004, .T. ) ;
#39634 = CARTESIAN_POINT ( 'NONE',  ( 29.73654696047771751, -7.541957041131760242, 9.346911106860231300 ) ) ;
#39635 = EDGE_CURVE ( 'NONE', #15981, #63362, #30782, .T. ) ;
#39636 = AXIS2_PLACEMENT_3D ( 'NONE', #10930, #62129, #51834 ) ;
#39637 = CARTESIAN_POINT ( 'NONE',  ( 36.00000000000000711, -4.074242145636093326, -12.08151691381188719 ) ) ;
#39638 = EDGE_LOOP ( 'NONE', ( #37095, #2163, #42393, #34171 ) ) ;
#39639 = DIRECTION ( 'NONE',  ( 0.000000000000000000, 0.01356324068817998940, -0.9999080150203990547 ) ) ;
#39640 = CYLINDRICAL_SURFACE ( 'NONE', #63384, 4.999999999999999112 ) ;
#39641 = CARTESIAN_POINT ( 'NONE',  ( 0.2915757698887310734, -9.248369946372577033, 8.040595355212914797 ) ) ;
#39642 = CYLINDRICAL_SURFACE ( 'NONE', #34372, 12.18649999999999878 ) ;
#39643 = ORIENTED_EDGE ( 'NONE', *, *, #32637, .F. ) ;
#39644 = DIRECTION ( 'NONE',  ( 1.000000000000000000, 0.000000000000000000, 0.000000000000000000 ) ) ;
#39645 = VECTOR ( 'NONE', #10972, 1000.000000000000000 ) ;
#39646 = CARTESIAN_POINT ( 'NONE',  ( -11.31614860309490922, -29.68432482266972272, -9.654990830001235480 ) ) ;
#39647 = DIRECTION ( 'NONE',  ( 0.000000000000000000, 0.4935949184179200810, -0.8696919319575219243 ) ) ;
#39649 = ORIENTED_EDGE ( 'NONE', *, *, #9714, .T. ) ;
#39648 = CARTESIAN_POINT ( 'NONE',  ( 5.516018279890452902, 0.005042957932159071975, 0.004525000489649949435 ) ) ;
#39650 = CARTESIAN_POINT ( 'NONE',  ( -37.00000000000000711, -11.90598845858530730, -4.561791185930540671 ) ) ;
#39651 = ORIENTED_EDGE ( 'NONE', *, *, #54912, .T. ) ;
#39652 = DIRECTION ( 'NONE',  ( 0.000000000000000000, -0.01356324068817998940, 0.9999080150203990547 ) ) ;
#39653 = ORIENTED_EDGE ( 'NONE', *, *, #25305, .T. ) ;
#39654 = FACE_OUTER_BOUND ( 'NONE', #36495, .T. ) ;
#39655 = CARTESIAN_POINT ( 'NONE',  ( 12.61303456006366552, -11.71602035781408269, -2.601723401083803289 ) ) ;
#39656 = EDGE_CURVE ( 'NONE', #8671, #4651, #240, .T. ) ;
#39657 = CARTESIAN_POINT ( 'NONE',  ( 35.00000000000000000, 4.705694406421931860E-17, -3.469127814946512892E-15 ) ) ;
#39658 = CARTESIAN_POINT ( 'NONE',  ( 0.7400311444011756778, -6.506979270898107792, -10.56075429936773880 ) ) ;
#39659 = AXIS2_PLACEMENT_3D ( 'NONE', #45735, #10814, #15786 ) ;
#39660 = CARTESIAN_POINT ( 'NONE',  ( 0.3610902822527200517, -12.27530799859939314, 0.2623004149194189116 ) ) ;
#39661 = CARTESIAN_POINT ( 'NONE',  ( -27.09602251845210219, -0.1644056400645331761, -2.320865065108511427 ) ) ;
#39662 = CARTESIAN_POINT ( 'NONE',  ( 0.3002738374340822580, -3.979745968261130695, -11.59380198135586326 ) ) ;
#39664 = ORIENTED_EDGE ( 'NONE', *, *, #27593, .F. ) ;
#39663 = DIRECTION ( 'NONE',  ( -1.000000000000000000, 0.000000000000000000, 0.000000000000000000 ) ) ;
#39665 = EDGE_CURVE ( 'NONE', #51949, #32084, #16706, .T. ) ;
#39666 = ORIENTED_EDGE ( 'NONE', *, *, #32416, .T. ) ;
#39667 = CARTESIAN_POINT ( 'NONE',  ( 11.12460659294225351, -13.44996865318204904, -1.166173210671453742 ) ) ;
#39668 = ORIENTED_EDGE ( 'NONE', *, *, #21216, .F. ) ;
#39669 = EDGE_CURVE ( 'NONE', #44514, #58860, #24671, .T. ) ;
#39670 = CIRCLE ( 'NONE', #58833, 4.999999999999999112 ) ;
#39671 = ORIENTED_EDGE ( 'NONE', *, *, #553, .F. ) ;
#39673 = CONICAL_SURFACE ( 'NONE', #41802, 7.938172270156617749, 1.280189991382167047 ) ;
#39672 = CARTESIAN_POINT ( 'NONE',  ( 1.014383007554945149, 1.731118468094080987, -12.37541872618880312 ) ) ;
#39674 = CARTESIAN_POINT ( 'NONE',  ( 3.152665057734040488, 0.000000000000000000, 0.000000000000000000 ) ) ;
#39675 = CARTESIAN_POINT ( 'NONE',  ( -27.08485414902839139, -2.214586389210154493, 0.5952588087544555817 ) ) ;
#39676 = CARTESIAN_POINT ( 'NONE',  ( -35.00000000000000000, 0.000000000000000000, 0.000000000000000000 ) ) ;
#39677 = CARTESIAN_POINT ( 'NONE',  ( -35.00000000000000000, 4.339012074900111315, -10.91536515067643620 ) ) ;
#39678 = VECTOR ( 'NONE', #55401, 1000.000000000000000 ) ;
#39679 = CARTESIAN_POINT ( 'NONE',  ( 0.3537226245948368875, 10.75912040401517267, -5.910416419900417218 ) ) ;
#39680 = EDGE_CURVE ( 'NONE', #29332, #11288, #36306, .T. ) ;
#39681 = CARTESIAN_POINT ( 'NONE',  ( 1.372161826076674362, -11.20801830616791328, -5.789954543171356605 ) ) ;
#39682 = EDGE_LOOP ( 'NONE', ( #52863, #53009, #60395, #27060 ) ) ;
#39683 = LINE ( 'NONE', #8442, #36055 ) ;
#39684 = VECTOR ( 'NONE', #52854, 1000.000000000000000 ) ;
#39685 = DIRECTION ( 'NONE',  ( 0.000000000000000000, 0.01356324068817999808, -0.9999080150203990547 ) ) ;
#39686 = CARTESIAN_POINT ( 'NONE',  ( 0.000000000000000000, 6.750946897830712778, 1.593658756657066355 ) ) ;
#39687 = B_SPLINE_CURVE_WITH_KNOTS ( 'NONE', 3,
 ( #27478, #47779, #58089, #2230, #22509, #42770, #63065, #17528, #37795, #12504, #41685, #1475, #41024 ),
 .UNSPECIFIED., .F., .F.,
 ( 4, 3, 3, 3, 4 ),
 ( 8.673617379884035472E-19, 6.607593386745688247E-05, 0.0001321518677373530843, 0.0001982171734706230282, 0.0002642860854759495302 ),
 .UNSPECIFIED. ) ;
#39688 = ORIENTED_EDGE ( 'NONE', *, *, #51338, .F. ) ;
#39689 = CONICAL_SURFACE ( 'NONE', #64134, 7.938172270156617749, 1.280189991382167047 ) ;
#39690 = PRODUCT_RELATED_PRODUCT_CATEGORY ( 'part', '', ( #49305 ) ) ;
#39691 = EDGE_CURVE ( 'NONE', #52755, #55501, #1669, .T. ) ;
#39692 = CARTESIAN_POINT ( 'NONE',  ( 41.46388549984528282, -1.589384660823696782, -18.83126657550987915 ) ) ;
#39693 = CIRCLE ( 'NONE', #36516, 5.000000000000000888 ) ;
#39694 = CARTESIAN_POINT ( 'NONE',  ( -35.05012975565874456, -0.01039213056760649075, 0.009279204628454365902 ) ) ;
#39695 = ORIENTED_EDGE ( 'NONE', *, *, #18915, .F. ) ;
#39696 = DIRECTION ( 'NONE',  ( 1.000000000000000000, 0.000000000000000000, 0.000000000000000000 ) ) ;
#39697 = DIRECTION ( 'NONE',  ( -1.000000000000000000, 0.000000000000000000, 0.000000000000000000 ) ) ;
#39698 = FACE_OUTER_BOUND ( 'NONE', #49830, .T. ) ;
#39699 = CARTESIAN_POINT ( 'NONE',  ( 37.00000000000000711, 4.705694406421931860E-17, -3.469127814946512892E-15 ) ) ;
#39700 = DIRECTION ( 'NONE',  ( 0.000000000000000000, 0.000000000000000000, -1.000000000000000000 ) ) ;
#39701 = ORIENTED_EDGE ( 'NONE', *, *, #14104, .T. ) ;
#39702 = CARTESIAN_POINT ( 'NONE',  ( 2.305787727787084407, 0.1666591538752685842, 7.654065630109507801 ) ) ;
#39703 = DIRECTION ( 'NONE',  ( 0.000000000000000000, 0.000000000000000000, 1.000000000000000000 ) ) ;
#39704 = CARTESIAN_POINT ( 'NONE',  ( -18.31776534785701216, 3.837936424772297794, -11.37033739218235695 ) ) ;
#39705 = ORIENTED_EDGE ( 'NONE', *, *, #58883, .F. ) ;
#39706 = CARTESIAN_POINT ( 'NONE',  ( 8.815713299111846979, 2.649613430600505914, 13.23998980317660035 ) ) ;
#39707 = CARTESIAN_POINT ( 'NONE',  ( 2.241526690369557429, 6.620271521148430871, 3.802233103835192640 ) ) ;
#39708 = ORIENTED_EDGE ( 'NONE', *, *, #5883, .F. ) ;
#39709 = EDGE_CURVE ( 'NONE', #32907, #3342, #16166, .T. ) ;
#39710 = EDGE_CURVE ( 'NONE', #64727, #8331, #60746, .T. ) ;
#39711 = AXIS2_PLACEMENT_3D ( 'NONE', #46747, #41091, #61370 ) ;
#39712 = AXIS2_PLACEMENT_3D ( 'NONE', #29200, #3934, #24198 ) ;
#39713 = ORIENTED_EDGE ( 'NONE', *, *, #40744, .F. ) ;
#39714 = ORIENTED_EDGE ( 'NONE', *, *, #54665, .T. ) ;
#39715 = DIRECTION ( 'NONE',  ( 1.000000000000000000, -0.000000000000000000, -0.000000000000000000 ) ) ;
#39716 = EDGE_CURVE ( 'NONE', #12670, #19302, #56539, .T. ) ;
#39717 = AXIS2_PLACEMENT_3D ( 'NONE', #11719, #32002, #47333 ) ;
#39718 = VERTEX_POINT ( 'NONE', #31460 ) ;
#39719 = CARTESIAN_POINT ( 'NONE',  ( 1.109979610370702918, -12.24510427445497029, -2.646302643132570243 ) ) ;
#39720 = DIRECTION ( 'NONE',  ( -1.000000000000000000, 0.000000000000000000, 0.000000000000000000 ) ) ;
#39721 = DIRECTION ( 'NONE',  ( 0.000000000000000000, 0.01356324068817992175, -0.9999080150203990547 ) ) ;
#39722 = CARTESIAN_POINT ( 'NONE',  ( -36.00000000000000711, -1.457575200925635528, 12.66641127287625501 ) ) ;
#39723 = AXIS2_PLACEMENT_3D ( 'NONE', #58034, #17131, #6506 ) ;
#39724 = CARTESIAN_POINT ( 'NONE',  ( -16.02805653289875920, -28.24868299250882941, 10.29995797863329621 ) ) ;
#39725 = CARTESIAN_POINT ( 'NONE',  ( 2.241534463349551753, 9.451863027432619807E-16, 7.634462073473348376 ) ) ;
#39727 = ORIENTED_EDGE ( 'NONE', *, *, #47319, .T. ) ;
#39726 = CARTESIAN_POINT ( 'NONE',  ( 1.549075743843701503, 7.618376504787362613, 10.12891450359415124 ) ) ;
#39728 = DIRECTION ( 'NONE',  ( -1.000000000000000000, 0.000000000000000000, 0.000000000000000000 ) ) ;
#39729 = EDGE_LOOP ( 'NONE', ( #37104, #40330, #52468, #5227 ) ) ;
#39730 = FACE_OUTER_BOUND ( 'NONE', #12824, .T. ) ;
#39731 = AXIS2_PLACEMENT_3D ( 'NONE', #1511, #21789, #16770 ) ;
#39732 = VERTEX_POINT ( 'NONE', #21493 ) ;
#39733 = VERTEX_POINT ( 'NONE', #56762 ) ;
#39734 = DIRECTION ( 'NONE',  ( 0.000000000000000000, -0.9847383929261636082, 0.1740410799127514174 ) ) ;
#39735 = CARTESIAN_POINT ( 'NONE',  ( 16.25880638382997745, -34.36679772354796114, 6.546306705357587852 ) ) ;
#39736 = ADVANCED_FACE ( 'NONE', ( #16507 ), #36776, .T. ) ;
#39737 = AXIS2_PLACEMENT_3D ( 'NONE', #63119, #38838, #58140 ) ;
#39738 = CARTESIAN_POINT ( 'NONE',  ( -47.00000000000000711, 0.000000000000000000, 0.000000000000000000 ) ) ;
#39739 = DIRECTION ( 'NONE',  ( 0.3865475372811021937, -0.2971585806051852408, -0.8730852074079749059 ) ) ;
#39740 = CARTESIAN_POINT ( 'NONE',  ( -35.00000000000000000, 0.000000000000000000, 0.000000000000000000 ) ) ;
#39741 = DIRECTION ( 'NONE',  ( -1.000000000000000000, 0.000000000000000000, 0.000000000000000000 ) ) ;
#39742 = ORIENTED_EDGE ( 'NONE', *, *, #343, .T. ) ;
#39743 = ORIENTED_EDGE ( 'NONE', *, *, #22590, .F. ) ;
#39744 = CARTESIAN_POINT ( 'NONE',  ( -36.00000000000000711, -5.710938531231627202, -11.39945968423477751 ) ) ;
#39745 = VERTEX_POINT ( 'NONE', #1555 ) ;
#39746 = VECTOR ( 'NONE', #43634, 1000.000000000000000 ) ;
#39747 = ORIENTED_EDGE ( 'NONE', *, *, #41222, .T. ) ;
#39748 = CARTESIAN_POINT ( 'NONE',  ( 2.241528039335008771, -1.341200777944199674, 7.515727438419998130 ) ) ;
#39749 = CARTESIAN_POINT ( 'NONE',  ( -22.30861784526116054, 0.8834205920623713348, -3.671054459752221444 ) ) ;
#39750 = DIRECTION ( 'NONE',  ( 0.000000000000000000, 0.01356324068817991828, -0.9999080150203990547 ) ) ;
#39751 = CARTESIAN_POINT ( 'NONE',  ( 0.000000000000000000, 0.000000000000000000, 0.000000000000000000 ) ) ;
#39752 = EDGE_CURVE ( 'NONE', #3825, #125, #40573, .T. ) ;
#39753 = CARTESIAN_POINT ( 'NONE',  ( -35.00000000000000000, -10.92721691015459307, 4.309077947445612899 ) ) ;
#39754 = AXIS2_PLACEMENT_3D ( 'NONE', #29600, #44562, #14625 ) ;
#39755 = CARTESIAN_POINT ( 'NONE',  ( 47.00000000000000711, 4.705694406421931860E-17, -3.469127814946512892E-15 ) ) ;
#39756 = ORIENTED_EDGE ( 'NONE', *, *, #59260, .F. ) ;
#39757 = ORIENTED_EDGE ( 'NONE', *, *, #14911, .T. ) ;
#39758 = CYLINDRICAL_SURFACE ( 'NONE', #28555, 2.899999999999994582 ) ;
#39759 = CARTESIAN_POINT ( 'NONE',  ( 0.000000000000000000, 0.7281529553922073683, 7.464569195442786409 ) ) ;
#39760 = VECTOR ( 'NONE', #36434, 1000.000000000000000 ) ;
#39761 = DIRECTION ( 'NONE',  ( -1.000000000000000000, 0.000000000000000000, 0.000000000000000000 ) ) ;
#39762 = CARTESIAN_POINT ( 'NONE',  ( -41.00000000000000711, -1.694065894508600678E-18, 0.000000000000000000 ) ) ;
#39763 = DIRECTION ( 'NONE',  ( -1.000000000000000000, 0.000000000000000000, 0.000000000000000000 ) ) ;
#39764 = ADVANCED_FACE ( 'NONE', ( #37423 ), #57585, .T. ) ;
#39765 = CIRCLE ( 'NONE', #5816, 7.499999999999988454 ) ;
#39766 = CARTESIAN_POINT ( 'NONE',  ( 3.862716043132853105, -11.00608440648994346, -7.819365458621474474 ) ) ;
#39767 = FACE_OUTER_BOUND ( 'NONE', #8398, .T. ) ;
#39768 = CARTESIAN_POINT ( 'NONE',  ( 2.556980015513344640, 6.074557383032630931, 4.795979673457624770 ) ) ;
#39769 = EDGE_CURVE ( 'NONE', #3146, #65336, #47428, .T. ) ;
#39770 = CARTESIAN_POINT ( 'NONE',  ( -37.00000000000000711, 0.000000000000000000, 0.000000000000000000 ) ) ;
#39771 = ORIENTED_EDGE ( 'NONE', *, *, #57163, .T. ) ;
#39772 = DIRECTION ( 'NONE',  ( 0.000000000000000000, 0.000000000000000000, -1.000000000000000000 ) ) ;
#39773 = DIRECTION ( 'NONE',  ( 0.000000000000000000, 0.4198891015602657650, -0.9075754196709565624 ) ) ;
#39774 = CARTESIAN_POINT ( 'NONE',  ( 5.536195898058073439, 0.003145317580921150064, -0.007896796515810348624 ) ) ;
#39775 = B_SPLINE_CURVE_WITH_KNOTS ( 'NONE', 3,
 ( #13935, #49548, #48890, #23617, #43888, #43218, #53214, #54198, #28270, #22632 ),
 .UNSPECIFIED., .F., .F.,
 ( 4, 3, 3, 4 ),
 ( 1.226634733346699542E-18, 6.607638129004514633E-05, 9.911389841680577823E-05, 0.0001667630577588626365 ),
 .UNSPECIFIED. ) ;
#39776 = VECTOR ( 'NONE', #46753, 1000.000000000000000 ) ;
#39777 = ADVANCED_FACE ( 'NONE', ( #42386 ), #19702, .T. ) ;
#39778 = CARTESIAN_POINT ( 'NONE',  ( 2.770579946183333586, -6.607710183380604896, -4.165025702425915632 ) ) ;
#39779 = CARTESIAN_POINT ( 'NONE',  ( -27.45775109278351067, -11.83395752356219255, -1.989333891161980894 ) ) ;
#39780 = ORIENTED_EDGE ( 'NONE', *, *, #63940, .F. ) ;
#39781 = CARTESIAN_POINT ( 'NONE',  ( -37.00000000000000711, 0.000000000000000000, 0.000000000000000000 ) ) ;
#39782 = CARTESIAN_POINT ( 'NONE',  ( 5.515188684475870851, 0.004442604682416481134, 0.002983184900674867857 ) ) ;
#39783 = CARTESIAN_POINT ( 'NONE',  ( -8.110750208426855679, -28.65453171996802695, -10.34333599818553928 ) ) ;
#39784 = ORIENTED_EDGE ( 'NONE', *, *, #65034, .T. ) ;
#39785 = FACE_OUTER_BOUND ( 'NONE', #14408, .T. ) ;
#39786 = CARTESIAN_POINT ( 'NONE',  ( -27.69083675036838343, -10.87160676531835257, -8.024211436650034557 ) ) ;
#39787 = CARTESIAN_POINT ( 'NONE',  ( -22.27756824490284160, -0.9472004376381237822, -3.558840239148768791 ) ) ;
#39788 = ADVANCED_FACE ( 'NONE', ( #53722 ), #63661, .T. ) ;
#39789 = EDGE_CURVE ( 'NONE', #59168, #18816, #43546, .T. ) ;
#39790 = CARTESIAN_POINT ( 'NONE',  ( 19.28625800530496903, 25.00000000000000000, 11.87904264843580471 ) ) ;
#39791 = CARTESIAN_POINT ( 'NONE',  ( -14.11589373245165469, 8.250315036047107142, 8.713914264323175729 ) ) ;
#39792 = CIRCLE ( 'NONE', #46175, 12.75000000000000178 ) ;
#39793 = DIRECTION ( 'NONE',  ( 0.000000000000000000, -0.9999080150203992767, -0.01356324068816951341 ) ) ;
#39794 = ORIENTED_EDGE ( 'NONE', *, *, #7215, .F. ) ;
#39795 = DIRECTION ( 'NONE',  ( 1.000000000000000000, 0.000000000000000000, 0.000000000000000000 ) ) ;
#39796 = CARTESIAN_POINT ( 'NONE',  ( -27.08430418657511396, 1.333569526609277300, 1.863523114787992041 ) ) ;
#39798 = DIRECTION ( 'NONE',  ( -1.000000000000000000, -1.836970198721029688E-16, -0.000000000000000000 ) ) ;
#39797 =( BOUNDED_CURVE ( )  B_SPLINE_CURVE ( 3, ( #57854, #62805, #36569, #11298 ),
 .UNSPECIFIED., .F., .F. ) 
 B_SPLINE_CURVE_WITH_KNOTS ( ( 4, 4 ),
 ( 5.154170548125383888, 5.159499013664793132 ),
 .UNSPECIFIED. ) 
 CURVE ( )  GEOMETRIC_REPRESENTATION_ITEM ( )  RATIONAL_B_SPLINE_CURVE ( ( 1.000000000000000000, 0.9999976339559824012, 0.9999976339559824012, 1.000000000000000000 ) ) 
 REPRESENTATION_ITEM ( '' )  );
#39799 = CARTESIAN_POINT ( 'NONE',  ( 35.00000000000000000, -2.627174906296994905, -11.44858830469739530 ) ) ;
#39800 = CARTESIAN_POINT ( 'NONE',  ( -35.00000000000000000, 0.000000000000000000, 0.000000000000000000 ) ) ;
#39801 = DIRECTION ( 'NONE',  ( -1.000000000000000000, -0.000000000000000000, 0.000000000000000000 ) ) ;
#39802 = DIRECTION ( 'NONE',  ( 1.000000000000000000, 0.000000000000000000, 0.000000000000000000 ) ) ;
#39803 = FACE_OUTER_BOUND ( 'NONE', #23607, .T. ) ;
#39804 = ORIENTED_EDGE ( 'NONE', *, *, #51398, .F. ) ;
#39805 = AXIS2_PLACEMENT_3D ( 'NONE', #29019, #4070, #7756 ) ;
#39806 = ORIENTED_EDGE ( 'NONE', *, *, #32624, .T. ) ;
#39807 = CARTESIAN_POINT ( 'NONE',  ( -18.50195596262152620, -5.100756500577913854, -10.86505773444920564 ) ) ;
#39808 = ORIENTED_EDGE ( 'NONE', *, *, #47537, .F. ) ;
#39809 = SHAPE_REPRESENTATION_RELATIONSHIP ( 'NONE' , 'NONE' ,  #13953, #19082 ) ;
#39810 = DIRECTION ( 'NONE',  ( -1.000000000000000000, -0.000000000000000000, 0.000000000000000000 ) ) ;
#39811 = CARTESIAN_POINT ( 'NONE',  ( -37.00000000000000711, 9.733281772932279807, -8.235637554476541666 ) ) ;
#39812 = ORIENTED_EDGE ( 'NONE', *, *, #46604, .T. ) ;
#39813 = FACE_OUTER_BOUND ( 'NONE', #29758, .T. ) ;
#39814 = CARTESIAN_POINT ( 'NONE',  ( -10.00000000000000178, 0.000000000000000000, 0.000000000000000000 ) ) ;
#39815 = CARTESIAN_POINT ( 'NONE',  ( 23.96381627259500746, -3.708881761758332729, 12.98433744281732061 ) ) ;
#39816 = ORIENTED_EDGE ( 'NONE', *, *, #17117, .F. ) ;
#39817 = VERTEX_POINT ( 'NONE', #38409 ) ;
#39818 = CYLINDRICAL_SURFACE ( 'NONE', #5594, 2.899999999999994582 ) ;
#39819 = EDGE_CURVE ( 'NONE', #22363, #57005, #54408, .T. ) ;
#39820 = ORIENTED_EDGE ( 'NONE', *, *, #23283, .F. ) ;
#39821 = CARTESIAN_POINT ( 'NONE',  ( 6.810356414152409776, -6.143480531804472733, -10.31617154035105521 ) ) ;
#39822 = ORIENTED_EDGE ( 'NONE', *, *, #22076, .F. ) ;
#39823 = CARTESIAN_POINT ( 'NONE',  ( 5.514624014163232779, 0.001255375129358076965, 0.003946330869975007462 ) ) ;
#39824 = CARTESIAN_POINT ( 'NONE',  ( 2.247112776671470247, 7.135103076758483098, -2.720990995225236908 ) ) ;
#39825 = ADVANCED_FACE ( 'NONE', ( #34632 ), #28427, .T. ) ;
#39826 = CARTESIAN_POINT ( 'NONE',  ( 35.00000000000000000, 6.280308599560279426, 9.926225166346956286 ) ) ;
#39827 = DIRECTION ( 'NONE',  ( 0.000000000000000000, 0.01356324068817998940, -0.9999080150203990547 ) ) ;
#39828 = CARTESIAN_POINT ( 'NONE',  ( 36.00000000000000711, -8.624332853795991127, 9.390600770288079602 ) ) ;
#39829 = VERTEX_POINT ( 'NONE', #7485 ) ;
#39830 = CARTESIAN_POINT ( 'NONE',  ( 2.280717697723835258, 7.645922213779907217, -0.1564731737570369263 ) ) ;
#39831 = CARTESIAN_POINT ( 'NONE',  ( 2.665405856346786617, 2.226920474533502059, -9.304623509366180656 ) ) ;
#39832 = CARTESIAN_POINT ( 'NONE',  ( -35.00000000000000000, 11.95840593935201213, 2.346765782874477679 ) ) ;
#39833 = DIRECTION ( 'NONE',  ( 0.000000000000000000, 0.01356324068817992175, -0.9999080150203990547 ) ) ;
#39834 = CARTESIAN_POINT ( 'NONE',  ( 12.89950770217806664, 12.24699127810561627, -5.693691681728255460 ) ) ;
#39835 = CARTESIAN_POINT ( 'NONE',  ( 24.40116933105910846, -0.3707949922271567278, 13.49969628832376856 ) ) ;
#39836 = CARTESIAN_POINT ( 'NONE',  ( 0.000000000000000000, 0.000000000000000000, 0.000000000000000000 ) ) ;
#39837 = DIRECTION ( 'NONE',  ( 1.000000000000000000, -0.000000000000000000, -0.000000000000000000 ) ) ;
#39838 = CARTESIAN_POINT ( 'NONE',  ( -30.18541646480307250, -1.416020129149132334, 25.00000000000000000 ) ) ;
#39839 = CIRCLE ( 'NONE', #30264, 5.000000000000000888 ) ;
#39840 = EDGE_CURVE ( 'NONE', #32947, #13249, #19781, .T. ) ;
#39841 = EDGE_LOOP ( 'NONE', ( #12470, #53964, #57945, #8099 ) ) ;
#39842 = CARTESIAN_POINT ( 'NONE',  ( -18.43828812910839687, 6.163775148567135709, -10.29989178887608503 ) ) ;
#39843 = EDGE_CURVE ( 'NONE', #45163, #38116, #42684, .T. ) ;
#39844 = ORIENTED_EDGE ( 'NONE', *, *, #28296, .F. ) ;
#39845 = CARTESIAN_POINT ( 'NONE',  ( 5.514624014163232779, 0.004137701579365678402, 0.0001700579043834099459 ) ) ;
#39846 = DIRECTION ( 'NONE',  ( 0.000000000000000000, 0.7196168960969767658, 0.6943713148249667233 ) ) ;
#39847 = LINE ( 'NONE', #35165, #51590 ) ;
#39848 = DIRECTION ( 'NONE',  ( 1.000000000000000000, 0.000000000000000000, -0.000000000000000000 ) ) ;
#39849 = EDGE_CURVE ( 'NONE', #33165, #4569, #48036, .T. ) ;
#39850 = CARTESIAN_POINT ( 'NONE',  ( 35.00000000000000000, 10.49591321039688019, 5.273331777780226659 ) ) ;
#39851 = ORIENTED_EDGE ( 'NONE', *, *, #2976, .F. ) ;
#39852 = AXIS2_PLACEMENT_3D ( 'NONE', #26471, #10856, #574 ) ;
#39853 = CARTESIAN_POINT ( 'NONE',  ( 5.516018279890452902, -0.006707902355168857828, -0.0009545156522405044090 ) ) ;
#39854 = CARTESIAN_POINT ( 'NONE',  ( 2.251152103363644130, -3.709836606813365023, 6.676162264140674374 ) ) ;
#39855 = CARTESIAN_POINT ( 'NONE',  ( -27.08954555554373300, 2.082904663687279889, 0.9924303381770370747 ) ) ;
#39856 = DIRECTION ( 'NONE',  ( 1.000000000000000000, -0.000000000000000000, 0.000000000000000000 ) ) ;
#39857 = EDGE_CURVE ( 'NONE', #38941, #38782, #65006, .T. ) ;
#39858 = DIRECTION ( 'NONE',  ( 0.000000000000000000, -0.01356324068817998940, 0.9999080150203990547 ) ) ;
#39859 = AXIS2_PLACEMENT_3D ( 'NONE', #50905, #26285, #36244 ) ;
#39860 = VERTEX_POINT ( 'NONE', #43385 ) ;
#39861 = EDGE_CURVE ( 'NONE', #34161, #56661, #44601, .T. ) ;
#39862 = DIRECTION ( 'NONE',  ( 0.000000000000000000, 0.8989688749565173387, 0.4380125133593943398 ) ) ;
#39863 = ORIENTED_EDGE ( 'NONE', *, *, #17377, .F. ) ;
#39864 = DIRECTION ( 'NONE',  ( 0.000000000000000000, -0.2960891610144577579, -0.9551603052523459647 ) ) ;
#39865 = DIRECTION ( 'NONE',  ( 1.000000000000000000, 0.000000000000000000, 0.000000000000000000 ) ) ;
#39866 = CARTESIAN_POINT ( 'NONE',  ( 2.241352910868909643, -1.243507963608144751, 7.532448145350502777 ) ) ;
#39867 = LINE ( 'NONE', #54531, #2289 ) ;
#39868 = AXIS2_PLACEMENT_3D ( 'NONE', #8024, #29271, #28288 ) ;
#39869 = ORIENTED_EDGE ( 'NONE', *, *, #2595, .F. ) ;
#39870 = ORIENTED_EDGE ( 'NONE', *, *, #3544, .T. ) ;
#39872 = EDGE_CURVE ( 'NONE', #49136, #19519, #24676, .T. ) ;
#39871 = CARTESIAN_POINT ( 'NONE',  ( 2.000000000000001776, 0.000000000000000000, 0.000000000000000000 ) ) ;
#39873 = ORIENTED_EDGE ( 'NONE', *, *, #5267, .T. ) ;
#39874 = CARTESIAN_POINT ( 'NONE',  ( 35.00000000000000000, 6.303578524887091916, 10.42955799785312720 ) ) ;
#39875 = LINE ( 'NONE', #35841, #5630 ) ;
#39876 = DIRECTION ( 'NONE',  ( -0.000000000000000000, -1.000000000000000000, -0.000000000000000000 ) ) ;
#39877 = DIRECTION ( 'NONE',  ( 0.000000000000000000, 0.01356324068817992175, -0.9999080150203990547 ) ) ;
#39878 = CARTESIAN_POINT ( 'NONE',  ( 1.014383007554944705, 9.280879504741051278, -8.367379244277028505 ) ) ;
#39879 = DIRECTION ( 'NONE',  ( 0.000000000000000000, 0.9999080150203989437, 0.01356324068818338426 ) ) ;
#39880 = CARTESIAN_POINT ( 'NONE',  ( 0.4626703367445904047, -12.30872794628575839, -0.2831487465614367371 ) ) ;
#39881 = ORIENTED_EDGE ( 'NONE', *, *, #23571, .T. ) ;
#39883 = EDGE_LOOP ( 'NONE', ( #20877, #52656, #32928, #6797 ) ) ;
#39882 = CARTESIAN_POINT ( 'NONE',  ( -22.28482751661422157, -3.347211412506306605, -1.587261331312506352 ) ) ;
#39884 = VERTEX_POINT ( 'NONE', #11342 ) ;
#39885 = CARTESIAN_POINT ( 'NONE',  ( 36.00000000000000711, -9.076753354953932984, 8.954052073409695112 ) ) ;
#39886 = AXIS2_PLACEMENT_3D ( 'NONE', #57443, #25878, #52470 ) ;
#39887 = LINE ( 'NONE', #34564, #37432 ) ;
#39888 = ORIENTED_EDGE ( 'NONE', *, *, #28396, .F. ) ;
#39889 = DIRECTION ( 'NONE',  ( 0.000000000000000000, -1.000000000000000000, 0.000000000000000000 ) ) ;
#39890 = ORIENTED_EDGE ( 'NONE', *, *, #4853, .T. ) ;
#39891 = CARTESIAN_POINT ( 'NONE',  ( 36.00000000000000711, -12.74921544981110877, 0.1414404973753431438 ) ) ;
#39892 = CARTESIAN_POINT ( 'NONE',  ( 35.00000000000000000, 5.636262487437473823, 10.80478261802175233 ) ) ;
#39893 = CARTESIAN_POINT ( 'NONE',  ( 2.589278595513260672, 7.197074516942324252, -2.875840518181366434 ) ) ;
#39894 = VERTEX_POINT ( 'NONE', #30625 ) ;
#39895 = EDGE_LOOP ( 'NONE', ( #65065, #24114, #28592, #49090 ) ) ;
#39896 = CARTESIAN_POINT ( 'NONE',  ( 2.000000000000001776, -6.664893814313694875, -3.439359016433563898 ) ) ;
#39897 = ORIENTED_EDGE ( 'NONE', *, *, #25177, .T. ) ;
#39898 = DIRECTION ( 'NONE',  ( 0.000000000000000000, 0.9937233664769765662, -0.1118654143051580896 ) ) ;
#39899 = ORIENTED_EDGE ( 'NONE', *, *, #49877, .F. ) ;
#39900 = ORIENTED_EDGE ( 'NONE', *, *, #43176, .F. ) ;
#39901 = ORIENTED_EDGE ( 'NONE', *, *, #47893, .F. ) ;
#39902 = DIRECTION ( 'NONE',  ( 1.000000000000000000, -0.000000000000000000, 0.000000000000000000 ) ) ;
#39903 = LINE ( 'NONE', #29282, #65515 ) ;
#39904 = EDGE_CURVE ( 'NONE', #28963, #62960, #45629, .T. ) ;
#39905 = CARTESIAN_POINT ( 'NONE',  ( -25.42680463514451361, 3.516354806213017437, -1.651747791411759314 ) ) ;
#39906 = DIRECTION ( 'NONE',  ( 1.000000000000000000, 0.000000000000000000, 0.000000000000000000 ) ) ;
#39907 = EDGE_LOOP ( 'NONE', ( #41299, #12150, #58909, #32493 ) ) ;
#39908 = AXIS2_PLACEMENT_3D ( 'NONE', #15369, #56253, #39981 ) ;
#39909 = DIRECTION ( 'NONE',  ( -1.000000000000000000, 0.000000000000000000, 0.000000000000000000 ) ) ;
#39910 = CIRCLE ( 'NONE', #13336, 12.18649999999999878 ) ;
#39911 = ORIENTED_EDGE ( 'NONE', *, *, #8692, .T. ) ;
#39912 = CARTESIAN_POINT ( 'NONE',  ( 35.00000000000000000, 4.705694406421931860E-17, -3.469127814946512892E-15 ) ) ;
#39913 = DIRECTION ( 'NONE',  ( 0.000000000000000000, -0.01356324068817991828, 0.9999080150203990547 ) ) ;
#39914 = VERTEX_POINT ( 'NONE', #55602 ) ;
#39915 = CARTESIAN_POINT ( 'NONE',  ( -27.75615700819353293, 12.49246195788914093, -5.125355884365527359 ) ) ;
#39916 = CARTESIAN_POINT ( 'NONE',  ( 0.2869720083484354478, 3.994435966590065057, 11.58405933820302103 ) ) ;
#39917 = DIRECTION ( 'NONE',  ( 0.000000000000000000, 0.000000000000000000, 1.000000000000000000 ) ) ;
#39918 = CIRCLE ( 'NONE', #45095, 2.999999999999995559 ) ;
#39919 = ORIENTED_EDGE ( 'NONE', *, *, #60397, .F. ) ;
#39920 = EDGE_CURVE ( 'NONE', #51949, #60783, #51924, .T. ) ;
#39921 = ORIENTED_EDGE ( 'NONE', *, *, #12857, .F. ) ;
#39922 = CARTESIAN_POINT ( 'NONE',  ( 2.247112776671470247, -7.635437439951568095, 0.1165461824817482089 ) ) ;
#39923 = ORIENTED_EDGE ( 'NONE', *, *, #9747, .F. ) ;
#39924 = EDGE_CURVE ( 'NONE', #2564, #38245, #15120, .T. ) ;
#39925 = CARTESIAN_POINT ( 'NONE',  ( 0.2647959493198542846, 10.67808515296911054, 5.995292100780825528 ) ) ;
#39926 = CARTESIAN_POINT ( 'NONE',  ( 0.9232167919969169745, 9.809608956680866854, 7.691547553333150766 ) ) ;
#39927 = DIRECTION ( 'NONE',  ( 0.3939253465568944290, 0.7910971609033170537, 0.4679616473074926231 ) ) ;
#39928 = DIRECTION ( 'NONE',  ( -1.000000000000000000, 0.000000000000000000, -0.000000000000000000 ) ) ;
#39929 = EDGE_CURVE ( 'NONE', #46169, #39745, #30134, .T. ) ;
#39930 = CARTESIAN_POINT ( 'NONE',  ( 1.283627346226609012, -9.278077665801919949, 8.503905436511940863 ) ) ;
#39931 = ORIENTED_EDGE ( 'NONE', *, *, #30362, .F. ) ;
#39932 = DIRECTION ( 'NONE',  ( 1.000000000000000000, 0.000000000000000000, 0.000000000000000000 ) ) ;
#39933 = DIRECTION ( 'NONE',  ( 0.9606638835031803270, 0.1133241553124329504, -0.2535400141108139493 ) ) ;
#39934 = DIRECTION ( 'NONE',  ( 0.000000000000000000, 0.000000000000000000, 1.000000000000000000 ) ) ;
#39935 = CARTESIAN_POINT ( 'NONE',  ( 2.000000000000001776, 0.000000000000000000, 0.000000000000000000 ) ) ;
#39936 = DIRECTION ( 'NONE',  ( 0.000000000000000000, 1.000000000000000000, 0.000000000000000000 ) ) ;
#39937 = EDGE_CURVE ( 'NONE', #22527, #26195, #6659, .T. ) ;
#39938 = CARTESIAN_POINT ( 'NONE',  ( 3.100650473569741994, -5.429218121582416678, 5.767490999797090900 ) ) ;
#39939 = EDGE_CURVE ( 'NONE', #27434, #26369, #56580, .T. ) ;
#39940 = CARTESIAN_POINT ( 'NONE',  ( 5.520433897694421610, -0.007082458259338119365, -0.01329351892497969249 ) ) ;
#39941 = DIRECTION ( 'NONE',  ( -1.000000000000000000, -0.000000000000000000, 0.000000000000000000 ) ) ;
#39942 = DIRECTION ( 'NONE',  ( -1.000000000000000000, 0.000000000000000000, 0.000000000000000000 ) ) ;
#39943 = ADVANCED_FACE ( 'NONE', ( #60565 ), #50613, .T. ) ;
#39944 = B_SPLINE_CURVE_WITH_KNOTS ( 'NONE', 3,
 ( #52676, #1140, #37354, #57325, #1488, #16441, #62612, #21764, #42014, #42652, #62295, #52353, #7101, #6792, #22065, #42321, #57666, #18073, #23385, #34001, #23731, #18419 ),
 .UNSPECIFIED., .F., .F.,
 ( 4, 2, 2, 2, 2, 2, 2, 2, 2, 2, 4 ),
 ( 4.249187360970369464E-18, 0.001238599178509041483, 0.002477198357018077328, 0.003715797535527113390, 0.004954396714036149452, 0.005573696303290667266, 0.006192995892545185947, 0.006812295481799704629, 0.007431595071054223310, 0.008670194249563258071, 0.009908793428072295434 ),
 .UNSPECIFIED. ) ;
#39945 = CIRCLE ( 'NONE', #46327, 5.000000000000000888 ) ;
#39946 = EDGE_LOOP ( 'NONE', ( #42921, #6040, #23137, #40030 ) ) ;
#39947 = CARTESIAN_POINT ( 'NONE',  ( 11.81877095885896267, -11.76046328181930889, -2.390220360951764711 ) ) ;
#39948 = EDGE_CURVE ( 'NONE', #34038, #50294, #1342, .T. ) ;
#39949 = CIRCLE ( 'NONE', #42075, 1.500000000000000222 ) ;
#39950 = ORIENTED_EDGE ( 'NONE', *, *, #11402, .T. ) ;
#39951 = CYLINDRICAL_SURFACE ( 'NONE', #35266, 4.999999999999999112 ) ;
#39952 = CARTESIAN_POINT ( 'NONE',  ( -22.27721038036499479, -3.635620891621744288, 0.5802312083658510700 ) ) ;
#39953 = CARTESIAN_POINT ( 'NONE',  ( -21.23983773598477498, -7.447593303288433830, 25.00000000000000000 ) ) ;
#39954 = EDGE_CURVE ( 'NONE', #9287, #45349, #1046, .T. ) ;
#39955 = CARTESIAN_POINT ( 'NONE',  ( 2.255723233589905785, -1.196143347837295146, -7.544965460066120677 ) ) ;
#39956 = ORIENTED_EDGE ( 'NONE', *, *, #60954, .F. ) ;
#39957 = VERTEX_POINT ( 'NONE', #25653 ) ;
#39958 = VERTEX_POINT ( 'NONE', #15350 ) ;
#39959 = CARTESIAN_POINT ( 'NONE',  ( 2.835339799623986856, 2.985412098050598928, -7.241165502254415465 ) ) ;
#39960 = CARTESIAN_POINT ( 'NONE',  ( 2.969415267404766912, 3.597837242549764003, -7.007431655063588671 ) ) ;
#39961 = ORIENTED_EDGE ( 'NONE', *, *, #631, .F. ) ;
#39962 = CARTESIAN_POINT ( 'NONE',  ( 0.000000000000000000, 6.662861565602083758, -1.421313227905602883 ) ) ;
#39963 = CARTESIAN_POINT ( 'NONE',  ( 37.00000000000000711, 0.2661492558803343900, -12.18359334611896827 ) ) ;
#39964 = LINE ( 'NONE', #39303, #14190 ) ;
#39965 = ORIENTED_EDGE ( 'NONE', *, *, #40794, .F. ) ;
#39966 = DIRECTION ( 'NONE',  ( 1.000000000000000000, 0.000000000000000000, 0.000000000000000000 ) ) ;
#39967 = CARTESIAN_POINT ( 'NONE',  ( -0.4406170177989157666, -30.53628804997674706, -15.30998899416534975 ) ) ;
#39968 = DIRECTION ( 'NONE',  ( 0.000000000000000000, 0.01356324068817992175, -0.9999080150203990547 ) ) ;
#39970 = EDGE_LOOP ( 'NONE', ( #55775, #61389, #26565, #30279 ) ) ;
#39969 = LINE ( 'NONE', #19714, #55354 ) ;
#39971 = CARTESIAN_POINT ( 'NONE',  ( -35.00000000000000000, 0.3025107581132838175, -11.74226168163341377 ) ) ;
#39972 = ORIENTED_EDGE ( 'NONE', *, *, #16527, .F. ) ;
#39973 = CARTESIAN_POINT ( 'NONE',  ( 0.3675815128205894289, -9.574637318042015011, 7.689697408877242957 ) ) ;
#39974 = EDGE_LOOP ( 'NONE', ( #62127, #17222, #45961, #32283 ) ) ;
#39975 = CYLINDRICAL_SURFACE ( 'NONE', #41166, 2.899999999999994582 ) ;
#39976 = DIRECTION ( 'NONE',  ( -0.3865475372811021382, 0.8598319252293163961, -0.3335716741247106154 ) ) ;
#39977 = DIRECTION ( 'NONE',  ( 1.000000000000000000, 0.000000000000000000, 0.000000000000000000 ) ) ;
#39978 = LINE ( 'NONE', #5401, #30172 ) ;
#39979 = CARTESIAN_POINT ( 'NONE',  ( -22.27719412087655471, 0.5341638063192103436, 3.642699606241609711 ) ) ;
#39980 = EDGE_CURVE ( 'NONE', #31042, #26347, #42027, .T. ) ;
#39981 = DIRECTION ( 'NONE',  ( 0.000000000000000000, 0.3193015301359742319, 0.9476531711828044546 ) ) ;
#39982 = CARTESIAN_POINT ( 'NONE',  ( 0.2655924914740778187, -4.147079829127179984, -11.52280271232874753 ) ) ;
#39983 = DIRECTION ( 'NONE',  ( 0.000000000000000000, 0.9467777615094583599, 0.3218879778915939571 ) ) ;
#39984 = DIRECTION ( 'NONE',  ( 1.000000000000000000, 0.000000000000000000, -0.000000000000000000 ) ) ;
#39986 = ORIENTED_EDGE ( 'NONE', *, *, #51600, .F. ) ;
#39985 = CARTESIAN_POINT ( 'NONE',  ( -35.00000000000000000, 0.000000000000000000, 0.000000000000000000 ) ) ;
#39987 = B_SPLINE_CURVE_WITH_KNOTS ( 'NONE', 3,
 ( #44015, #39995, #14392, #29053, #5093, #50650, #49982, #40312, #8768, #45315 ),
 .UNSPECIFIED., .F., .F.,
 ( 4, 3, 3, 4 ),
 ( 0.000000000000000000, 6.991367980366405095E-05, 0.0001398269368981362335, 0.0001763147164361759890 ),
 .UNSPECIFIED. ) ;
#39988 = ORIENTED_EDGE ( 'NONE', *, *, #47808, .T. ) ;
#39989 = CARTESIAN_POINT ( 'NONE',  ( 13.39780866403243564, -12.21976414386113241, -5.755504928417656707 ) ) ;
#39990 = VERTEX_POINT ( 'NONE', #46590 ) ;
#39991 =( REPRESENTATION_RELATIONSHIP ('NONE','NONE', #63658, #45039 ) REPRESENTATION_RELATIONSHIP_WITH_TRANSFORMATION ( #2873 )SHAPE_REPRESENTATION_RELATIONSHIP( ) );
#39992 = ORIENTED_EDGE ( 'NONE', *, *, #58012, .F. ) ;
#39993 = EDGE_CURVE ( 'NONE', #42493, #14627, #2429, .T. ) ;
#39994 = CARTESIAN_POINT ( 'NONE',  ( 1.014383007554946925, -12.48801387563329612, 0.4441500209062635429 ) ) ;
#39995 = CARTESIAN_POINT ( 'NONE',  ( -27.08426571771018132, 0.2528330215897400257, 2.277536580310452141 ) ) ;
#39996 = DIRECTION ( 'NONE',  ( 0.000000000000000000, 0.01356324068817992175, -0.9999080150203990547 ) ) ;
#39997 = DIRECTION ( 'NONE',  ( -0.000000000000000000, -1.000000000000000000, -0.000000000000000000 ) ) ;
#39998 = CARTESIAN_POINT ( 'NONE',  ( 2.280717697722507875, 7.238333660706348205, 2.468022724684118874 ) ) ;
#39999 = EDGE_CURVE ( 'NONE', #42172, #33099, #46279, .T. ) ;
#40000 = VECTOR ( 'NONE', #53719, 1000.000000000000227 ) ;
#40001 = DIRECTION ( 'NONE',  ( 0.000000000000000000, 0.01356324068817992175, -0.9999080150203990547 ) ) ;
#40002 =( BOUNDED_SURFACE ( )  B_SPLINE_SURFACE ( 3, 1, ( 
 ( #10835, #50753 ),
 ( #16492, #56052 ),
 ( #26138, #859 ),
 ( #46416, #25810 ) ),
 .UNSPECIFIED., .F., .F., .F. ) 
 B_SPLINE_SURFACE_WITH_KNOTS ( ( 4, 4 ),
 ( 2, 2 ),
 ( 0.000000000000000000, 1.000000000000000000 ),
 ( 0.000000000000000000, 1.000000000000000000 ),
 .UNSPECIFIED. ) 
 GEOMETRIC_REPRESENTATION_ITEM ( )  RATIONAL_B_SPLINE_SURFACE ( (
 ( 1.000000000000000000, 1.000000000000000000),
 ( 0.9942764183789327692, 0.8450855930916580938),
 ( 0.9942764183789327692, 0.8450855930916580938),
 ( 1.000000000000000000, 1.000000000000000000) ) ) 
 REPRESENTATION_ITEM ( '' )  SURFACE ( )  );
#40003 = ORIENTED_EDGE ( 'NONE', *, *, #42539, .T. ) ;
#40004 = CARTESIAN_POINT ( 'NONE',  ( 3.031336079628712099, 0.4165536638489088506, 7.886784934834594196 ) ) ;
#40005 = FACE_OUTER_BOUND ( 'NONE', #25398, .T. ) ;
#40006 = CARTESIAN_POINT ( 'NONE',  ( -27.10719052120871098, 2.116547233941204809, 1.044362304621460069 ) ) ;
#40007 = EDGE_CURVE ( 'NONE', #7090, #15788, #13042, .T. ) ;
#40008 = ORIENTED_EDGE ( 'NONE', *, *, #10255, .F. ) ;
#40009 = DIRECTION ( 'NONE',  ( 1.000000000000000000, 0.000000000000000000, -0.000000000000000000 ) ) ;
#40010 = DIRECTION ( 'NONE',  ( -1.000000000000000000, -0.000000000000000000, 0.000000000000000000 ) ) ;
#40011 = CARTESIAN_POINT ( 'NONE',  ( -46.64267184946612588, -0.6617291737840982346, -12.54075111122643271 ) ) ;
#40012 = EDGE_LOOP ( 'NONE', ( #25757, #48495, #40727, #23314 ) ) ;
#40013 = CARTESIAN_POINT ( 'NONE',  ( 2.305787727787083519, 6.711944854845874886, -3.682701754025442753 ) ) ;
#40014 = CARTESIAN_POINT ( 'NONE',  ( 8.843349564596783452, -31.89871022336353334, 13.45657735392122589 ) ) ;
#40015 = DIRECTION ( 'NONE',  ( 0.000000000000000000, 0.01356324068817998940, -0.9999080150203990547 ) ) ;
#40016 = EDGE_CURVE ( 'NONE', #61800, #39558, #6052, .T. ) ;
#40017 = EDGE_CURVE ( 'NONE', #50103, #48840, #27912, .T. ) ;
#40018 = CARTESIAN_POINT ( 'NONE',  ( -37.00000000000000711, -7.499679039484122178, 9.040300684349668714 ) ) ;
#40019 = CARTESIAN_POINT ( 'NONE',  ( 35.00000000000000000, 7.376655759824880754, -9.700295462048687867 ) ) ;
#40020 = VERTEX_POINT ( 'NONE', #12981 ) ;
#40021 = AXIS2_PLACEMENT_3D ( 'NONE', #12747, #33698, #53001 ) ;
#40022 = CARTESIAN_POINT ( 'NONE',  ( 2.241317068080781016, 0.09149433816015992149, 7.633845645378816158 ) ) ;
#40023 = CARTESIAN_POINT ( 'NONE',  ( 0.3278977287071249136, -12.12129679591847164, 1.885359334311925705 ) ) ;
#40024 = DIRECTION ( 'NONE',  ( 1.000000000000000000, 0.000000000000000000, 0.000000000000000000 ) ) ;
#40025 = EDGE_LOOP ( 'NONE', ( #60922, #30838, #34935, #56814 ) ) ;
#40026 = EDGE_CURVE ( 'NONE', #51803, #22718, #23643, .T. ) ;
#40027 = CARTESIAN_POINT ( 'NONE',  ( 11.12897774696030417, 0.3461397579055390250, 13.49616809366566983 ) ) ;
#40028 = DIRECTION ( 'NONE',  ( 1.000000000000000000, -0.000000000000000000, 0.000000000000000000 ) ) ;
#40029 = ORIENTED_EDGE ( 'NONE', *, *, #19601, .F. ) ;
#40030 = ORIENTED_EDGE ( 'NONE', *, *, #42456, .T. ) ;
#40031 = AXIS2_PLACEMENT_3D ( 'NONE', #42177, #62464, #27896 ) ;
#40032 = VERTEX_POINT ( 'NONE', #16982 ) ;
#40033 = ORIENTED_EDGE ( 'NONE', *, *, #56308, .T. ) ;
#40034 = CARTESIAN_POINT ( 'NONE',  ( -37.00000000000000711, 8.699265615722982403, 8.534258022646129760 ) ) ;
#40035 = CARTESIAN_POINT ( 'NONE',  ( -35.05012975565874456, 0.008684292310206072341, 0.01089417657933153954 ) ) ;
#40036 = DIRECTION ( 'NONE',  ( -1.000000000000000000, 0.000000000000000000, -0.000000000000000000 ) ) ;
#40037 = CARTESIAN_POINT ( 'NONE',  ( -10.95212338237647920, -9.902220863987562183, 9.175839033069923545 ) ) ;
#40038 = CARTESIAN_POINT ( 'NONE',  ( -10.20982488791560883, -26.83227745022078992, 13.82162602233992565 ) ) ;
#40039 = CARTESIAN_POINT ( 'NONE',  ( 23.48125385833485268, 2.900065688388548057, -13.18851851003229925 ) ) ;
#40041 = ORIENTED_EDGE ( 'NONE', *, *, #46576, .F. ) ;
#40040 = CARTESIAN_POINT ( 'NONE',  ( -29.43980975494970309, -3.641506875706030488, 25.00000000000000000 ) ) ;
#40042 = DIRECTION ( 'NONE',  ( 0.000000000000000000, 0.01356324068817998940, -0.9999080150203990547 ) ) ;
#40043 = ORIENTED_EDGE ( 'NONE', *, *, #46912, .T. ) ;
#40044 = DIRECTION ( 'NONE',  ( 1.000000000000000000, 0.000000000000000000, 0.000000000000000000 ) ) ;
#40045 = ORIENTED_EDGE ( 'NONE', *, *, #44915, .F. ) ;
#40046 = VERTEX_POINT ( 'NONE', #32272 ) ;
#40047 = CARTESIAN_POINT ( 'NONE',  ( -22.29570301036918423, -0.8918611685731179239, 3.629130197778196454 ) ) ;
#40048 = CARTESIAN_POINT ( 'NONE',  ( 15.82775651593409627, -34.24354600359715306, 7.361827980272476424 ) ) ;
#40049 = CARTESIAN_POINT ( 'NONE',  ( 1.948354844647129269, 9.612178954895149730, 7.125078658758032368 ) ) ;
#40050 = ADVANCED_FACE ( 'NONE', ( #57235 ), #2713, .T. ) ;
#40051 = DIRECTION ( 'NONE',  ( -1.000000000000000000, 0.000000000000000000, 0.000000000000000000 ) ) ;
#40052 = CARTESIAN_POINT ( 'NONE',  ( -37.00000000000000711, 0.01609748574461371262, -11.74614673114903951 ) ) ;
#40053 = ORIENTED_EDGE ( 'NONE', *, *, #32866, .F. ) ;
#40054 = EDGE_CURVE ( 'NONE', #58956, #22574, #44893, .T. ) ;
#40055 = ORIENTED_EDGE ( 'NONE', *, *, #58339, .F. ) ;
#40056 = CARTESIAN_POINT ( 'NONE',  ( -22.71097035706202405, -4.089776368546547580, -2.846599994298351977 ) ) ;
#40057 = ORIENTED_EDGE ( 'NONE', *, *, #60966, .T. ) ;
#40058 = ORIENTED_EDGE ( 'NONE', *, *, #60686, .F. ) ;
#40059 = ADVANCED_FACE ( 'NONE', ( #21669 ), #11990, .T. ) ;
#40060 = CARTESIAN_POINT ( 'NONE',  ( 35.00000000000000000, 7.718225330433935660, 9.430788938293964918 ) ) ;
#40061 = CARTESIAN_POINT ( 'NONE',  ( 2.241506898688417238, 1.364429914801517318, 7.511570207700565938 ) ) ;
#40062 = CARTESIAN_POINT ( 'NONE',  ( 17.70424766539830941, -7.192594383037563155, 9.609139074359166699 ) ) ;
#40063 = CARTESIAN_POINT ( 'NONE',  ( -22.27719443589224113, 1.139586749255988796, -3.500848524682612872 ) ) ;
#40064 = AXIS2_PLACEMENT_3D ( 'NONE', #43320, #3119, #13396 ) ;
#40065 = CARTESIAN_POINT ( 'NONE',  ( -19.56743653832047158, -33.00000000000000000, 5.000000000000000888 ) ) ;
#40066 = DIRECTION ( 'NONE',  ( -1.000000000000000000, -0.000000000000000000, -0.000000000000000000 ) ) ;
#40067 = ORIENTED_EDGE ( 'NONE', *, *, #5585, .T. ) ;
#40068 = ORIENTED_EDGE ( 'NONE', *, *, #47640, .T. ) ;
#40069 = ADVANCED_FACE ( 'NONE', ( #62205 ), #21975, .T. ) ;
#40070 = DIRECTION ( 'NONE',  ( -1.000000000000000000, -0.000000000000000000, 0.000000000000000000 ) ) ;
#40071 = EDGE_CURVE ( 'NONE', #37494, #35347, #196, .T. ) ;
#40072 = LINE ( 'NONE', #189, #35045 ) ;
#40073 = CIRCLE ( 'NONE', #12493, 5.000000000000000888 ) ;
#40074 = DIRECTION ( 'NONE',  ( -1.000000000000000000, 0.000000000000000000, -0.000000000000000000 ) ) ;
#40075 = ADVANCED_FACE ( 'NONE', ( #1710 ), #58556, .T. ) ;
#40076 = CARTESIAN_POINT ( 'NONE',  ( 5.590291635455702846, -9.340929066271097980, 7.541605757018187361 ) ) ;
#40077 = CARTESIAN_POINT ( 'NONE',  ( -35.00000000000000000, 0.000000000000000000, 0.000000000000000000 ) ) ;
#40078 = AXIS2_PLACEMENT_3D ( 'NONE', #58386, #59696, #54717 ) ;
#40079 = CARTESIAN_POINT ( 'NONE',  ( 5.741342436335442834, -9.898584468105083189, -9.185852332820985566 ) ) ;
#40080 = CARTESIAN_POINT ( 'NONE',  ( -35.00000000000000000, -11.95840593935199792, -2.346765782874564277 ) ) ;
#40081 = CARTESIAN_POINT ( 'NONE',  ( 2.653899356899585893, 6.118160465318848829, 4.792827201941034510 ) ) ;
#40082 = ORIENTED_EDGE ( 'NONE', *, *, #61208, .F. ) ;
#40083 = CARTESIAN_POINT ( 'NONE',  ( 2.507146904658100084, -0.2163149345877113661, 7.719969556433168734 ) ) ;
#40084 = CARTESIAN_POINT ( 'NONE',  ( 35.00000000000000000, -5.644643009979139592, -10.30098186818248074 ) ) ;
#40085 = CARTESIAN_POINT ( 'NONE',  ( 2.827825597296800719, 6.550135365664094600, 6.207590800588408619 ) ) ;
#40086 = EDGE_CURVE ( 'NONE', #18084, #4318, #6996, .T. ) ;
#40087 = EDGE_CURVE ( 'NONE', #23349, #45003, #46989, .T. ) ;
#40088 = CARTESIAN_POINT ( 'NONE',  ( -11.32744364968826112, -33.39367328239853094, -11.05351320890539668 ) ) ;
#40089 = CARTESIAN_POINT ( 'NONE',  ( 35.00000000000000000, 4.705694406421931860E-17, -3.469127814946512892E-15 ) ) ;
#40090 = ORIENTED_EDGE ( 'NONE', *, *, #41500, .F. ) ;
#40091 = CARTESIAN_POINT ( 'NONE',  ( 2.256373768223413734, -2.487510024221220473, 7.223078030710456510 ) ) ;
#40092 = CARTESIAN_POINT ( 'NONE',  ( 0.2646305136544065406, -12.03696649559616105, 2.256625640822277568 ) ) ;
#40093 = CARTESIAN_POINT ( 'NONE',  ( 17.02556425888772296, -28.50707051634331890, -9.313930266526256219 ) ) ;
#40094 = ORIENTED_EDGE ( 'NONE', *, *, #24511, .F. ) ;
#40095 = CARTESIAN_POINT ( 'NONE',  ( 35.00000000000000000, 1.456211999474505969, 11.65554240571055011 ) ) ;
#40096 = DIRECTION ( 'NONE',  ( -1.000000000000000000, 0.000000000000000000, 0.000000000000000000 ) ) ;
#40097 = DIRECTION ( 'NONE',  ( 0.000000000000000000, -0.9346839223284501008, 0.3554799084909072149 ) ) ;
#40099 = ORIENTED_EDGE ( 'NONE', *, *, #22358, .T. ) ;
#40098 = LINE ( 'NONE', #39790, #22222 ) ;
#40100 = CARTESIAN_POINT ( 'NONE',  ( -35.00000000000000000, 8.146229107149400406, 9.063649021438985542 ) ) ;
#40101 = CIRCLE ( 'NONE', #19951, 6.936499999999990784 ) ;
#40102 = FACE_OUTER_BOUND ( 'NONE', #63597, .T. ) ;
#40103 = VERTEX_POINT ( 'NONE', #57569 ) ;
#40104 = CARTESIAN_POINT ( 'NONE',  ( 6.361445718264521432, -4.355102044641763648, 25.00000000000000000 ) ) ;
#40105 = CARTESIAN_POINT ( 'NONE',  ( -27.08456565417846562, 1.328664661356744325, 1.867985369021563535 ) ) ;
#40106 = CIRCLE ( 'NONE', #12484, 12.73084802173761787 ) ;
#40107 = CARTESIAN_POINT ( 'NONE',  ( -14.65039111264524863, 8.403879406532434260, -10.56534429714927370 ) ) ;
#40108 = CARTESIAN_POINT ( 'NONE',  ( 2.000000000000001776, -6.750946897830688798, -1.593658756657146292 ) ) ;
#40109 = CARTESIAN_POINT ( 'NONE',  ( -35.04834644901396956, -0.0002835132723631789337, -0.01383120537649086199 ) ) ;
#40110 = CARTESIAN_POINT ( 'NONE',  ( -30.18541646480307250, -0.9627431840302674848, -11.97002451358074815 ) ) ;
#40111 = CYLINDRICAL_SURFACE ( 'NONE', #50994, 12.18650000000000055 ) ;
#40113 = VERTEX_POINT ( 'NONE', #32581 ) ;
#40112 = AXIS2_PLACEMENT_3D ( 'NONE', #17760, #31713, #56703 ) ;
#40114 = ORIENTED_EDGE ( 'NONE', *, *, #14917, .F. ) ;
#40115 = CARTESIAN_POINT ( 'NONE',  ( 2.268878695253354394, -5.025754889199090414, 5.759001817705848403 ) ) ;
#40116 = VERTEX_POINT ( 'NONE', #52257 ) ;
#40117 = CIRCLE ( 'NONE', #10408, 12.18650000000000233 ) ;
#40118 =( NAMED_UNIT ( * ) PLANE_ANGLE_UNIT ( ) SI_UNIT ( $, .RADIAN. ) );
#40119 = DIRECTION ( 'NONE',  ( 0.000000000000000000, -1.000000000000000000, 0.000000000000000000 ) ) ;
#40120 = CARTESIAN_POINT ( 'NONE',  ( 47.00000000000000711, 4.705694406421931860E-17, -3.469127814946512892E-15 ) ) ;
#40121 = ORIENTED_EDGE ( 'NONE', *, *, #25308, .T. ) ;
#40122 = CARTESIAN_POINT ( 'NONE',  ( 17.27839441901508621, -10.52068335315807524, 5.771933972472480967 ) ) ;
#40123 = EDGE_CURVE ( 'NONE', #23816, #38680, #62522, .T. ) ;
#40124 = LINE ( 'NONE', #54797, #4034 ) ;
#40125 = DIRECTION ( 'NONE',  ( 1.000000000000000000, 0.000000000000000000, 0.000000000000000000 ) ) ;
#40126 = ORIENTED_EDGE ( 'NONE', *, *, #12755, .F. ) ;
#40127 = ORIENTED_EDGE ( 'NONE', *, *, #55847, .T. ) ;
#40128 = DIRECTION ( 'NONE',  ( 1.000000000000000000, 0.000000000000000000, -0.000000000000000000 ) ) ;
#40129 = ORIENTED_EDGE ( 'NONE', *, *, #30941, .T. ) ;
#40130 = CARTESIAN_POINT ( 'NONE',  ( 5.520433897694421610, 0.01329351892497962311, -0.007082458259338250336 ) ) ;
#40131 = VERTEX_POINT ( 'NONE', #47271 ) ;
#40132 = CARTESIAN_POINT ( 'NONE',  ( 0.3675815128205912052, -2.391755495700685241, 12.04510820461658582 ) ) ;
#40133 = DIRECTION ( 'NONE',  ( -1.000000000000000000, 0.000000000000000000, 0.000000000000000000 ) ) ;
#40135 = EDGE_CURVE ( 'NONE', #5900, #61338, #52888, .T. ) ;
#40134 = CARTESIAN_POINT ( 'NONE',  ( 2.931247277082674962, -4.248542803114378152, 6.618030015945717714 ) ) ;
#40136 = CYLINDRICAL_SURFACE ( 'NONE', #19992, 7.499999999999988454 ) ;
#40137 = CARTESIAN_POINT ( 'NONE',  ( 37.00000000000000711, 4.705694406421931860E-17, -3.469127814946512892E-15 ) ) ;
#40138 = ORIENTED_EDGE ( 'NONE', *, *, #41045, .T. ) ;
#40139 = CARTESIAN_POINT ( 'NONE',  ( 1.375507693218858574, -12.04466556545208178, 3.754650692913366505 ) ) ;
#40140 = CARTESIAN_POINT ( 'NONE',  ( -37.00000000000000711, 0.000000000000000000, 0.000000000000000000 ) ) ;
#40141 = ADVANCED_FACE ( 'NONE', ( #47910 ), #20590, .F. ) ;
#40142 = CARTESIAN_POINT ( 'NONE',  ( -27.27855387000350262, 12.26939275170278343, 5.631341004100471892 ) ) ;
#40143 = CARTESIAN_POINT ( 'NONE',  ( 2.241528039335009659, -7.521191296022424311, 1.310213701658565100 ) ) ;
#40144 = CARTESIAN_POINT ( 'NONE',  ( 22.85977700535744006, -4.208561018118428088, 12.82933600296545684 ) ) ;
#40145 = DIRECTION ( 'NONE',  ( -1.000000000000000000, 0.000000000000000000, 0.000000000000000000 ) ) ;
#40146 = DIRECTION ( 'NONE',  ( 0.000000000000000000, 0.4698238015817302604, 0.8827602140260348840 ) ) ;
#40147 = CARTESIAN_POINT ( 'NONE',  ( -4.590058209962335489, 6.612760447609789871, 25.00000000000000000 ) ) ;
#40148 = EDGE_CURVE ( 'NONE', #28450, #43944, #29568, .T. ) ;
#40149 = EDGE_CURVE ( 'NONE', #42450, #10792, #9608, .T. ) ;
#40150 = AXIS2_PLACEMENT_3D ( 'NONE', #14532, #4603, #34811 ) ;
#40151 = VERTEX_POINT ( 'NONE', #3697 ) ;
#40152 = CARTESIAN_POINT ( 'NONE',  ( -15.52346636470029040, 8.464258284448757053, -8.506501996115177988 ) ) ;
#40153 = AXIS2_PLACEMENT_3D ( 'NONE', #12290, #6674, #26945 ) ;
#40154 = CIRCLE ( 'NONE', #3031, 5.000000000000000888 ) ;
#40155 = ORIENTED_EDGE ( 'NONE', *, *, #4180, .F. ) ;
#40156 = LINE ( 'NONE', #45166, #21156 ) ;
#40157 = CARTESIAN_POINT ( 'NONE',  ( 0.2657645697724692058, -0.1513403555226406350, 12.24540328300721903 ) ) ;
#40158 = CARTESIAN_POINT ( 'NONE',  ( -18.08686583997275221, 5.151216734910927464, -12.47858029384662970 ) ) ;
#40159 = CIRCLE ( 'NONE', #59318, 12.18650000000000055 ) ;
#40160 = CARTESIAN_POINT ( 'NONE',  ( 3.152665057734040488, 0.000000000000000000, 0.000000000000000000 ) ) ;
#40161 = CARTESIAN_POINT ( 'NONE',  ( 2.297017764050034661, 2.462009443075729109, -7.246120070222707099 ) ) ;
#40162 = VERTEX_POINT ( 'NONE', #23627 ) ;
#40163 = FACE_OUTER_BOUND ( 'NONE', #34678, .T. ) ;
#40164 = CARTESIAN_POINT ( 'NONE',  ( 2.260457164927185847, -3.699855525213191942, 6.685239696063469239 ) ) ;
#40165 = CARTESIAN_POINT ( 'NONE',  ( 8.937200413559443390, 4.246084004433933856, 11.22641390959094565 ) ) ;
#40166 = VECTOR ( 'NONE', #20202, 1000.000000000000000 ) ;
#40167 = CARTESIAN_POINT ( 'NONE',  ( 2.034671305879537151, 6.436604249851601622, -9.742055912617745506 ) ) ;
#40168 = EDGE_CURVE ( 'NONE', #57837, #52191, #39887, .T. ) ;
#40169 = CARTESIAN_POINT ( 'NONE',  ( -17.57573412780800126, -9.333560918461788702, 7.571049167956692472 ) ) ;
#40170 = LINE ( 'NONE', #60461, #63770 ) ;
#40171 =( BOUNDED_SURFACE ( )  B_SPLINE_SURFACE ( 3, 1, ( 
 ( #1973, #671 ),
 ( #42179, #16933 ),
 ( #20930, #26577 ),
 ( #46870, #10968 ) ),
 .UNSPECIFIED., .F., .F., .F. ) 
 B_SPLINE_SURFACE_WITH_KNOTS ( ( 4, 4 ),
 ( 2, 2 ),
 ( 0.000000000000000000, 1.000000000000000000 ),
 ( 0.000000000000000000, 1.000000000000000000 ),
 .UNSPECIFIED. ) 
 GEOMETRIC_REPRESENTATION_ITEM ( )  RATIONAL_B_SPLINE_SURFACE ( (
 ( 1.000000000000000000, 1.000000000000000000),
 ( 0.6933888150995267674, 0.9895912004443193632),
 ( 0.6933888150995267674, 0.9895912004443193632),
 ( 1.000000000000000000, 1.000000000000000000) ) ) 
 REPRESENTATION_ITEM ( '' )  SURFACE ( )  );
#40172 = ORIENTED_EDGE ( 'NONE', *, *, #14814, .F. ) ;
#40173 = FACE_OUTER_BOUND ( 'NONE', #57940, .T. ) ;
#40174 = VERTEX_POINT ( 'NONE', #43899 ) ;
#40175 = CARTESIAN_POINT ( 'NONE',  ( 0.3223008802179234134, -0.2444878876722378358, -12.26274332232494579 ) ) ;
#40176 = CARTESIAN_POINT ( 'NONE',  ( 2.941278708680199916, 4.615461433467311636, -4.048809123187888659 ) ) ;
#40177 = CARTESIAN_POINT ( 'NONE',  ( 2.889800649504073782, -6.016320774579815733, 1.129261637821590947 ) ) ;
#40178 = DIRECTION ( 'NONE',  ( 1.000000000000000000, -0.000000000000000000, 0.000000000000000000 ) ) ;
#40179 = EDGE_CURVE ( 'NONE', #48583, #65768, #53402, .T. ) ;
#40180 = VECTOR ( 'NONE', #6982, 1000.000000000000000 ) ;
#40181 = VERTEX_POINT ( 'NONE', #53884 ) ;
#40182 = ORIENTED_EDGE ( 'NONE', *, *, #35510, .F. ) ;
#40183 = ORIENTED_EDGE ( 'NONE', *, *, #18904, .F. ) ;
#40184 = CARTESIAN_POINT ( 'NONE',  ( 35.00000000000000000, 10.64792938439763859, 5.927257550915197015 ) ) ;
#40185 = CARTESIAN_POINT ( 'NONE',  ( 0.3040950598368152291, -0.2511348647274793677, -12.25911170648142701 ) ) ;
#40186 = CARTESIAN_POINT ( 'NONE',  ( 8.937200413559443390, 4.476360154859203355, 25.00000000000000000 ) ) ;
#40187 = CARTESIAN_POINT ( 'NONE',  ( 0.2911222467163546712, 12.25291251554515526, 0.2144311696656072685 ) ) ;
#40189 = CARTESIAN_POINT ( 'NONE',  ( 2.430348790457637964, 6.566563360302426489, -4.016278121583773952 ) ) ;
#40188 = CIRCLE ( 'NONE', #26433, 5.000000000000000000 ) ;
#40190 = CARTESIAN_POINT ( 'NONE',  ( 35.00000000000000000, -11.54110654723647400, 2.185196060784003524 ) ) ;
#40191 = CYLINDRICAL_SURFACE ( 'NONE', #54127, 5.000000000000000888 ) ;
#40192 = EDGE_LOOP ( 'NONE', ( #59980, #16440, #19538, #9443 ) ) ;
#40194 = ORIENTED_EDGE ( 'NONE', *, *, #3078, .F. ) ;
#40193 = CARTESIAN_POINT ( 'NONE',  ( 0.3675815128205912052, -10.76447900494944321, 5.910255304480407368 ) ) ;
#40195 = ORIENTED_EDGE ( 'NONE', *, *, #442, .F. ) ;
#40196 = CARTESIAN_POINT ( 'NONE',  ( -22.70624764888619751, 4.591418580540064021, -2.547047087672808630 ) ) ;
#40197 = CIRCLE ( 'NONE', #65674, 4.999999999999999112 ) ;
#40198 = CYLINDRICAL_SURFACE ( 'NONE', #34257, 5.000000000000001776 ) ;
#40199 = VERTEX_POINT ( 'NONE', #18317 ) ;
#40200 = FACE_BOUND ( 'NONE', #22153, .T. ) ;
#40202 = EDGE_LOOP ( 'NONE', ( #62079, #13932, #10239, #11995 ) ) ;
#40201 = AXIS2_PLACEMENT_3D ( 'NONE', #57953, #27337, #12365 ) ;
#40203 = CIRCLE ( 'NONE', #24167, 5.000000000000001776 ) ;
#40204 = DIRECTION ( 'NONE',  ( 0.000000000000000000, 0.01356324068817998940, -0.9999080150203990547 ) ) ;
#40205 = ADVANCED_FACE ( 'NONE', ( #59859 ), #14285, .T. ) ;
#40206 = CARTESIAN_POINT ( 'NONE',  ( 5.536195898058073439, -0.001224473329857533226, -0.008411485181668796121 ) ) ;
#40207 = DIRECTION ( 'NONE',  ( 1.000000000000000000, -0.000000000000000000, -0.000000000000000000 ) ) ;
#40208 = CARTESIAN_POINT ( 'NONE',  ( 3.848792418524904502, -10.99609134338280825, 4.807220403714089763 ) ) ;
#40209 = VERTEX_POINT ( 'NONE', #54861 ) ;
#40210 = ORIENTED_EDGE ( 'NONE', *, *, #53098, .F. ) ;
#40211 = AXIS2_PLACEMENT_3D ( 'NONE', #21936, #61496, #51563 ) ;
#40212 = LINE ( 'NONE', #50869, #49074 ) ;
#40213 = EDGE_CURVE ( 'NONE', #38510, #8110, #28596, .T. ) ;
#40214 = EDGE_LOOP ( 'NONE', ( #39021, #38049, #48723, #48118 ) ) ;
#40215 = LINE ( 'NONE', #29921, #20976 ) ;
#40216 = ORIENTED_EDGE ( 'NONE', *, *, #7397, .T. ) ;
#40217 = EDGE_LOOP ( 'NONE', ( #58652, #62622, #64085, #20414 ) ) ;
#40218 = CIRCLE ( 'NONE', #26454, 12.75000000000000178 ) ;
#40219 = EDGE_LOOP ( 'NONE', ( #41746, #18050, #1573, #17130 ) ) ;
#40220 = CARTESIAN_POINT ( 'NONE',  ( 2.368238019615030776, -5.763545178420138804, 5.070835960312876090 ) ) ;
#40221 = CARTESIAN_POINT ( 'NONE',  ( 1.549075743843499886, 11.66216484053741276, 4.962709020479369570 ) ) ;
#40222 = CARTESIAN_POINT ( 'NONE',  ( 0.000000000000000000, -5.457833520448679643, 4.281014542496493824 ) ) ;
#40224 = EDGE_CURVE ( 'NONE', #60956, #52121, #14080, .T. ) ;
#40223 = LINE ( 'NONE', #34582, #24508 ) ;
#40225 = CARTESIAN_POINT ( 'NONE',  ( -35.04660725145885891, -0.003039313842339400138, -0.01191704700716593457 ) ) ;
#40226 = ORIENTED_EDGE ( 'NONE', *, *, #24942, .T. ) ;
#40227 = CARTESIAN_POINT ( 'NONE',  ( 35.00000000000000000, 4.426194442447407340, 11.35427606708800852 ) ) ;
#40228 = VERTEX_POINT ( 'NONE', #55179 ) ;
#40229 = DIRECTION ( 'NONE',  ( 1.000000000000000000, -0.000000000000000000, 0.000000000000000000 ) ) ;
#40230 = CARTESIAN_POINT ( 'NONE',  ( -18.21154635310088565, -5.491257917030544888, -12.33504523915716966 ) ) ;
#40231 = EDGE_CURVE ( 'NONE', #27273, #47988, #57632, .T. ) ;
#40232 = ORIENTED_EDGE ( 'NONE', *, *, #31540, .F. ) ;
#40233 = CARTESIAN_POINT ( 'NONE',  ( 0.3278977287071211943, -10.74546228373870704, 5.917385921415761807 ) ) ;
#40234 = CARTESIAN_POINT ( 'NONE',  ( 26.08439714455133185, 11.40113243194252846, 3.743551691817327942 ) ) ;
#40235 = CARTESIAN_POINT ( 'NONE',  ( -22.27706485742869091, 0.3729136217356220917, 3.662257305743802149 ) ) ;
#40236 = AXIS2_PLACEMENT_3D ( 'NONE', #25530, #40493, #34829 ) ;
#40237 = EDGE_LOOP ( 'NONE', ( #61543, #58069, #5839, #4881 ) ) ;
#40238 = CARTESIAN_POINT ( 'NONE',  ( 2.241352910868908310, 7.633946224498473931, -0.08337961031706911386 ) ) ;
#40239 = EDGE_CURVE ( 'NONE', #9384, #36860, #65153, .T. ) ;
#40240 = AXIS2_PLACEMENT_3D ( 'NONE', #25773, #20119, #61656 ) ;
#40241 = VERTEX_POINT ( 'NONE', #18656 ) ;
#40242 = CARTESIAN_POINT ( 'NONE',  ( -25.54417658651491863, -7.498517398407823720, 11.22596262356930197 ) ) ;
#40243 = SURFACE_STYLE_USAGE ( .BOTH. , #19975 ) ;
#40244 = CARTESIAN_POINT ( 'NONE',  ( 2.305787727787083519, 6.711944854845874886, -3.682701754025442753 ) ) ;
#40245 = DIRECTION ( 'NONE',  ( 1.000000000000000000, 0.000000000000000000, -0.000000000000000000 ) ) ;
#40246 = CARTESIAN_POINT ( 'NONE',  ( 12.19101310789403136, 11.82374128125938739, -2.055631940355953091 ) ) ;
#40247 = ORIENTED_EDGE ( 'NONE', *, *, #21650, .T. ) ;
#40248 = DIRECTION ( 'NONE',  ( 1.000000000000000000, 0.000000000000000000, 0.000000000000000000 ) ) ;
#40249 = DIRECTION ( 'NONE',  ( -1.000000000000000000, 0.000000000000000000, 0.000000000000000000 ) ) ;
#40250 = LINE ( 'NONE', #10012, #36411 ) ;
#40251 = DIRECTION ( 'NONE',  ( 0.000000000000000000, 0.9937233664769756780, -0.1118654143051653060 ) ) ;
#40252 = VECTOR ( 'NONE', #6473, 1000.000000000000000 ) ;
#40253 = AXIS2_PLACEMENT_3D ( 'NONE', #11483, #5548, #25152 ) ;
#40254 = VECTOR ( 'NONE', #16881, 1000.000000000000000 ) ;
#40255 = CARTESIAN_POINT ( 'NONE',  ( -9.857630741398546448, -27.64257788600498600, -14.42778837489968424 ) ) ;
#40256 = DIRECTION ( 'NONE',  ( 1.000000000000000000, -0.000000000000000000, -0.000000000000000000 ) ) ;
#40257 = CARTESIAN_POINT ( 'NONE',  ( 2.256373768223411957, -5.936694589811224887, -4.807932997207762682 ) ) ;
#40258 = CARTESIAN_POINT ( 'NONE',  ( -7.181456785175555524, -5.890186129966251904, -10.45493698471458188 ) ) ;
#40259 = CARTESIAN_POINT ( 'NONE',  ( 2.000000000000001776, 0.8935325819928834346, 7.446583077151348817 ) ) ;
#40260 = EDGE_CURVE ( 'NONE', #22630, #30460, #48090, .T. ) ;
#40261 = ORIENTED_EDGE ( 'NONE', *, *, #40778, .T. ) ;
#40262 = CARTESIAN_POINT ( 'NONE',  ( -27.09602251845210930, -1.302811993375582844, -1.927725285107534603 ) ) ;
#40263 = ORIENTED_EDGE ( 'NONE', *, *, #28309, .T. ) ;
#40264 = DIRECTION ( 'NONE',  ( 0.000000000000000000, -0.01356324068817998940, 0.9999080150203990547 ) ) ;
#40265 = CARTESIAN_POINT ( 'NONE',  ( -22.28506771379528573, 3.091577134491935830, -2.081613609299053369 ) ) ;
#40266 = FACE_OUTER_BOUND ( 'NONE', #39202, .T. ) ;
#40267 = CARTESIAN_POINT ( 'NONE',  ( 2.241311220309654129, -1.234192392742715860, -7.533971938435956694 ) ) ;
#40268 = EDGE_LOOP ( 'NONE', ( #21768, #877, #62857, #61601 ) ) ;
#40269 = VERTEX_POINT ( 'NONE', #38914 ) ;
#40270 = ORIENTED_EDGE ( 'NONE', *, *, #10709, .F. ) ;
#40271 = LINE ( 'NONE', #55600, #46119 ) ;
#40272 = CARTESIAN_POINT ( 'NONE',  ( -22.27721698446158172, 0.6951119527728008007, 3.615509722105048951 ) ) ;
#40273 = ADVANCED_FACE ( 'NONE', ( #8322 ), #48902, .T. ) ;
#40274 = EDGE_LOOP ( 'NONE', ( #11786, #15751, #60845, #49259 ) ) ;
#40275 = CYLINDRICAL_SURFACE ( 'NONE', #6925, 4.000000000000000000 ) ;
#40276 = B_SPLINE_CURVE_WITH_KNOTS ( 'NONE', 3,
 ( #27151, #11517, #36472, #37110, #17170, #11204, #41781, #62077, #10525, #30801, #31787, #52096, #26821, #1574, #21848, #42093 ),
 .UNSPECIFIED., .F., .F.,
 ( 4, 3, 3, 3, 3, 4 ),
 ( 2.178818782297515178E-15, 0.0002126834539179851184, 0.0004253519300366563854, 0.0006380165497224616006, 0.0007442707582428764734, 0.0009453531351414631379 ),
 .UNSPECIFIED. ) ;
#40277 = LINE ( 'NONE', #54637, #4986 ) ;
#40278 = DIRECTION ( 'NONE',  ( 0.000000000000000000, -0.01356324068817998940, 0.9999080150203990547 ) ) ;
#40279 = VERTEX_POINT ( 'NONE', #8653 ) ;
#40280 = FACE_OUTER_BOUND ( 'NONE', #8254, .T. ) ;
#40281 = AXIS2_PLACEMENT_3D ( 'NONE', #61576, #4442, #4782 ) ;
#40282 = EDGE_CURVE ( 'NONE', #58319, #3877, #51270, .T. ) ;
#40283 = CARTESIAN_POINT ( 'NONE',  ( 3.616736114193129126, -30.77385512440640980, -15.02426791487768831 ) ) ;
#40284 = DIRECTION ( 'NONE',  ( -1.000000000000000000, -1.836970198721029688E-16, 0.000000000000000000 ) ) ;
#40286 = ORIENTED_EDGE ( 'NONE', *, *, #36821, .F. ) ;
#40285 = CARTESIAN_POINT ( 'NONE',  ( -27.08850691366518504, 1.648570643966304594, 1.609738257842355580 ) ) ;
#40287 = DIRECTION ( 'NONE',  ( 1.000000000000000000, 0.000000000000000000, 0.000000000000000000 ) ) ;
#40288 = ADVANCED_FACE ( 'NONE', ( #59518 ), #34869, .T. ) ;
#40289 = ORIENTED_EDGE ( 'NONE', *, *, #41972, .F. ) ;
#40290 = DIRECTION ( 'NONE',  ( -1.000000000000000000, 0.000000000000000000, 0.000000000000000000 ) ) ;
#40291 = ORIENTED_EDGE ( 'NONE', *, *, #525, .F. ) ;
#40292 = CARTESIAN_POINT ( 'NONE',  ( -27.01437459610461644, -8.723448335974111956, -8.240233560378637634 ) ) ;
#40293 = CARTESIAN_POINT ( 'NONE',  ( 12.93934141822999528, -9.509120055689606943, -7.322759090511362423 ) ) ;
#40294 = AXIS2_PLACEMENT_3D ( 'NONE', #10340, #49621, #14352 ) ;
#40295 = DIRECTION ( 'NONE',  ( -1.000000000000000000, 0.000000000000000000, 0.000000000000000000 ) ) ;
#40296 = CARTESIAN_POINT ( 'NONE',  ( 1.459561108993791434, -6.861308540877895545, -10.62073135189161199 ) ) ;
#40297 = CARTESIAN_POINT ( 'NONE',  ( -27.20650584082916978, 3.154168801321778126, 0.2670256460080390748 ) ) ;
#40298 = CARTESIAN_POINT ( 'NONE',  ( 0.3341166715381305719, -12.26652061402056049, 0.2526177176099637656 ) ) ;
#40300 = EDGE_CURVE ( 'NONE', #44356, #58956, #53936, .T. ) ;
#40299 = CARTESIAN_POINT ( 'NONE',  ( 12.47628546223243617, 0.000000000000000000, 11.99999999999999645 ) ) ;
#40301 = CARTESIAN_POINT ( 'NONE',  ( -27.08416781016246588, 2.253489850813972240, -0.4141677382007631913 ) ) ;
#40302 = DIRECTION ( 'NONE',  ( -1.000000000000000000, 0.000000000000000000, 0.000000000000000000 ) ) ;
#40304 = VERTEX_POINT ( 'NONE', #4984 ) ;
#40303 = CARTESIAN_POINT ( 'NONE',  ( 4.225017978203527313, -10.87119238259119314, 8.008815562465079196 ) ) ;
#40305 = CARTESIAN_POINT ( 'NONE',  ( -35.05012975565874456, -0.002839961651356822867, -0.01363945138521795858 ) ) ;
#40306 = ORIENTED_EDGE ( 'NONE', *, *, #4712, .T. ) ;
#40307 = CARTESIAN_POINT ( 'NONE',  ( 9.687175622948608122, -13.48729812737142986, -0.5854820436212360146 ) ) ;
#40308 = ORIENTED_EDGE ( 'NONE', *, *, #8534, .T. ) ;
#40309 = ADVANCED_FACE ( 'NONE', ( #35212 ), #40198, .T. ) ;
#40310 = EDGE_LOOP ( 'NONE', ( #22741, #9946, #10249, #17049 ) ) ;
#40311 = CARTESIAN_POINT ( 'NONE',  ( 0.2915757698887279648, 8.040595355212950324, 9.248369946372557493 ) ) ;
#40312 = CARTESIAN_POINT ( 'NONE',  ( -27.08417174366084623, 0.3802265912085586175, 2.259388872100069889 ) ) ;
#40313 = AXIS2_PLACEMENT_3D ( 'NONE', #27223, #3280, #2956 ) ;
#40314 = CARTESIAN_POINT ( 'NONE',  ( -27.08776759928964850, -2.217308861843129364, 0.6183458186125468936 ) ) ;
#40315 = EDGE_CURVE ( 'NONE', #58425, #28230, #23796, .T. ) ;
#40316 = CARTESIAN_POINT ( 'NONE',  ( 35.00000000000000000, 4.705694406421931860E-17, -3.469127814946512892E-15 ) ) ;
#40317 = CARTESIAN_POINT ( 'NONE',  ( 0.2646305136544072623, 10.67138229758237777, -6.008537389229307024 ) ) ;
#40318 = DIRECTION ( 'NONE',  ( 0.000000000000000000, -0.01356324068817999114, 0.9999080150203989437 ) ) ;
#40319 = EDGE_CURVE ( 'NONE', #14103, #28435, #62623, .T. ) ;
#40320 = ORIENTED_EDGE ( 'NONE', *, *, #13930, .T. ) ;
#40321 = CARTESIAN_POINT ( 'NONE',  ( 2.899286259009673739, -6.239228647238591385, 4.769992516330216148 ) ) ;
#40322 = ADVANCED_FACE ( 'NONE', ( #968, #60831 ), #16260, .F. ) ;
#40323 = LINE ( 'NONE', #4793, #56869 ) ;
#40324 = CARTESIAN_POINT ( 'NONE',  ( 1.549075743843931097, 12.34675572956519218, 2.862200647101266870 ) ) ;
#40325 = ORIENTED_EDGE ( 'NONE', *, *, #40392, .F. ) ;
#40326 = CIRCLE ( 'NONE', #47797, 12.75000000000000178 ) ;
#40327 = AXIS2_PLACEMENT_3D ( 'NONE', #11946, #47863, #28237 ) ;
#40328 = CARTESIAN_POINT ( 'NONE',  ( 31.50196089333760696, -3.063567359192289619, 24.19471064305899688 ) ) ;
#40329 = DIRECTION ( 'NONE',  ( 1.000000000000000000, 0.000000000000000000, 0.000000000000000000 ) ) ;
#40330 = ORIENTED_EDGE ( 'NONE', *, *, #32319, .T. ) ;
#40331 = LINE ( 'NONE', #15405, #6478 ) ;
#40332 = CARTESIAN_POINT ( 'NONE',  ( 9.648902782409225054, -32.13880772996252233, 13.06387094875849897 ) ) ;
#40333 = CYLINDRICAL_SURFACE ( 'NONE', #7791, 12.18649999999999878 ) ;
#40334 = AXIS2_PLACEMENT_3D ( 'NONE', #28510, #48818, #6940 ) ;
#40335 = EDGE_CURVE ( 'NONE', #32047, #54583, #62920, .T. ) ;
#40336 = EDGE_CURVE ( 'NONE', #54640, #44205, #10907, .T. ) ;
#40337 = CARTESIAN_POINT ( 'NONE',  ( -27.08429572838383947, -1.859677275556421927, 1.338867938658193424 ) ) ;
#40338 = CARTESIAN_POINT ( 'NONE',  ( -37.00000000000000711, 0.000000000000000000, 0.000000000000000000 ) ) ;
#40339 = CIRCLE ( 'NONE', #48875, 5.000000000000000000 ) ;
#40340 = ORIENTED_EDGE ( 'NONE', *, *, #28308, .F. ) ;
#40341 = CARTESIAN_POINT ( 'NONE',  ( 2.273267844204866162, 0.1513603614830498212, 7.643541951623946673 ) ) ;
#40342 = CARTESIAN_POINT ( 'NONE',  ( -22.27718150314433387, 3.507884203786638011, 1.117371044661051638 ) ) ;
#40343 = DIRECTION ( 'NONE',  ( -1.000000000000000000, 0.000000000000000000, 0.000000000000000000 ) ) ;
#40344 = ORIENTED_EDGE ( 'NONE', *, *, #708, .T. ) ;
#40345 = CARTESIAN_POINT ( 'NONE',  ( -37.00000000000000711, 2.968224442958403486, 11.81949347079748058 ) ) ;
#40346 = FACE_OUTER_BOUND ( 'NONE', #10002, .T. ) ;
#40347 = ORIENTED_EDGE ( 'NONE', *, *, #43612, .T. ) ;
#40348 = ADVANCED_FACE ( 'NONE', ( #324 ), #20602, .T. ) ;
#40349 = AXIS2_PLACEMENT_3D ( 'NONE', #24941, #50546, #54557 ) ;
#40350 = VERTEX_POINT ( 'NONE', #4671 ) ;
#40351 = VERTEX_POINT ( 'NONE', #61157 ) ;
#40352 = ADVANCED_FACE ( 'NONE', ( #10942 ), #15588, .T. ) ;
#40353 = VERTEX_POINT ( 'NONE', #25920 ) ;
#40354 = CARTESIAN_POINT ( 'NONE',  ( 37.00000000000000711, 4.705694406421931860E-17, -3.469127814946512892E-15 ) ) ;
#40355 = CARTESIAN_POINT ( 'NONE',  ( 0.2653519890518156177, 6.123091032184292182, -10.60552241699060794 ) ) ;
#40356 = CARTESIAN_POINT ( 'NONE',  ( 35.00000000000000000, 5.672855678558685888, -10.28547182238010116 ) ) ;
#40357 = CARTESIAN_POINT ( 'NONE',  ( 0.2651627923886321070, 4.271101819784510312, -11.47719387551881987 ) ) ;
#40358 = CARTESIAN_POINT ( 'NONE',  ( -16.21117406328131594, -35.00000000000000000, 4.142385751841761277 ) ) ;
#40359 = CARTESIAN_POINT ( 'NONE',  ( -18.04208054618453616, 11.95114819866064693, 1.265206980359397271 ) ) ;
#40361 = EDGE_LOOP ( 'NONE', ( #61364, #19459, #57030, #55629 ) ) ;
#40360 = CARTESIAN_POINT ( 'NONE',  ( 0.2650492594609249464, -12.04046128294316631, -2.234872523101302466 ) ) ;
#40362 = DIRECTION ( 'NONE',  ( 0.6147887355352468219, -0.7886918350401329603, 0.000000000000000000 ) ) ;
#40363 = EDGE_CURVE ( 'NONE', #10842, #43145, #17434, .T. ) ;
#40364 = EDGE_LOOP ( 'NONE', ( #26100, #32195, #56989, #29068 ) ) ;
#40365 = CARTESIAN_POINT ( 'NONE',  ( 35.00000000000000000, 4.705694406421931860E-17, -3.469127814946512892E-15 ) ) ;
#40366 = ORIENTED_EDGE ( 'NONE', *, *, #19104, .F. ) ;
#40367 = ORIENTED_EDGE ( 'NONE', *, *, #40388, .T. ) ;
#40368 = CARTESIAN_POINT ( 'NONE',  ( 35.00000000000000000, -1.591260454995155671, 12.08216339958901742 ) ) ;
#40369 = CARTESIAN_POINT ( 'NONE',  ( 9.992127424269058977, -32.24574823824644909, 12.88148438038762400 ) ) ;
#40370 = DIRECTION ( 'NONE',  ( -1.000000000000000000, 0.000000000000000000, -0.000000000000000000 ) ) ;
#40371 = VECTOR ( 'NONE', #2606, 1000.000000000000114 ) ;
#40373 = VECTOR ( 'NONE', #24092, 1000.000000000000000 ) ;
#40372 = CARTESIAN_POINT ( 'NONE',  ( 2.507146904658100972, 7.640248566386913076, -1.127530020444418746 ) ) ;
#40374 = CARTESIAN_POINT ( 'NONE',  ( 0.9296196016823207176, -2.573053270830310435, 12.19921892949957964 ) ) ;
#40375 = CARTESIAN_POINT ( 'NONE',  ( 2.305787727787083519, 5.970480882365222897, 4.792270232040915623 ) ) ;
#40376 = ORIENTED_EDGE ( 'NONE', *, *, #29067, .F. ) ;
#40377 =( BOUNDED_CURVE ( )  B_SPLINE_CURVE ( 3, ( #26489, #12181, #42414, #62709 ),
 .UNSPECIFIED., .F., .F. ) 
 B_SPLINE_CURVE_WITH_KNOTS ( ( 4, 4 ),
 ( 4.670929601778163409, 4.712388980384690562 ),
 .UNSPECIFIED. ) 
 CURVE ( )  GEOMETRIC_REPRESENTATION_ITEM ( )  RATIONAL_B_SPLINE_CURVE ( ( 1.000000000000000000, 0.9998567651231480280, 0.9998567651231480280, 1.000000000000000000 ) ) 
 REPRESENTATION_ITEM ( '' )  );
#40378 = ORIENTED_EDGE ( 'NONE', *, *, #13054, .T. ) ;
#40379 = CARTESIAN_POINT ( 'NONE',  ( -35.00000000000000000, 3.827046518385245122, -11.56998259273173701 ) ) ;
#40380 = ORIENTED_EDGE ( 'NONE', *, *, #39112, .T. ) ;
#40381 = EDGE_CURVE ( 'NONE', #55675, #9403, #50274, .T. ) ;
#40382 = EDGE_CURVE ( 'NONE', #12941, #49613, #40666, .T. ) ;
#40383 = VERTEX_POINT ( 'NONE', #21911 ) ;
#40384 = DIRECTION ( 'NONE',  ( 1.000000000000000000, 0.000000000000000000, 0.000000000000000000 ) ) ;
#40385 = CARTESIAN_POINT ( 'NONE',  ( 0.3675815128205894289, 10.50067073900660652, -6.367184624550055183 ) ) ;
#40386 = CARTESIAN_POINT ( 'NONE',  ( 2.241509619876138171, 1.287997509666571005, 7.525055189891909357 ) ) ;
#40387 = DIRECTION ( 'NONE',  ( -1.000000000000000000, 0.000000000000000000, 0.000000000000000000 ) ) ;
#40388 = EDGE_CURVE ( 'NONE', #64491, #38510, #56275, .T. ) ;
#40390 = VECTOR ( 'NONE', #23121, 1000.000000000000000 ) ;
#40389 = CARTESIAN_POINT ( 'NONE',  ( 2.000000000000001776, 0.000000000000000000, 0.000000000000000000 ) ) ;
#40391 = CARTESIAN_POINT ( 'NONE',  ( 2.000000000000001776, -6.935703035393425253, 0.1051458740707039013 ) ) ;
#40392 = EDGE_CURVE ( 'NONE', #55347, #55842, #21589, .T. ) ;
#40393 = CARTESIAN_POINT ( 'NONE',  ( 27.72497957433742855, -12.75711206765212324, 4.419907683352735539 ) ) ;
#40394 = AXIS2_PLACEMENT_3D ( 'NONE', #6898, #36134, #41803 ) ;
#40395 = ORIENTED_EDGE ( 'NONE', *, *, #7551, .F. ) ;
#40396 = ORIENTED_EDGE ( 'NONE', *, *, #16723, .T. ) ;
#40397 = ADVANCED_FACE ( 'NONE', ( #11590 ), #49535, .F. ) ;
#40398 = DIRECTION ( 'NONE',  ( 0.000000000000000000, -0.01356324068817998940, 0.9999080150203990547 ) ) ;
#40399 = CARTESIAN_POINT ( 'NONE',  ( 2.260457164927184071, 7.499412009325160611, -1.462935478981523207 ) ) ;
#40400 = VECTOR ( 'NONE', #61725, 1000.000000000000000 ) ;
#40401 = DIRECTION ( 'NONE',  ( 0.000000000000000000, -0.01356324068817992175, 0.9999080150203990547 ) ) ;
#40402 = CARTESIAN_POINT ( 'NONE',  ( 6.716177905018834160, -7.149925761153411941, 9.639490146783378677 ) ) ;
#40403 = FACE_OUTER_BOUND ( 'NONE', #39060, .T. ) ;
#40404 = AXIS2_PLACEMENT_3D ( 'NONE', #16520, #31475, #58313 ) ;
#40405 = FACE_OUTER_BOUND ( 'NONE', #2895, .T. ) ;
#40406 = CARTESIAN_POINT ( 'NONE',  ( 2.241352910868910531, 5.901537464758519036, -4.843133558968066410 ) ) ;
#40407 = CARTESIAN_POINT ( 'NONE',  ( -27.08417568107323703, -2.142502990753192282, -0.8117865859100446002 ) ) ;
#40408 = AXIS2_PLACEMENT_3D ( 'NONE', #59351, #63660, #18136 ) ;
#40409 = EDGE_LOOP ( 'NONE', ( #8975, #55803 ) ) ;
#40410 = CARTESIAN_POINT ( 'NONE',  ( 2.573738926104376823, -0.2352053552897994393, 7.741646296020606499 ) ) ;
#40411 = CARTESIAN_POINT ( 'NONE',  ( -14.11589373245165469, 8.250315036047107142, 8.713914264323175729 ) ) ;
#40412 = DIRECTION ( 'NONE',  ( 0.000000000000000000, -1.000000000000000000, 0.000000000000000000 ) ) ;
#40413 = AXIS2_PLACEMENT_3D ( 'NONE', #30046, #60307, #5120 ) ;
#40414 = ADVANCED_FACE ( 'NONE', ( #37180 ), #42482, .T. ) ;
#40415 = CIRCLE ( 'NONE', #25576, 5.000000000000000888 ) ;
#40416 = CARTESIAN_POINT ( 'NONE',  ( 37.00000000000000711, 4.705694406421931860E-17, -3.469127814946512892E-15 ) ) ;
#40417 = ADVANCED_FACE ( 'NONE', ( #32836 ), #62781, .T. ) ;
#40418 = CARTESIAN_POINT ( 'NONE',  ( 2.305787727787083519, -7.135468203930003028, 2.774453000917123990 ) ) ;
#40419 = EDGE_LOOP ( 'NONE', ( #38485, #53645, #14026, #46720 ) ) ;
#40420 = AXIS2_PLACEMENT_3D ( 'NONE', #34430, #43410, #3870 ) ;
#40421 = CARTESIAN_POINT ( 'NONE',  ( -27.10719052120871098, -2.116547233941210138, -1.044362304621491377 ) ) ;
#40422 = CARTESIAN_POINT ( 'NONE',  ( 5.515539859299206427, 0.004509673239148338786, 0.004037661319610840079 ) ) ;
#40423 = CARTESIAN_POINT ( 'NONE',  ( 9.461050110694847248, -32.74574823825055603, -12.19700847635464669 ) ) ;
#40424 = ORIENTED_EDGE ( 'NONE', *, *, #8120, .F. ) ;
#40425 = DIRECTION ( 'NONE',  ( -1.000000000000000000, 0.000000000000000000, 0.000000000000000000 ) ) ;
#40426 = CARTESIAN_POINT ( 'NONE',  ( -22.65996813707687352, 4.828298130757343820, 0.2230532344361134678 ) ) ;
#40427 = CARTESIAN_POINT ( 'NONE',  ( -22.29018399051993882, -1.024613686459451944, -3.576688584977248730 ) ) ;
#40428 = ADVANCED_FACE ( 'NONE', ( #48185 ), #32510, .F. ) ;
#40430 = ORIENTED_EDGE ( 'NONE', *, *, #11214, .T. ) ;
#40429 = DIRECTION ( 'NONE',  ( 0.000000000000000000, 0.5155538571770172940, 0.8568571761675919385 ) ) ;
#40431 = CARTESIAN_POINT ( 'NONE',  ( -27.10512513516274424, 2.289566223068224993, 0.5469390009825837451 ) ) ;
#40432 = VECTOR ( 'NONE', #37525, 1000.000000000000000 ) ;
#40433 = CIRCLE ( 'NONE', #52141, 12.74999999999999822 ) ;
#40434 = FACE_OUTER_BOUND ( 'NONE', #45271, .T. ) ;
#40435 = ORIENTED_EDGE ( 'NONE', *, *, #11464, .F. ) ;
#40436 = AXIS2_PLACEMENT_3D ( 'NONE', #41062, #52628, #7368 ) ;
#40437 = CARTESIAN_POINT ( 'NONE',  ( 0.09505933169494876211, -0.1369491540312630928, -11.99999999999999112 ) ) ;
#40438 = VECTOR ( 'NONE', #4424, 1000.000000000000000 ) ;
#40439 = DIRECTION ( 'NONE',  ( 0.000000000000000000, 0.01356324068817991828, -0.9999080150203990547 ) ) ;
#40440 = CARTESIAN_POINT ( 'NONE',  ( -17.98378524109403287, 7.072918058914841488, -11.50120456127047142 ) ) ;
#40441 = LINE ( 'NONE', #14825, #63762 ) ;
#40442 = CARTESIAN_POINT ( 'NONE',  ( 0.3053067050349180800, -11.43920902168903631, -4.409108891833770194 ) ) ;
#40443 = CIRCLE ( 'NONE', #34082, 12.18649999999999700 ) ;
#40444 = CARTESIAN_POINT ( 'NONE',  ( 2.241509619876138171, 2.647089031563667483, -7.160887714159589912 ) ) ;
#40445 = DIRECTION ( 'NONE',  ( 0.000000000000000000, 0.000000000000000000, -1.000000000000000000 ) ) ;
#40446 = EDGE_CURVE ( 'NONE', #41793, #13375, #43152, .T. ) ;
#40447 = VERTEX_POINT ( 'NONE', #22568 ) ;
#40448 = DIRECTION ( 'NONE',  ( 0.000000000000000000, -0.8827602140260367714, 0.4698238015817268742 ) ) ;
#40449 = EDGE_LOOP ( 'NONE', ( #22842, #39392, #45066, #7404 ) ) ;
#40450 =( NAMED_UNIT ( * ) SI_UNIT ( $, .STERADIAN. ) SOLID_ANGLE_UNIT ( ) );
#40451 = EDGE_CURVE ( 'NONE', #52651, #34584, #38161, .T. ) ;
#40452 = DIRECTION ( 'NONE',  ( 0.000000000000000000, -0.01356324068817999114, 0.9999080150203989437 ) ) ;
#40453 = FACE_OUTER_BOUND ( 'NONE', #1388, .T. ) ;
#40454 = ORIENTED_EDGE ( 'NONE', *, *, #5789, .F. ) ;
#40456 = DIRECTION ( 'NONE',  ( 0.000000000000000000, 0.9289767198167925288, -0.3701381553399118451 ) ) ;
#40455 = AXIS2_PLACEMENT_3D ( 'NONE', #57918, #26991, #42574 ) ;
#40457 = CARTESIAN_POINT ( 'NONE',  ( 35.00000000000000000, 11.72397916322012179, -0.7214809346829029746 ) ) ;
#40458 = CARTESIAN_POINT ( 'NONE',  ( 2.260457164927723639, -5.016645293558778640, -5.763213574030600306 ) ) ;
#40459 = ORIENTED_EDGE ( 'NONE', *, *, #31815, .T. ) ;
#40460 = ORIENTED_EDGE ( 'NONE', *, *, #25701, .T. ) ;
#40461 = DIRECTION ( 'NONE',  ( -1.000000000000000000, 0.000000000000000000, 0.000000000000000000 ) ) ;
#40462 = AXIS2_PLACEMENT_3D ( 'NONE', #7472, #58713, #7828 ) ;
#40463 = ORIENTED_EDGE ( 'NONE', *, *, #31827, .T. ) ;
#40464 = DIRECTION ( 'NONE',  ( 1.000000000000000000, -0.000000000000000000, -0.000000000000000000 ) ) ;
#40465 = DIRECTION ( 'NONE',  ( -1.000000000000000000, -0.000000000000000000, -0.000000000000000000 ) ) ;
#40466 = CARTESIAN_POINT ( 'NONE',  ( 37.00000000000000711, 11.65554240571056788, -1.456211999474385843 ) ) ;
#40467 = EDGE_CURVE ( 'NONE', #281, #60006, #13545, .T. ) ;
#40468 = CARTESIAN_POINT ( 'NONE',  ( 2.241317068080780128, 7.142175514530117120, -2.696905536171223083 ) ) ;
#40469 = AXIS2_PLACEMENT_3D ( 'NONE', #25725, #4474, #14730 ) ;
#40470 = CARTESIAN_POINT ( 'NONE',  ( 2.241352910868908310, 7.202080440908741998, 2.532612177304466972 ) ) ;
#40471 = CARTESIAN_POINT ( 'NONE',  ( -35.00000000000000000, 11.61175578952786047, 1.771820996347196697 ) ) ;
#40472 = CIRCLE ( 'NONE', #49012, 2.899999999999994582 ) ;
#40473 = EDGE_CURVE ( 'NONE', #50124, #13608, #55532, .T. ) ;
#40474 = CARTESIAN_POINT ( 'NONE',  ( -22.71097035706202760, -2.118550233809395777, -4.510116093748293586 ) ) ;
#40475 = EDGE_LOOP ( 'NONE', ( #2174, #28585, #61966, #10760 ) ) ;
#40476 = CARTESIAN_POINT ( 'NONE',  ( 0.7446945582518929019, -11.77484212699360455, 3.906659168236906954 ) ) ;
#40477 = EDGE_CURVE ( 'NONE', #37749, #21913, #41066, .T. ) ;
#40478 = DIRECTION ( 'NONE',  ( -0.000000000000000000, -0.000000000000000000, -1.000000000000000000 ) ) ;
#40479 = CARTESIAN_POINT ( 'NONE',  ( -37.00000000000000711, 2.544412758416015219, -11.91791701451263741 ) ) ;
#40480 = CARTESIAN_POINT ( 'NONE',  ( 9.963898962030125261, 13.44886489065879331, -1.176091836301444760 ) ) ;
#40481 = CARTESIAN_POINT ( 'NONE',  ( -19.69476066079020171, -4.201994156881551312, 12.82938989607585789 ) ) ;
#40482 = CARTESIAN_POINT ( 'NONE',  ( 0.2648978790185602672, 4.312320170909236694, 11.46165506714229565 ) ) ;
#40483 = LINE ( 'NONE', #23918, #6872 ) ;
#40484 = B_SPLINE_CURVE_WITH_KNOTS ( 'NONE', 3,
 ( #62777, #17895, #11585, #6622, #47193, #1636 ),
 .UNSPECIFIED., .F., .F.,
 ( 4, 2, 4 ),
 ( 0.000000000000000000, 0.0004528561986909394226, 0.0009057123973818788452 ),
 .UNSPECIFIED. ) ;
#40485 = CARTESIAN_POINT ( 'NONE',  ( -11.40165637462999904, -7.508992741355383416, 25.00000000000000000 ) ) ;
#40486 = AXIS2_PLACEMENT_3D ( 'NONE', #40052, #19128, #9145 ) ;
#40487 = CIRCLE ( 'NONE', #26687, 6.936499999999987232 ) ;
#40488 = VERTEX_POINT ( 'NONE', #43822 ) ;
#40489 = DIRECTION ( 'NONE',  ( 0.000000000000000000, 0.01356324068817991828, -0.9999080150203990547 ) ) ;
#40490 = EDGE_CURVE ( 'NONE', #8767, #44513, #65070, .T. ) ;
#40491 = CIRCLE ( 'NONE', #15051, 5.000000000000000888 ) ;
#40492 = ORIENTED_EDGE ( 'NONE', *, *, #49447, .T. ) ;
#40493 = DIRECTION ( 'NONE',  ( -1.000000000000000000, 0.000000000000000000, 0.000000000000000000 ) ) ;
#40494 = CARTESIAN_POINT ( 'NONE',  ( -22.29115169517546136, -3.712980101756718554, 0.2790989024812929875 ) ) ;
#40495 = DIRECTION ( 'NONE',  ( 0.000000000000000000, -0.01356324068817998940, 0.9999080150203990547 ) ) ;
#40496 = CARTESIAN_POINT ( 'NONE',  ( 2.781367136452037592, -7.743208838465379884, -1.052455537429842769 ) ) ;
#40497 = CARTESIAN_POINT ( 'NONE',  ( 2.000000000000001776, 3.859771122243123465, -5.613913289150012531 ) ) ;
#40498 = ORIENTED_EDGE ( 'NONE', *, *, #65634, .T. ) ;
#40499 = B_SPLINE_CURVE_WITH_KNOTS ( 'NONE', 3,
 ( #37994, #31685, #11416, #26720, #51997, #27687, #11106, #6777, #21749, #1470, #32348, #6440, #47995, #56990, #47013, #51682, #16733, #61970, #36692, #41679, #57309, #37006, #27051, #31380, #12069, #17404 ),
 .UNSPECIFIED., .F., .F.,
 ( 4, 2, 2, 2, 2, 2, 2, 2, 2, 2, 2, 2, 4 ),
 ( 7.806255641895631925E-18, 0.001111772592860239871, 0.002223545185720471936, 0.003335317778580703784, 0.004447090371440936066, 0.005002976667871053724, 0.005558862964301172251, 0.006114749260731289909, 0.006670635557161407568, 0.007226521853591526094, 0.007782408150021643753, 0.008338294446451760544, 0.008894180742881879070 ),
 .UNSPECIFIED. ) ;
#40500 = FACE_OUTER_BOUND ( 'NONE', #22360, .T. ) ;
#40502 = CIRCLE ( 'NONE', #20387, 5.000000000000001776 ) ;
#40501 = DIRECTION ( 'NONE',  ( 0.000000000000000000, 0.9868265225415254749, 0.1617819965527686754 ) ) ;
#40503 = CARTESIAN_POINT ( 'NONE',  ( -27.09048036756548683, 2.083857239072910428, 0.9969423855787087341 ) ) ;
#40504 = CARTESIAN_POINT ( 'NONE',  ( 2.241528039335008327, -6.603755931420462133, -3.830846649711583840 ) ) ;
#40505 = EDGE_CURVE ( 'NONE', #65658, #18567, #53493, .T. ) ;
#40506 = CARTESIAN_POINT ( 'NONE',  ( -37.00000000000000711, -5.814360711498210321, -10.70999494708499000 ) ) ;
#40507 = EDGE_LOOP ( 'NONE', ( #52843, #25099, #29993, #8139 ) ) ;
#40508 = CARTESIAN_POINT ( 'NONE',  ( 0.3665391374699467075, 12.13918562134721668, -1.872534962004676728 ) ) ;
#40509 = AXIS2_PLACEMENT_3D ( 'NONE', #5012, #15936, #5681 ) ;
#40510 = ORIENTED_EDGE ( 'NONE', *, *, #26860, .F. ) ;
#40511 = AXIS2_PLACEMENT_3D ( 'NONE', #9595, #10586, #19922 ) ;
#40512 = CARTESIAN_POINT ( 'NONE',  ( 0.3675815128205894289, -0.2638082659427565813, -12.27743992903066328 ) ) ;
#40513 = CARTESIAN_POINT ( 'NONE',  ( 2.000000000000001776, 0.000000000000000000, 0.000000000000000000 ) ) ;
#40514 = DIRECTION ( 'NONE',  ( 0.000000000000000000, 0.01356324068817998940, -0.9999080150203989437 ) ) ;
#40515 = CARTESIAN_POINT ( 'NONE',  ( -35.00000000000000000, -4.339012074900030491, 10.91536515067646818 ) ) ;
#40516 = AXIS2_PLACEMENT_3D ( 'NONE', #5550, #26144, #25474 ) ;
#40517 = VECTOR ( 'NONE', #25681, 1000.000000000000000 ) ;
#40518 = VECTOR ( 'NONE', #34383, 1000.000000000000000 ) ;
#40519 = ORIENTED_EDGE ( 'NONE', *, *, #40473, .T. ) ;
#40520 = ORIENTED_EDGE ( 'NONE', *, *, #30588, .T. ) ;
#40521 = CARTESIAN_POINT ( 'NONE',  ( -30.04163406560897442, 0.3900926402758986278, 12.00202977223371192 ) ) ;
#40522 = ORIENTED_EDGE ( 'NONE', *, *, #6237, .F. ) ;
#40523 = CARTESIAN_POINT ( 'NONE',  ( 35.00000000000000000, 4.705694406421931860E-17, -3.469127814946512892E-15 ) ) ;
#40524 = FACE_OUTER_BOUND ( 'NONE', #9448, .T. ) ;
#40525 = CARTESIAN_POINT ( 'NONE',  ( 37.00000000000000711, -3.473736367725341889, -12.26766708251990501 ) ) ;
#40526 = CARTESIAN_POINT ( 'NONE',  ( -27.32343372485684085, 2.674948176236206621, -1.382463360572536493 ) ) ;
#40527 = CARTESIAN_POINT ( 'NONE',  ( 1.719304012338836563, -7.017415949612288095, 10.62216384465580710 ) ) ;
#40528 = CARTESIAN_POINT ( 'NONE',  ( 1.287602823388476647, 11.16629420487894642, -5.809161206979844394 ) ) ;
#40529 = CARTESIAN_POINT ( 'NONE',  ( 0.6511581176963597839, -12.37037447926123690, -0.3309006379877566517 ) ) ;
#40530 = VERTEX_POINT ( 'NONE', #7939 ) ;
#40531 = EDGE_CURVE ( 'NONE', #36171, #56420, #23212, .T. ) ;
#40532 = CARTESIAN_POINT ( 'NONE',  ( 3.152665057734079568, -2.258875078502220024, -7.609997527621126245 ) ) ;
#40533 = ORIENTED_EDGE ( 'NONE', *, *, #16035, .T. ) ;
#40534 = CARTESIAN_POINT ( 'NONE',  ( 0.9232167919969109793, -2.570564963838065431, -12.19756235544081591 ) ) ;
#40535 = CIRCLE ( 'NONE', #62842, 4.500000000000000888 ) ;
#40536 = EDGE_CURVE ( 'NONE', #54366, #43796, #42289, .T. ) ;
#40537 = AXIS2_PLACEMENT_3D ( 'NONE', #57466, #51512, #11249 ) ;
#40538 = CARTESIAN_POINT ( 'NONE',  ( -27.09048036756548683, 1.905306051557106084, -1.306202114107871015 ) ) ;
#40539 = EDGE_LOOP ( 'NONE', ( #22996, #27190, #42120, #37845 ) ) ;
#40540 = CIRCLE ( 'NONE', #10823, 5.000000000000000888 ) ;
#40541 = DIRECTION ( 'NONE',  ( 0.000000000000000000, 0.9651210252299803338, 0.2618041379715598249 ) ) ;
#40542 = ORIENTED_EDGE ( 'NONE', *, *, #45132, .T. ) ;
#40543 = CARTESIAN_POINT ( 'NONE',  ( 26.34661844826604593, 11.53221627053869369, 3.317828791472333005 ) ) ;
#40544 = CARTESIAN_POINT ( 'NONE',  ( 5.046549821695511362, -9.819109663588886150, -9.265868187600728945 ) ) ;
#40545 = DIRECTION ( 'NONE',  ( 0.000000000000000000, 0.01356324068817992175, -0.9999080150203990547 ) ) ;
#40546 = CARTESIAN_POINT ( 'NONE',  ( 2.368238019615203971, 7.150288915654831712, -2.793778585134612413 ) ) ;
#40547 = VERTEX_POINT ( 'NONE', #43474 ) ;
#40548 = AXIS2_PLACEMENT_3D ( 'NONE', #19943, #14932, #56169 ) ;
#40549 = ORIENTED_EDGE ( 'NONE', *, *, #32438, .F. ) ;
#40550 = DIRECTION ( 'NONE',  ( 0.000000000000000000, -0.01356324068817998940, 0.9999080150203990547 ) ) ;
#40551 = VERTEX_POINT ( 'NONE', #44786 ) ;
#40552 = DIRECTION ( 'NONE',  ( 0.000000000000000000, 0.9868265225415265851, -0.1617819965527619031 ) ) ;
#40553 = ORIENTED_EDGE ( 'NONE', *, *, #42067, .T. ) ;
#40554 = CIRCLE ( 'NONE', #2366, 2.899999999999995026 ) ;
#40555 = VERTEX_POINT ( 'NONE', #64729 ) ;
#40556 = VERTEX_POINT ( 'NONE', #34489 ) ;
#40557 = CARTESIAN_POINT ( 'NONE',  ( -37.00000000000000711, 0.000000000000000000, 0.000000000000000000 ) ) ;
#40558 = ADVANCED_FACE ( 'NONE', ( #38839 ), #63753, .F. ) ;
#40559 = CARTESIAN_POINT ( 'NONE',  ( 0.9972908435452138010, -25.72582856205513480, 15.66294124711422775 ) ) ;
#40560 = CARTESIAN_POINT ( 'NONE',  ( 0.000000000000000000, 0.000000000000000000, 0.000000000000000000 ) ) ;
#40561 = FACE_OUTER_BOUND ( 'NONE', #10491, .T. ) ;
#40562 = CARTESIAN_POINT ( 'NONE',  ( 35.00000000000000000, -7.474872387601069867, -9.060822531526026680 ) ) ;
#40563 = ORIENTED_EDGE ( 'NONE', *, *, #62896, .T. ) ;
#40564 = CARTESIAN_POINT ( 'NONE',  ( 1.633930747250415205, 11.34237452761254694, 5.718685543473949195 ) ) ;
#40565 = AXIS2_PLACEMENT_3D ( 'NONE', #15618, #31570, #65273 ) ;
#40566 = VERTEX_POINT ( 'NONE', #48498 ) ;
#40567 = CARTESIAN_POINT ( 'NONE',  ( -36.00000000000000711, 12.74613886779085448, -0.3137578094507843529 ) ) ;
#40568 = CARTESIAN_POINT ( 'NONE',  ( -27.09229696323321335, 0.6397626223479224716, 2.225368503508827978 ) ) ;
#40569 = ORIENTED_EDGE ( 'NONE', *, *, #14469, .T. ) ;
#40570 = CARTESIAN_POINT ( 'NONE',  ( 0.2648321136542706733, -10.67551415837654361, 5.999882851577440057 ) ) ;
#40571 = LINE ( 'NONE', #46240, #27558 ) ;
#40572 = DIRECTION ( 'NONE',  ( -1.000000000000000000, 0.000000000000000000, 0.000000000000000000 ) ) ;
#40573 = CIRCLE ( 'NONE', #43754, 6.936499999999989008 ) ;
#40574 = EDGE_CURVE ( 'NONE', #10064, #8848, #13240, .T. ) ;
#40575 = CIRCLE ( 'NONE', #17229, 2.899999999999996803 ) ;
#40576 = CIRCLE ( 'NONE', #18291, 5.000000000000000888 ) ;
#40577 = AXIS2_PLACEMENT_3D ( 'NONE', #59804, #61108, #64762 ) ;
#40578 = VERTEX_POINT ( 'NONE', #4242 ) ;
#40579 = DIRECTION ( 'NONE',  ( -1.000000000000000000, 0.000000000000000000, 0.000000000000000000 ) ) ;
#40580 =( BOUNDED_SURFACE ( )  B_SPLINE_SURFACE ( 3, 1, ( 
 ( #43028, #19080 ),
 ( #53353, #13108 ),
 ( #38710, #59651 ),
 ( #58337, #39347 ) ),
 .UNSPECIFIED., .F., .F., .F. ) 
 B_SPLINE_SURFACE_WITH_KNOTS ( ( 4, 4 ),
 ( 2, 2 ),
 ( 0.000000000000000000, 1.000000000000000000 ),
 ( 0.000000000000000000, 1.000000000000000000 ),
 .UNSPECIFIED. ) 
 GEOMETRIC_REPRESENTATION_ITEM ( )  RATIONAL_B_SPLINE_SURFACE ( (
 ( 1.000000000000000000, 1.000000000000000000),
 ( 0.9932032654565553509, 0.8386279382598736953),
 ( 0.9932032654565553509, 0.8386279382598736953),
 ( 1.000000000000000000, 1.000000000000000000) ) ) 
 REPRESENTATION_ITEM ( '' )  SURFACE ( )  );
#40581 = ORIENTED_EDGE ( 'NONE', *, *, #65767, .T. ) ;
#40582 = DIRECTION ( 'NONE',  ( 0.000000000000000000, -0.3554799084909036067, -0.9346839223284515441 ) ) ;
#40583 = DIRECTION ( 'NONE',  ( 0.6442147435043042991, 0.000000000000000000, 0.7648446667472313942 ) ) ;
#40584 = CARTESIAN_POINT ( 'NONE',  ( -35.00000000000000000, -6.950793414699719008, -10.68873102412850074 ) ) ;
#40585 = CARTESIAN_POINT ( 'NONE',  ( 2.290907136832899482, -3.684064771923272197, -6.705538900522698853 ) ) ;
#40586 = DIRECTION ( 'NONE',  ( 1.000000000000000000, 0.000000000000000000, 0.000000000000000000 ) ) ;
#40587 = ORIENTED_EDGE ( 'NONE', *, *, #23042, .T. ) ;
#40588 = DIRECTION ( 'NONE',  ( -0.7886918350401376232, 0.6147887355352408267, 0.000000000000000000 ) ) ;
#40589 = CARTESIAN_POINT ( 'NONE',  ( -27.08429572838383947, -0.5764601019425836803, -2.217805374070540125 ) ) ;
#40590 = DIRECTION ( 'NONE',  ( -1.000000000000000000, 0.000000000000000000, 0.000000000000000000 ) ) ;
#40591 = CARTESIAN_POINT ( 'NONE',  ( -47.00000000000000711, 0.000000000000000000, 0.000000000000000000 ) ) ;
#40592 = AXIS2_PLACEMENT_3D ( 'NONE', #15339, #35613, #30310 ) ;
#40593 = EDGE_CURVE ( 'NONE', #38861, #57898, #29189, .T. ) ;
#40594 = CARTESIAN_POINT ( 'NONE',  ( 0.3006302518451990924, 12.25587491745531032, -0.2259616664572675626 ) ) ;
#40595 = CONICAL_SURFACE ( 'NONE', #11923, 7.938172270156617749, 1.280189991382167047 ) ;
#40596 = LINE ( 'NONE', #45581, #43381 ) ;
#40597 = EDGE_CURVE ( 'NONE', #29543, #30254, #38729, .T. ) ;
#40598 = CARTESIAN_POINT ( 'NONE',  ( 0.2650492594609225594, -2.234872523101260278, 12.04046128294317342 ) ) ;
#40599 = CARTESIAN_POINT ( 'NONE',  ( 1.948354844646953188, -1.364409644999331039, 11.88693049004095670 ) ) ;
#40600 = CARTESIAN_POINT ( 'NONE',  ( 2.261269890822069861, 0.1394916642590906530, -7.639767381742373686 ) ) ;
#40601 = B_SPLINE_CURVE_WITH_KNOTS ( 'NONE', 3,
 ( #65044, #19176, #49769, #44763, #39448, #59749, #35097, #9847, #14178, #34468, #60075, #9189, #39786, #30139 ),
 .UNSPECIFIED., .F., .F.,
 ( 4, 2, 2, 2, 2, 2, 4 ),
 ( 0.000000000000000000, 0.001836665365673664872, 0.002754998048510496657, 0.003673330731347328876, 0.004591663414184160227, 0.005509996097020991579, 0.007346661462694656017 ),
 .UNSPECIFIED. ) ;
#40602 = EDGE_CURVE ( 'NONE', #14759, #45661, #48142, .T. ) ;
#40603 = ORIENTED_EDGE ( 'NONE', *, *, #65740, .F. ) ;
#40604 = AXIS2_PLACEMENT_3D ( 'NONE', #62169, #6321, #21269 ) ;
#40605 = ORIENTED_EDGE ( 'NONE', *, *, #21143, .T. ) ;
#40606 = DIRECTION ( 'NONE',  ( 0.000000000000000000, 0.5243256840888503856, 0.8515178078024905339 ) ) ;
#40607 = CARTESIAN_POINT ( 'NONE',  ( 46.85239813472878723, -0.6216812786252600143, -9.954194587011503614 ) ) ;
#40608 = CARTESIAN_POINT ( 'NONE',  ( -37.00000000000000711, -5.865551165831157654, 11.32068061209293219 ) ) ;
#40609 = CARTESIAN_POINT ( 'NONE',  ( 2.298277635560819654, -1.166137492762092887, -7.564013289873369850 ) ) ;
#40610 = ORIENTED_EDGE ( 'NONE', *, *, #38489, .F. ) ;
#40611 = EDGE_CURVE ( 'NONE', #22391, #27971, #6693, .T. ) ;
#40612 = VECTOR ( 'NONE', #7013, 1000.000000000000000 ) ;
#40613 = ORIENTED_EDGE ( 'NONE', *, *, #28170, .F. ) ;
#40614 = VERTEX_POINT ( 'NONE', #18885 ) ;
#40615 = CARTESIAN_POINT ( 'NONE',  ( 5.515188684475870851, 0.0003622115669626745408, 0.005339000964282161928 ) ) ;
#40616 = CIRCLE ( 'NONE', #46990, 5.000000000000000000 ) ;
#40618 = AXIS2_PLACEMENT_3D ( 'NONE', #20741, #61292, #16060 ) ;
#40617 = CARTESIAN_POINT ( 'NONE',  ( 36.00000000000000711, 12.08151691381189963, -4.074242145636052470 ) ) ;
#40619 = ORIENTED_EDGE ( 'NONE', *, *, #24512, .F. ) ;
#40620 = CARTESIAN_POINT ( 'NONE',  ( -35.00000000000000000, -10.30098186818253758, 5.644643009979033899 ) ) ;
#40621 = CARTESIAN_POINT ( 'NONE',  ( 2.941278708680199916, -0.1348063076487378276, 6.138172921908580548 ) ) ;
#40622 = DIRECTION ( 'NONE',  ( 1.000000000000000000, 0.000000000000000000, 0.000000000000000000 ) ) ;
#40623 = ORIENTED_EDGE ( 'NONE', *, *, #2146, .F. ) ;
#40624 = CARTESIAN_POINT ( 'NONE',  ( -22.28939870658739864, 0.2834927284407818271, 3.707376022556837736 ) ) ;
#40625 = CARTESIAN_POINT ( 'NONE',  ( -6.778443870680789907, -27.08263571440718209, -15.40204062588007083 ) ) ;
#40626 = DIRECTION ( 'NONE',  ( 1.000000000000000000, -0.000000000000000000, 0.000000000000000000 ) ) ;
#40627 = ORIENTED_EDGE ( 'NONE', *, *, #55234, .T. ) ;
#40628 = CARTESIAN_POINT ( 'NONE',  ( 35.00000000000000000, -11.59605747147790211, -5.300372733891605570 ) ) ;
#40629 = VERTEX_POINT ( 'NONE', #39143 ) ;
#40630 = CARTESIAN_POINT ( 'NONE',  ( -47.00000000000000711, 0.000000000000000000, 0.000000000000000000 ) ) ;
#40631 = VERTEX_POINT ( 'NONE', #59438 ) ;
#40632 = CARTESIAN_POINT ( 'NONE',  ( 0.4613984246114877785, -8.128335150814447019, -9.246873830555978557 ) ) ;
#40633 = CARTESIAN_POINT ( 'NONE',  ( 13.41123448928980366, -10.79486891117419134, -5.246219947578315335 ) ) ;
#40634 = CARTESIAN_POINT ( 'NONE',  ( 5.514970785353741078, 0.002796696073589870733, 0.003805873180274323229 ) ) ;
#40635 = FACE_OUTER_BOUND ( 'NONE', #55964, .T. ) ;
#40636 = AXIS2_PLACEMENT_3D ( 'NONE', #36178, #27204, #41171 ) ;
#40637 = DIRECTION ( 'NONE',  ( -0.000000000000000000, -1.000000000000000000, -0.000000000000000000 ) ) ;
#40638 = CARTESIAN_POINT ( 'NONE',  ( 0.3109076770649020771, -12.25911371383827841, 0.2359198520040733382 ) ) ;
#40639 = CARTESIAN_POINT ( 'NONE',  ( 1.719304012341583476, 7.581471372739232883, -10.22720798541541498 ) ) ;
#40640 = DIRECTION ( 'NONE',  ( 0.000000000000000000, -0.01356324068818001369, 0.9999080150203990547 ) ) ;
#40641 = CARTESIAN_POINT ( 'NONE',  ( 2.034671305879987013, -4.647127512369094937, 10.71175679137298609 ) ) ;
#40643 = ORIENTED_EDGE ( 'NONE', *, *, #56850, .F. ) ;
#40642 = CARTESIAN_POINT ( 'NONE',  ( 6.993057411323677641, -4.515497414218242689, 12.72858834154033758 ) ) ;
#40644 = DIRECTION ( 'NONE',  ( -1.000000000000000000, 0.000000000000000000, 0.000000000000000000 ) ) ;
#40645 = CIRCLE ( 'NONE', #14058, 5.000000000000000888 ) ;
#40646 = ORIENTED_EDGE ( 'NONE', *, *, #17127, .T. ) ;
#40647 = DIRECTION ( 'NONE',  ( -0.000000000000000000, -1.000000000000000000, -0.000000000000000000 ) ) ;
#40648 = ORIENTED_EDGE ( 'NONE', *, *, #10190, .F. ) ;
#40649 = AXIS2_PLACEMENT_3D ( 'NONE', #55943, #11050, #30993 ) ;
#40650 = DIRECTION ( 'NONE',  ( -1.000000000000000000, 0.000000000000000000, 0.000000000000000000 ) ) ;
#40651 = ORIENTED_EDGE ( 'NONE', *, *, #57878, .T. ) ;
#40652 = CARTESIAN_POINT ( 'NONE',  ( 0.3675815128205894289, -12.27743992903066328, 0.2638082659427993804 ) ) ;
#40653 = CARTESIAN_POINT ( 'NONE',  ( 0.2671309869109484980, 6.263183022891178453, 10.52409658627918532 ) ) ;
#40654 = CARTESIAN_POINT ( 'NONE',  ( -27.08639648637141306, -2.215564006614440640, 0.6092497698725120037 ) ) ;
#40655 = CARTESIAN_POINT ( 'NONE',  ( -36.00000000000000711, -12.31350058095525846, 3.307597835713200762 ) ) ;
#40656 = EDGE_CURVE ( 'NONE', #38263, #39189, #23692, .T. ) ;
#40657 = CYLINDRICAL_SURFACE ( 'NONE', #7510, 12.18649999999999878 ) ;
#40658 = ORIENTED_EDGE ( 'NONE', *, *, #47038, .T. ) ;
#40659 = DIRECTION ( 'NONE',  ( -1.000000000000000000, 0.000000000000000000, 0.000000000000000000 ) ) ;
#40660 = EDGE_LOOP ( 'NONE', ( #43626, #60732, #7619, #50882 ) ) ;
#40661 = CARTESIAN_POINT ( 'NONE',  ( 2.491965175173379343, 0.2120508241295852025, 7.715025372670630155 ) ) ;
#40662 = DIRECTION ( 'NONE',  ( -1.000000000000000000, 0.000000000000000000, 0.000000000000000000 ) ) ;
#40663 = CARTESIAN_POINT ( 'NONE',  ( -2.822269947909834986, 4.599275498345582136, 11.08601571419042031 ) ) ;
#40664 = VERTEX_POINT ( 'NONE', #20178 ) ;
#40665 = VECTOR ( 'NONE', #22280, 1000.000000000000000 ) ;
#40666 = CIRCLE ( 'NONE', #339, 4.999999999999999112 ) ;
#40667 = CARTESIAN_POINT ( 'NONE',  ( -27.09861164373112885, -1.025570525056644033, 2.097104182796081240 ) ) ;
#40668 = CIRCLE ( 'NONE', #2430, 12.75000000000000178 ) ;
#40669 = EDGE_CURVE ( 'NONE', #61654, #21666, #2481, .T. ) ;
#40670 = CARTESIAN_POINT ( 'NONE',  ( 49.43099673984273323, -0.1154732602011161596, -5.319553669056248602 ) ) ;
#40671 = ADVANCED_FACE ( 'NONE', ( #24852 ), #19857, .T. ) ;
#40672 = VECTOR ( 'NONE', #34988, 1000.000000000000000 ) ;
#40673 = CARTESIAN_POINT ( 'NONE',  ( -35.00000000000000000, -12.26766708251994231, 3.473736367725209551 ) ) ;
#40674 = CYLINDRICAL_SURFACE ( 'NONE', #58320, 7.499999999999988454 ) ;
#40675 = EDGE_CURVE ( 'NONE', #64767, #15355, #5906, .T. ) ;
#40676 = ORIENTED_EDGE ( 'NONE', *, *, #28526, .F. ) ;
#40677 = CARTESIAN_POINT ( 'NONE',  ( 0.2653519991613807472, 2.148211862903072866, -12.05632699103096783 ) ) ;
#40678 = CARTESIAN_POINT ( 'NONE',  ( 13.92922077006917014, -33.59874296436205299, 9.921733781850763378 ) ) ;
#40679 = CARTESIAN_POINT ( 'NONE',  ( 1.634816307077032960, -3.661851000130445399, -12.16351623921555181 ) ) ;
#40680 = CIRCLE ( 'NONE', #16238, 7.499999999999988454 ) ;
#40681 = AXIS2_PLACEMENT_3D ( 'NONE', #33510, #22887, #53479 ) ;
#40682 = EDGE_CURVE ( 'NONE', #33165, #17827, #45131, .T. ) ;
#40683 = B_SPLINE_CURVE_WITH_KNOTS ( 'NONE', 3,
 ( #22931, #43185, #63458, #23242, #43503, #63785, #59800, #19572, #64441, #34819, #34187, #19234, #4615, #43851, #54495, #49193 ),
 .UNSPECIFIED., .F., .F.,
 ( 4, 3, 3, 3, 3, 4 ),
 ( 0.000000000000000000, 0.0002999043160757414064, 0.0005998071753051159626, 0.0008997092107374784131, 0.001204458948196456295, 0.001510329163478117687 ),
 .UNSPECIFIED. ) ;
#40684 = CARTESIAN_POINT ( 'NONE',  ( -35.00000000000000000, 3.704519465651306742, 11.60979404548636218 ) ) ;
#40685 = ORIENTED_EDGE ( 'NONE', *, *, #31160, .F. ) ;
#40686 = DIRECTION ( 'NONE',  ( 0.000000000000000000, -0.01356324068817998940, 0.9999080150203990547 ) ) ;
#40687 = EDGE_CURVE ( 'NONE', #57207, #50893, #10515, .T. ) ;
#40688 = CARTESIAN_POINT ( 'NONE',  ( -22.27719443589224113, 3.500848524682622198, 1.139586749255943054 ) ) ;
#40689 = CIRCLE ( 'NONE', #12019, 5.000000000000000000 ) ;
#40690 = CARTESIAN_POINT ( 'NONE',  ( -22.28694879868232803, 3.570244315741564645, -1.011812214896719686 ) ) ;
#40691 = ORIENTED_EDGE ( 'NONE', *, *, #10949, .F. ) ;
#40692 = CARTESIAN_POINT ( 'NONE',  ( 0.000000000000000000, 0.000000000000000000, 0.000000000000000000 ) ) ;
#40693 = DIRECTION ( 'NONE',  ( -1.000000000000000000, 0.000000000000000000, 0.000000000000000000 ) ) ;
#40694 = ORIENTED_EDGE ( 'NONE', *, *, #41164, .T. ) ;
#40695 = ORIENTED_EDGE ( 'NONE', *, *, #32816, .T. ) ;
#40696 = ORIENTED_EDGE ( 'NONE', *, *, #32069, .T. ) ;
#40697 = AXIS2_PLACEMENT_3D ( 'NONE', #55940, #65567, #60594 ) ;
#40698 = ORIENTED_EDGE ( 'NONE', *, *, #3875, .T. ) ;
#40699 = EDGE_CURVE ( 'NONE', #47008, #49125, #244, .T. ) ;
#40700 = CARTESIAN_POINT ( 'NONE',  ( 47.00000000000000711, 4.705694406421931860E-17, -3.469127814946512892E-15 ) ) ;
#40701 = CARTESIAN_POINT ( 'NONE',  ( -22.51237073810381162, -2.986282257334726520, 3.263711251981911143 ) ) ;
#40702 = CARTESIAN_POINT ( 'NONE',  ( 2.889800649504073782, -6.039722463373545125, 0.9965440656173527589 ) ) ;
#40703 = CARTESIAN_POINT ( 'NONE',  ( 6.511148368283224741, -4.283242813471564325, 11.20980722696366882 ) ) ;
#40704 = CARTESIAN_POINT ( 'NONE',  ( 5.515188684475870851, -0.004804816249379324430, -0.002355816063606793170 ) ) ;
#40705 = CARTESIAN_POINT ( 'NONE',  ( -7.119438362040798829, -32.04078451673858297, 13.23628618373588317 ) ) ;
#40706 = CARTESIAN_POINT ( 'NONE',  ( 24.54370396021021605, 1.234610750962751080, -13.44821043565675467 ) ) ;
#40708 = ORIENTED_EDGE ( 'NONE', *, *, #6637, .T. ) ;
#40707 = FACE_OUTER_BOUND ( 'NONE', #9326, .T. ) ;
#40709 = DIRECTION ( 'NONE',  ( -1.000000000000000000, -1.836970198721029688E-16, 0.000000000000000000 ) ) ;
#40710 = VERTEX_POINT ( 'NONE', #35468 ) ;
#40711 = VECTOR ( 'NONE', #64401, 1000.000000000000000 ) ;
#40712 = CARTESIAN_POINT ( 'NONE',  ( 37.00000000000000711, 1.791059740004421919, -12.05416472667166339 ) ) ;
#40713 = ORIENTED_EDGE ( 'NONE', *, *, #35349, .T. ) ;
#40714 = CIRCLE ( 'NONE', #16327, 12.74999999999999822 ) ;
#40715 = EDGE_LOOP ( 'NONE', ( #59140, #1371, #63082, #54220 ) ) ;
#40716 = CARTESIAN_POINT ( 'NONE',  ( -22.27756824490284160, -0.9591204781040139071, 3.555646273932171919 ) ) ;
#40717 = CARTESIAN_POINT ( 'NONE',  ( 7.310206959902322055, -27.15910349781274391, 15.27822828334930350 ) ) ;
#40719 = DIRECTION ( 'NONE',  ( 0.000000000000000000, -0.01356324068817999114, 0.9999080150203989437 ) ) ;
#40718 = AXIS2_PLACEMENT_3D ( 'NONE', #6755, #11084, #6106 ) ;
#40720 = CIRCLE ( 'NONE', #57726, 5.000000000000000888 ) ;
#40721 = CARTESIAN_POINT ( 'NONE',  ( 2.080613030138687147, 0.000000000000000000, 0.000000000000000000 ) ) ;
#40722 = DIRECTION ( 'NONE',  ( -1.000000000000000000, 0.000000000000000000, 0.000000000000000000 ) ) ;
#40723 = CARTESIAN_POINT ( 'NONE',  ( -10.00000000000000178, 0.000000000000000000, 0.000000000000000000 ) ) ;
#40724 = ORIENTED_EDGE ( 'NONE', *, *, #11374, .F. ) ;
#40725 = EDGE_LOOP ( 'NONE', ( #31903, #10947, #30669, #54385 ) ) ;
#40726 = CARTESIAN_POINT ( 'NONE',  ( -35.00000000000000000, 0.000000000000000000, 0.000000000000000000 ) ) ;
#40727 = ORIENTED_EDGE ( 'NONE', *, *, #25308, .F. ) ;
#40728 = CIRCLE ( 'NONE', #46061, 12.73084802173761787 ) ;
#40729 = VERTEX_POINT ( 'NONE', #51113 ) ;
#40730 = CIRCLE ( 'NONE', #57694, 12.18649999999999878 ) ;
#40731 = CYLINDRICAL_SURFACE ( 'NONE', #20042, 12.18649999999999878 ) ;
#40732 = DIRECTION ( 'NONE',  ( -0.3939253465568944290, -0.7103112711423410497, -0.5833358547425164797 ) ) ;
#40733 = CARTESIAN_POINT ( 'NONE',  ( 2.941278708680199916, -2.952340773940071550, -5.383216837018973244 ) ) ;
#40734 = CARTESIAN_POINT ( 'NONE',  ( 1.014383007554945815, -12.22116704270658971, 2.605923236272090993 ) ) ;
#40735 = DIRECTION ( 'NONE',  ( -1.000000000000000000, 0.000000000000000000, 0.000000000000000000 ) ) ;
#40736 = AXIS2_PLACEMENT_3D ( 'NONE', #23117, #38069, #12798 ) ;
#40737 = EDGE_CURVE ( 'NONE', #54875, #32724, #7786, .T. ) ;
#40738 = CARTESIAN_POINT ( 'NONE',  ( 0.000000000000000000, 0.000000000000000000, 0.000000000000000000 ) ) ;
#40739 = EDGE_LOOP ( 'NONE', ( #27267, #55744, #57424, #15615, #53460, #19578 ) ) ;
#40740 = ORIENTED_EDGE ( 'NONE', *, *, #49128, .F. ) ;
#40741 = CIRCLE ( 'NONE', #47120, 2.899999999999995026 ) ;
#40742 = DIRECTION ( 'NONE',  ( 1.000000000000000000, -0.000000000000000000, -0.000000000000000000 ) ) ;
#40743 = DIRECTION ( 'NONE',  ( 0.000000000000000000, 1.000000000000000000, -0.000000000000000000 ) ) ;
#40744 = EDGE_CURVE ( 'NONE', #48793, #42095, #45443, .T. ) ;
#40745 = DIRECTION ( 'NONE',  ( -1.000000000000000000, -0.000000000000000000, 0.000000000000000000 ) ) ;
#40746 = CARTESIAN_POINT ( 'NONE',  ( 6.550563172034069126, -7.779754947801418297, 9.145170272292368452 ) ) ;
#40747 = VECTOR ( 'NONE', #36937, 1000.000000000000000 ) ;
#40748 = EDGE_CURVE ( 'NONE', #64826, #30538, #62501, .T. ) ;
#40749 = CARTESIAN_POINT ( 'NONE',  ( 3.426183256940671829, -10.95277051985667605, 4.917698437020844082 ) ) ;
#40750 = B_SPLINE_CURVE_WITH_KNOTS ( 'NONE', 3,
 ( #14687, #5403, #424, #9717, #4772, #30004, #35312, #45968, #5748, #10059, #45303, #20693, #24700, #40638, #61247, #35642, #40298, #64915, #39660, #55624, #55937, #9378 ),
 .UNSPECIFIED., .F., .F.,
 ( 4, 3, 3, 3, 3, 3, 3, 4 ),
 ( 1.149970062512530604E-18, 4.449119708436735838E-05, 6.626296329540299560E-05, 8.803456484962497708E-05, 0.0001098060367612783733, 0.0001315774408628487678, 0.0001760698110411146094, 0.0001829697163287828600 ),
 .UNSPECIFIED. ) ;
#40751 = CARTESIAN_POINT ( 'NONE',  ( 5.514970785353741078, 0.004694330894494710971, 0.0005190732562555225478 ) ) ;
#40752 = EDGE_CURVE ( 'NONE', #5409, #16864, #25167, .T. ) ;
#40753 = CARTESIAN_POINT ( 'NONE',  ( 3.415098594035642421, 3.602609866107200354, -11.44847010818049604 ) ) ;
#40754 = B_SPLINE_CURVE_WITH_KNOTS ( 'NONE', 3,
 ( #58957, #27343, #64239, #42620, #22709, #2773, #62925, #18714, #17389, #23032 ),
 .UNSPECIFIED., .F., .F.,
 ( 4, 3, 3, 4 ),
 ( 5.401523115762188335E-05, 0.0008136511341527786004, 0.004068255670953086281, 0.005063778443040916136 ),
 .UNSPECIFIED. ) ;
#40755 = CARTESIAN_POINT ( 'NONE',  ( -27.08416781016246588, -2.158663327075695637, -0.7680651426971915052 ) ) ;
#40756 = EDGE_CURVE ( 'NONE', #29429, #32831, #16275, .T. ) ;
#40757 = B_SPLINE_CURVE_WITH_KNOTS ( 'NONE', 3,
 ( #20338, #60918, #62527, #57909, #42563, #7020, #51930, #31942, #22980, #16988 ),
 .UNSPECIFIED., .F., .F.,
 ( 4, 3, 3, 4 ),
 ( 1.075835082704897855E-17, 6.991367980366405095E-05, 0.0001398269368981362064, 0.0001763147164361797566 ),
 .UNSPECIFIED. ) ;
#40758 = VERTEX_POINT ( 'NONE', #31149 ) ;
#40759 = AXIS2_PLACEMENT_3D ( 'NONE', #18869, #24170, #34776 ) ;
#40760 = DIRECTION ( 'NONE',  ( 1.000000000000000000, 0.000000000000000000, 0.000000000000000000 ) ) ;
#40761 = VECTOR ( 'NONE', #44800, 1000.000000000000000 ) ;
#40762 = DIRECTION ( 'NONE',  ( 0.000000000000000000, 0.01356324068817998940, -0.9999080150203990547 ) ) ;
#40763 = B_SPLINE_CURVE_WITH_KNOTS ( 'NONE', 3,
 ( #52561, #63804, #37576, #16957, #8296, #28566, #27927, #48236, #7987, #52864, #23256, #22615, #2685, #58870, #6989, #63167 ),
 .UNSPECIFIED., .F., .F.,
 ( 4, 3, 3, 3, 3, 4 ),
 ( 2.710505431213761085E-19, 0.0003017745587525226449, 0.0006035491769808692952, 0.0009053241094668096345, 0.001207275924541012166, 0.001510325902535038321 ),
 .UNSPECIFIED. ) ;
#40764 = CIRCLE ( 'NONE', #49297, 12.18650000000000233 ) ;
#40765 = CARTESIAN_POINT ( 'NONE',  ( 0.2851083653049504285, -0.4107471485392698018, 25.00000000000000000 ) ) ;
#40766 = CARTESIAN_POINT ( 'NONE',  ( -37.00000000000000711, -12.08151691381193160, 4.074242145635959211 ) ) ;
#40767 = CIRCLE ( 'NONE', #18490, 5.000000000000000888 ) ;
#40768 = ORIENTED_EDGE ( 'NONE', *, *, #46011, .T. ) ;
#40769 = DIRECTION ( 'NONE',  ( 0.000000000000000000, 0.000000000000000000, 1.000000000000000000 ) ) ;
#40770 = CARTESIAN_POINT ( 'NONE',  ( 3.100650473569588783, 6.622643684997381541, 4.345221797103435257 ) ) ;
#40771 = EDGE_CURVE ( 'NONE', #29925, #59870, #5415, .T. ) ;
#40772 = CIRCLE ( 'NONE', #52471, 12.74999999999999822 ) ;
#40773 = CARTESIAN_POINT ( 'NONE',  ( 12.50310467286144167, -29.27802453453052323, -5.021082754746766241 ) ) ;
#40774 = ORIENTED_EDGE ( 'NONE', *, *, #65343, .F. ) ;
#40775 = DIRECTION ( 'NONE',  ( 0.000000000000000000, 0.000000000000000000, 1.000000000000000000 ) ) ;
#40776 = DIRECTION ( 'NONE',  ( -1.000000000000000000, 0.000000000000000000, 0.000000000000000000 ) ) ;
#40777 = CARTESIAN_POINT ( 'NONE',  ( -22.27706485742869091, -0.9221835209182183135, -3.563814065926679042 ) ) ;
#40778 = EDGE_CURVE ( 'NONE', #48808, #19993, #31776, .T. ) ;
#40779 = AXIS2_PLACEMENT_3D ( 'NONE', #11366, #1076, #30655 ) ;
#40781 = VERTEX_POINT ( 'NONE', #36461 ) ;
#40780 = CARTESIAN_POINT ( 'NONE',  ( -35.00000000000000000, -7.146664589317976102, 9.321877890560418933 ) ) ;
#40782 = FACE_OUTER_BOUND ( 'NONE', #47814, .T. ) ;
#40783 = ADVANCED_FACE ( 'NONE', ( #6537 ), #22144, .T. ) ;
#40784 = CARTESIAN_POINT ( 'NONE',  ( 2.781367136452309818, -7.442815111163310959, -2.381060477055452651 ) ) ;
#40785 = EDGE_CURVE ( 'NONE', #60941, #51695, #50646, .T. ) ;
#40786 = ORIENTED_EDGE ( 'NONE', *, *, #24683, .F. ) ;
#40787 = ADVANCED_FACE ( 'NONE', ( #26473 ), #56296, .F. ) ;
#40788 = CYLINDRICAL_SURFACE ( 'NONE', #11055, 12.75000000000000178 ) ;
#40789 = CARTESIAN_POINT ( 'NONE',  ( -9.130651553988846203, 12.72949299159512115, -4.509469149381835962 ) ) ;
#40790 = DIRECTION ( 'NONE',  ( 0.000000000000000000, 0.8276889981568920085, -0.5611870653623802774 ) ) ;
#40791 = FACE_OUTER_BOUND ( 'NONE', #45898, .T. ) ;
#40792 =( BOUNDED_SURFACE ( )  B_SPLINE_SURFACE ( 3, 1, ( 
 ( #62007, #37041 ),
 ( #58009, #31720 ),
 ( #53004, #7434 ),
 ( #51714, #6155 ) ),
 .UNSPECIFIED., .F., .F., .F. ) 
 B_SPLINE_SURFACE_WITH_KNOTS ( ( 4, 4 ),
 ( 2, 2 ),
 ( 0.000000000000000000, 1.000000000000000000 ),
 ( 0.000000000000000000, 1.000000000000000000 ),
 .UNSPECIFIED. ) 
 GEOMETRIC_REPRESENTATION_ITEM ( )  RATIONAL_B_SPLINE_SURFACE ( (
 ( 1.000000000000000000, 1.000000000000000000),
 ( 0.6933888150995267674, 0.9895912004443193632),
 ( 0.6933888150995267674, 0.9895912004443193632),
 ( 1.000000000000000000, 1.000000000000000000) ) ) 
 REPRESENTATION_ITEM ( '' )  SURFACE ( )  );
#40793 = CARTESIAN_POINT ( 'NONE',  ( 0.000000000000000000, 6.441884263200846839, -2.217201541069800275 ) ) ;
#40794 = EDGE_CURVE ( 'NONE', #59884, #41431, #23673, .T. ) ;
#40795 = CARTESIAN_POINT ( 'NONE',  ( -27.78468958554971380, 25.00000000000000000, 8.565911087387465983 ) ) ;
#40796 = CARTESIAN_POINT ( 'NONE',  ( 0.2646305136544072623, 10.53923716745246963, 6.237419468587114046 ) ) ;
#40797 = VERTEX_POINT ( 'NONE', #32113 ) ;
#40798 = CARTESIAN_POINT ( 'NONE',  ( 35.00000000000000000, 8.352657516904789858, 8.258652103341336925 ) ) ;
#40799 = VERTEX_POINT ( 'NONE', #22480 ) ;
#40800 = DIRECTION ( 'NONE',  ( 0.000000000000000000, 0.01356324068818000328, -0.9999080150203990547 ) ) ;
#40801 = CARTESIAN_POINT ( 'NONE',  ( 2.844750968616289732, 1.686994672842381693, 7.651810733888897431 ) ) ;
#40802 = VECTOR ( 'NONE', #3061, 1000.000000000000000 ) ;
#40803 = CYLINDRICAL_SURFACE ( 'NONE', #9732, 7.499999999999988454 ) ;
#40804 = ORIENTED_EDGE ( 'NONE', *, *, #631, .T. ) ;
#40805 = DIRECTION ( 'NONE',  ( 1.000000000000000000, 0.000000000000000000, 0.000000000000000000 ) ) ;
#40806 = DIRECTION ( 'NONE',  ( -1.000000000000000000, 0.000000000000000000, 0.000000000000000000 ) ) ;
#40807 = CARTESIAN_POINT ( 'NONE',  ( -22.27722015946438816, -1.271715168852058708, 3.455127654605140819 ) ) ;
#40808 = EDGE_LOOP ( 'NONE', ( #50648, #22907, #8942, #19088 ) ) ;
#40809 = ORIENTED_EDGE ( 'NONE', *, *, #34251, .F. ) ;
#40810 = CARTESIAN_POINT ( 'NONE',  ( 2.280717697723834814, -7.238333660707024109, -2.468022724683533564 ) ) ;
#40811 = AXIS2_PLACEMENT_3D ( 'NONE', #30062, #4492, #25088 ) ;
#40812 = VECTOR ( 'NONE', #2924, 1000.000000000000000 ) ;
#40813 = ORIENTED_EDGE ( 'NONE', *, *, #19973, .T. ) ;
#40814 = CARTESIAN_POINT ( 'NONE',  ( 35.00000000000000000, 4.705694406421931860E-17, -3.469127814946512892E-15 ) ) ;
#40815 = LINE ( 'NONE', #25181, #57589 ) ;
#40816 = DIRECTION ( 'NONE',  ( 0.000000000000000000, 0.000000000000000000, 1.000000000000000000 ) ) ;
#40817 = CARTESIAN_POINT ( 'NONE',  ( 2.257661810676420799, 7.131864446283263881, -2.739276463085611901 ) ) ;
#40818 = EDGE_CURVE ( 'NONE', #48048, #5162, #62368, .T. ) ;
#40819 = CARTESIAN_POINT ( 'NONE',  ( 0.2653141334712582622, -10.58342934917116018, 6.161213243425222252 ) ) ;
#40820 = CARTESIAN_POINT ( 'NONE',  ( 0.3675815128205894289, 11.62724744438065727, 3.951233083390508050 ) ) ;
#40821 = VERTEX_POINT ( 'NONE', #57401 ) ;
#40822 = DIRECTION ( 'NONE',  ( 0.000000000000000000, -0.7621620551276424571, 0.6473862847818206978 ) ) ;
#40823 = CARTESIAN_POINT ( 'NONE',  ( 22.64108410429532370, 10.50347544506924891, -5.812766615855110786 ) ) ;
#40824 = CARTESIAN_POINT ( 'NONE',  ( 5.530133899448235191, 0.006998616117864070972, -0.01437126147332074694 ) ) ;
#40825 = FACE_OUTER_BOUND ( 'NONE', #29203, .T. ) ;
#40826 = AXIS2_PLACEMENT_3D ( 'NONE', #55643, #29682, #40001 ) ;
#40827 = CARTESIAN_POINT ( 'NONE',  ( -19.55186598411636467, -3.901828651817480953, 12.92480312515320229 ) ) ;
#40828 = DIRECTION ( 'NONE',  ( 1.000000000000000000, 0.000000000000000000, 0.000000000000000000 ) ) ;
#40829 = DIRECTION ( 'NONE',  ( -0.000000000000000000, -0.000000000000000000, -1.000000000000000000 ) ) ;
#40830 = EDGE_CURVE ( 'NONE', #35611, #51290, #2202, .T. ) ;
#40831 = CYLINDRICAL_SURFACE ( 'NONE', #52280, 12.18649999999999878 ) ;
#40833 = AXIS2_PLACEMENT_3D ( 'NONE', #15620, #35891, #46548 ) ;
#40832 = AXIS2_PLACEMENT_3D ( 'NONE', #14507, #9518, #64403 ) ;
#40834 = ORIENTED_EDGE ( 'NONE', *, *, #9218, .F. ) ;
#40835 = DIRECTION ( 'NONE',  ( 1.000000000000000000, 0.000000000000000000, 0.000000000000000000 ) ) ;
#40836 = VERTEX_POINT ( 'NONE', #62694 ) ;
#40837 = CARTESIAN_POINT ( 'NONE',  ( -2.747351760715558200, -5.743695276321967746, 10.56617162187726322 ) ) ;
#40838 = CARTESIAN_POINT ( 'NONE',  ( -35.00000000000000000, -5.814360711498210321, -10.70999494708499000 ) ) ;
#40839 = AXIS2_PLACEMENT_3D ( 'NONE', #26742, #16099, #32040 ) ;
#40840 = CARTESIAN_POINT ( 'NONE',  ( 5.514970785353741078, 0.002619824551223701864, 0.003929719953530115030 ) ) ;
#40841 = CARTESIAN_POINT ( 'NONE',  ( 2.491965175173920688, -7.634639040875003779, -1.130870800982851865 ) ) ;
#40842 = CYLINDRICAL_SURFACE ( 'NONE', #48805, 12.18649999999999878 ) ;
#40843 = EDGE_CURVE ( 'NONE', #29123, #22816, #10934, .T. ) ;
#40844 = ORIENTED_EDGE ( 'NONE', *, *, #46160, .T. ) ;
#40845 = CARTESIAN_POINT ( 'NONE',  ( 0.000000000000000000, 0.000000000000000000, 0.000000000000000000 ) ) ;
#40846 = DIRECTION ( 'NONE',  ( 0.000000000000000000, 0.4198891015602590482, 0.9075754196709595600 ) ) ;
#40847 = DIRECTION ( 'NONE',  ( 1.000000000000000000, 0.000000000000000000, 0.000000000000000000 ) ) ;
#40848 = CARTESIAN_POINT ( 'NONE',  ( -27.20102706715913499, -0.5453431011645057946, 2.585824624629319946 ) ) ;
#40849 = AXIS2_PLACEMENT_3D ( 'NONE', #34821, #45159, #65417 ) ;
#40850 = B_SPLINE_CURVE_WITH_KNOTS ( 'NONE', 3,
 ( #43371, #53036, #63996, #59340, #18786, #48717 ),
 .UNSPECIFIED., .F., .F.,
 ( 4, 2, 4 ),
 ( 0.0001654224980408358430, 0.0006219428995476486118, 0.001078463301054461299 ),
 .UNSPECIFIED. ) ;
#40851 = CARTESIAN_POINT ( 'NONE',  ( -17.39032955383490275, -6.043477806738668079, 10.36841493105847611 ) ) ;
#40852 = CARTESIAN_POINT ( 'NONE',  ( 2.241352910868908310, 2.689314586382351546, 7.145045428366586293 ) ) ;
#40853 = VERTEX_POINT ( 'NONE', #3538 ) ;
#40854 = CARTESIAN_POINT ( 'NONE',  ( -27.10719052120871098, -0.5475695427849570640, 2.295785794152556125 ) ) ;
#40855 = ORIENTED_EDGE ( 'NONE', *, *, #33952, .T. ) ;
#40856 = CARTESIAN_POINT ( 'NONE',  ( 0.2648978790185602672, -0.1321385342561549048, -12.24533305150758267 ) ) ;
#40857 = FACE_OUTER_BOUND ( 'NONE', #3966, .T. ) ;
#40858 = DIRECTION ( 'NONE',  ( -1.000000000000000000, 0.000000000000000000, 0.000000000000000000 ) ) ;
#40859 = CYLINDRICAL_SURFACE ( 'NONE', #16071, 4.999999999999999112 ) ;
#40860 = EDGE_CURVE ( 'NONE', #34948, #5010, #62973, .T. ) ;
#40861 = ORIENTED_EDGE ( 'NONE', *, *, #5390, .F. ) ;
#40862 = EDGE_LOOP ( 'NONE', ( #4483, #30147, #9762, #19879 ) ) ;
#40863 = CARTESIAN_POINT ( 'NONE',  ( 0.2638984909335716500, -1.930290337333974593, -12.09426044257626209 ) ) ;
#40864 = EDGE_CURVE ( 'NONE', #5514, #44, #5666, .T. ) ;
#40865 = ORIENTED_EDGE ( 'NONE', *, *, #24074, .T. ) ;
#40866 = CARTESIAN_POINT ( 'NONE',  ( -35.00000000000000000, -7.376655759824951808, 9.700295462048636352 ) ) ;
#40867 = CARTESIAN_POINT ( 'NONE',  ( 2.241352910868909643, -7.145045428366594287, 2.689314586382326677 ) ) ;
#40868 = CARTESIAN_POINT ( 'NONE',  ( 1.937114397841932290, 10.63710405811933946, 7.182898292393801398 ) ) ;
#40869 = CARTESIAN_POINT ( 'NONE',  ( 1.287602823384980555, 9.277923463524217595, 8.506034117234060332 ) ) ;
#40870 = LINE ( 'NONE', #51189, #49199 ) ;
#40871 = EDGE_CURVE ( 'NONE', #2584, #64575, #15741, .T. ) ;
#40872 = CARTESIAN_POINT ( 'NONE',  ( 0.5572780756290610649, 10.83930267798936420, -5.905274004878195093 ) ) ;
#40873 = DIRECTION ( 'NONE',  ( -1.000000000000000000, 0.000000000000000000, 0.000000000000000000 ) ) ;
#40874 = VERTEX_POINT ( 'NONE', #33102 ) ;
#40876 = CIRCLE ( 'NONE', #12193, 4.999999999999999112 ) ;
#40875 =( REPRESENTATION_RELATIONSHIP ('NONE','NONE', #63658, #25052 ) REPRESENTATION_RELATIONSHIP_WITH_TRANSFORMATION ( #27140 )SHAPE_REPRESENTATION_RELATIONSHIP( ) );
#40877 = CARTESIAN_POINT ( 'NONE',  ( -9.289599981290024289, -10.79669820059283758, -5.251390403865245027 ) ) ;
#40878 = EDGE_LOOP ( 'NONE', ( #48390, #53818, #64968, #3334 ) ) ;
#40879 = CARTESIAN_POINT ( 'NONE',  ( -35.04834644901396956, -0.007161132384425688939, -0.01183641858480926831 ) ) ;
#40880 = AXIS2_PLACEMENT_3D ( 'NONE', #16741, #48002, #7093 ) ;
#40881 = DIRECTION ( 'NONE',  ( 0.000000000000000000, -0.01356324068817991828, 0.9999080150203990547 ) ) ;
#40882 = ORIENTED_EDGE ( 'NONE', *, *, #17117, .T. ) ;
#40883 = CARTESIAN_POINT ( 'NONE',  ( 2.000000000000001776, 0.000000000000000000, 0.000000000000000000 ) ) ;
#40884 = EDGE_LOOP ( 'NONE', ( #20081, #63215, #19734, #48322, #50643, #1145 ) ) ;
#40885 = CARTESIAN_POINT ( 'NONE',  ( 2.000000000000001776, -1.956810415765224187, 6.654767106875530303 ) ) ;
#40886 = CARTESIAN_POINT ( 'NONE',  ( 4.915077328917121235, -9.915524164001334739, -9.162427078388006407 ) ) ;
#40887 = CARTESIAN_POINT ( 'NONE',  ( -36.00000000000000711, 0.9416912585474430664, 12.71517666308948513 ) ) ;
#40888 = CARTESIAN_POINT ( 'NONE',  ( -27.08702828306176258, -2.226264228964706327, -0.5765135930309283063 ) ) ;
#40889 = EDGE_LOOP ( 'NONE', ( #64043, #22674, #20721, #36989 ) ) ;
#40890 = ORIENTED_EDGE ( 'NONE', *, *, #29562, .T. ) ;
#40891 = CARTESIAN_POINT ( 'NONE',  ( 3.152665057734129750, -7.102135024645910732, 3.546019893116286958 ) ) ;
#40892 = EDGE_LOOP ( 'NONE', ( #20750, #2723, #37245, #4363 ) ) ;
#40893 = CARTESIAN_POINT ( 'NONE',  ( 0.9232167919969109793, -11.84868134597554423, -3.872606616958390369 ) ) ;
#40894 = ORIENTED_EDGE ( 'NONE', *, *, #6684, .T. ) ;
#40895 = ORIENTED_EDGE ( 'NONE', *, *, #47258, .T. ) ;
#40896 = ORIENTED_EDGE ( 'NONE', *, *, #45180, .T. ) ;
#40897 = DIRECTION ( 'NONE',  ( 0.000000000000000000, 0.9847383929261624980, -0.1740410799127578012 ) ) ;
#40898 = DIRECTION ( 'NONE',  ( 0.000000000000000000, 0.6478160128811947249, -0.7617968321374877227 ) ) ;
#40899 = CIRCLE ( 'NONE', #53629, 2.899999999999994582 ) ;
#40900 = EDGE_CURVE ( 'NONE', #6695, #18713, #13467, .T. ) ;
#40901 = CARTESIAN_POINT ( 'NONE',  ( -23.18047892478189453, 4.338318103648307833, -2.037851053449307948 ) ) ;
#40902 = DIRECTION ( 'NONE',  ( -1.000000000000000000, 0.000000000000000000, 0.000000000000000000 ) ) ;
#40903 = EDGE_LOOP ( 'NONE', ( #4476, #47133, #11316, #18429 ) ) ;
#40904 = CARTESIAN_POINT ( 'NONE',  ( -35.00000000000000000, 10.30098186818257666, -5.644643009978957515 ) ) ;
#40905 = EDGE_CURVE ( 'NONE', #24684, #4330, #59803, .T. ) ;
#40906 = ORIENTED_EDGE ( 'NONE', *, *, #9030, .F. ) ;
#40907 = DIRECTION ( 'NONE',  ( -1.000000000000000000, 0.000000000000000000, 0.000000000000000000 ) ) ;
#40908 = DIRECTION ( 'NONE',  ( -1.000000000000000000, -0.000000000000000000, 0.000000000000000000 ) ) ;
#40909 = DIRECTION ( 'NONE',  ( 1.000000000000000000, -0.000000000000000000, 0.000000000000000000 ) ) ;
#40910 = CARTESIAN_POINT ( 'NONE',  ( -18.49080574448724690, -13.49999999999999822, -2.827202046691532642E-15 ) ) ;
#40911 = CARTESIAN_POINT ( 'NONE',  ( 37.00000000000000711, 10.64792938439763859, 5.927257550915197015 ) ) ;
#40912 = LINE ( 'NONE', #25955, #52533 ) ;
#40913 = CARTESIAN_POINT ( 'NONE',  ( 0.8375941296816821202, -10.57337970710580599, -6.548446001456700749 ) ) ;
#40914 = ADVANCED_FACE ( 'NONE', ( #28129 ), #34420, .T. ) ;
#40915 = ORIENTED_EDGE ( 'NONE', *, *, #43712, .T. ) ;
#40916 = CARTESIAN_POINT ( 'NONE',  ( 0.000000000000000000, -1.865193240757140991, 6.552473556515165498 ) ) ;
#40917 = VERTEX_POINT ( 'NONE', #8828 ) ;
#40918 = CARTESIAN_POINT ( 'NONE',  ( 35.00000000000000000, -11.72195762423410414, -0.7536123767498126291 ) ) ;
#40919 = CARTESIAN_POINT ( 'NONE',  ( 19.22959543997423637, -28.98134239863147954, -5.957279114860658531 ) ) ;
#40920 = CARTESIAN_POINT ( 'NONE',  ( 1.014403380171174041, -26.55354399125274867, 16.22408933255776731 ) ) ;
#40921 = CARTESIAN_POINT ( 'NONE',  ( 2.241311220309521790, -3.736531646286333164, -6.657499176698745913 ) ) ;
#40922 = CARTESIAN_POINT ( 'NONE',  ( 2.000000000000001776, 6.606214214351074254, 2.114938770769925647 ) ) ;
#40923 = ADVANCED_FACE ( 'NONE', ( #2876 ), #43739, .T. ) ;
#40924 = EDGE_CURVE ( 'NONE', #11428, #16086, #54053, .T. ) ;
#40925 = ORIENTED_EDGE ( 'NONE', *, *, #59979, .F. ) ;
#40926 = DIRECTION ( 'NONE',  ( -1.000000000000000000, 0.000000000000000000, 0.000000000000000000 ) ) ;
#40927 = DIRECTION ( 'NONE',  ( 1.000000000000000000, 0.000000000000000000, 0.000000000000000000 ) ) ;
#40928 = CARTESIAN_POINT ( 'NONE',  ( 2.903928887688524529, 2.041797854847264393, 8.528865300111828418 ) ) ;
#40929 = CARTESIAN_POINT ( 'NONE',  ( 1.719304012339844867, -12.64775761152577971, 1.452142814149586902 ) ) ;
#40930 = EDGE_CURVE ( 'NONE', #46588, #646, #33259, .T. ) ;
#40931 = CARTESIAN_POINT ( 'NONE',  ( 0.2834382757448002943, 12.25055062943084927, -0.2027202995057415524 ) ) ;
#40932 = CARTESIAN_POINT ( 'NONE',  ( 1.937114397841935398, -5.226660192101514113, -11.72279974487468834 ) ) ;
#40933 = CARTESIAN_POINT ( 'NONE',  ( 0.2652384770603652409, -2.191555293694056328, 12.04846497255942062 ) ) ;
#40934 = FACE_OUTER_BOUND ( 'NONE', #10598, .T. ) ;
#40935 = CARTESIAN_POINT ( 'NONE',  ( 35.00000000000000000, 4.705694406421931860E-17, -3.469127814946512892E-15 ) ) ;
#40936 = ADVANCED_FACE ( 'NONE', ( #55356 ), #30078, .T. ) ;
#40937 = VECTOR ( 'NONE', #14325, 1000.000000000000000 ) ;
#40938 = EDGE_LOOP ( 'NONE', ( #46370, #29453, #42050, #61142 ) ) ;
#40939 = EDGE_CURVE ( 'NONE', #3105, #18651, #45091, .T. ) ;
#40940 = ORIENTED_EDGE ( 'NONE', *, *, #11683, .F. ) ;
#40941 = CARTESIAN_POINT ( 'NONE',  ( -16.00005080000000035, 0.000000000000000000, -2.999999999999995559 ) ) ;
#40942 = DIRECTION ( 'NONE',  ( 0.000000000000000000, 0.01356324068817999114, -0.9999080150203990547 ) ) ;
#40943 = CARTESIAN_POINT ( 'NONE',  ( -35.00000000000000000, 11.13736569743281457, -4.946702696913053643 ) ) ;
#40944 = CARTESIAN_POINT ( 'NONE',  ( 2.249013661412873066, -1.207748565001795393, -7.540851674529120530 ) ) ;
#40945 = VERTEX_POINT ( 'NONE', #5494 ) ;
#40946 = ORIENTED_EDGE ( 'NONE', *, *, #41792, .F. ) ;
#40947 = EDGE_LOOP ( 'NONE', ( #30962, #54725, #10961, #50370 ) ) ;
#40948 = CARTESIAN_POINT ( 'NONE',  ( 29.66301245255163366, -8.641839016897280956, 8.340436526386785232 ) ) ;
#40949 = CARTESIAN_POINT ( 'NONE',  ( -21.17861794710831091, -11.44571409049744481, -3.604945070120774808 ) ) ;
#40950 = ORIENTED_EDGE ( 'NONE', *, *, #101, .F. ) ;
#40951 = DIRECTION ( 'NONE',  ( 1.000000000000000000, 0.000000000000000000, -0.000000000000000000 ) ) ;
#40952 = CARTESIAN_POINT ( 'NONE',  ( 37.00000000000000711, 11.66664283989686979, 5.143145423404151373 ) ) ;
#40953 = ORIENTED_EDGE ( 'NONE', *, *, #23288, .T. ) ;
#40954 = AXIS2_PLACEMENT_3D ( 'NONE', #6910, #12861, #53107 ) ;
#40955 = CARTESIAN_POINT ( 'NONE',  ( -37.00000000000000711, 8.258652103341553641, -8.352657516904583801 ) ) ;
#40956 = CARTESIAN_POINT ( 'NONE',  ( 7.085269882676524134, -28.78331678329937304, -12.46778293907698121 ) ) ;
#40957 = FACE_OUTER_BOUND ( 'NONE', #44911, .T. ) ;
#40958 = ORIENTED_EDGE ( 'NONE', *, *, #46028, .F. ) ;
#40959 = DIRECTION ( 'NONE',  ( -0.000000000000000000, -0.000000000000000000, -1.000000000000000000 ) ) ;
#40960 = ORIENTED_EDGE ( 'NONE', *, *, #16703, .F. ) ;
#40961 = CARTESIAN_POINT ( 'NONE',  ( 1.462291587750005561, -10.08151577214924188, 7.633056170898021797 ) ) ;
#40962 = EDGE_LOOP ( 'NONE', ( #16353, #39596, #27888, #55806 ) ) ;
#40963 = DIRECTION ( 'NONE',  ( -1.000000000000000000, 0.000000000000000000, 0.000000000000000000 ) ) ;
#40964 = AXIS2_PLACEMENT_3D ( 'NONE', #35392, #51038, #50710 ) ;
#40965 = DIRECTION ( 'NONE',  ( -1.000000000000000000, 0.000000000000000000, 0.000000000000000000 ) ) ;
#40966 = CARTESIAN_POINT ( 'NONE',  ( 2.276905613633651182, 3.955794200962202911, 6.543460433228652562 ) ) ;
#40967 = DIRECTION ( 'NONE',  ( 0.000000000000000000, -0.2355298848897378061, -0.9718671068226493182 ) ) ;
#40968 = DIRECTION ( 'NONE',  ( -1.000000000000000000, -0.000000000000000000, 0.000000000000000000 ) ) ;
#40969 = DIRECTION ( 'NONE',  ( 0.000000000000000000, -0.000000000000000000, 1.000000000000000000 ) ) ;
#40970 = DIRECTION ( 'NONE',  ( 0.000000000000000000, 1.000000000000000000, 0.000000000000000000 ) ) ;
#40971 = LINE ( 'NONE', #26996, #13991 ) ;
#40973 = ORIENTED_EDGE ( 'NONE', *, *, #22089, .F. ) ;
#40972 = CARTESIAN_POINT ( 'NONE',  ( 6.601852703653428911, -8.834089529978390587, 10.21601470017478341 ) ) ;
#40974 = CARTESIAN_POINT ( 'NONE',  ( -22.51237073810381162, -4.418556976583611906, 0.2145858836692225990 ) ) ;
#40975 = EDGE_CURVE ( 'NONE', #37151, #29673, #26909, .T. ) ;
#40976 =( BOUNDED_SURFACE ( )  B_SPLINE_SURFACE ( 3, 1, ( 
 ( #49427, #60036 ),
 ( #34729, #44081 ),
 ( #64662, #13795 ),
 ( #48434, #43748 ) ),
 .UNSPECIFIED., .F., .F., .F. ) 
 B_SPLINE_SURFACE_WITH_KNOTS ( ( 4, 4 ),
 ( 2, 2 ),
 ( 0.000000000000000000, 1.000000000000000000 ),
 ( 0.000000000000000000, 1.000000000000000000 ),
 .UNSPECIFIED. ) 
 GEOMETRIC_REPRESENTATION_ITEM ( )  RATIONAL_B_SPLINE_SURFACE ( (
 ( 1.000000000000000000, 1.000000000000000000),
 ( 0.6933888150995267674, 0.9895912004443193632),
 ( 0.6933888150995267674, 0.9895912004443193632),
 ( 1.000000000000000000, 1.000000000000000000) ) ) 
 REPRESENTATION_ITEM ( '' )  SURFACE ( )  );
#40977 = ORIENTED_EDGE ( 'NONE', *, *, #9075, .T. ) ;
#40978 = CARTESIAN_POINT ( 'NONE',  ( 12.37382948190224141, -10.69513828756983287, -8.245931121816388654 ) ) ;
#40979 = ORIENTED_EDGE ( 'NONE', *, *, #47258, .F. ) ;
#40980 = CARTESIAN_POINT ( 'NONE',  ( 2.963017218115631124, -5.778072204777605414, -5.350609950027729766 ) ) ;
#40981 = VERTEX_POINT ( 'NONE', #46051 ) ;
#40982 = CARTESIAN_POINT ( 'NONE',  ( -35.00000000000000000, 2.865935305911801123, -12.42372387097879383 ) ) ;
#40983 = CARTESIAN_POINT ( 'NONE',  ( 0.3675815128205912052, 11.62724744438071056, -3.951233083390353062 ) ) ;
#40984 = CARTESIAN_POINT ( 'NONE',  ( 35.00000000000000000, -8.927548052240835474, 8.295159312811946961 ) ) ;
#40985 = CYLINDRICAL_SURFACE ( 'NONE', #56074, 2.899999999999994582 ) ;
#40986 = CARTESIAN_POINT ( 'NONE',  ( 36.00000000000000711, 10.93004082984027825, 6.564808257521646873 ) ) ;
#40987 = ADVANCED_FACE ( 'NONE', ( #30723 ), #36035, .T. ) ;
#40988 = ORIENTED_EDGE ( 'NONE', *, *, #21806, .F. ) ;
#40989 = DIRECTION ( 'NONE',  ( 0.000000000000000000, 0.01356324068817992522, -0.9999080150203990547 ) ) ;
#40990 = ORIENTED_EDGE ( 'NONE', *, *, #17864, .F. ) ;
#40991 = CARTESIAN_POINT ( 'NONE',  ( 3.092491956584988877, 0.4473002062003109680, 7.905533744258577578 ) ) ;
#40992 = CYLINDRICAL_SURFACE ( 'NONE', #12211, 5.000000000000000888 ) ;
#40993 = CARTESIAN_POINT ( 'NONE',  ( -18.39456087108311522, -4.498649229773558744, 12.72900479644374094 ) ) ;
#40994 = VERTEX_POINT ( 'NONE', #25104 ) ;
#40995 = CARTESIAN_POINT ( 'NONE',  ( 2.000000000000001776, 0.000000000000000000, 0.000000000000000000 ) ) ;
#40996 = VECTOR ( 'NONE', #45663, 1000.000000000000000 ) ;
#40997 = CARTESIAN_POINT ( 'NONE',  ( 36.00000000000000711, -10.02106554660714011, -7.882940143791743459 ) ) ;
#40998 = CARTESIAN_POINT ( 'NONE',  ( -36.00000000000000711, -11.59605747147783106, -5.300372733891766330 ) ) ;
#40999 = CARTESIAN_POINT ( 'NONE',  ( 37.00000000000000711, -11.05394794832825767, 5.130401251914841865 ) ) ;
#41000 = CARTESIAN_POINT ( 'NONE',  ( 2.000000000000001776, -1.018311147294094443, -6.861346417234492456 ) ) ;
#41001 = EDGE_LOOP ( 'NONE', ( #7583, #8897, #60983, #11680 ) ) ;
#41002 = CARTESIAN_POINT ( 'NONE',  ( -35.00000000000000000, 0.000000000000000000, 0.000000000000000000 ) ) ;
#41003 = CARTESIAN_POINT ( 'NONE',  ( 0.000000000000000000, 0.7281529553923131726, -7.464569195442812166 ) ) ;
#41004 = CARTESIAN_POINT ( 'NONE',  ( 0.8375941296809052972, -3.890418817177767163, -11.81283813871897692 ) ) ;
#41005 = ADVANCED_FACE ( 'NONE', ( #56008 ), #15514, .F. ) ;
#41006 = CARTESIAN_POINT ( 'NONE',  ( -35.00000000000000000, -4.074242145635921908, -12.08151691381194404 ) ) ;
#41007 = CARTESIAN_POINT ( 'NONE',  ( 17.94443053578330094, -10.27027613361345004, 8.791042504289096726 ) ) ;
#41008 = ORIENTED_EDGE ( 'NONE', *, *, #54595, .T. ) ;
#41009 = LINE ( 'NONE', #31034, #46093 ) ;
#41010 = CARTESIAN_POINT ( 'NONE',  ( -22.27718112499583469, 3.412978993569800057, 1.380338971069110521 ) ) ;
#41011 = CARTESIAN_POINT ( 'NONE',  ( -22.28169757117799321, 3.561623073126538586, -0.9841724999439870336 ) ) ;
#41012 = EDGE_LOOP ( 'NONE', ( #8021, #63519, #42922, #2622 ) ) ;
#41013 = FACE_OUTER_BOUND ( 'NONE', #60229, .T. ) ;
#41014 = CARTESIAN_POINT ( 'NONE',  ( 3.152665057735501097, 6.622010822086128456, -4.377619405893580229 ) ) ;
#41015 = ORIENTED_EDGE ( 'NONE', *, *, #44334, .T. ) ;
#41016 = ORIENTED_EDGE ( 'NONE', *, *, #701, .T. ) ;
#41017 = ORIENTED_EDGE ( 'NONE', *, *, #40135, .T. ) ;
#41018 = EDGE_CURVE ( 'NONE', #12415, #10704, #19505, .T. ) ;
#41019 = ORIENTED_EDGE ( 'NONE', *, *, #62711, .F. ) ;
#41020 = CARTESIAN_POINT ( 'NONE',  ( 37.00000000000000711, 11.13736569743274352, -4.946702696913214403 ) ) ;
#41021 = CARTESIAN_POINT ( 'NONE',  ( 35.00000000000000000, 3.614449339633649227, 11.17622378668002092 ) ) ;
#41022 = LINE ( 'NONE', #61304, #46071 ) ;
#41023 = DIRECTION ( 'NONE',  ( -1.000000000000000000, 0.000000000000000000, 0.000000000000000000 ) ) ;
#41024 = CARTESIAN_POINT ( 'NONE',  ( 0.2648978790185610999, -6.008231198269058382, 10.67083876753489946 ) ) ;
#41025 = CARTESIAN_POINT ( 'NONE',  ( -5.876491384319547429, -28.27454061773107696, 11.46433771796954382 ) ) ;
#41026 = DIRECTION ( 'NONE',  ( 0.000000000000000000, 0.01356324068817998940, -0.9999080150203990547 ) ) ;
#41028 = ORIENTED_EDGE ( 'NONE', *, *, #35035, .T. ) ;
#41027 = CARTESIAN_POINT ( 'NONE',  ( -37.00000000000000711, 0.000000000000000000, 0.000000000000000000 ) ) ;
#41029 = CARTESIAN_POINT ( 'NONE',  ( -35.00000000000000000, 7.379373053629018742, -10.39746860227882586 ) ) ;
#41030 = ORIENTED_EDGE ( 'NONE', *, *, #48792, .F. ) ;
#41031 = DIRECTION ( 'NONE',  ( 0.000000000000000000, 0.000000000000000000, 1.000000000000000000 ) ) ;
#41032 = EDGE_LOOP ( 'NONE', ( #15547, #7571, #8195, #19622 ) ) ;
#41033 = ORIENTED_EDGE ( 'NONE', *, *, #10570, .T. ) ;
#41034 = AXIS2_PLACEMENT_3D ( 'NONE', #59956, #44973, #34648 ) ;
#41035 = CARTESIAN_POINT ( 'NONE',  ( -22.28856623400852399, -0.9049353338066428165, 3.603818606161804716 ) ) ;
#41036 = CARTESIAN_POINT ( 'NONE',  ( 12.91449914267798960, -28.36597991684631026, 12.93464570467208752 ) ) ;
#41037 = DIRECTION ( 'NONE',  ( -0.000000000000000000, -1.000000000000000000, -0.000000000000000000 ) ) ;
#41038 = CARTESIAN_POINT ( 'NONE',  ( 2.994568964204212591, 7.825096839971888762, -0.9739368093813937088 ) ) ;
#41039 = CIRCLE ( 'NONE', #51703, 2.899999999999996803 ) ;
#41040 = CARTESIAN_POINT ( 'NONE',  ( 1.549075743844145370, -2.862200647101428075, 12.34675572956523304 ) ) ;
#41041 = DIRECTION ( 'NONE',  ( -1.000000000000000000, 0.000000000000000000, 0.000000000000000000 ) ) ;
#41042 = ORIENTED_EDGE ( 'NONE', *, *, #63405, .T. ) ;
#41043 = ADVANCED_FACE ( 'NONE', ( #19467 ), #35043, .T. ) ;
#41044 = ORIENTED_EDGE ( 'NONE', *, *, #29940, .F. ) ;
#41045 = EDGE_CURVE ( 'NONE', #65334, #50289, #22695, .T. ) ;
#41046 = LINE ( 'NONE', #46059, #57130 ) ;
#41047 = ORIENTED_EDGE ( 'NONE', *, *, #1449, .T. ) ;
#41048 = EDGE_CURVE ( 'NONE', #18977, #6781, #64062, .T. ) ;
#41049 = EDGE_LOOP ( 'NONE', ( #59213, #37332, #16578, #5988 ) ) ;
#41050 = CARTESIAN_POINT ( 'NONE',  ( 2.000000000000001776, 0.000000000000000000, 0.000000000000000000 ) ) ;
#41051 = CARTESIAN_POINT ( 'NONE',  ( 0.9232167919969163083, -10.58277433962385494, 6.587352952801118100 ) ) ;
#41052 = CARTESIAN_POINT ( 'NONE',  ( -22.29570301036918423, 0.8918611685731360206, -3.629130197778208888 ) ) ;
#41053 = CARTESIAN_POINT ( 'NONE',  ( 2.241352910868908310, 1.243507963608194045, -7.532448145350496560 ) ) ;
#41054 = CARTESIAN_POINT ( 'NONE',  ( 2.253265082352433613, 7.637296367516833939, 0.1282654837134977743 ) ) ;
#41055 = CARTESIAN_POINT ( 'NONE',  ( -7.184946476706033813, -1.341365231991552998, -11.92630736377528500 ) ) ;
#41056 = ADVANCED_FACE ( 'NONE', ( #45372 ), #20767, .T. ) ;
#41057 = CARTESIAN_POINT ( 'NONE',  ( 35.00000000000000000, 4.705694406421931860E-17, -3.469127814946512892E-15 ) ) ;
#41058 = ADVANCED_FACE ( 'NONE', ( #20108 ), #39673, .T. ) ;
#41059 = VERTEX_POINT ( 'NONE', #25760 ) ;
#41060 = CARTESIAN_POINT ( 'NONE',  ( 37.00000000000000711, -9.557269938331499404, 7.561043153948067364 ) ) ;
#41061 = LINE ( 'NONE', #65661, #9557 ) ;
#41062 = CARTESIAN_POINT ( 'NONE',  ( -35.00000000000000000, 0.000000000000000000, 0.000000000000000000 ) ) ;
#41063 = CARTESIAN_POINT ( 'NONE',  ( 6.802398627868447178, -6.309174925604525086, 10.20958905146123286 ) ) ;
#41064 = EDGE_CURVE ( 'NONE', #37494, #42367, #35710, .T. ) ;
#41065 = CYLINDRICAL_SURFACE ( 'NONE', #16073, 5.000000000000000888 ) ;
#41066 = B_SPLINE_CURVE_WITH_KNOTS ( 'NONE', 3,
 ( #44451, #18234, #38501, #54128, #53811, #2949 ),
 .UNSPECIFIED., .F., .F.,
 ( 4, 2, 4 ),
 ( 0.0001654224980408265460, 0.0006219428995476446002, 0.001078463301054462817 ),
 .UNSPECIFIED. ) ;
#41067 = CARTESIAN_POINT ( 'NONE',  ( 1.375507693220370919, 2.770709900327031239, -12.30831170622617243 ) ) ;
#41068 = CARTESIAN_POINT ( 'NONE',  ( 8.929416320216105873, 2.411192301257917059, -11.75776610390553323 ) ) ;
#41069 = EDGE_LOOP ( 'NONE', ( #40396, #61186, #6723, #40768 ) ) ;
#41070 = CARTESIAN_POINT ( 'NONE',  ( 0.2650492433740076481, 10.66007796911768857, 6.027445608088885187 ) ) ;
#41071 = CARTESIAN_POINT ( 'NONE',  ( 2.969415267405037806, 0.9841783286029369693, -7.815364626284241112 ) ) ;
#41072 = CARTESIAN_POINT ( 'NONE',  ( 145.1370849898475797, 3.309064568108273190E-14, 0.000000000000000000 ) ) ;
#41073 = AXIS2_PLACEMENT_3D ( 'NONE', #27798, #48100, #54059 ) ;
#41074 = CIRCLE ( 'NONE', #30446, 6.936499999999989896 ) ;
#41075 = CARTESIAN_POINT ( 'NONE',  ( -8.419536088387953754, -32.40770164631213390, -12.72556558505306157 ) ) ;
#41076 = CYLINDRICAL_SURFACE ( 'NONE', #42540, 4.999999999999999112 ) ;
#41077 = ORIENTED_EDGE ( 'NONE', *, *, #59094, .T. ) ;
#41078 = CARTESIAN_POINT ( 'NONE',  ( -18.07060594675151322, -4.850101347397025364, -12.59940754866924983 ) ) ;
#41079 = CARTESIAN_POINT ( 'NONE',  ( -27.66223155157100422, -11.89179406365635217, -6.414297969418397471 ) ) ;
#41080 = CARTESIAN_POINT ( 'NONE',  ( 19.27363075669222425, -28.98570064806743929, -5.846556568011616939 ) ) ;
#41081 = VERTEX_POINT ( 'NONE', #4507 ) ;
#41082 = FACE_OUTER_BOUND ( 'NONE', #1549, .T. ) ;
#41083 = FACE_OUTER_BOUND ( 'NONE', #16925, .T. ) ;
#41084 = FACE_OUTER_BOUND ( 'NONE', #54663, .T. ) ;
#41086 = ORIENTED_EDGE ( 'NONE', *, *, #19134, .T. ) ;
#41085 = DIRECTION ( 'NONE',  ( 0.000000000000000000, 0.01356324068817998940, -0.9999080150203989437 ) ) ;
#41087 = CARTESIAN_POINT ( 'NONE',  ( 35.00000000000000000, -6.265926637539568134, -11.10408318471057321 ) ) ;
#41088 = ADVANCED_FACE ( 'NONE', ( #35389 ), #55696, .T. ) ;
#41089 = CARTESIAN_POINT ( 'NONE',  ( 2.491965175174208014, -7.322278065136096359, -2.439431489055742475 ) ) ;
#41090 = EDGE_LOOP ( 'NONE', ( #2555, #43299, #16946, #11969 ) ) ;
#41091 = DIRECTION ( 'NONE',  ( -1.000000000000000000, -0.000000000000000000, 0.000000000000000000 ) ) ;
#41092 = CARTESIAN_POINT ( 'NONE',  ( -27.08704841010891684, 1.313007237775888125, 1.888108843317890528 ) ) ;
#41093 = CYLINDRICAL_SURFACE ( 'NONE', #7800, 12.74999999999999822 ) ;
#41094 = CARTESIAN_POINT ( 'NONE',  ( 1.719304012341272836, -1.452142814148833949, -12.64775761152634281 ) ) ;
#41095 = CARTESIAN_POINT ( 'NONE',  ( 0.3401186441510236635, -11.44115600261388188, -4.436257390736940920 ) ) ;
#41096 = DIRECTION ( 'NONE',  ( 0.9946347501772865307, 0.000000000000000000, -0.1034490876700550205 ) ) ;
#41097 = DIRECTION ( 'NONE',  ( 0.3939253465568944290, 0.8603393047164938912, 0.3234796780324392107 ) ) ;
#41098 = ORIENTED_EDGE ( 'NONE', *, *, #42829, .T. ) ;
#41099 = DIRECTION ( 'NONE',  ( 1.000000000000000000, 0.000000000000000000, -0.000000000000000000 ) ) ;
#41100 = ORIENTED_EDGE ( 'NONE', *, *, #62194, .F. ) ;
#41101 = DIRECTION ( 'NONE',  ( 0.000000000000000000, -0.9551603052523448545, 0.2960891610144612551 ) ) ;
#41102 = CARTESIAN_POINT ( 'NONE',  ( 0.3160775863651062445, 11.43919651388225667, 4.419114254409931775 ) ) ;
#41103 = ADVANCED_FACE ( 'NONE', ( #11125 ), #56694, .T. ) ;
#41104 = CARTESIAN_POINT ( 'NONE',  ( -14.47334165536100059, 0.000000000000000000, 0.000000000000000000 ) ) ;
#41105 = ORIENTED_EDGE ( 'NONE', *, *, #4315, .F. ) ;
#41106 = DIRECTION ( 'NONE',  ( -0.000000000000000000, -1.000000000000000000, -0.000000000000000000 ) ) ;
#41107 = CARTESIAN_POINT ( 'NONE',  ( 37.00000000000000711, -10.91536515067650903, -4.339012074899918581 ) ) ;
#41108 = ADVANCED_FACE ( 'NONE', ( #41697 ), #41358, .T. ) ;
#41109 = FACE_BOUND ( 'NONE', #32849, .T. ) ;
#41110 = EDGE_LOOP ( 'NONE', ( #60005, #29098, #9291, #33519 ) ) ;
#41111 = ORIENTED_EDGE ( 'NONE', *, *, #52632, .F. ) ;
#41112 = CARTESIAN_POINT ( 'NONE',  ( 26.08439714455133185, -12.97057518889163674, 3.743551691817328386 ) ) ;
#41113 = EDGE_CURVE ( 'NONE', #39990, #38220, #31399, .T. ) ;
#41114 = ORIENTED_EDGE ( 'NONE', *, *, #16654, .T. ) ;
#41115 = DIRECTION ( 'NONE',  ( -1.000000000000000000, 0.000000000000000000, 0.000000000000000000 ) ) ;
#41116 = AXIS2_PLACEMENT_3D ( 'NONE', #2967, #8581, #43491 ) ;
#41117 = DIRECTION ( 'NONE',  ( 0.000000000000000000, 0.7381862504171975425, -0.6745969609292638003 ) ) ;
#41118 = CARTESIAN_POINT ( 'NONE',  ( 0.3665391374699464300, -8.095513416941292562, 9.237363111276737371 ) ) ;
#41119 = CARTESIAN_POINT ( 'NONE',  ( -27.09602251845159415, 1.018053071731315429, -2.092130925171141076 ) ) ;
#41120 = CARTESIAN_POINT ( 'NONE',  ( 9.612882454814815958, 13.47023598955341583, -0.9106303824545893821 ) ) ;
#41121 = LINE ( 'NONE', #61404, #14704 ) ;
#41122 = CIRCLE ( 'NONE', #11413, 4.999999999999998224 ) ;
#41123 = EDGE_CURVE ( 'NONE', #31517, #36643, #51381, .T. ) ;
#41124 = CARTESIAN_POINT ( 'NONE',  ( 2.305787727787084407, 7.508843116234155346, 1.493241775258449255 ) ) ;
#41125 = ORIENTED_EDGE ( 'NONE', *, *, #1605, .T. ) ;
#41126 = CARTESIAN_POINT ( 'NONE',  ( -37.00000000000000711, -12.31350058095525846, 3.307597835713201651 ) ) ;
#41127 = EDGE_CURVE ( 'NONE', #3400, #23545, #47087, .T. ) ;
#41128 = CARTESIAN_POINT ( 'NONE',  ( -37.00000000000000711, -11.54110654723650420, 2.185196060783841432 ) ) ;
#41129 = CARTESIAN_POINT ( 'NONE',  ( 35.00000000000000000, 8.830544224263075392, 9.196955404009196755 ) ) ;
#41130 = DIRECTION ( 'NONE',  ( -1.000000000000000000, -0.000000000000000000, -0.000000000000000000 ) ) ;
#41131 = CARTESIAN_POINT ( 'NONE',  ( 0.000000000000000000, 0.000000000000000000, 0.000000000000000000 ) ) ;
#41132 = DIRECTION ( 'NONE',  ( -1.000000000000000000, 0.000000000000000000, 0.000000000000000000 ) ) ;
#41133 = DIRECTION ( 'NONE',  ( 0.000000000000000000, 0.5987040770935622147, -0.8009703041134207391 ) ) ;
#41134 = CARTESIAN_POINT ( 'NONE',  ( 0.2646305136544065406, 4.312539723326135110, 11.46223899740601304 ) ) ;
#41135 = EDGE_CURVE ( 'NONE', #14636, #59375, #62959, .T. ) ;
#41136 = ORIENTED_EDGE ( 'NONE', *, *, #58352, .F. ) ;
#41137 = CARTESIAN_POINT ( 'NONE',  ( -37.00000000000000711, -6.891188680298757419, -9.512294188640973758 ) ) ;
#41138 = EDGE_CURVE ( 'NONE', #12885, #64920, #59335, .T. ) ;
#41139 = VERTEX_POINT ( 'NONE', #42016 ) ;
#41140 = CARTESIAN_POINT ( 'NONE',  ( 0.2648978790185602672, 0.1321385342562404197, 12.24533305150758089 ) ) ;
#41141 = CARTESIAN_POINT ( 'NONE',  ( 41.00000000000000711, -1.694065894508600678E-18, 0.000000000000000000 ) ) ;
#41142 = EDGE_CURVE ( 'NONE', #47440, #57990, #17304, .T. ) ;
#41143 = CARTESIAN_POINT ( 'NONE',  ( 0.2653519789438765208, -12.05632450344284301, 2.148225749114954564 ) ) ;
#41144 = CARTESIAN_POINT ( 'NONE',  ( 2.247112776671284173, 2.501955819907980771, -7.214825360831188306 ) ) ;
#41145 = ORIENTED_EDGE ( 'NONE', *, *, #53370, .T. ) ;
#41146 = CARTESIAN_POINT ( 'NONE',  ( -35.04643116707788408, -0.004425962698862209721, 0.01135624435143547939 ) ) ;
#41147 = DIRECTION ( 'NONE',  ( 0.000000000000000000, 0.01356324068817999808, -0.9999080150203990547 ) ) ;
#41148 = CARTESIAN_POINT ( 'NONE',  ( 37.00000000000000711, 10.54834585426228877, 6.102719229070555862 ) ) ;
#41149 = CARTESIAN_POINT ( 'NONE',  ( -27.32337605527167312, -0.3676050637290663725, 2.988381643048326097 ) ) ;
#41150 = VECTOR ( 'NONE', #49094, 1000.000000000000000 ) ;
#41151 = CARTESIAN_POINT ( 'NONE',  ( 8.937200413559443390, 4.476360154859203355, -12.73625532737111143 ) ) ;
#41152 = DIRECTION ( 'NONE',  ( 0.000000000000000000, -0.6876994588534296460, 0.7259954919231248471 ) ) ;
#41153 = VECTOR ( 'NONE', #7620, 1000.000000000000000 ) ;
#41154 =( BOUNDED_SURFACE ( )  B_SPLINE_SURFACE ( 3, 1, ( 
 ( #39853, #59486 ),
 ( #34836, #49212 ),
 ( #35170, #9251 ),
 ( #54515, #55477 ) ),
 .UNSPECIFIED., .F., .F., .F. ) 
 B_SPLINE_SURFACE_WITH_KNOTS ( ( 4, 4 ),
 ( 2, 2 ),
 ( 0.000000000000000000, 1.000000000000000000 ),
 ( 0.000000000000000000, 1.000000000000000000 ),
 .UNSPECIFIED. ) 
 GEOMETRIC_REPRESENTATION_ITEM ( )  RATIONAL_B_SPLINE_SURFACE ( (
 ( 1.000000000000000000, 1.000000000000000000),
 ( 0.9942764183789327692, 0.8450855930916585379),
 ( 0.9942764183789327692, 0.8450855930916585379),
 ( 1.000000000000000000, 1.000000000000000000) ) ) 
 REPRESENTATION_ITEM ( '' )  SURFACE ( )  );
#41155 = ORIENTED_EDGE ( 'NONE', *, *, #29690, .F. ) ;
#41156 = CARTESIAN_POINT ( 'NONE',  ( -27.10512513516321320, -0.5469390009827510557, 2.289566223069553708 ) ) ;
#41157 = ORIENTED_EDGE ( 'NONE', *, *, #2299, .F. ) ;
#41158 = DIRECTION ( 'NONE',  ( 0.000000000000000000, 0.01356324068817998940, -0.9999080150203989437 ) ) ;
#41159 = DIRECTION ( 'NONE',  ( 1.000000000000000000, 0.000000000000000000, 0.000000000000000000 ) ) ;
#41160 = AXIS2_PLACEMENT_3D ( 'NONE', #21854, #22158, #16535 ) ;
#41161 = CARTESIAN_POINT ( 'NONE',  ( -35.00000000000000000, 0.000000000000000000, 0.000000000000000000 ) ) ;
#41162 = CARTESIAN_POINT ( 'NONE',  ( -8.766550606785775912, -2.870938393825745116, 11.65238521198515187 ) ) ;
#41163 = ADVANCED_FACE ( 'NONE', ( #52678 ), #7103, .T. ) ;
#41164 = EDGE_CURVE ( 'NONE', #19811, #15014, #12039, .T. ) ;
#41165 = VERTEX_POINT ( 'NONE', #27706 ) ;
#41166 = AXIS2_PLACEMENT_3D ( 'NONE', #14375, #60585, #44619 ) ;
#41167 = VERTEX_POINT ( 'NONE', #52986 ) ;
#41168 = CARTESIAN_POINT ( 'NONE',  ( 37.00000000000000711, -8.052525312709825300, 8.551552972817161091 ) ) ;
#41169 = ORIENTED_EDGE ( 'NONE', *, *, #52465, .T. ) ;
#41170 = CARTESIAN_POINT ( 'NONE',  ( 2.000000000000001776, 0.000000000000000000, 0.000000000000000000 ) ) ;
#41171 = DIRECTION ( 'NONE',  ( 0.000000000000000000, 0.01356324068817992175, -0.9999080150203990547 ) ) ;
#41172 = DIRECTION ( 'NONE',  ( -0.000000000000000000, -0.000000000000000000, -1.000000000000000000 ) ) ;
#41173 = CARTESIAN_POINT ( 'NONE',  ( -27.15511094194038222, 2.092607239484540749, -1.375165223101512346 ) ) ;
#41174 = CARTESIAN_POINT ( 'NONE',  ( 0.000000000000000000, -6.664893814313694875, -3.439359016433563898 ) ) ;
#41175 = CARTESIAN_POINT ( 'NONE',  ( -6.533703001908491181, -1.140004534245788737, 11.94583671674990555 ) ) ;
#41176 = ORIENTED_EDGE ( 'NONE', *, *, #17340, .F. ) ;
#41177 = EDGE_CURVE ( 'NONE', #23637, #20211, #49237, .T. ) ;
#41178 = CARTESIAN_POINT ( 'NONE',  ( 2.373367633546871414, -2.455525055524842237, -7.275198254387436059 ) ) ;
#41179 = ORIENTED_EDGE ( 'NONE', *, *, #60221, .T. ) ;
#41180 = B_SPLINE_CURVE_WITH_KNOTS ( 'NONE', 3,
 ( #53325, #7769, #43651, #23062, #8098, #8414, #22739, #28367, #33680, #58656, #28688, #18070, #33362, #49003 ),
 .UNSPECIFIED., .F., .F.,
 ( 4, 2, 2, 2, 2, 2, 4 ),
 ( 1.301042606982605321E-18, 0.002148955746805324314, 0.003223433620207984303, 0.004297911493610643424, 0.006446867240415959932, 0.007521345113818616451, 0.008595822987221272971 ),
 .UNSPECIFIED. ) ;
#41181 = CARTESIAN_POINT ( 'NONE',  ( -22.27711351828769892, 2.547249869018266999, 2.657880562424656201 ) ) ;
#41182 = CARTESIAN_POINT ( 'NONE',  ( 0.2638984909335716500, 9.508791614589302554, -7.718810690098965921 ) ) ;
#41183 = CARTESIAN_POINT ( 'NONE',  ( 18.06777465640019997, 8.467087186347326266, 10.54078692479376045 ) ) ;
#41184 = EDGE_CURVE ( 'NONE', #22716, #42272, #22844, .T. ) ;
#41185 = VERTEX_POINT ( 'NONE', #18745 ) ;
#41186 = CARTESIAN_POINT ( 'NONE',  ( -15.59741926310024773, -34.17135967094577609, 7.744809993482618005 ) ) ;
#41187 = VERTEX_POINT ( 'NONE', #49348 ) ;
#41188 = DIRECTION ( 'NONE',  ( -1.000000000000000000, -0.000000000000000000, -0.000000000000000000 ) ) ;
#41189 = CARTESIAN_POINT ( 'NONE',  ( 5.520433897694421610, -0.009283255140285096713, -0.01186170453199835231 ) ) ;
#41190 = CARTESIAN_POINT ( 'NONE',  ( 2.305787727787084407, 2.774453000917148415, 7.135468203929992370 ) ) ;
#41191 = CARTESIAN_POINT ( 'NONE',  ( -26.58307969160926021, -3.634951060761377750, -23.96081192854774500 ) ) ;
#41192 = VERTEX_POINT ( 'NONE', #13719 ) ;
#41193 = ORIENTED_EDGE ( 'NONE', *, *, #65168, .F. ) ;
#41194 = CYLINDRICAL_SURFACE ( 'NONE', #4544, 12.18650000000000055 ) ;
#41195 = B_SPLINE_CURVE_WITH_KNOTS ( 'NONE', 3,
 ( #20633, #62168, #31260, #56533, #55874, #25950, #61834, #5334, #16622, #41212, #41881, #56876, #36223, #21617, #55550, #10976 ),
 .UNSPECIFIED., .F., .F.,
 ( 4, 2, 2, 2, 2, 2, 2, 4 ),
 ( 2.163628596297127287E-17, 0.002218008919589290178, 0.003327013379383922907, 0.004436017839178555203, 0.005545022298973183161, 0.006654026758767811987, 0.007763031218562439946, 0.008872035678357067037 ),
 .UNSPECIFIED. ) ;
#41196 = EDGE_CURVE ( 'NONE', #37677, #56356, #63283, .T. ) ;
#41197 = ORIENTED_EDGE ( 'NONE', *, *, #21400, .F. ) ;
#41198 = CARTESIAN_POINT ( 'NONE',  ( -37.00000000000000711, -11.47561260193580956, 5.556331110570369880 ) ) ;
#41199 = ORIENTED_EDGE ( 'NONE', *, *, #31435, .T. ) ;
#41200 = ORIENTED_EDGE ( 'NONE', *, *, #962, .F. ) ;
#41201 = ORIENTED_EDGE ( 'NONE', *, *, #22422, .F. ) ;
#41202 = DIRECTION ( 'NONE',  ( 0.000000000000000000, -0.01356324068817998940, 0.9999080150203990547 ) ) ;
#41203 = CARTESIAN_POINT ( 'NONE',  ( -3.987543989681922696, -25.89241204356462589, 15.41372194231675330 ) ) ;
#41204 = FACE_OUTER_BOUND ( 'NONE', #5376, .T. ) ;
#41205 = CARTESIAN_POINT ( 'NONE',  ( 9.612870878434209843, 11.96650298090372289, -0.9106810471525464967 ) ) ;
#41206 = DIRECTION ( 'NONE',  ( 0.000000000000000000, 0.01356324068817992175, -0.9999080150203990547 ) ) ;
#41207 = EDGE_LOOP ( 'NONE', ( #51123, #13807, #51168, #13793 ) ) ;
#41208 = LINE ( 'NONE', #40227, #3612 ) ;
#41209 = AXIS2_PLACEMENT_3D ( 'NONE', #38633, #31983, #52633 ) ;
#41210 = ORIENTED_EDGE ( 'NONE', *, *, #34680, .F. ) ;
#41211 = DIRECTION ( 'NONE',  ( -1.000000000000000000, 0.000000000000000000, 0.000000000000000000 ) ) ;
#41212 = CARTESIAN_POINT ( 'NONE',  ( -3.491752571392269910, 11.78957267686408095, 6.587477860936952645 ) ) ;
#41213 = CONICAL_SURFACE ( 'NONE', #28452, 15.00000000000000000, 0.5235987755983000369 ) ;
#41214 = DIRECTION ( 'NONE',  ( -1.000000000000000000, 0.000000000000000000, 0.000000000000000000 ) ) ;
#41215 = CARTESIAN_POINT ( 'NONE',  ( 0.2647959493198551728, -7.983607158780263724, -9.285851961022039802 ) ) ;
#41216 = CARTESIAN_POINT ( 'NONE',  ( 28.45979645211560438, 10.25197200398427810, 6.251877464400086737 ) ) ;
#41217 = CARTESIAN_POINT ( 'NONE',  ( 2.507146904658097863, -7.719969556433177615, -0.2163149345877387331 ) ) ;
#41218 = AXIS2_PLACEMENT_3D ( 'NONE', #31644, #61265, #51955 ) ;
#41219 = EDGE_CURVE ( 'NONE', #31308, #45530, #14165, .T. ) ;
#41220 = ORIENTED_EDGE ( 'NONE', *, *, #37598, .T. ) ;
#41221 = DIRECTION ( 'NONE',  ( 0.000000000000000000, -0.9903235168508535136, -0.1387779952735919697 ) ) ;
#41222 = EDGE_CURVE ( 'NONE', #29123, #14422, #21946, .T. ) ;
#41223 = ORIENTED_EDGE ( 'NONE', *, *, #38160, .T. ) ;
#41224 = CARTESIAN_POINT ( 'NONE',  ( -24.38941346611472483, -9.755923631413494945, 9.333302870830756603 ) ) ;
#41225 = CARTESIAN_POINT ( 'NONE',  ( -9.737135312703241397, -26.73636926326595642, -14.00099174170044058 ) ) ;
#41226 = CARTESIAN_POINT ( 'NONE',  ( 14.99320290036091308, -28.92253633446381400, 11.50449902612425923 ) ) ;
#41227 = EDGE_CURVE ( 'NONE', #13636, #23085, #18435, .T. ) ;
#41228 = CARTESIAN_POINT ( 'NONE',  ( 35.00000000000000000, -8.389074212634222150, 8.839356091080130540 ) ) ;
#41229 = CARTESIAN_POINT ( 'NONE',  ( 35.00000000000000000, 11.66953048682399441, -3.511814412392164186 ) ) ;
#41230 = VERTEX_POINT ( 'NONE', #48671 ) ;
#41231 = FACE_OUTER_BOUND ( 'NONE', #1487, .T. ) ;
#41232 = CARTESIAN_POINT ( 'NONE',  ( 1.283627346226907884, 5.810034161408880848, -11.16434663959580398 ) ) ;
#41233 = CARTESIAN_POINT ( 'NONE',  ( 35.00000000000000000, 8.927548052240892318, -8.295159312811890118 ) ) ;
#41234 = CARTESIAN_POINT ( 'NONE',  ( 23.89564968379661281, -11.31614867562879034, -7.366089092235777791 ) ) ;
#41235 = AXIS2_PLACEMENT_3D ( 'NONE', #29844, #55125, #4930 ) ;
#41236 = CYLINDRICAL_SURFACE ( 'NONE', #15928, 6.595312090839647645 ) ;
#41237 = VECTOR ( 'NONE', #23649, 1000.000000000000000 ) ;
#41238 = CARTESIAN_POINT ( 'NONE',  ( -35.04660725145885891, -0.008590646501108684455, -0.008800808525128425361 ) ) ;
#41239 = CARTESIAN_POINT ( 'NONE',  ( 1.549075743846074271, -5.743768701986616598, -11.29795072957547575 ) ) ;
#41240 = CARTESIAN_POINT ( 'NONE',  ( -27.08416781016246588, 1.744495588874932279, -1.485424708116795722 ) ) ;
#41241 = CARTESIAN_POINT ( 'NONE',  ( 5.516018279890452902, -0.006707902355168857828, -0.0009545156522405044090 ) ) ;
#41242 = AXIS2_PLACEMENT_3D ( 'NONE', #18258, #28540, #33543 ) ;
#41243 = EDGE_CURVE ( 'NONE', #54635, #50600, #39319, .T. ) ;
#41244 = ORIENTED_EDGE ( 'NONE', *, *, #36690, .F. ) ;
#41245 = EDGE_CURVE ( 'NONE', #15906, #27211, #55582, .T. ) ;
#41246 = VECTOR ( 'NONE', #47882, 1000.000000000000000 ) ;
#41247 = CIRCLE ( 'NONE', #25310, 2.899999999999994582 ) ;
#41248 = ORIENTED_EDGE ( 'NONE', *, *, #27856, .F. ) ;
#41249 = CARTESIAN_POINT ( 'NONE',  ( 0.2648978790185593790, 1.996248716311628479, 12.08224454301449313 ) ) ;
#41250 = CARTESIAN_POINT ( 'NONE',  ( 49.00067463083239971, -0.2018647702349731232, 0.7653472444253841545 ) ) ;
#41251 = CARTESIAN_POINT ( 'NONE',  ( -35.00000000000000000, 0.000000000000000000, 0.000000000000000000 ) ) ;
#41252 = AXIS2_PLACEMENT_3D ( 'NONE', #28627, #22675, #43255 ) ;
#41253 = CARTESIAN_POINT ( 'NONE',  ( 0.3675815128205894289, -1.872154644482166397, 12.13672785388549613 ) ) ;
#41254 = VERTEX_POINT ( 'NONE', #63946 ) ;
#41255 = EDGE_CURVE ( 'NONE', #45626, #56247, #43894, .T. ) ;
#41256 = VERTEX_POINT ( 'NONE', #53977 ) ;
#41257 = AXIS2_PLACEMENT_3D ( 'NONE', #28881, #8930, #3952 ) ;
#41258 = EDGE_LOOP ( 'NONE', ( #65800, #38183, #31697, #37997 ) ) ;
#41259 = CARTESIAN_POINT ( 'NONE',  ( 2.639814597422739606, 7.763021810282392465, 0.2564041122425372854 ) ) ;
#41260 = DIRECTION ( 'NONE',  ( -1.000000000000000000, -0.000000000000000000, 0.000000000000000000 ) ) ;
#41261 = ORIENTED_EDGE ( 'NONE', *, *, #21400, .T. ) ;
#41262 = DIRECTION ( 'NONE',  ( 1.000000000000000000, 0.000000000000000000, 0.000000000000000000 ) ) ;
#41263 = CARTESIAN_POINT ( 'NONE',  ( 37.00000000000000711, 4.705694406421931860E-17, -3.469127814946512892E-15 ) ) ;
#41264 = ORIENTED_EDGE ( 'NONE', *, *, #24030, .T. ) ;
#41265 = DIRECTION ( 'NONE',  ( -1.000000000000000000, 0.000000000000000000, 0.000000000000000000 ) ) ;
#41266 = CARTESIAN_POINT ( 'NONE',  ( 13.85759530760289060, -30.12605952702162426, -5.992721990255803988 ) ) ;
#41267 = DIRECTION ( 'NONE',  ( -1.000000000000000000, 0.000000000000000000, 0.000000000000000000 ) ) ;
#41268 = ORIENTED_EDGE ( 'NONE', *, *, #17408, .T. ) ;
#41269 = CARTESIAN_POINT ( 'NONE',  ( 145.1370849898475797, 3.309064568108273190E-14, 0.000000000000000000 ) ) ;
#41270 = EDGE_CURVE ( 'NONE', #50979, #52347, #15217, .T. ) ;
#41271 = ORIENTED_EDGE ( 'NONE', *, *, #24901, .F. ) ;
#41272 = CARTESIAN_POINT ( 'NONE',  ( 1.459561108994217316, 7.633517148169352673, -10.08002506399590104 ) ) ;
#41273 = ORIENTED_EDGE ( 'NONE', *, *, #7929, .T. ) ;
#41274 = CARTESIAN_POINT ( 'NONE',  ( 37.25000000000000711, -45.00200000000000244, 4.499999999999997335 ) ) ;
#41275 = EDGE_CURVE ( 'NONE', #44872, #53953, #31180, .T. ) ;
#41276 = CARTESIAN_POINT ( 'NONE',  ( 2.889800649504073782, 1.129261637821610709, 6.016320774579811292 ) ) ;
#41277 = CARTESIAN_POINT ( 'NONE',  ( 2.000000000000001776, -6.812627895098285258, -0.04423456934733380197 ) ) ;
#41278 = DIRECTION ( 'NONE',  ( 0.000000000000000000, 0.01356324068817992175, -0.9999080150203990547 ) ) ;
#41280 = CARTESIAN_POINT ( 'NONE',  ( 2.000000000000001776, -3.155844197800145690, 6.177028383390419819 ) ) ;
#41279 = AXIS2_PLACEMENT_3D ( 'NONE', #57202, #41892, #21948 ) ;
#41281 = CARTESIAN_POINT ( 'NONE',  ( 0.000000000000000000, -7.248432822490255667, 1.926193556692974429 ) ) ;
#41282 = CARTESIAN_POINT ( 'NONE',  ( -27.09150307427447402, -0.1754204729056269008, -2.306459590995633135 ) ) ;
#41283 = CARTESIAN_POINT ( 'NONE',  ( 35.00000000000000000, 7.215058775251253387, -9.821084925794595577 ) ) ;
#41285 = VERTEX_POINT ( 'NONE', #29352 ) ;
#41284 = CARTESIAN_POINT ( 'NONE',  ( 5.329935900150571726, -10.23194172168328464, 8.808226182152964157 ) ) ;
#41286 = CARTESIAN_POINT ( 'NONE',  ( 37.00000000000000711, 8.052525312709883920, -8.551552972817113130 ) ) ;
#41287 = ORIENTED_EDGE ( 'NONE', *, *, #32541, .F. ) ;
#41288 = CIRCLE ( 'NONE', #957, 12.74999999999999822 ) ;
#41289 = CARTESIAN_POINT ( 'NONE',  ( 0.2911222467163508965, -4.392242282524938091, 11.44063169461054486 ) ) ;
#41290 = CARTESIAN_POINT ( 'NONE',  ( 35.00000000000000000, 12.01765980939841683, -2.021542716731445921 ) ) ;
#41291 = ORIENTED_EDGE ( 'NONE', *, *, #50736, .T. ) ;
#41292 = CARTESIAN_POINT ( 'NONE',  ( 0.2647959493198550618, 7.983607158780327673, 9.285851961021984735 ) ) ;
#41293 = CARTESIAN_POINT ( 'NONE',  ( -27.08429572838383947, -2.279961732801590646, 0.2296550094122822017 ) ) ;
#41294 = LINE ( 'NONE', #52292, #23829 ) ;
#41295 = CARTESIAN_POINT ( 'NONE',  ( 2.000000000000001776, -5.396716205731451943, 4.158041573745051345 ) ) ;
#41296 = VECTOR ( 'NONE', #63731, 1000.000000000000000 ) ;
#41297 = EDGE_CURVE ( 'NONE', #24621, #33199, #3582, .T. ) ;
#41298 = CARTESIAN_POINT ( 'NONE',  ( 29.03457606387295087, -7.862146963512102182, 10.97436308512422265 ) ) ;
#41299 = ORIENTED_EDGE ( 'NONE', *, *, #10363, .T. ) ;
#41300 = CYLINDRICAL_SURFACE ( 'NONE', #5680, 12.74999999999999822 ) ;
#41301 = ADVANCED_FACE ( 'NONE', ( #30341 ), #59959, .T. ) ;
#41302 = CIRCLE ( 'NONE', #52993, 4.999999999999999112 ) ;
#41303 = VERTEX_POINT ( 'NONE', #20353 ) ;
#41304 = CARTESIAN_POINT ( 'NONE',  ( 35.00000000000000000, 10.54834585426228877, 6.102719229070555862 ) ) ;
#41305 = DIRECTION ( 'NONE',  ( -1.000000000000000000, 0.000000000000000000, -0.000000000000000000 ) ) ;
#41306 = ADVANCED_FACE ( 'NONE', ( #421 ), #60263, .T. ) ;
#41307 = ORIENTED_EDGE ( 'NONE', *, *, #22336, .T. ) ;
#41308 = CIRCLE ( 'NONE', #65688, 12.75000000000000178 ) ;
#41309 = CARTESIAN_POINT ( 'NONE',  ( -27.08579483061179261, -0.9690219683526719585, 2.081508743190592092 ) ) ;
#41310 = FACE_OUTER_BOUND ( 'NONE', #54660, .T. ) ;
#41311 = CARTESIAN_POINT ( 'NONE',  ( 0.000000000000000000, -6.606214214351077807, 2.114938770769887455 ) ) ;
#41312 = DIRECTION ( 'NONE',  ( 1.000000000000000000, 0.000000000000000000, 0.000000000000000000 ) ) ;
#41313 = CARTESIAN_POINT ( 'NONE',  ( 9.384597055785796726, 7.262755914012919867, 11.38454852282039198 ) ) ;
#41314 = DIRECTION ( 'NONE',  ( 1.000000000000000000, 0.000000000000000000, 0.000000000000000000 ) ) ;
#41315 = CARTESIAN_POINT ( 'NONE',  ( 37.00000000000000711, 8.146229107149528303, 9.063649021438866527 ) ) ;
#41316 = CARTESIAN_POINT ( 'NONE',  ( -23.18047892478189098, -2.738168160732679990, 3.933989833240137290 ) ) ;
#41317 = AXIS2_PLACEMENT_3D ( 'NONE', #23813, #54722, #44378 ) ;
#41318 = ORIENTED_EDGE ( 'NONE', *, *, #39577, .F. ) ;
#41319 = CARTESIAN_POINT ( 'NONE',  ( 35.00000000000000000, -11.73808581813437613, 0.4353888892049613824 ) ) ;
#41320 = DIRECTION ( 'NONE',  ( 0.000000000000000000, -0.01356324068817998940, 0.9999080150203990547 ) ) ;
#41321 = ADVANCED_FACE ( 'NONE', ( #65560 ), #10365, .T. ) ;
#41322 = ORIENTED_EDGE ( 'NONE', *, *, #64471, .F. ) ;
#41323 = CONICAL_SURFACE ( 'NONE', #23317, 2.214855479030549468, 1.249045772030607848 ) ;
#41324 = CARTESIAN_POINT ( 'NONE',  ( 0.3675815128205894289, 10.50067073900651771, 6.367184624550202621 ) ) ;
#41325 = CARTESIAN_POINT ( 'NONE',  ( 2.000000000000001776, 4.604744433234757572, -5.919993978425451608 ) ) ;
#41326 = DIRECTION ( 'NONE',  ( 0.000000000000000000, -0.3218879778915842427, 0.9467777615094616905 ) ) ;
#41327 = ORIENTED_EDGE ( 'NONE', *, *, #33046, .F. ) ;
#41328 = DIRECTION ( 'NONE',  ( 0.000000000000000000, 0.000000000000000000, 1.000000000000000000 ) ) ;
#41329 = DIRECTION ( 'NONE',  ( -1.000000000000000000, 0.000000000000000000, 0.000000000000000000 ) ) ;
#41330 = ORIENTED_EDGE ( 'NONE', *, *, #30145, .T. ) ;
#41331 = CYLINDRICAL_SURFACE ( 'NONE', #37023, 5.000000000000000888 ) ;
#41332 = ORIENTED_EDGE ( 'NONE', *, *, #53491, .F. ) ;
#41333 = ORIENTED_EDGE ( 'NONE', *, *, #48663, .T. ) ;
#41334 = CIRCLE ( 'NONE', #43426, 5.000000000000001776 ) ;
#41335 = CARTESIAN_POINT ( 'NONE',  ( -27.35552965826136429, -1.320216934008378473, -2.810569013793753346 ) ) ;
#41336 = ADVANCED_FACE ( 'NONE', ( #40635 ), #54654, .T. ) ;
#41337 = ORIENTED_EDGE ( 'NONE', *, *, #64696, .F. ) ;
#41338 = CARTESIAN_POINT ( 'NONE',  ( 2.406456491626836502, 9.333533259762544887, 4.662370073862575737 ) ) ;
#41339 = CARTESIAN_POINT ( 'NONE',  ( -22.27710395300133328, -3.562137928983395874, 0.9291085174899338384 ) ) ;
#41340 = LINE ( 'NONE', #11733, #48224 ) ;
#41341 = CARTESIAN_POINT ( 'NONE',  ( 1.000000000000000888, 0.08317740279931498670, 7.499538753794337431 ) ) ;
#41342 = ORIENTED_EDGE ( 'NONE', *, *, #42483, .T. ) ;
#41343 =( BOUNDED_SURFACE ( )  B_SPLINE_SURFACE ( 3, 1, ( 
 ( #45013, #55655 ),
 ( #39694, #10090 ),
 ( #54979, #50666 ),
 ( #9407, #29696 ) ),
 .UNSPECIFIED., .F., .F., .F. ) 
 B_SPLINE_SURFACE_WITH_KNOTS ( ( 4, 4 ),
 ( 2, 2 ),
 ( 0.000000000000000000, 1.000000000000000000 ),
 ( 0.000000000000000000, 1.000000000000000000 ),
 .UNSPECIFIED. ) 
 GEOMETRIC_REPRESENTATION_ITEM ( )  RATIONAL_B_SPLINE_SURFACE ( (
 ( 1.000000000000000000, 1.000000000000000000),
 ( 0.8716676215708681896, 0.8964445200148167814),
 ( 0.8716676215708681896, 0.8964445200148167814),
 ( 1.000000000000000000, 1.000000000000000000) ) ) 
 REPRESENTATION_ITEM ( '' )  SURFACE ( )  );
#41344 = CARTESIAN_POINT ( 'NONE',  ( 5.514970785353741078, -0.003805873180274802012, -0.002796696073589725016 ) ) ;
#41345 = CARTESIAN_POINT ( 'NONE',  ( -4.228765754682470401, -25.91303510919334485, 15.38236557491807766 ) ) ;
#41346 = DIRECTION ( 'NONE',  ( 1.000000000000000000, -0.000000000000000000, 0.000000000000000000 ) ) ;
#41348 = ORIENTED_EDGE ( 'NONE', *, *, #60490, .T. ) ;
#41347 = CARTESIAN_POINT ( 'NONE',  ( 0.2653519789438754661, -12.06397564829376101, -2.104833950422703825 ) ) ;
#41349 = CARTESIAN_POINT ( 'NONE',  ( 2.241537034860907163, -2.615577641485573146, 7.172440248506149807 ) ) ;
#41350 = ADVANCED_FACE ( 'NONE', ( #60929 ), #34340, .T. ) ;
#41351 = ORIENTED_EDGE ( 'NONE', *, *, #41113, .T. ) ;
#41352 = CARTESIAN_POINT ( 'NONE',  ( -35.00000000000000000, 8.927548052241016663, -8.295159312811756891 ) ) ;
#41353 = ORIENTED_EDGE ( 'NONE', *, *, #38040, .T. ) ;
#41354 = ORIENTED_EDGE ( 'NONE', *, *, #49689, .F. ) ;
#41355 = DIRECTION ( 'NONE',  ( -1.000000000000000000, -0.000000000000000000, -0.000000000000000000 ) ) ;
#41356 = CARTESIAN_POINT ( 'NONE',  ( 17.05023968204111284, -34.49999999999999289, 4.356789313881303194 ) ) ;
#41357 = EDGE_CURVE ( 'NONE', #23545, #21056, #40714, .T. ) ;
#41358 = CYLINDRICAL_SURFACE ( 'NONE', #54545, 12.18649999999999878 ) ;
#41359 = ORIENTED_EDGE ( 'NONE', *, *, #8194, .T. ) ;
#41360 = CARTESIAN_POINT ( 'NONE',  ( 2.305787727787085295, 7.566723232958088019, -1.164987321564654676 ) ) ;
#41361 = CARTESIAN_POINT ( 'NONE',  ( -20.73885153823040639, 11.61492743593955801, -3.067692064997443957 ) ) ;
#41362 = CARTESIAN_POINT ( 'NONE',  ( 2.000000000000001776, -6.935703035393428806, -0.1051458740708305362 ) ) ;
#41363 = ORIENTED_EDGE ( 'NONE', *, *, #21347, .F. ) ;
#41364 = ORIENTED_EDGE ( 'NONE', *, *, #209, .F. ) ;
#41365 = LINE ( 'NONE', #9461, #56070 ) ;
#41366 = EDGE_LOOP ( 'NONE', ( #49921, #61448, #1500, #3485 ) ) ;
#41367 = VERTEX_POINT ( 'NONE', #55935 ) ;
#41368 = CARTESIAN_POINT ( 'NONE',  ( 5.536195898058073439, 0.006344799443923436130, 0.005656495196970911903 ) ) ;
#41369 = DIRECTION ( 'NONE',  ( 0.000000000000000000, -0.01356324068817998940, 0.9999080150203990547 ) ) ;
#41370 = CARTESIAN_POINT ( 'NONE',  ( -25.00000000000000355, -28.99999999999999645, 1.530808498934191521E-15 ) ) ;
#41371 = DIRECTION ( 'NONE',  ( 0.000000000000000000, -0.01356324068817998940, 0.9999080150203990547 ) ) ;
#41372 = CYLINDRICAL_SURFACE ( 'NONE', #9315, 2.899999999999994582 ) ;
#41373 = EDGE_CURVE ( 'NONE', #34813, #39295, #4088, .T. ) ;
#41374 = CARTESIAN_POINT ( 'NONE',  ( -8.891032880924177206, 25.00000000000000000, -3.860857758255646921 ) ) ;
#41375 = VECTOR ( 'NONE', #25534, 1000.000000000000000 ) ;
#41376 = AXIS2_PLACEMENT_3D ( 'NONE', #1253, #36131, #51141 ) ;
#41377 = CARTESIAN_POINT ( 'NONE',  ( -22.27709082389155171, -0.8996430462092220859, -3.569727173833839640 ) ) ;
#41378 = AXIS2_PLACEMENT_3D ( 'NONE', #62394, #13422, #19416 ) ;
#41379 = ORIENTED_EDGE ( 'NONE', *, *, #39929, .F. ) ;
#41380 = CARTESIAN_POINT ( 'NONE',  ( -37.00000000000000711, 0.000000000000000000, 0.000000000000000000 ) ) ;
#41381 = VECTOR ( 'NONE', #36609, 1000.000000000000000 ) ;
#41382 = EDGE_CURVE ( 'NONE', #9789, #30228, #4722, .T. ) ;
#41383 = CARTESIAN_POINT ( 'NONE',  ( 6.147033604836291687, -8.616929040695943343, 8.360196263819061002 ) ) ;
#41384 = DIRECTION ( 'NONE',  ( 0.000000000000000000, 0.8989688749565172277, 0.4380125133593943398 ) ) ;
#41385 = AXIS2_PLACEMENT_3D ( 'NONE', #39543, #65139, #28922 ) ;
#41386 = CARTESIAN_POINT ( 'NONE',  ( -35.00000000000000000, 10.99909370905157324, 5.246972444134057056 ) ) ;
#41387 = CARTESIAN_POINT ( 'NONE',  ( 0.8375941296815080372, 2.537217542322766750, -12.17542732751335777 ) ) ;
#41388 = FACE_OUTER_BOUND ( 'NONE', #63217, .T. ) ;
#41389 = ORIENTED_EDGE ( 'NONE', *, *, #49, .T. ) ;
#41390 = CARTESIAN_POINT ( 'NONE',  ( -27.20164183316782314, 2.339520810540427043, 1.232966507052623895 ) ) ;
#41391 = DIRECTION ( 'NONE',  ( 0.000000000000000000, 0.01356324068817298112, -0.9999080150203990547 ) ) ;
#41392 = CARTESIAN_POINT ( 'NONE',  ( 9.537768711910022290, -32.77116127932499268, 12.15562491790719513 ) ) ;
#41393 = CIRCLE ( 'NONE', #40313, 1.500000000000000444 ) ;
#41394 = CARTESIAN_POINT ( 'NONE',  ( -28.85619398320021745, 3.750539801530000439, 12.96855624952675612 ) ) ;
#41395 = DIRECTION ( 'NONE',  ( -1.000000000000000000, 0.000000000000000000, 0.000000000000000000 ) ) ;
#41396 = EDGE_CURVE ( 'NONE', #58893, #8992, #39978, .T. ) ;
#41397 = ORIENTED_EDGE ( 'NONE', *, *, #55416, .T. ) ;
#41398 = CARTESIAN_POINT ( 'NONE',  ( -25.00000000000000355, -9.999999999999998224, -24.00000000000000000 ) ) ;
#41399 = CARTESIAN_POINT ( 'NONE',  ( -35.00000000000000000, 0.000000000000000000, 0.000000000000000000 ) ) ;
#41400 = CARTESIAN_POINT ( 'NONE',  ( 13.20768530587737288, -34.09315906254132500, -9.434917751661075158 ) ) ;
#41401 = ORIENTED_EDGE ( 'NONE', *, *, #30529, .F. ) ;
#41402 = EDGE_CURVE ( 'NONE', #23822, #14988, #18004, .T. ) ;
#41403 = DIRECTION ( 'NONE',  ( 0.000000000000000000, 0.7621620551276332423, 0.6473862847818313560 ) ) ;
#41404 = DIRECTION ( 'NONE',  ( -1.000000000000000000, 0.000000000000000000, 0.000000000000000000 ) ) ;
#41405 = FACE_OUTER_BOUND ( 'NONE', #30696, .T. ) ;
#41407 = EDGE_LOOP ( 'NONE', ( #46414, #12819, #39121, #12174 ) ) ;
#41406 = DIRECTION ( 'NONE',  ( 0.000000000000000000, 0.01356324068817998940, -0.9999080150203990547 ) ) ;
#41408 = LINE ( 'NONE', #55750, #34155 ) ;
#41409 = AXIS2_PLACEMENT_3D ( 'NONE', #61034, #45726, #4534 ) ;
#41410 = EDGE_CURVE ( 'NONE', #60081, #64143, #55621, .T. ) ;
#41411 = DIRECTION ( 'NONE',  ( 0.000000000000000000, -0.01356324068817991828, 0.9999080150203990547 ) ) ;
#41412 = ORIENTED_EDGE ( 'NONE', *, *, #45939, .F. ) ;
#41413 = LINE ( 'NONE', #42382, #23784 ) ;
#41414 = CARTESIAN_POINT ( 'NONE',  ( 5.514970785353741078, 0.004233694591582517000, -0.002093325033904037177 ) ) ;
#41415 = CARTESIAN_POINT ( 'NONE',  ( 0.2648978790185584908, -7.972372351883092456, 9.295532325666423290 ) ) ;
#41416 = DIRECTION ( 'NONE',  ( -1.000000000000000000, 0.000000000000000000, 0.000000000000000000 ) ) ;
#41417 = DIRECTION ( 'NONE',  ( 0.000000000000000000, 0.6745969609292609137, 0.7381862504172000961 ) ) ;
#41418 = CARTESIAN_POINT ( 'NONE',  ( 2.241506898688418126, 2.574154135948788280, -7.187425579579779011 ) ) ;
#41420 = ORIENTED_EDGE ( 'NONE', *, *, #14337, .T. ) ;
#41419 = CARTESIAN_POINT ( 'NONE',  ( 1.014383007554947591, 0.4441500209063078408, 12.48801387563330145 ) ) ;
#41421 = ADVANCED_FACE ( 'NONE', ( #30982 ), #53507, .T. ) ;
#41422 = ORIENTED_EDGE ( 'NONE', *, *, #65610, .T. ) ;
#41423 = CARTESIAN_POINT ( 'NONE',  ( 35.00000000000000000, -10.80478261802177897, 5.636262487437428526 ) ) ;
#41424 = ORIENTED_EDGE ( 'NONE', *, *, #14604, .T. ) ;
#41425 = CYLINDRICAL_SURFACE ( 'NONE', #24145, 5.000000000000000888 ) ;
#41426 = AXIS2_PLACEMENT_3D ( 'NONE', #29483, #65386, #54464 ) ;
#41427 = CARTESIAN_POINT ( 'NONE',  ( -17.97314397134535469, 4.332534348537287805, 11.19277487034911012 ) ) ;
#41428 = B_SPLINE_CURVE_WITH_KNOTS ( 'NONE', 3,
 ( #22403, #8431, #14391, #53675, #4100, #44014, #29365, #39672, #43336, #19405, #38698, #18086, #44320, #48368, #64286, #39010 ),
 .UNSPECIFIED., .F., .F.,
 ( 4, 3, 3, 3, 3, 4 ),
 ( 5.421010862427522170E-19, 0.0003017745587525240002, 0.0006035491769808742826, 0.0009053241094668172239, 0.001207275924540914154, 0.001510325902534833623 ),
 .UNSPECIFIED. ) ;
#41429 = CARTESIAN_POINT ( 'NONE',  ( 35.00000000000000000, -2.936739658819788712, 11.37311665002366290 ) ) ;
#41431 = VERTEX_POINT ( 'NONE', #61559 ) ;
#41430 = AXIS2_PLACEMENT_3D ( 'NONE', #13221, #23197, #43457 ) ;
#41432 = CARTESIAN_POINT ( 'NONE',  ( 35.00000000000000000, -10.39746860227895731, -7.379373053628834889 ) ) ;
#41433 = CARTESIAN_POINT ( 'NONE',  ( -24.62662350575228487, -9.678819843908897269, 7.096674636486683063 ) ) ;
#41434 = CARTESIAN_POINT ( 'NONE',  ( -22.27721688985630522, -1.293557211780054006, 3.446999288411557227 ) ) ;
#41435 = ORIENTED_EDGE ( 'NONE', *, *, #50095, .T. ) ;
#41436 = ORIENTED_EDGE ( 'NONE', *, *, #13501, .T. ) ;
#41437 = CARTESIAN_POINT ( 'NONE',  ( 27.76677820897042182, -12.45056549256346479, 5.221417433310395317 ) ) ;
#41438 = ORIENTED_EDGE ( 'NONE', *, *, #61923, .F. ) ;
#41439 = CIRCLE ( 'NONE', #64789, 12.74999999999999822 ) ;
#41440 = CARTESIAN_POINT ( 'NONE',  ( 23.20859878307385316, -9.989936526681711726, -6.655393916305755830 ) ) ;
#41441 = CARTESIAN_POINT ( 'NONE',  ( -27.08935880048753120, 0.5666837974575801296, -2.235999130317600336 ) ) ;
#41442 = CARTESIAN_POINT ( 'NONE',  ( 1.000000000000000888, 1.693411908627200146, 7.306323022404582979 ) ) ;
#41443 = CARTESIAN_POINT ( 'NONE',  ( -27.08506889328327816, 0.9597901767732768263, -2.083363953276920366 ) ) ;
#41444 = CARTESIAN_POINT ( 'NONE',  ( -35.05175862995318425, -0.008949502803497905168, -0.008837625261055859216 ) ) ;
#41445 = CARTESIAN_POINT ( 'NONE',  ( 26.25871678826176847, -11.49115831596997062, 3.460539353551115305 ) ) ;
#41446 = DIRECTION ( 'NONE',  ( 1.000000000000000000, 0.000000000000000000, -0.000000000000000000 ) ) ;
#41447 = CIRCLE ( 'NONE', #38277, 12.74999999999999822 ) ;
#41448 = ORIENTED_EDGE ( 'NONE', *, *, #2492, .T. ) ;
#41449 = DIRECTION ( 'NONE',  ( -1.000000000000000000, 0.000000000000000000, 0.000000000000000000 ) ) ;
#41450 = AXIS2_PLACEMENT_3D ( 'NONE', #2185, #41416, #62055 ) ;
#41451 = DIRECTION ( 'NONE',  ( 1.000000000000000000, 0.000000000000000000, -0.000000000000000000 ) ) ;
#41452 = DIRECTION ( 'NONE',  ( 1.000000000000000000, -0.000000000000000000, -0.000000000000000000 ) ) ;
#41453 = CARTESIAN_POINT ( 'NONE',  ( -7.962338368258669696, 7.023910026709175192, -9.755115923264007449 ) ) ;
#41454 = CARTESIAN_POINT ( 'NONE',  ( -37.00000000000000711, -0.7214809346827719683, -11.72397916322013245 ) ) ;
#41455 = FACE_OUTER_BOUND ( 'NONE', #17510, .T. ) ;
#41456 = ORIENTED_EDGE ( 'NONE', *, *, #41882, .F. ) ;
#41457 = EDGE_CURVE ( 'NONE', #33917, #48302, #12569, .T. ) ;
#41458 = AXIS2_PLACEMENT_3D ( 'NONE', #40089, #8870, #34461 ) ;
#41459 = COLOUR_RGB ( '', 0.66274510, 0.83137255, 0.94901961) ;
#41460 = ORIENTED_EDGE ( 'NONE', *, *, #23344, .T. ) ;
#41461 = VECTOR ( 'NONE', #37746, 1000.000000000000000 ) ;
#41462 = LINE ( 'NONE', #278, #19517 ) ;
#41463 = EDGE_LOOP ( 'NONE', ( #12230, #65481, #21779, #54870 ) ) ;
#41464 = CARTESIAN_POINT ( 'NONE',  ( 5.516018279890452902, -0.003580555109620835435, 0.005752102158674384652 ) ) ;
#41465 = CARTESIAN_POINT ( 'NONE',  ( 3.152665057736256493, -0.9030954876717440793, 7.886634106564762270 ) ) ;
#41466 = CARTESIAN_POINT ( 'NONE',  ( 1.372161826076670588, -10.03232826862084082, -7.648244077827061282 ) ) ;
#41467 = DIRECTION ( 'NONE',  ( -1.000000000000000000, -1.836970198721029688E-16, -0.000000000000000000 ) ) ;
#41468 = ORIENTED_EDGE ( 'NONE', *, *, #59595, .T. ) ;
#41469 = CARTESIAN_POINT ( 'NONE',  ( 5.516018279890452902, 0.0009545156522404378389, -0.006707902355168868236 ) ) ;
#41470 = FACE_OUTER_BOUND ( 'NONE', #3346, .T. ) ;
#41471 = DIRECTION ( 'NONE',  ( 0.000000000000000000, -0.2006870767258961963, 0.9796553971857727694 ) ) ;
#41472 = CARTESIAN_POINT ( 'NONE',  ( 2.000000000000001776, 3.224464355699941720, -6.771471746881976728 ) ) ;
#41473 = CIRCLE ( 'NONE', #43570, 5.000000000000001776 ) ;
#41474 = ADVANCED_FACE ( 'NONE', ( #32850 ), #63132, .T. ) ;
#41475 = CIRCLE ( 'NONE', #30844, 12.18650000000000055 ) ;
#41476 = CARTESIAN_POINT ( 'NONE',  ( 0.2648978790185584908, 6.237101853238694815, -10.53870023327857197 ) ) ;
#41477 = DIRECTION ( 'NONE',  ( 0.000000000000000000, -0.01356324068817999114, 0.9999080150203989437 ) ) ;
#41478 = ORIENTED_EDGE ( 'NONE', *, *, #53310, .F. ) ;
#41479 = EDGE_CURVE ( 'NONE', #37563, #10290, #54602, .T. ) ;
#41480 = CARTESIAN_POINT ( 'NONE',  ( 47.00000000000000711, 4.705694406421931860E-17, -3.469127814946512892E-15 ) ) ;
#41481 = ORIENTED_EDGE ( 'NONE', *, *, #15589, .T. ) ;
#41482 = EDGE_CURVE ( 'NONE', #2029, #39221, #64115, .T. ) ;
#41483 = CARTESIAN_POINT ( 'NONE',  ( -35.04660725145885891, -0.01123650152077631907, -0.004999447127077803754 ) ) ;
#41484 = CARTESIAN_POINT ( 'NONE',  ( 2.241449424704146764, 7.194804211893846002, 2.553400830064003646 ) ) ;
#41485 = CARTESIAN_POINT ( 'NONE',  ( 5.514970785353741078, -0.003929719953530087274, -0.002619824551223206600 ) ) ;
#41486 = CIRCLE ( 'NONE', #3327, 6.936499999999989008 ) ;
#41487 = CARTESIAN_POINT ( 'NONE',  ( 26.83852350919729801, -11.22119259825004711, 4.265317526618762400 ) ) ;
#41488 = CARTESIAN_POINT ( 'NONE',  ( -9.068975030232913070, -3.147254398582626678, 11.58080990864780979 ) ) ;
#41489 = EDGE_LOOP ( 'NONE', ( #7133, #2953, #60712, #33418 ) ) ;
#41491 = ORIENTED_EDGE ( 'NONE', *, *, #43907, .F. ) ;
#41490 = EDGE_CURVE ( 'NONE', #49219, #47265, #16007, .T. ) ;
#41492 = CARTESIAN_POINT ( 'NONE',  ( 0.2655924914740778187, 7.905499957109361375, -9.352877839710522778 ) ) ;
#41493 = ORIENTED_EDGE ( 'NONE', *, *, #39535, .T. ) ;
#41494 = AXIS2_PLACEMENT_3D ( 'NONE', #44547, #64507, #23978 ) ;
#41495 = CARTESIAN_POINT ( 'NONE',  ( -27.08423923533013422, -2.274768056034772279, 0.2759775751761906482 ) ) ;
#41496 = FACE_OUTER_BOUND ( 'NONE', #19835, .T. ) ;
#41497 = CARTESIAN_POINT ( 'NONE',  ( 2.080613030138687147, 0.000000000000000000, 0.000000000000000000 ) ) ;
#41498 = CARTESIAN_POINT ( 'NONE',  ( 37.00000000000000711, -4.237620530777882699, -11.42599468261428086 ) ) ;
#41499 = CARTESIAN_POINT ( 'NONE',  ( -35.00000000000000000, -11.98254675519229906, 2.220215194441857331 ) ) ;
#41500 = EDGE_CURVE ( 'NONE', #48647, #39184, #52165, .T. ) ;
#41501 = CARTESIAN_POINT ( 'NONE',  ( 35.00000000000000000, -3.340853584269612764, -11.26103545359855040 ) ) ;
#41502 = CARTESIAN_POINT ( 'NONE',  ( 0.000000000000000000, 0.000000000000000000, 0.000000000000000000 ) ) ;
#41503 = EDGE_LOOP ( 'NONE', ( #50875, #12456, #39727, #7288 ) ) ;
#41504 = AXIS2_PLACEMENT_3D ( 'NONE', #5882, #26140, #31757 ) ;
#41505 = CARTESIAN_POINT ( 'NONE',  ( 2.770579946183338471, -2.384572752174033639, -7.437949029067715934 ) ) ;
#41506 = ORIENTED_EDGE ( 'NONE', *, *, #46094, .T. ) ;
#41507 = CARTESIAN_POINT ( 'NONE',  ( 21.75117853020661585, -12.54259235896871694, -4.997187019246493556 ) ) ;
#41509 = DIRECTION ( 'NONE',  ( 0.000000000000000000, -0.6478160128812003871, 0.7617968321374831708 ) ) ;
#41508 = AXIS2_PLACEMENT_3D ( 'NONE', #13123, #29706, #48709 ) ;
#41510 = AXIS2_PLACEMENT_3D ( 'NONE', #28839, #18219, #13224 ) ;
#41511 = ORIENTED_EDGE ( 'NONE', *, *, #49286, .F. ) ;
#41512 = EDGE_CURVE ( 'NONE', #15981, #14636, #7884, .T. ) ;
#41513 = DIRECTION ( 'NONE',  ( 0.000000000000000000, -0.7790879021242440583, 0.6269146997508067143 ) ) ;
#41514 = CARTESIAN_POINT ( 'NONE',  ( -19.30028543097103011, -30.00000000000000355, 5.909123879098597598 ) ) ;
#41515 = VERTEX_POINT ( 'NONE', #17596 ) ;
#41516 = DIRECTION ( 'NONE',  ( 0.2227494284590502138, 0.000000000000000000, 0.9748757316300199482 ) ) ;
#41517 = CARTESIAN_POINT ( 'NONE',  ( -17.92531974009792606, -29.71422580122515456, -8.391737566681648275 ) ) ;
#41518 = AXIS2_PLACEMENT_3D ( 'NONE', #23399, #48026, #24063 ) ;
#41519 = DIRECTION ( 'NONE',  ( 1.000000000000000000, 0.000000000000000000, 0.000000000000000000 ) ) ;
#41520 = ORIENTED_EDGE ( 'NONE', *, *, #53241, .F. ) ;
#41522 = ADVANCED_FACE ( 'NONE', ( #48510 ), #32522, .F. ) ;
#41521 = VERTEX_POINT ( 'NONE', #42495 ) ;
#41523 = DIRECTION ( 'NONE',  ( 0.000000000000000000, -0.01356324068817991828, 0.9999080150203990547 ) ) ;
#41524 = ORIENTED_EDGE ( 'NONE', *, *, #37502, .T. ) ;
#41525 = CARTESIAN_POINT ( 'NONE',  ( -35.00000000000000000, 0.01609748574461371262, -11.74614673114903951 ) ) ;
#41526 = EDGE_LOOP ( 'NONE', ( #18194, #26643, #370, #6788 ) ) ;
#41527 = ORIENTED_EDGE ( 'NONE', *, *, #62145, .T. ) ;
#41528 = ORIENTED_EDGE ( 'NONE', *, *, #29081, .F. ) ;
#41529 = CIRCLE ( 'NONE', #106, 2.899999999999994582 ) ;
#41530 = CARTESIAN_POINT ( 'NONE',  ( 37.00000000000000711, -4.237174932027311769, -12.02534193257719686 ) ) ;
#41531 = CARTESIAN_POINT ( 'NONE',  ( 0.4626703367442792092, 11.46957824750455046, 4.475905684073717694 ) ) ;
#41532 = AXIS2_PLACEMENT_3D ( 'NONE', #44273, #64541, #19016 ) ;
#41533 = DIRECTION ( 'NONE',  ( 0.000000000000000000, -0.9467777615094604693, -0.3218879778915876289 ) ) ;
#41534 = CARTESIAN_POINT ( 'NONE',  ( 2.258463476536644254, 2.740340677911331291, -7.131741622455316509 ) ) ;
#41535 = PLANE ( 'NONE',  #62465 ) ;
#41536 = ORIENTED_EDGE ( 'NONE', *, *, #39630, .T. ) ;
#41537 = CIRCLE ( 'NONE', #29854, 6.936499999999989008 ) ;
#41538 = CARTESIAN_POINT ( 'NONE',  ( 35.00000000000000000, 4.018060380616396365, -11.50504120060944757 ) ) ;
#41539 =( BOUNDED_CURVE ( )  B_SPLINE_CURVE ( 3, ( #16031, #15394, #15699, #35977 ),
 .UNSPECIFIED., .F., .F. ) 
 B_SPLINE_CURVE_WITH_KNOTS ( ( 4, 4 ),
 ( 4.755771627453653672, 4.791948434006704005 ),
 .UNSPECIFIED. ) 
 CURVE ( )  GEOMETRIC_REPRESENTATION_ITEM ( )  RATIONAL_B_SPLINE_CURVE ( ( 1.000000000000000000, 0.9998909395293115177, 0.9998909395293115177, 1.000000000000000000 ) ) 
 REPRESENTATION_ITEM ( '' )  );
#41540 = ORIENTED_EDGE ( 'NONE', *, *, #26702, .F. ) ;
#41541 = DIRECTION ( 'NONE',  ( -1.000000000000000000, 0.000000000000000000, 0.000000000000000000 ) ) ;
#41542 = CARTESIAN_POINT ( 'NONE',  ( -27.10307689719060065, 0.6678239540327367552, 2.250862122746719152 ) ) ;
#41543 = VECTOR ( 'NONE', #23287, 1000.000000000000000 ) ;
#41544 = FACE_OUTER_BOUND ( 'NONE', #49998, .T. ) ;
#41545 = CARTESIAN_POINT ( 'NONE',  ( 0.3537226245948356662, -2.388187631842599412, 12.04110684114372276 ) ) ;
#41546 = CARTESIAN_POINT ( 'NONE',  ( -27.08429572838383947, -0.2296550094122856711, -2.279961732801603080 ) ) ;
#41547 = AXIS2_PLACEMENT_3D ( 'NONE', #26828, #47129, #18523 ) ;
#41548 = CARTESIAN_POINT ( 'NONE',  ( 2.000000000000001776, 3.859771122243047081, 5.613913289150030295 ) ) ;
#41549 = EDGE_CURVE ( 'NONE', #25350, #4916, #29094, .T. ) ;
#41550 = ORIENTED_EDGE ( 'NONE', *, *, #44115, .F. ) ;
#41551 = CARTESIAN_POINT ( 'NONE',  ( 35.00000000000000000, 4.705694406421931860E-17, -3.469127814946512892E-15 ) ) ;
#41552 = CIRCLE ( 'NONE', #12886, 4.999999999999999112 ) ;
#41553 = ORIENTED_EDGE ( 'NONE', *, *, #22585, .T. ) ;
#41554 = CARTESIAN_POINT ( 'NONE',  ( 2.177405672432020545, 4.457418613955601572, 10.27382588316165624 ) ) ;
#41555 = CARTESIAN_POINT ( 'NONE',  ( 3.474069148988125466, -25.85800187936593986, -15.46552914816620827 ) ) ;
#41556 = CARTESIAN_POINT ( 'NONE',  ( 18.81741048081455503, -29.91393404465042849, 6.911695701493934862 ) ) ;
#41557 = VECTOR ( 'NONE', #4076, 1000.000000000000114 ) ;
#41559 = VECTOR ( 'NONE', #43295, 1000.000000000000000 ) ;
#41558 = CARTESIAN_POINT ( 'NONE',  ( -27.10113028276028402, -0.6639289823109559840, -2.245923868550880886 ) ) ;
#41560 = CARTESIAN_POINT ( 'NONE',  ( -35.05175862995318425, -0.01216930940958933782, -0.003178856583451253326 ) ) ;
#41561 = ORIENTED_EDGE ( 'NONE', *, *, #6307, .T. ) ;
#41562 = EDGE_CURVE ( 'NONE', #48679, #46698, #3633, .T. ) ;
#41563 = DIRECTION ( 'NONE',  ( -1.000000000000000000, 0.000000000000000000, 0.000000000000000000 ) ) ;
#41564 = CARTESIAN_POINT ( 'NONE',  ( 0.2648321136542706178, 2.265911310221971231, -12.03456865502703188 ) ) ;
#41565 = CARTESIAN_POINT ( 'NONE',  ( 21.47693580707085559, 11.78067291942578443, -2.319680692362900754 ) ) ;
#41566 = DIRECTION ( 'NONE',  ( 1.000000000000000000, 0.000000000000000000, 0.000000000000000000 ) ) ;
#41567 = AXIS2_PLACEMENT_3D ( 'NONE', #9941, #4647, #39538 ) ;
#41568 = VECTOR ( 'NONE', #57359, 1000.000000000000000 ) ;
#41569 = CIRCLE ( 'NONE', #26718, 7.499999999999988454 ) ;
#41570 = EDGE_CURVE ( 'NONE', #19519, #64188, #438, .T. ) ;
#41571 = DIRECTION ( 'NONE',  ( -0.000000000000000000, -1.000000000000000000, -0.000000000000000000 ) ) ;
#41572 = CARTESIAN_POINT ( 'NONE',  ( -22.27384469013076185, 0.3730095848193410446, 3.663183248998782116 ) ) ;
#41573 = ADVANCED_FACE ( 'NONE', ( #27892 ), #58154, .T. ) ;
#41574 = DIRECTION ( 'NONE',  ( 0.000000000000000000, 0.01356324068817992175, -0.9999080150203990547 ) ) ;
#41575 = B_SPLINE_CURVE_WITH_KNOTS ( 'NONE', 3,
 ( #52263, #43232, #57577, #62866, #21981, #52595, #62213, #11996, #27290, #47276, #42234, #52894, #1717 ),
 .UNSPECIFIED., .F., .F.,
 ( 4, 3, 3, 3, 4 ),
 ( 3.878959614448865017E-18, 6.607593386745471407E-05, 0.0001321518677373519459, 0.0001982171734706200195, 0.0002642860854759489881 ),
 .UNSPECIFIED. ) ;
#41576 = CARTESIAN_POINT ( 'NONE',  ( 36.00000000000000711, 10.84030624090615724, 6.711949091238026632 ) ) ;
#41577 = CARTESIAN_POINT ( 'NONE',  ( 5.530133899448235191, -0.01149180883054537645, -0.01111090067015099367 ) ) ;
#41578 = AXIS2_PLACEMENT_3D ( 'NONE', #35779, #25840, #42087 ) ;
#41579 = AXIS2_PLACEMENT_3D ( 'NONE', #21564, #11888, #47486 ) ;
#41580 = EDGE_LOOP ( 'NONE', ( #8403, #59332, #27075, #53379 ) ) ;
#41581 = VECTOR ( 'NONE', #45093, 1000.000000000000000 ) ;
#41582 = ORIENTED_EDGE ( 'NONE', *, *, #62290, .T. ) ;
#41583 = CARTESIAN_POINT ( 'NONE',  ( 2.556980015514067173, -6.584367695372273843, 4.067895092073629648 ) ) ;
#41584 = CARTESIAN_POINT ( 'NONE',  ( 40.83349710434615076, -1.696348104764147768, 18.10529304745326584 ) ) ;
#41585 = LINE ( 'NONE', #31295, #6699 ) ;
#41586 = ADVANCED_FACE ( 'NONE', ( #49497 ), #3285, .T. ) ;
#41587 = VECTOR ( 'NONE', #21415, 1000.000000000000000 ) ;
#41588 = CARTESIAN_POINT ( 'NONE',  ( 0.3610902822527252143, -1.873269382026075291, 12.13436647668549995 ) ) ;
#41589 = EDGE_LOOP ( 'NONE', ( #41536, #19262, #31010, #8798 ) ) ;
#41590 = EDGE_CURVE ( 'NONE', #3801, #58474, #38683, .T. ) ;
#41591 = AXIS2_PLACEMENT_3D ( 'NONE', #3213, #23481, #59380 ) ;
#41592 = ORIENTED_EDGE ( 'NONE', *, *, #19539, .T. ) ;
#41593 = EDGE_LOOP ( 'NONE', ( #21820, #20966, #47733, #65137 ) ) ;
#41594 = CARTESIAN_POINT ( 'NONE',  ( 2.000000000000001776, 1.058508696395052517, -6.730038252034905355 ) ) ;
#41595 = EDGE_CURVE ( 'NONE', #58998, #29569, #31225, .T. ) ;
#41596 = CARTESIAN_POINT ( 'NONE',  ( 2.000000000000001776, -6.662861565602071323, 1.421313227905616650 ) ) ;
#41597 = ORIENTED_EDGE ( 'NONE', *, *, #22409, .F. ) ;
#41598 = EDGE_CURVE ( 'NONE', #62046, #53449, #23560, .T. ) ;
#41599 = CARTESIAN_POINT ( 'NONE',  ( 37.25000000000000711, -27.56270118634207122, 0.7455576661145019157 ) ) ;
#41600 = EDGE_CURVE ( 'NONE', #416, #29168, #8912, .T. ) ;
#41601 = CIRCLE ( 'NONE', #55420, 5.000000000000000000 ) ;
#41602 = FACE_OUTER_BOUND ( 'NONE', #12829, .T. ) ;
#41603 = EDGE_LOOP ( 'NONE', ( #48099, #50936, #36397, #5258 ) ) ;
#41604 = CARTESIAN_POINT ( 'NONE',  ( 2.280717697724240267, 4.794838658390990105, -5.957695241725613933 ) ) ;
#41605 = CARTESIAN_POINT ( 'NONE',  ( 12.84304429912246981, -30.00680404000052448, -7.859709520792301340 ) ) ;
#41606 = CARTESIAN_POINT ( 'NONE',  ( 2.241311220309654129, 7.141707286456011161, 2.698144003945220692 ) ) ;
#41607 = ORIENTED_EDGE ( 'NONE', *, *, #22497, .F. ) ;
#41608 = EDGE_CURVE ( 'NONE', #42144, #23300, #59784, .T. ) ;
#41609 = CARTESIAN_POINT ( 'NONE',  ( 2.241352910868910531, 5.901537464758454199, 4.843133558968147234 ) ) ;
#41610 = ORIENTED_EDGE ( 'NONE', *, *, #6068, .F. ) ;
#41611 = CARTESIAN_POINT ( 'NONE',  ( 2.889800649504073782, -5.774917447012985150, -2.030191121417194378 ) ) ;
#41612 = DIRECTION ( 'NONE',  ( 1.000000000000000000, -0.000000000000000000, -0.000000000000000000 ) ) ;
#41613 = CARTESIAN_POINT ( 'NONE',  ( -9.179144435730854923, -32.64956785249903959, 12.36195000407851907 ) ) ;
#41614 = DIRECTION ( 'NONE',  ( 1.000000000000000000, 0.000000000000000000, 0.000000000000000000 ) ) ;
#41615 = AXIS2_PLACEMENT_3D ( 'NONE', #3639, #13879, #39162 ) ;
#41617 = AXIS2_PLACEMENT_3D ( 'NONE', #48394, #2842, #63317 ) ;
#41616 = CARTESIAN_POINT ( 'NONE',  ( 2.241536586108913376, -6.608496983003814940, 3.822683724643440417 ) ) ;
#41618 = CARTESIAN_POINT ( 'NONE',  ( 37.00000000000000711, 4.705694406421931860E-17, -3.469127814946512892E-15 ) ) ;
#41619 = CARTESIAN_POINT ( 'NONE',  ( -30.09739282105660862, -2.991438519309432387, -13.18809029152657608 ) ) ;
#41620 = CARTESIAN_POINT ( 'NONE',  ( 8.538029044866334516, 5.442243673389044467, -10.69694707505074760 ) ) ;
#41622 = VERTEX_POINT ( 'NONE', #44158 ) ;
#41621 = CARTESIAN_POINT ( 'NONE',  ( -18.58686583997247155, 5.151216734910867068, -12.47858029384659417 ) ) ;
#41623 = CARTESIAN_POINT ( 'NONE',  ( 2.000000000000001776, -6.883677378339461583, 0.8544109087185534079 ) ) ;
#41624 = VERTEX_POINT ( 'NONE', #59143 ) ;
#41625 = CARTESIAN_POINT ( 'NONE',  ( 2.000000000000001776, 1.865193240757184290, -6.552473556515182374 ) ) ;
#41626 = CYLINDRICAL_SURFACE ( 'NONE', #36213, 12.75000000000000178 ) ;
#41627 = ORIENTED_EDGE ( 'NONE', *, *, #25875, .T. ) ;
#41628 = CARTESIAN_POINT ( 'NONE',  ( 1.459561108993356005, -12.62847742794678929, 0.6317018236574121204 ) ) ;
#41629 = CARTESIAN_POINT ( 'NONE',  ( 1.020182472824462394, 11.88926988382094230, -3.852445298735137857 ) ) ;
#41630 = CARTESIAN_POINT ( 'NONE',  ( -47.00000000000000711, 0.000000000000000000, 0.000000000000000000 ) ) ;
#41632 = AXIS2_PLACEMENT_3D ( 'NONE', #14055, #24362, #34345 ) ;
#41631 = LINE ( 'NONE', #33214, #47594 ) ;
#41633 = DIRECTION ( 'NONE',  ( 1.000000000000000000, 0.000000000000000000, 0.000000000000000000 ) ) ;
#41634 = EDGE_CURVE ( 'NONE', #36481, #48679, #12084, .T. ) ;
#41635 = ORIENTED_EDGE ( 'NONE', *, *, #36721, .T. ) ;
#41636 = CARTESIAN_POINT ( 'NONE',  ( -17.13740638563841756, -7.345997652321633709, -9.495308414869118252 ) ) ;
#41637 = AXIS2_PLACEMENT_3D ( 'NONE', #61346, #22101, #37392 ) ;
#41638 = ORIENTED_EDGE ( 'NONE', *, *, #26045, .T. ) ;
#41639 = CYLINDRICAL_SURFACE ( 'NONE', #32772, 5.000000000000000888 ) ;
#41640 = CIRCLE ( 'NONE', #1319, 6.936499999999989896 ) ;
#41641 = DIRECTION ( 'NONE',  ( -1.000000000000000000, 0.000000000000000000, 0.000000000000000000 ) ) ;
#41642 = DIRECTION ( 'NONE',  ( -1.000000000000000000, 0.000000000000000000, -0.000000000000000000 ) ) ;
#41643 = ORIENTED_EDGE ( 'NONE', *, *, #4053, .T. ) ;
#41644 = ADVANCED_FACE ( 'NONE', ( #33839 ), #8577, .T. ) ;
#41645 = B_SPLINE_CURVE_WITH_KNOTS ( 'NONE', 3,
 ( #52110, #51136, #61744, #46785, #26498, #1586, #52454, #6891, #31173, #46457, #10883, #6566, #21859, #20540, #51481, #11217 ),
 .UNSPECIFIED., .F., .F.,
 ( 4, 3, 3, 3, 3, 4 ),
 ( 0.000000000000000000, 0.0003017745587525255181, 0.0006035491769808753668, 0.0009053241094668198260, 0.001207275924539022221, 0.001510325902531028074 ),
 .UNSPECIFIED. ) ;
#41646 = CARTESIAN_POINT ( 'NONE',  ( -27.09150307427400861, -1.001311209615671549, 2.085162835056704189 ) ) ;
#41647 = CARTESIAN_POINT ( 'NONE',  ( 27.37598419994968069, 12.63452493104432506, 4.764905059084485472 ) ) ;
#41648 = CYLINDRICAL_SURFACE ( 'NONE', #25629, 12.74999999999999822 ) ;
#41649 = CARTESIAN_POINT ( 'NONE',  ( 2.000000000000001776, 2.480520636974191895, 6.345145617221231049 ) ) ;
#41650 = DIRECTION ( 'NONE',  ( 0.3939253465568943180, -0.7103112711423530401, 0.5833358547425019358 ) ) ;
#41651 = EDGE_CURVE ( 'NONE', #23831, #6864, #45032, .T. ) ;
#41652 = DIRECTION ( 'NONE',  ( 0.000000000000000000, -0.9551603052523510717, 0.2960891610144412156 ) ) ;
#41653 = DIRECTION ( 'NONE',  ( 0.000000000000000000, 0.000000000000000000, -1.000000000000000000 ) ) ;
#41654 = CARTESIAN_POINT ( 'NONE',  ( -35.00000000000000000, 10.70999494708501132, -5.814360711498173018 ) ) ;
#41655 = AXIS2_PLACEMENT_3D ( 'NONE', #17976, #41923, #53571 ) ;
#41656 = ADVANCED_FACE ( 'NONE', ( #43486 ), #30848, .F. ) ;
#41657 = VECTOR ( 'NONE', #2066, 1000.000000000000000 ) ;
#41658 = CIRCLE ( 'NONE', #18342, 5.000000000000001776 ) ;
#41659 = ORIENTED_EDGE ( 'NONE', *, *, #42803, .T. ) ;
#41660 = FACE_OUTER_BOUND ( 'NONE', #25733, .T. ) ;
#41661 = CARTESIAN_POINT ( 'NONE',  ( 0.3106921474978480147, -12.25904950202577481, -0.2354703039889393112 ) ) ;
#41662 = ORIENTED_EDGE ( 'NONE', *, *, #60447, .F. ) ;
#41663 = CARTESIAN_POINT ( 'NONE',  ( 2.889800649504073782, -2.156828754871430665, -5.728825117897728525 ) ) ;
#41664 = CARTESIAN_POINT ( 'NONE',  ( 0.3675815128205912052, 8.093875121226199454, -9.235491948679927177 ) ) ;
#41665 = CARTESIAN_POINT ( 'NONE',  ( -9.734731986197230569, 12.56932029542845974, -4.929511566481978413 ) ) ;
#41666 = ORIENTED_EDGE ( 'NONE', *, *, #33870, .T. ) ;
#41667 = B_SPLINE_CURVE_WITH_KNOTS ( 'NONE', 3,
 ( #65048, #49775, #24489, #19525, #57061, #30461, #6195, #863, #1202, #25154, #557, #60733, #31760, #50757, #15167, #62047, #45423, #40431, #5886 ),
 .UNSPECIFIED., .F., .F.,
 ( 4, 3, 3, 3, 3, 3, 4 ),
 ( 0.000000000000000000, 2.832085443540566458E-05, 4.217789847394524017E-05, 5.603488375045718604E-05, 6.989180858578818178E-05, 9.821094829918303128E-05, 0.0001178165571465086142 ),
 .UNSPECIFIED. ) ;
#41668 = CARTESIAN_POINT ( 'NONE',  ( -17.50255050041978677, 2.687144849813047909, 11.69642965478562324 ) ) ;
#41669 = CARTESIAN_POINT ( 'NONE',  ( -22.70624764888619751, -3.282666355490664767, 4.097886656202270217 ) ) ;
#41670 = ORIENTED_EDGE ( 'NONE', *, *, #52571, .T. ) ;
#41671 = LINE ( 'NONE', #7393, #6242 ) ;
#41672 = EDGE_LOOP ( 'NONE', ( #19059, #25260, #43711, #51599 ) ) ;
#41673 = VERTEX_POINT ( 'NONE', #3632 ) ;
#41674 = COLOUR_RGB ( '', 0.40784314, 0.44705882, 0.49803922) ;
#41675 = EDGE_CURVE ( 'NONE', #65264, #40614, #13873, .T. ) ;
#41676 = DIRECTION ( 'NONE',  ( 1.000000000000000000, 0.000000000000000000, 0.000000000000000000 ) ) ;
#41677 = ORIENTED_EDGE ( 'NONE', *, *, #58148, .F. ) ;
#41678 = ADVANCED_FACE ( 'NONE', ( #54479 ), #8911, .T. ) ;
#41679 = CARTESIAN_POINT ( 'NONE',  ( -25.95039640524091951, -10.26692734564517195, 6.213570374660478457 ) ) ;
#41680 = DIRECTION ( 'NONE',  ( -1.000000000000000000, 0.000000000000000000, 0.000000000000000000 ) ) ;
#41681 = DIRECTION ( 'NONE',  ( -1.000000000000000000, 0.000000000000000000, 0.000000000000000000 ) ) ;
#41682 = DIRECTION ( 'NONE',  ( 0.000000000000000000, 0.000000000000000000, 1.000000000000000000 ) ) ;
#41683 = EDGE_LOOP ( 'NONE', ( #3324, #27289, #42972, #12794, #24325, #14594 ) ) ;
#41684 = AXIS2_PLACEMENT_3D ( 'NONE', #21979, #26312, #32275 ) ;
#41685 = CARTESIAN_POINT ( 'NONE',  ( 0.2651627682582908263, -6.046625184671059472, 10.64925413290591827 ) ) ;
#41686 = CARTESIAN_POINT ( 'NONE',  ( -1.046707184715866212, -25.73493584727765082, 15.64955084339668012 ) ) ;
#41687 = DIRECTION ( 'NONE',  ( -1.000000000000000000, 0.000000000000000000, 0.000000000000000000 ) ) ;
#41689 = ORIENTED_EDGE ( 'NONE', *, *, #62921, .T. ) ;
#41688 = DIRECTION ( 'NONE',  ( 1.000000000000000000, 0.000000000000000000, 0.000000000000000000 ) ) ;
#41690 = EDGE_CURVE ( 'NONE', #54252, #59964, #54841, .T. ) ;
#41691 = CARTESIAN_POINT ( 'NONE',  ( -28.12644806133159392, 10.04153257883247363, -6.577776757711345290 ) ) ;
#41692 = ORIENTED_EDGE ( 'NONE', *, *, #6714, .T. ) ;
#41693 = CARTESIAN_POINT ( 'NONE',  ( 2.827825597296800275, 4.031992772939004155, 8.073505504738395899 ) ) ;
#41694 = VERTEX_POINT ( 'NONE', #59835 ) ;
#41695 = CYLINDRICAL_SURFACE ( 'NONE', #2950, 7.499999999999988454 ) ;
#41696 = DIRECTION ( 'NONE',  ( -1.000000000000000000, 0.000000000000000000, 0.000000000000000000 ) ) ;
#41697 = FACE_OUTER_BOUND ( 'NONE', #63320, .T. ) ;
#41698 = ORIENTED_EDGE ( 'NONE', *, *, #1759, .F. ) ;
#41699 = CARTESIAN_POINT ( 'NONE',  ( 0.5547464869798242049, 8.164898018378810463, 9.256151063740572837 ) ) ;
#41700 = ADVANCED_FACE ( 'NONE', ( #46181 ), #301, .T. ) ;
#41701 = FACE_OUTER_BOUND ( 'NONE', #24746, .T. ) ;
#41702 = CARTESIAN_POINT ( 'NONE',  ( 0.3341166715381320151, -12.03629799686216373, 2.378838837789055471 ) ) ;
#41703 = ORIENTED_EDGE ( 'NONE', *, *, #38696, .T. ) ;
#41704 = CIRCLE ( 'NONE', #30025, 5.000000000000000888 ) ;
#41705 = ORIENTED_EDGE ( 'NONE', *, *, #13511, .F. ) ;
#41706 = CARTESIAN_POINT ( 'NONE',  ( 2.440552418640494547, 7.547055375260062426, 1.531218882877318999 ) ) ;
#41707 = ORIENTED_EDGE ( 'NONE', *, *, #41064, .T. ) ;
#41708 = EDGE_LOOP ( 'NONE', ( #10453, #58174, #51392, #10954 ) ) ;
#41710 = VECTOR ( 'NONE', #41260, 1000.000000000000000 ) ;
#41709 = LINE ( 'NONE', #62311, #25351 ) ;
#41711 = CARTESIAN_POINT ( 'NONE',  ( -25.00000000000000355, -30.00000000000000000, 5.000000000000000888 ) ) ;
#41712 = CARTESIAN_POINT ( 'NONE',  ( 2.241509619876138171, -7.160887714159601458, -2.647089031563641726 ) ) ;
#41713 = CARTESIAN_POINT ( 'NONE',  ( -47.00000000000000711, 0.000000000000000000, 0.000000000000000000 ) ) ;
#41714 = DIRECTION ( 'NONE',  ( 0.000000000000000000, 0.2355298848897516562, 0.9718671068226458765 ) ) ;
#41715 = CARTESIAN_POINT ( 'NONE',  ( -9.862567555648398709, -3.268643206080108499, -11.54748364193017451 ) ) ;
#41716 = AXIS2_PLACEMENT_3D ( 'NONE', #25645, #1037, #14994 ) ;
#41717 = DIRECTION ( 'NONE',  ( 1.000000000000000000, 0.000000000000000000, 0.000000000000000000 ) ) ;
#41718 = EDGE_CURVE ( 'NONE', #28421, #13640, #4591, .T. ) ;
#41719 = ORIENTED_EDGE ( 'NONE', *, *, #40086, .F. ) ;
#41720 = DIRECTION ( 'NONE',  ( 1.000000000000000000, -0.000000000000000000, -0.000000000000000000 ) ) ;
#41721 = CARTESIAN_POINT ( 'NONE',  ( -3.384821952288626257, -5.980207314672072449, 10.44102928066339331 ) ) ;
#41722 = AXIS2_PLACEMENT_3D ( 'NONE', #2149, #32064, #22777 ) ;
#41723 = EDGE_CURVE ( 'NONE', #1524, #54137, #34395, .T. ) ;
#41724 = VECTOR ( 'NONE', #22964, 1000.000000000000114 ) ;
#41725 = CARTESIAN_POINT ( 'NONE',  ( 0.3675815128205894289, 4.447030445008336663, -11.44679196252404729 ) ) ;
#41726 = DIRECTION ( 'NONE',  ( -1.000000000000000000, 0.000000000000000000, -0.000000000000000000 ) ) ;
#41727 = CARTESIAN_POINT ( 'NONE',  ( 5.516018279890452902, 0.006440244342253413461, -0.002104829434641034870 ) ) ;
#41728 = CARTESIAN_POINT ( 'NONE',  ( 0.5572780756289984483, 2.443667122521743451, -12.09922454589811025 ) ) ;
#41729 = CARTESIAN_POINT ( 'NONE',  ( -22.27834755396594346, 2.305389312780943278, 2.876353066242370637 ) ) ;
#41730 = EDGE_CURVE ( 'NONE', #939, #659, #15267, .T. ) ;
#41732 = EDGE_LOOP ( 'NONE', ( #23304, #33609, #17016, #23505, #39483, #30893 ) ) ;
#41731 = EDGE_CURVE ( 'NONE', #61002, #34346, #27524, .T. ) ;
#41733 = CARTESIAN_POINT ( 'NONE',  ( -19.02967556479664069, -11.99999999999998934, 9.262893081595934602E-16 ) ) ;
#41734 = DIRECTION ( 'NONE',  ( 0.000000000000000000, -0.01356324068817999114, 0.9999080150203989437 ) ) ;
#41735 = DIRECTION ( 'NONE',  ( -1.000000000000000000, 0.000000000000000000, 0.000000000000000000 ) ) ;
#41736 = CARTESIAN_POINT ( 'NONE',  ( 0.000000000000000000, 6.767909380267608022, -0.7805499053121014441 ) ) ;
#41737 = ADVANCED_FACE ( 'NONE', ( #60807 ), #19910, .T. ) ;
#41738 = AXIS2_PLACEMENT_3D ( 'NONE', #25035, #45306, #40302 ) ;
#41739 = CARTESIAN_POINT ( 'NONE',  ( 35.00000000000000000, 4.705694406421931860E-17, -3.469127814946512892E-15 ) ) ;
#41740 = CARTESIAN_POINT ( 'NONE',  ( 1.937114397841935398, -7.182898292393691264, -10.63710405811941229 ) ) ;
#41741 =( BOUNDED_SURFACE ( )  B_SPLINE_SURFACE ( 3, 1, ( 
 ( #39470, #8898 ),
 ( #18229, #9206 ),
 ( #34486, #8561 ),
 ( #43469, #38831 ) ),
 .UNSPECIFIED., .F., .F., .F. ) 
 B_SPLINE_SURFACE_WITH_KNOTS ( ( 4, 4 ),
 ( 2, 2 ),
 ( 0.000000000000000000, 1.000000000000000000 ),
 ( 0.000000000000000000, 1.000000000000000000 ),
 .UNSPECIFIED. ) 
 GEOMETRIC_REPRESENTATION_ITEM ( )  RATIONAL_B_SPLINE_SURFACE ( (
 ( 1.000000000000000000, 1.000000000000000000),
 ( 0.9942764183789327692, 0.8450855930916580938),
 ( 0.9942764183789327692, 0.8450855930916580938),
 ( 1.000000000000000000, 1.000000000000000000) ) ) 
 REPRESENTATION_ITEM ( '' )  SURFACE ( )  );
#41742 = ORIENTED_EDGE ( 'NONE', *, *, #27161, .F. ) ;
#41743 = CARTESIAN_POINT ( 'NONE',  ( 2.241536586108913820, 7.634468130435847932, -0.006292724672674973423 ) ) ;
#41744 = DIRECTION ( 'NONE',  ( 1.000000000000000000, 0.000000000000000000, 0.000000000000000000 ) ) ;
#41745 = FACE_OUTER_BOUND ( 'NONE', #8741, .T. ) ;
#41746 = ORIENTED_EDGE ( 'NONE', *, *, #63719, .T. ) ;
#41747 = CARTESIAN_POINT ( 'NONE',  ( 3.092491956585722512, 7.070043156103611892, 3.565393530441222314 ) ) ;
#41748 = CYLINDRICAL_SURFACE ( 'NONE', #48054, 4.999999999999999112 ) ;
#41749 = CARTESIAN_POINT ( 'NONE',  ( 5.514970785353741078, 0.004713149585127533910, -0.0003039746380528451919 ) ) ;
#41750 = AXIS2_PLACEMENT_3D ( 'NONE', #56772, #27454, #21155 ) ;
#41752 = ORIENTED_EDGE ( 'NONE', *, *, #61961, .F. ) ;
#41751 = CARTESIAN_POINT ( 'NONE',  ( 35.00000000000000000, 6.547236723514018308, -9.752226076388918585 ) ) ;
#41753 = CARTESIAN_POINT ( 'NONE',  ( 35.00000000000000000, 9.430788938294046631, -7.718225330433843290 ) ) ;
#41754 = EDGE_CURVE ( 'NONE', #32750, #9298, #62029, .T. ) ;
#41755 = DIRECTION ( 'NONE',  ( 0.000000000000000000, -0.01356324068817991828, 0.9999080150203990547 ) ) ;
#41756 = ORIENTED_EDGE ( 'NONE', *, *, #26334, .F. ) ;
#41757 = CARTESIAN_POINT ( 'NONE',  ( 0.2759803524722189705, -9.504501710971656081, 7.727919584673414555 ) ) ;
#41758 = CARTESIAN_POINT ( 'NONE',  ( 36.00000000000000711, 4.237174932027401475, 12.02534193257715600 ) ) ;
#41759 = DIRECTION ( 'NONE',  ( 0.000000000000000000, 0.01356324068817998940, -0.9999080150203990547 ) ) ;
#41760 = DIRECTION ( 'NONE',  ( 0.000000000000000000, 0.8276889981568879007, 0.5611870653623863836 ) ) ;
#41761 = DIRECTION ( 'NONE',  ( -1.000000000000000000, -0.000000000000000000, 0.000000000000000000 ) ) ;
#41762 = DIRECTION ( 'NONE',  ( 0.000000000000000000, 0.01356324068818000848, -0.9999080150203990547 ) ) ;
#41764 = ORIENTED_EDGE ( 'NONE', *, *, #53920, .F. ) ;
#41763 = CARTESIAN_POINT ( 'NONE',  ( 5.514624014163232779, -0.003946330869975260731, -0.001255375129357653909 ) ) ;
#41765 = VERTEX_POINT ( 'NONE', #19602 ) ;
#41766 = CARTESIAN_POINT ( 'NONE',  ( 2.241534463349553086, -0.005244187652451783553, 7.634462073473345711 ) ) ;
#41767 = VERTEX_POINT ( 'NONE', #60146 ) ;
#41768 = FILL_AREA_STYLE_COLOUR ( '', #6972 ) ;
#41769 = DIRECTION ( 'NONE',  ( 0.000000000000000000, 0.000000000000000000, 1.000000000000000000 ) ) ;
#41770 = CIRCLE ( 'NONE', #30044, 12.75000000000000178 ) ;
#41771 = CARTESIAN_POINT ( 'NONE',  ( 36.00000000000000711, 11.47561260193577048, -5.556331110570448928 ) ) ;
#41772 = CARTESIAN_POINT ( 'NONE',  ( 0.2655924914740778187, 4.229867354073712171, -11.49267051747963997 ) ) ;
#41773 = ORIENTED_EDGE ( 'NONE', *, *, #30998, .F. ) ;
#41774 = CARTESIAN_POINT ( 'NONE',  ( 1.937114397841932290, 8.920887662793592909, -9.228205347192362851 ) ) ;
#41775 = CARTESIAN_POINT ( 'NONE',  ( 0.2646305136544072623, 11.46223899740606100, -4.312539723326019647 ) ) ;
#41777 = B_SPLINE_CURVE_WITH_KNOTS ( 'NONE', 3,
 ( #43127, #12877, #27850, #17876, #18559, #33156, #8877, #17556 ),
 .UNSPECIFIED., .F., .F.,
 ( 4, 2, 2, 4 ),
 ( 2.453269466693398698E-18, 0.001774887840461971235, 0.002662331760692956528, 0.003549775680923942470 ),
 .UNSPECIFIED. ) ;
#41776 = CARTESIAN_POINT ( 'NONE',  ( -35.00000000000000000, -8.839356091079983102, -8.389074212634382022 ) ) ;
#41778 = ORIENTED_EDGE ( 'NONE', *, *, #60290, .F. ) ;
#41779 = AXIS2_PLACEMENT_3D ( 'NONE', #38609, #3385, #18681 ) ;
#41780 = ORIENTED_EDGE ( 'NONE', *, *, #1005, .T. ) ;
#41781 = CARTESIAN_POINT ( 'NONE',  ( 2.781367136452208122, 7.636197200465840496, -1.659348694504450217 ) ) ;
#41782 = VERTEX_POINT ( 'NONE', #14891 ) ;
#41783 = DIRECTION ( 'NONE',  ( 1.000000000000000000, -0.000000000000000000, 0.000000000000000000 ) ) ;
#41784 = B_SPLINE_CURVE_WITH_KNOTS ( 'NONE', 3,
 ( #47237, #1684, #21950, #27257, #42198, #1993, #62488 ),
 .UNSPECIFIED., .F., .F.,
 ( 4, 3, 4 ),
 ( 0.000000000000000000, 0.001700533616330544059, 0.005002426799371351152 ),
 .UNSPECIFIED. ) ;
#41785 = CARTESIAN_POINT ( 'NONE',  ( -35.00000000000000000, 4.732539170486427693, -11.23004253107759176 ) ) ;
#41786 = DIRECTION ( 'NONE',  ( 1.000000000000000000, 0.000000000000000000, 0.000000000000000000 ) ) ;
#41787 = LINE ( 'NONE', #62382, #34744 ) ;
#41788 = CARTESIAN_POINT ( 'NONE',  ( 9.575800908719084958, 13.45729701195361372, -1.072919909436246266 ) ) ;
#41789 = DIRECTION ( 'NONE',  ( -0.9582930651793754029, 0.08045274594386021827, 0.2742293873734361065 ) ) ;
#41790 = AXIS2_PLACEMENT_3D ( 'NONE', #6298, #58145, #26899 ) ;
#41791 = CARTESIAN_POINT ( 'NONE',  ( 2.255723233588951437, 7.499053486174019234, 1.456523090672637410 ) ) ;
#41792 = EDGE_CURVE ( 'NONE', #55068, #18977, #49294, .T. ) ;
#41793 = VERTEX_POINT ( 'NONE', #62753 ) ;
#41794 = CARTESIAN_POINT ( 'NONE',  ( -35.00000000000000000, 8.366449238204365813, 9.621072037177025749 ) ) ;
#41795 = ORIENTED_EDGE ( 'NONE', *, *, #6838, .T. ) ;
#41796 = CARTESIAN_POINT ( 'NONE',  ( 0.000000000000000000, -0.4804830611969332366, -6.919838746524582085 ) ) ;
#41797 = CARTESIAN_POINT ( 'NONE',  ( -22.27384469013076185, -2.625926801827875412, 2.581192766446261722 ) ) ;
#41799 = CARTESIAN_POINT ( 'NONE',  ( 37.00000000000000711, 0.1414404973753909112, 12.74921544981110522 ) ) ;
#41798 = VECTOR ( 'NONE', #30599, 1000.000000000000000 ) ;
#41800 = CARTESIAN_POINT ( 'NONE',  ( 2.262775599886258426, -3.942403752832051467, 6.546038779272026709 ) ) ;
#41801 = DIRECTION ( 'NONE',  ( 1.000000000000000000, 0.000000000000000000, -0.000000000000000000 ) ) ;
#41802 = AXIS2_PLACEMENT_3D ( 'NONE', #60674, #10780, #24429 ) ;
#41803 = DIRECTION ( 'NONE',  ( -1.000000000000000000, 0.000000000000000000, 0.000000000000000000 ) ) ;
#41804 = ORIENTED_EDGE ( 'NONE', *, *, #1827, .F. ) ;
#41805 = CIRCLE ( 'NONE', #11006, 5.000000000000000888 ) ;
#41806 = ORIENTED_EDGE ( 'NONE', *, *, #15964, .F. ) ;
#41807 = EDGE_CURVE ( 'NONE', #44942, #9046, #51420, .T. ) ;
#41808 = LINE ( 'NONE', #21539, #14174 ) ;
#41809 = VERTEX_POINT ( 'NONE', #36165 ) ;
#41810 = DIRECTION ( 'NONE',  ( 1.000000000000000000, 0.000000000000000000, 0.000000000000000000 ) ) ;
#41811 = CARTESIAN_POINT ( 'NONE',  ( -35.00000000000000000, -5.015831474386382105, 10.62137734850266391 ) ) ;
#41812 = AXIS2_PLACEMENT_3D ( 'NONE', #1008, #21275, #15624 ) ;
#41813 = CARTESIAN_POINT ( 'NONE',  ( 0.2646305136544065406, -4.064188116014473273, -11.55263159009962592 ) ) ;
#41814 = DIRECTION ( 'NONE',  ( 1.000000000000000000, 0.000000000000000000, -0.000000000000000000 ) ) ;
#41815 = EDGE_CURVE ( 'NONE', #20113, #44262, #33363, .T. ) ;
#41816 = VERTEX_POINT ( 'NONE', #6271 ) ;
#41817 = CIRCLE ( 'NONE', #36505, 2.899999999999995026 ) ;
#41818 = CARTESIAN_POINT ( 'NONE',  ( 0.000000000000000000, 0.000000000000000000, 0.000000000000000000 ) ) ;
#41819 = DIRECTION ( 'NONE',  ( 0.000000000000000000, 0.000000000000000000, 1.000000000000000000 ) ) ;
#41820 = CARTESIAN_POINT ( 'NONE',  ( 0.4613984246114875010, -1.858723191796552987, 12.17044190070616771 ) ) ;
#41821 = CYLINDRICAL_SURFACE ( 'NONE', #62508, 11.99999999999998579 ) ;
#41822 = CIRCLE ( 'NONE', #17387, 5.000000000000000888 ) ;
#41823 = B_SPLINE_CURVE_WITH_KNOTS ( 'NONE', 3,
 ( #39250, #49583, #64514, #63861 ),
 .UNSPECIFIED., .F., .F.,
 ( 4, 4 ),
 ( 0.007620068080905808769, 0.01192914805994312565 ),
 .UNSPECIFIED. ) ;
#41824 = CARTESIAN_POINT ( 'NONE',  ( 0.2911222467163535610, 6.312159098066323359, -10.50411792397751576 ) ) ;
#41825 = CARTESIAN_POINT ( 'NONE',  ( 2.263328370261528999, 2.746620058315294433, 7.131064289852348637 ) ) ;
#41826 = ORIENTED_EDGE ( 'NONE', *, *, #13626, .T. ) ;
#41827 = AXIS2_PLACEMENT_3D ( 'NONE', #44394, #24797, #54737 ) ;
#41828 = CARTESIAN_POINT ( 'NONE',  ( 1.452237505248552996, 12.55261342181978002, -1.611965288198602408 ) ) ;
#41829 = ORIENTED_EDGE ( 'NONE', *, *, #15979, .F. ) ;
#41830 = DIRECTION ( 'NONE',  ( 0.000000000000000000, 0.01356324068817998940, -0.9999080150203990547 ) ) ;
#41831 = CARTESIAN_POINT ( 'NONE',  ( 2.241506898688419458, 7.187425579579805657, 2.574154135948715005 ) ) ;
#41832 = DIRECTION ( 'NONE',  ( -1.000000000000000000, 0.000000000000000000, -0.000000000000000000 ) ) ;
#41833 = CARTESIAN_POINT ( 'NONE',  ( 5.514970785353741078, 0.004694330894494369230, -0.0005190732562558711188 ) ) ;
#41834 = CARTESIAN_POINT ( 'NONE',  ( -8.109707593773686440, -2.369880750454201213, 11.76635280190479982 ) ) ;
#41835 = AXIS2_PLACEMENT_3D ( 'NONE', #9391, #50973, #44994 ) ;
#41836 = VERTEX_POINT ( 'NONE', #26530 ) ;
#41837 = ORIENTED_EDGE ( 'NONE', *, *, #28374, .F. ) ;
#41838 = DIRECTION ( 'NONE',  ( 1.000000000000000000, 0.000000000000000000, 0.000000000000000000 ) ) ;
#41839 = VERTEX_POINT ( 'NONE', #37154 ) ;
#41840 = CARTESIAN_POINT ( 'NONE',  ( 35.00000000000000000, 4.705694406421931860E-17, -3.469127814946512892E-15 ) ) ;
#41841 = DIRECTION ( 'NONE',  ( -1.000000000000000000, -0.000000000000000000, -0.000000000000000000 ) ) ;
#41842 = FACE_OUTER_BOUND ( 'NONE', #25984, .T. ) ;
#41843 = DIRECTION ( 'NONE',  ( 0.000000000000000000, -0.4698238015817237656, -0.8827602140260383257 ) ) ;
#41844 = CARTESIAN_POINT ( 'NONE',  ( 2.717984159217651907, 7.788152353088505286, -0.2836133496094412898 ) ) ;
#41845 = CARTESIAN_POINT ( 'NONE',  ( 5.516018279890452902, 0.006707902355169300182, -0.0009545156522407284051 ) ) ;
#41846 = CARTESIAN_POINT ( 'NONE',  ( 1.719304012343089161, 12.64775761152706401, -1.452142814147889816 ) ) ;
#41847 = ORIENTED_EDGE ( 'NONE', *, *, #57607, .F. ) ;
#41848 = AXIS2_PLACEMENT_3D ( 'NONE', #32244, #32554, #31280 ) ;
#41849 = EDGE_CURVE ( 'NONE', #43631, #15685, #65205, .T. ) ;
#41850 = CARTESIAN_POINT ( 'NONE',  ( 2.000000000000001776, 0.000000000000000000, 0.000000000000000000 ) ) ;
#41851 = ORIENTED_EDGE ( 'NONE', *, *, #50688, .T. ) ;
#41852 = DIRECTION ( 'NONE',  ( 0.000000000000000000, 0.9635499925192219095, 0.2675283385292248073 ) ) ;
#41853 = ADVANCED_FACE ( 'NONE', ( #11248 ), #52794, .T. ) ;
#41854 = CARTESIAN_POINT ( 'NONE',  ( 16.78263030916553689, 12.17295508002146320, 5.836879698929895888 ) ) ;
#41855 = CARTESIAN_POINT ( 'NONE',  ( -27.08639648637162622, 1.635407781268146898, 1.614109828501612443 ) ) ;
#41856 = VERTEX_POINT ( 'NONE', #31207 ) ;
#41857 = CARTESIAN_POINT ( 'NONE',  ( 0.000000000000000000, 7.493043167941614513, -0.3229614270519962638 ) ) ;
#41858 = CARTESIAN_POINT ( 'NONE',  ( -22.71097035706202760, 2.846599994298365743, -4.089776368546553798 ) ) ;
#41859 = B_SPLINE_CURVE_WITH_KNOTS ( 'NONE', 3,
 ( #49602, #55572, #19982, #64859, #39607, #50262 ),
 .UNSPECIFIED., .F., .F.,
 ( 4, 2, 4 ),
 ( 0.000000000000000000, 0.0004528561986909411031, 0.0009057123973818822062 ),
 .UNSPECIFIED. ) ;
#41860 = DIRECTION ( 'NONE',  ( -0.000000000000000000, -1.000000000000000000, -0.000000000000000000 ) ) ;
#41861 = ORIENTED_EDGE ( 'NONE', *, *, #47374, .F. ) ;
#41862 = VERTEX_POINT ( 'NONE', #51511 ) ;
#41863 = CARTESIAN_POINT ( 'NONE',  ( 0.000000000000000000, 4.962980376314068742, 4.846014654777798469 ) ) ;
#41864 = ORIENTED_EDGE ( 'NONE', *, *, #28091, .T. ) ;
#41865 = DIRECTION ( 'NONE',  ( -1.000000000000000000, 0.000000000000000000, -0.000000000000000000 ) ) ;
#41866 = ORIENTED_EDGE ( 'NONE', *, *, #43343, .T. ) ;
#41867 = CIRCLE ( 'NONE', #51434, 5.000000000000000888 ) ;
#41868 = ORIENTED_EDGE ( 'NONE', *, *, #51474, .F. ) ;
#41869 = ORIENTED_EDGE ( 'NONE', *, *, #44775, .F. ) ;
#41870 = CARTESIAN_POINT ( 'NONE',  ( 0.3654063281920718054, 4.446369912832507154, 11.44627072062580808 ) ) ;
#41871 = CARTESIAN_POINT ( 'NONE',  ( 2.000000000000001776, 0.000000000000000000, 0.000000000000000000 ) ) ;
#41872 = EDGE_CURVE ( 'NONE', #26911, #36952, #55673, .T. ) ;
#41873 = PLANE ( 'NONE',  #2344 ) ;
#41874 = CARTESIAN_POINT ( 'NONE',  ( 9.687175622948609899, 11.98570860552671391, -0.5854820436212360146 ) ) ;
#41875 = DIRECTION ( 'NONE',  ( 1.000000000000000000, 0.000000000000000000, 0.000000000000000000 ) ) ;
#41876 = ORIENTED_EDGE ( 'NONE', *, *, #13754, .F. ) ;
#41877 = DIRECTION ( 'NONE',  ( 0.000000000000000000, 0.000000000000000000, 1.000000000000000000 ) ) ;
#41878 = EDGE_CURVE ( 'NONE', #19477, #5474, #5958, .T. ) ;
#41879 = ORIENTED_EDGE ( 'NONE', *, *, #37083, .F. ) ;
#41880 = DIRECTION ( 'NONE',  ( 1.000000000000000000, -0.000000000000000000, 0.000000000000000000 ) ) ;
#41881 = CARTESIAN_POINT ( 'NONE',  ( -3.438323251045651396, 11.96547819944141544, 6.261536211207373803 ) ) ;
#41882 = EDGE_CURVE ( 'NONE', #18732, #34279, #1617, .T. ) ;
#41883 = CARTESIAN_POINT ( 'NONE',  ( 1.000000000000000888, 6.253963800348318003, -4.139799123620975685 ) ) ;
#41884 = CARTESIAN_POINT ( 'NONE',  ( 0.3401186441510233305, -2.382124782498441284, 12.03768714635923942 ) ) ;
#41885 = CARTESIAN_POINT ( 'NONE',  ( 0.3665391374699472626, 11.62960183138726933, 3.952034409876334475 ) ) ;
#41886 = CARTESIAN_POINT ( 'NONE',  ( -35.00000000000000000, 0.000000000000000000, 0.000000000000000000 ) ) ;
#41887 = VERTEX_POINT ( 'NONE', #21210 ) ;
#41888 = ADVANCED_FACE ( 'NONE', ( #16883 ), #18062, .F. ) ;
#41889 = CARTESIAN_POINT ( 'NONE',  ( -35.00000000000000000, -3.340853584269456888, -11.26103545359859304 ) ) ;
#41890 = VERTEX_POINT ( 'NONE', #46818 ) ;
#41891 = EDGE_CURVE ( 'NONE', #47105, #44216, #27006, .T. ) ;
#41892 = DIRECTION ( 'NONE',  ( -1.000000000000000000, 0.000000000000000000, 0.000000000000000000 ) ) ;
#41893 = CARTESIAN_POINT ( 'NONE',  ( -35.00000000000000000, 0.000000000000000000, 0.000000000000000000 ) ) ;
#41894 = CARTESIAN_POINT ( 'NONE',  ( 3.047904605210422169, 6.318654123925978361, -4.747272783555583686 ) ) ;
#41895 = CARTESIAN_POINT ( 'NONE',  ( -35.00000000000000000, 9.217970097227725645, 7.971186206369506699 ) ) ;
#41896 = CYLINDRICAL_SURFACE ( 'NONE', #61503, 6.936499999999988120 ) ;
#41897 = ORIENTED_EDGE ( 'NONE', *, *, #18021, .T. ) ;
#41898 = CIRCLE ( 'NONE', #64248, 19.00000000000000000 ) ;
#41899 = DIRECTION ( 'NONE',  ( 0.000000000000000000, 0.01356324068817998940, -0.9999080150203990547 ) ) ;
#41900 = CARTESIAN_POINT ( 'NONE',  ( -10.90165637463012516, -7.508992741355087652, 9.360289953322833867 ) ) ;
#41901 = DIRECTION ( 'NONE',  ( -1.000000000000000000, 0.000000000000000000, 0.000000000000000000 ) ) ;
#41902 = CARTESIAN_POINT ( 'NONE',  ( 7.188828048469327214, -31.44854185097339894, -14.13838964164549417 ) ) ;
#41903 = EDGE_CURVE ( 'NONE', #38263, #50140, #65252, .T. ) ;
#41904 = DIRECTION ( 'NONE',  ( -0.000000000000000000, -0.000000000000000000, -1.000000000000000000 ) ) ;
#41905 = CIRCLE ( 'NONE', #13245, 5.000000000000000000 ) ;
#41906 = CARTESIAN_POINT ( 'NONE',  ( -28.66013792860432119, -1.071635578228289587, -1.490739498621034720 ) ) ;
#41907 = PRODUCT_DEFINITION_SHAPE ( 'NONE', 'NONE',  #65813 ) ;
#41908 = CARTESIAN_POINT ( 'NONE',  ( 35.00000000000000000, -11.61175578952786758, -1.771820996347120092 ) ) ;
#41909 = CARTESIAN_POINT ( 'NONE',  ( -21.17861794710831091, -11.44571409049744481, -3.604945070120774808 ) ) ;
#41910 = CIRCLE ( 'NONE', #62098, 1.500000000000000444 ) ;
#41911 = ORIENTED_EDGE ( 'NONE', *, *, #2552, .F. ) ;
#41912 = VERTEX_POINT ( 'NONE', #57465 ) ;
#41913 = CARTESIAN_POINT ( 'NONE',  ( 2.368238019615342971, -6.556525400300611928, 3.992969450835649248 ) ) ;
#41914 = CARTESIAN_POINT ( 'NONE',  ( 41.38732981120778476, -1.602042930228849249, -17.55180477253563964 ) ) ;
#41915 = DIRECTION ( 'NONE',  ( 1.000000000000000000, 0.000000000000000000, 0.000000000000000000 ) ) ;
#41916 = CARTESIAN_POINT ( 'NONE',  ( 0.3057689695767503157, -1.901059295890996870, 12.11137787899271601 ) ) ;
#41917 = ORIENTED_EDGE ( 'NONE', *, *, #3587, .T. ) ;
#41918 = VERTEX_POINT ( 'NONE', #57138 ) ;
#41919 = ORIENTED_EDGE ( 'NONE', *, *, #7126, .F. ) ;
#41920 = CARTESIAN_POINT ( 'NONE',  ( 3.047904605209668549, 7.891858004695730067, 0.4249306449412027509 ) ) ;
#41921 = EDGE_CURVE ( 'NONE', #42603, #58929, #35482, .T. ) ;
#41922 = AXIS2_PLACEMENT_3D ( 'NONE', #9400, #25055, #30028 ) ;
#41923 = DIRECTION ( 'NONE',  ( 1.000000000000000000, -0.000000000000000000, 0.000000000000000000 ) ) ;
#41924 = EDGE_LOOP ( 'NONE', ( #38154, #65455, #36568, #1949 ) ) ;
#41925 = CYLINDRICAL_SURFACE ( 'NONE', #57048, 12.18649999999999878 ) ;
#41926 = DIRECTION ( 'NONE',  ( 0.000000000000000000, -0.01356324068817998940, 0.9999080150203990547 ) ) ;
#41927 = ORIENTED_EDGE ( 'NONE', *, *, #65265, .T. ) ;
#41928 =( BOUNDED_CURVE ( )  B_SPLINE_CURVE ( 3, ( #61508, #56547, #60530, #10315 ),
 .UNSPECIFIED., .F., .F. ) 
 B_SPLINE_CURVE_WITH_KNOTS ( ( 4, 4 ),
 ( 0.6002665644134519418, 0.6265323918907089729 ),
 .UNSPECIFIED. ) 
 CURVE ( )  GEOMETRIC_REPRESENTATION_ITEM ( )  RATIONAL_B_SPLINE_CURVE ( ( 1.000000000000000000, 0.9999425096852141426, 0.9999425096852141426, 1.000000000000000000 ) ) 
 REPRESENTATION_ITEM ( '' )  );
#41929 = LINE ( 'NONE', #16665, #40747 ) ;
#41930 = CARTESIAN_POINT ( 'NONE',  ( 13.40144019692491995, -30.08877117594819595, -6.927253557473251888 ) ) ;
#41931 = FACE_OUTER_BOUND ( 'NONE', #3268, .T. ) ;
#41932 = ORIENTED_EDGE ( 'NONE', *, *, #26617, .T. ) ;
#41933 = CYLINDRICAL_SURFACE ( 'NONE', #38460, 5.000000000000000888 ) ;
#41934 = ORIENTED_EDGE ( 'NONE', *, *, #8270, .F. ) ;
#41935 = COLOUR_RGB ( '', 0.66274510, 0.83137255, 0.94901961) ;
#41936 = DIRECTION ( 'NONE',  ( -1.000000000000000000, 0.000000000000000000, 0.000000000000000000 ) ) ;
#41937 = CARTESIAN_POINT ( 'NONE',  ( 2.241526690369556096, 4.920579984890965264, 5.837196604699864899 ) ) ;
#41938 = CARTESIAN_POINT ( 'NONE',  ( -3.498383876424262517, -31.27426290440205747, 14.18200193795962605 ) ) ;
#41939 = CARTESIAN_POINT ( 'NONE',  ( 35.00000000000000000, 12.18632975068352664, 0.06441628369840225743 ) ) ;
#41940 = DIRECTION ( 'NONE',  ( -0.2475719085175105416, 8.403603522408387294E-16, -0.9688695217174485563 ) ) ;
#41941 = EDGE_CURVE ( 'NONE', #47639, #34574, #26595, .T. ) ;
#41942 = CARTESIAN_POINT ( 'NONE',  ( 1.719304012340733934, -11.67935079956419031, -5.066286238786891438 ) ) ;
#41943 = CARTESIAN_POINT ( 'NONE',  ( 0.000000000000000000, -5.107597897712309098, -4.693343793638478978 ) ) ;
#41944 = CARTESIAN_POINT ( 'NONE',  ( 0.2651627682582892165, 4.271106202749272107, 11.47719223137561961 ) ) ;
#41945 = VERTEX_POINT ( 'NONE', #26869 ) ;
#41946 = DIRECTION ( 'NONE',  ( 1.000000000000000000, 0.000000000000000000, 0.000000000000000000 ) ) ;
#41947 = VECTOR ( 'NONE', #26604, 1000.000000000000000 ) ;
#41948 = ORIENTED_EDGE ( 'NONE', *, *, #65060, .F. ) ;
#41949 = CARTESIAN_POINT ( 'NONE',  ( 5.516018279890452902, 0.006286471671801929263, -0.002527316374434327665 ) ) ;
#41950 = EDGE_CURVE ( 'NONE', #57314, #54998, #39417, .T. ) ;
#41951 = CARTESIAN_POINT ( 'NONE',  ( 2.440552418640498100, -5.770332237304409695, -5.099602138956265129 ) ) ;
#41952 = EDGE_CURVE ( 'NONE', #46346, #60499, #54445, .T. ) ;
#41953 = EDGE_LOOP ( 'NONE', ( #14243, #57810, #19366, #12437 ) ) ;
#41954 = DIRECTION ( 'NONE',  ( 1.000000000000000000, 0.000000000000000000, -0.000000000000000000 ) ) ;
#41955 = CARTESIAN_POINT ( 'NONE',  ( 5.515188684475870851, -0.001485678338381749095, -0.005140903460551130705 ) ) ;
#41956 = FACE_OUTER_BOUND ( 'NONE', #30104, .T. ) ;
#41957 = CARTESIAN_POINT ( 'NONE',  ( 0.000000000000000000, -6.777474576704061171, -0.6925993764991672519 ) ) ;
#41958 = ORIENTED_EDGE ( 'NONE', *, *, #32927, .T. ) ;
#41959 = EDGE_LOOP ( 'NONE', ( #15573, #16745, #9852, #38727 ) ) ;
#41960 = DIRECTION ( 'NONE',  ( 0.000000000000000000, -0.01356324068817998940, 0.9999080150203990547 ) ) ;
#41961 = ORIENTED_EDGE ( 'NONE', *, *, #46621, .F. ) ;
#41962 = EDGE_CURVE ( 'NONE', #16830, #21918, #23189, .T. ) ;
#41963 = CARTESIAN_POINT ( 'NONE',  ( -37.00000000000000711, 11.86701198550360203, -2.772148766915989881 ) ) ;
#41964 = FACE_OUTER_BOUND ( 'NONE', #15036, .T. ) ;
#41965 = LINE ( 'NONE', #17026, #9493 ) ;
#41966 = EDGE_CURVE ( 'NONE', #32375, #61727, #38477, .T. ) ;
#41967 = ORIENTED_EDGE ( 'NONE', *, *, #14517, .F. ) ;
#41968 = B_SPLINE_CURVE_WITH_KNOTS ( 'NONE', 3,
 ( #47248, #1694, #51254, #1026, #15961, #36252, #5360, #40931, #10999, #25631, #45923, #40594, #60887, #31284, #61860, #10649, #51585, #35603, #50913, #56210, #6032, #21292 ),
 .UNSPECIFIED., .F., .F.,
 ( 4, 3, 3, 3, 3, 3, 3, 4 ),
 ( 1.230521702633870283E-18, 4.449119708436748713E-05, 6.626296329540296850E-05, 8.803456484962499063E-05, 0.0001098060367612792814, 0.0001315774408628494997, 0.0001760698110411141487, 0.0001829697163287829684 ),
 .UNSPECIFIED. ) ;
#41969 = CARTESIAN_POINT ( 'NONE',  ( 0.2915757698887307403, -4.392559307431826099, -11.44067056871812760 ) ) ;
#41970 = EDGE_CURVE ( 'NONE', #36702, #4408, #22540, .T. ) ;
#41971 = CIRCLE ( 'NONE', #6963, 7.499999999999988454 ) ;
#41972 = EDGE_CURVE ( 'NONE', #8982, #15694, #41777, .T. ) ;
#41973 = CARTESIAN_POINT ( 'NONE',  ( 29.20591975386996708, 10.31637300579003558, 8.717626168519132079 ) ) ;
#41974 = DIRECTION ( 'NONE',  ( -1.000000000000000000, 0.000000000000000000, -0.000000000000000000 ) ) ;
#41975 = EDGE_CURVE ( 'NONE', #34540, #1249, #48175, .T. ) ;
#41976 = CARTESIAN_POINT ( 'NONE',  ( 35.00000000000000000, 4.705694406421931860E-17, -3.469127814946512892E-15 ) ) ;
#41977 = CARTESIAN_POINT ( 'NONE',  ( 0.3401186441510253844, -5.912862694513639994, -10.75260364139051639 ) ) ;
#41978 = DIRECTION ( 'NONE',  ( 1.000000000000000000, 0.000000000000000000, 0.000000000000000000 ) ) ;
#41979 = PRODUCT_DEFINITION_FORMATION_WITH_SPECIFIED_SOURCE ( 'ANY', '', #54612, .NOT_KNOWN. ) ;
#41980 = LINE ( 'NONE', #46986, #22979 ) ;
#41981 = DIRECTION ( 'NONE',  ( -1.000000000000000000, 0.000000000000000000, 0.000000000000000000 ) ) ;
#41982 = ORIENTED_EDGE ( 'NONE', *, *, #52708, .F. ) ;
#41983 = FACE_OUTER_BOUND ( 'NONE', #33031, .T. ) ;
#41984 = DIRECTION ( 'NONE',  ( -1.000000000000000000, 0.000000000000000000, 0.000000000000000000 ) ) ;
#41985 = AXIS2_PLACEMENT_3D ( 'NONE', #3967, #19900, #33879 ) ;
#41986 = ORIENTED_EDGE ( 'NONE', *, *, #30332, .T. ) ;
#41987 = CARTESIAN_POINT ( 'NONE',  ( 1.462291587748181465, 10.62080802716765682, 6.862867011840884324 ) ) ;
#41988 = CARTESIAN_POINT ( 'NONE',  ( 0.4626703367448722348, -9.247028139127534629, -8.128802338754541168 ) ) ;
#41989 = VERTEX_POINT ( 'NONE', #13213 ) ;
#41990 = CARTESIAN_POINT ( 'NONE',  ( 2.241352910868908310, 6.569501556381442953, 3.889181972941473386 ) ) ;
#41991 = VERTEX_POINT ( 'NONE', #33498 ) ;
#41992 = CARTESIAN_POINT ( 'NONE',  ( -35.00000000000000000, -4.041347439435779343, -11.02904044024213270 ) ) ;
#41993 = ORIENTED_EDGE ( 'NONE', *, *, #53889, .F. ) ;
#41994 = ORIENTED_EDGE ( 'NONE', *, *, #41457, .T. ) ;
#41995 = AXIS2_PLACEMENT_3D ( 'NONE', #3863, #64022, #39072 ) ;
#41997 = ADVANCED_FACE ( 'NONE', ( #7563 ), #60573, .F. ) ;
#41996 = CARTESIAN_POINT ( 'NONE',  ( -27.08429572838383947, -1.859677275556421927, 1.338867938658193424 ) ) ;
#41998 = ORIENTED_EDGE ( 'NONE', *, *, #27172, .F. ) ;
#41999 = DIRECTION ( 'NONE',  ( 0.000000000000000000, -0.01356324068817998940, 0.9999080150203990547 ) ) ;
#42000 = CARTESIAN_POINT ( 'NONE',  ( 5.516018279890452902, 0.006707902355168863032, 0.0009545156522404598482 ) ) ;
#42001 = CARTESIAN_POINT ( 'NONE',  ( 35.00000000000000000, 2.080187960898561172, -12.57916205664482234 ) ) ;
#42002 = CARTESIAN_POINT ( 'NONE',  ( 0.7400311444011703488, -0.3548322008126197358, -12.39937114182724720 ) ) ;
#42003 = ORIENTED_EDGE ( 'NONE', *, *, #38711, .F. ) ;
#42004 = CYLINDRICAL_SURFACE ( 'NONE', #8683, 2.809571291727933851 ) ;
#42005 = CARTESIAN_POINT ( 'NONE',  ( 3.448218607682480563, -27.97504209443001955, 12.21548802405080991 ) ) ;
#42006 = CARTESIAN_POINT ( 'NONE',  ( -22.71097035706202405, -4.965150228107763297, -0.4203397252017324615 ) ) ;
#42008 = EDGE_LOOP ( 'NONE', ( #8352, #31773, #30568, #51601 ) ) ;
#42007 = DIRECTION ( 'NONE',  ( 1.000000000000000000, 0.000000000000000000, 0.000000000000000000 ) ) ;
#42009 = CARTESIAN_POINT ( 'NONE',  ( 0.000000000000000000, 0.000000000000000000, 0.000000000000000000 ) ) ;
#42010 = ORIENTED_EDGE ( 'NONE', *, *, #28898, .F. ) ;
#42011 = CARTESIAN_POINT ( 'NONE',  ( -35.00000000000000000, -0.1652884326465054177, 12.18537902504609072 ) ) ;
#42012 = ADVANCED_FACE ( 'NONE', ( #54101 ), #49137, .T. ) ;
#42013 = EDGE_LOOP ( 'NONE', ( #60663, #4054, #62865, #6210 ) ) ;
#42014 = CARTESIAN_POINT ( 'NONE',  ( 22.05006909623952183, -10.53419554220477217, -5.760554779199603459 ) ) ;
#42015 = CARTESIAN_POINT ( 'NONE',  ( 2.241506898688419458, -4.937416071751796309, -5.822995664778306768 ) ) ;
#42016 = CARTESIAN_POINT ( 'NONE',  ( 35.00000000000000000, 10.80478261802181628, -5.636262487437359248 ) ) ;
#42017 = VECTOR ( 'NONE', #17539, 1000.000000000000000 ) ;
#42018 = ORIENTED_EDGE ( 'NONE', *, *, #7441, .T. ) ;
#42019 = CARTESIAN_POINT ( 'NONE',  ( 36.00000000000000711, -1.457575200925455672, 12.66641127287626745 ) ) ;
#42020 = ADVANCED_FACE ( 'NONE', ( #45110 ), #61058, .T. ) ;
#42021 = DIRECTION ( 'NONE',  ( 1.000000000000000000, 0.000000000000000000, 0.000000000000000000 ) ) ;
#42022 = FACE_OUTER_BOUND ( 'NONE', #13830, .T. ) ;
#42023 = ORIENTED_EDGE ( 'NONE', *, *, #10374, .T. ) ;
#42024 = ORIENTED_EDGE ( 'NONE', *, *, #17943, .F. ) ;
#42025 = DIRECTION ( 'NONE',  ( 0.000000000000000000, -0.01356324068818000328, 0.9999080150203990547 ) ) ;
#42026 = VERTEX_POINT ( 'NONE', #10493 ) ;
#42027 = B_SPLINE_CURVE_WITH_KNOTS ( 'NONE', 3,
 ( #31303, #45947, #35621, #56919, #10347, #36615 ),
 .UNSPECIFIED., .F., .F.,
 ( 4, 2, 4 ),
 ( 0.0002637379172192601240, 0.0009975831966643354445, 0.001731428476109410711 ),
 .UNSPECIFIED. ) ;
#42028 = B_SPLINE_CURVE_WITH_KNOTS ( 'NONE', 3,
 ( #63454, #37553, #22249, #47535, #58499, #12931, #11617, #42510, #62809, #31887, #52206, #33212, #42186, #16940, #53523, #12271 ),
 .UNSPECIFIED., .F., .F.,
 ( 4, 3, 3, 3, 3, 4 ),
 ( 8.673617379884035472E-19, 0.0002176109881719744219, 0.0004352086762393612995, 0.0006528017811445412490, 0.0007615147961449995635, 0.0009453342004946792753 ),
 .UNSPECIFIED. ) ;
#42029 = EDGE_CURVE ( 'NONE', #28743, #34193, #43997, .T. ) ;
#42030 = ORIENTED_EDGE ( 'NONE', *, *, #14483, .T. ) ;
#42031 = CARTESIAN_POINT ( 'NONE',  ( 0.000000000000000000, -6.201547234537033937, 2.820401998297862978 ) ) ;
#42032 = CARTESIAN_POINT ( 'NONE',  ( 1.014383007554952032, -10.59286224865785542, 6.628652139012873867 ) ) ;
#42033 = CARTESIAN_POINT ( 'NONE',  ( -37.00000000000000711, 12.17626345777664376, -0.4993900848166082374 ) ) ;
#42034 = DIRECTION ( 'NONE',  ( -1.000000000000000000, -0.000000000000000000, -0.000000000000000000 ) ) ;
#42035 = DIRECTION ( 'NONE',  ( 1.000000000000000000, 0.000000000000000000, 0.000000000000000000 ) ) ;
#42036 = DIRECTION ( 'NONE',  ( 0.000000000000000000, -0.01356324068817998940, 0.9999080150203990547 ) ) ;
#42037 = CYLINDRICAL_SURFACE ( 'NONE', #33375, 12.18650000000000055 ) ;
#42038 = CIRCLE ( 'NONE', #54824, 5.000000000000000888 ) ;
#42039 = ORIENTED_EDGE ( 'NONE', *, *, #36212, .T. ) ;
#42040 = CARTESIAN_POINT ( 'NONE',  ( -27.78468958554971380, 25.00000000000000000, 8.565911087387465983 ) ) ;
#42041 = CARTESIAN_POINT ( 'NONE',  ( -3.386646625484277529, -11.12986073946647991, 4.506218457162742830 ) ) ;
#42042 = EDGE_CURVE ( 'NONE', #11684, #47167, #15322, .T. ) ;
#42043 = CIRCLE ( 'NONE', #44050, 12.74999999999999822 ) ;
#42044 = CARTESIAN_POINT ( 'NONE',  ( 0.3106921474978497355, 4.414111574791988346, -11.43920276778352907 ) ) ;
#42045 = LINE ( 'NONE', #62327, #25787 ) ;
#42046 = ADVANCED_FACE ( 'NONE', ( #55074 ), #30768, .T. ) ;
#42047 = DIRECTION ( 'NONE',  ( 0.000000000000000000, 0.01356324068817992175, -0.9999080150203990547 ) ) ;
#42048 = EDGE_CURVE ( 'NONE', #20926, #27786, #54403, .T. ) ;
#42049 = CARTESIAN_POINT ( 'NONE',  ( 35.00000000000000000, -11.73463472867578083, -3.287724142101374092 ) ) ;
#42050 = ORIENTED_EDGE ( 'NONE', *, *, #44652, .T. ) ;
#42051 = DIRECTION ( 'NONE',  ( 0.000000000000000000, 0.000000000000000000, 1.000000000000000000 ) ) ;
#42052 = LINE ( 'NONE', #48050, #17663 ) ;
#42053 = CARTESIAN_POINT ( 'NONE',  ( 0.3040950598368152291, -12.25911170648142701, 0.2511348647275222223 ) ) ;
#42054 = CARTESIAN_POINT ( 'NONE',  ( -25.00000000000000355, -30.00000000000000000, -5.000000000000000888 ) ) ;
#42055 = CARTESIAN_POINT ( 'NONE',  ( -26.56896637191177035, 10.48260233735502922, 5.841271018688308558 ) ) ;
#42056 = DIRECTION ( 'NONE',  ( -1.000000000000000000, 0.000000000000000000, 0.000000000000000000 ) ) ;
#42057 = VERTEX_POINT ( 'NONE', #55745 ) ;
#42058 = DIRECTION ( 'NONE',  ( 1.000000000000000000, 0.000000000000000000, -0.000000000000000000 ) ) ;
#42059 = DIRECTION ( 'NONE',  ( -0.000000000000000000, -0.000000000000000000, -1.000000000000000000 ) ) ;
#42060 = DIRECTION ( 'NONE',  ( -1.000000000000000000, -0.000000000000000000, 0.000000000000000000 ) ) ;
#42061 = ORIENTED_EDGE ( 'NONE', *, *, #47336, .T. ) ;
#42062 = CARTESIAN_POINT ( 'NONE',  ( 2.717984159219797302, 6.886544461123903282, 3.648459810929759684 ) ) ;
#42063 = FACE_OUTER_BOUND ( 'NONE', #52192, .T. ) ;
#42065 = ORIENTED_EDGE ( 'NONE', *, *, #27794, .T. ) ;
#42064 = DIRECTION ( 'NONE',  ( -1.000000000000000000, -0.000000000000000000, 0.000000000000000000 ) ) ;
#42066 = CARTESIAN_POINT ( 'NONE',  ( -37.00000000000000711, 0.000000000000000000, 0.000000000000000000 ) ) ;
#42067 = EDGE_CURVE ( 'NONE', #62829, #33917, #45084, .T. ) ;
#42068 = VECTOR ( 'NONE', #55679, 1000.000000000000114 ) ;
#42069 = CARTESIAN_POINT ( 'NONE',  ( -35.00000000000000000, 11.73808581813437968, -0.4353888892048790038 ) ) ;
#42070 = VERTEX_POINT ( 'NONE', #24485 ) ;
#42071 = DIRECTION ( 'NONE',  ( -0.000000000000000000, -1.000000000000000000, -0.000000000000000000 ) ) ;
#42072 = EDGE_CURVE ( 'NONE', #36819, #17286, #52511, .T. ) ;
#42073 = CARTESIAN_POINT ( 'NONE',  ( 35.00000000000000000, -11.35427606708803161, 4.426194442447358490 ) ) ;
#42075 = AXIS2_PLACEMENT_3D ( 'NONE', #18032, #43610, #38296 ) ;
#42074 = FACE_OUTER_BOUND ( 'NONE', #17651, .T. ) ;
#42076 = CYLINDRICAL_SURFACE ( 'NONE', #24467, 1.499999999999997780 ) ;
#42077 = DIRECTION ( 'NONE',  ( -1.000000000000000000, 0.000000000000000000, 0.000000000000000000 ) ) ;
#42078 = CARTESIAN_POINT ( 'NONE',  ( 0.3218525148189828045, 5.919623386703340984, 10.74192973049790645 ) ) ;
#42080 = EDGE_LOOP ( 'NONE', ( #6635, #54138, #26664, #48458 ) ) ;
#42079 = CARTESIAN_POINT ( 'NONE',  ( 0.3057689695767490945, 11.43929056598612171, -4.409323295154093714 ) ) ;
#42081 = ORIENTED_EDGE ( 'NONE', *, *, #47823, .F. ) ;
#42082 = CARTESIAN_POINT ( 'NONE',  ( 23.20059726473823503, 3.175887350242510898, -11.57493929936777377 ) ) ;
#42083 = ORIENTED_EDGE ( 'NONE', *, *, #62442, .T. ) ;
#42084 = EDGE_CURVE ( 'NONE', #19513, #50728, #3679, .T. ) ;
#42085 = CARTESIAN_POINT ( 'NONE',  ( -35.00000000000000000, 11.68758509253248334, -1.171570255487489609 ) ) ;
#42086 = CARTESIAN_POINT ( 'NONE',  ( 2.034671305879990566, 1.331347915349286204, 11.60021725667403203 ) ) ;
#42087 = DIRECTION ( 'NONE',  ( 0.000000000000000000, 0.01356324068817991481, -0.9999080150203990547 ) ) ;
#42088 = VERTEX_POINT ( 'NONE', #4559 ) ;
#42089 = CARTESIAN_POINT ( 'NONE',  ( -25.54417658651491863, -4.240019242199836391, 11.22596262356930197 ) ) ;
#42090 = CARTESIAN_POINT ( 'NONE',  ( 1.014383007554948701, -3.853787798429482603, 11.88680274101310630 ) ) ;
#42091 = VERTEX_POINT ( 'NONE', #25469 ) ;
#42092 = ORIENTED_EDGE ( 'NONE', *, *, #14672, .T. ) ;
#42093 = CARTESIAN_POINT ( 'NONE',  ( 2.305787727787085295, 7.508843116234176662, -1.493241775258346227 ) ) ;
#42094 = EDGE_CURVE ( 'NONE', #56806, #45280, #20650, .T. ) ;
#42095 = VERTEX_POINT ( 'NONE', #19521 ) ;
#42096 = CYLINDRICAL_SURFACE ( 'NONE', #10431, 12.18649999999999878 ) ;
#42097 = CARTESIAN_POINT ( 'NONE',  ( 5.516018279890452902, -0.006771744149385743039, -0.0002248006052446425063 ) ) ;
#42098 = CARTESIAN_POINT ( 'NONE',  ( 8.958004941509509322, 4.004350268857352013, 12.89476050860881173 ) ) ;
#42099 = ADVANCED_FACE ( 'NONE', ( #39785 ), #9846, .T. ) ;
#42100 = DIRECTION ( 'NONE',  ( -1.000000000000000000, 0.000000000000000000, 0.000000000000000000 ) ) ;
#42101 = CARTESIAN_POINT ( 'NONE',  ( -22.51237073810381517, 0.9543406717316886834, -4.319597983500836236 ) ) ;
#42102 = CARTESIAN_POINT ( 'NONE',  ( 2.276198483117263027, 7.501576331167730594, 1.479169956994091706 ) ) ;
#42103 = VERTEX_POINT ( 'NONE', #56051 ) ;
#42104 = CYLINDRICAL_SURFACE ( 'NONE', #39029, 5.000000000000001776 ) ;
#42105 = VERTEX_POINT ( 'NONE', #218 ) ;
#42106 = DIRECTION ( 'NONE',  ( 1.000000000000000000, 0.000000000000000000, 0.000000000000000000 ) ) ;
#42107 = CARTESIAN_POINT ( 'NONE',  ( -37.00000000000000711, 11.98254675519231860, -2.220215194441768514 ) ) ;
#42108 = CARTESIAN_POINT ( 'NONE',  ( -37.00000000000000711, 12.68495603654572079, 1.286231064351357256 ) ) ;
#42109 = DIRECTION ( 'NONE',  ( 0.000000000000000000, -0.01356324068817991828, 0.9999080150203990547 ) ) ;
#42110 = DIRECTION ( 'NONE',  ( 0.000000000000000000, 0.9635499925192219095, 0.2675283385292248073 ) ) ;
#42111 = VECTOR ( 'NONE', #16008, 1000.000000000000000 ) ;
#42112 = CARTESIAN_POINT ( 'NONE',  ( 0.2651627923886318294, -11.47719387551883941, -4.271101819784471232 ) ) ;
#42113 = EDGE_CURVE ( 'NONE', #27370, #31676, #34768, .T. ) ;
#42114 = ORIENTED_EDGE ( 'NONE', *, *, #40843, .T. ) ;
#42115 = VERTEX_POINT ( 'NONE', #4883 ) ;
#42116 = CARTESIAN_POINT ( 'NONE',  ( -27.09364415740217424, 0.1694361397562917371, 2.313349100776200817 ) ) ;
#42117 = CIRCLE ( 'NONE', #21964, 7.499999999999988454 ) ;
#42118 = EDGE_CURVE ( 'NONE', #4847, #15301, #65685, .T. ) ;
#42119 =( BOUNDED_CURVE ( )  B_SPLINE_CURVE ( 3, ( #49852, #4301, #24575, #29879 ),
 .UNSPECIFIED., .F., .F. ) 
 B_SPLINE_CURVE_WITH_KNOTS ( ( 4, 4 ),
 ( 5.652045941182875843, 5.686890868700008816 ),
 .UNSPECIFIED. ) 
 CURVE ( )  GEOMETRIC_REPRESENTATION_ITEM ( )  RATIONAL_B_SPLINE_CURVE ( ( 1.000000000000000000, 0.9998988218115538729, 0.9998988218115538729, 1.000000000000000000 ) ) 
 REPRESENTATION_ITEM ( '' )  );
#42120 = ORIENTED_EDGE ( 'NONE', *, *, #41598, .T. ) ;
#42121 = CARTESIAN_POINT ( 'NONE',  ( 0.3223008802179250232, 7.695050880595616150, -9.550960164375519312 ) ) ;
#42122 = DIRECTION ( 'NONE',  ( -1.000000000000000000, 0.000000000000000000, 0.000000000000000000 ) ) ;
#42123 = FACE_OUTER_BOUND ( 'NONE', #63033, .T. ) ;
#42124 = FACE_OUTER_BOUND ( 'NONE', #31332, .T. ) ;
#42125 = ORIENTED_EDGE ( 'NONE', *, *, #29208, .T. ) ;
#42126 = CYLINDRICAL_SURFACE ( 'NONE', #20786, 12.75000000000000178 ) ;
#42127 = LINE ( 'NONE', #20878, #25779 ) ;
#42128 = CARTESIAN_POINT ( 'NONE',  ( -26.43258404273187878, 0.2934201954354447306, -3.465947334857406137 ) ) ;
#42129 = DIRECTION ( 'NONE',  ( 1.000000000000000000, 1.685093406416449860E-16, -1.011030131491573426E-17 ) ) ;
#42130 = B_SPLINE_CURVE_WITH_KNOTS ( 'NONE', 3,
 ( #57673, #48361, #7423, #2811, #7108, #17428, #63286, #48674, #22071, #23072 ),
 .UNSPECIFIED., .F., .F.,
 ( 4, 3, 3, 4 ),
 ( 2.453269466693398698E-18, 6.607638129004548514E-05, 9.911389841680599507E-05, 0.0001667630577588613897 ),
 .UNSPECIFIED. ) ;
#42131 = CARTESIAN_POINT ( 'NONE',  ( -36.00000000000000711, 4.074242145636004508, 12.08151691381191917 ) ) ;
#42132 = FACE_OUTER_BOUND ( 'NONE', #3716, .T. ) ;
#42133 = VERTEX_POINT ( 'NONE', #5544 ) ;
#42134 = CARTESIAN_POINT ( 'NONE',  ( 0.3665391374699464300, 6.368473106897276637, -10.50279796150429945 ) ) ;
#42135 = VERTEX_POINT ( 'NONE', #15804 ) ;
#42136 = DIRECTION ( 'NONE',  ( 0.000000000000000000, 0.01356324068817998940, -0.9999080150203990547 ) ) ;
#42137 = CARTESIAN_POINT ( 'NONE',  ( -35.00000000000000000, -9.040300684349640292, -7.499679039484155041 ) ) ;
#42138 = CARTESIAN_POINT ( 'NONE',  ( 5.514624014163232779, -0.004045310349816146414, -0.0008859786816841948168 ) ) ;
#42139 = CARTESIAN_POINT ( 'NONE',  ( 3.152665057734129750, 3.161213418913565221, -7.281573230474259972 ) ) ;
#42140 = CARTESIAN_POINT ( 'NONE',  ( -6.407494522312451757, -1.624111497457272790, 11.88968263856500940 ) ) ;
#42141 = ORIENTED_EDGE ( 'NONE', *, *, #27020, .T. ) ;
#42142 = ORIENTED_EDGE ( 'NONE', *, *, #57044, .T. ) ;
#42143 = CARTESIAN_POINT ( 'NONE',  ( 0.3002738374340830352, 1.906042098269019824, 12.10874171309340497 ) ) ;
#42144 = VERTEX_POINT ( 'NONE', #52061 ) ;
#42145 = EDGE_CURVE ( 'NONE', #44513, #23007, #29144, .T. ) ;
#42146 = CARTESIAN_POINT ( 'NONE',  ( 1.577070743587938306, 1.421807588298878322, 11.92044867579712886 ) ) ;
#42147 = CARTESIAN_POINT ( 'NONE',  ( 0.2851083653049504285, -0.4107471485392698018, 11.99296822225285730 ) ) ;
#42148 = CARTESIAN_POINT ( 'NONE',  ( 21.90174657591892071, -13.47998113580522528, -0.7349207973210680755 ) ) ;
#42149 = DIRECTION ( 'NONE',  ( 0.000000000000000000, -0.9999080150203990547, -0.01356324068816951688 ) ) ;
#42150 = DIRECTION ( 'NONE',  ( -1.000000000000000000, 0.000000000000000000, 0.000000000000000000 ) ) ;
#42151 = CARTESIAN_POINT ( 'NONE',  ( 2.288423627607476973, -1.169285315515829371, 7.560204962263195938 ) ) ;
#42152 = DIRECTION ( 'NONE',  ( -1.000000000000000000, 0.000000000000000000, -0.000000000000000000 ) ) ;
#42153 = VERTEX_POINT ( 'NONE', #61692 ) ;
#42154 = CARTESIAN_POINT ( 'NONE',  ( 2.990245332647867738, -5.834301250882223400, 6.155689586375181044 ) ) ;
#42155 = VERTEX_POINT ( 'NONE', #20815 ) ;
#42156 = AXIS2_PLACEMENT_3D ( 'NONE', #47850, #27554, #16612 ) ;
#42157 =( NAMED_UNIT ( * ) PLANE_ANGLE_UNIT ( ) SI_UNIT ( $, .RADIAN. ) );
#42158 = DIRECTION ( 'NONE',  ( -1.000000000000000000, 0.000000000000000000, 0.000000000000000000 ) ) ;
#42159 = CARTESIAN_POINT ( 'NONE',  ( 5.536195898058073439, 0.007896796515810928022, -0.003145317580921069833 ) ) ;
#42160 = ADVANCED_FACE ( 'NONE', ( #31755 ), #31117, .T. ) ;
#42161 = CIRCLE ( 'NONE', #31590, 20.00000000000000000 ) ;
#42162 = CARTESIAN_POINT ( 'NONE',  ( 3.152665057734128862, 2.258875078502223133, 7.609997527621164437 ) ) ;
#42163 = ORIENTED_EDGE ( 'NONE', *, *, #50921, .T. ) ;
#42164 = CARTESIAN_POINT ( 'NONE',  ( -22.31328051695926007, -0.8849444482787947042, 3.685074213229300621 ) ) ;
#42165 = DIRECTION ( 'NONE',  ( -1.000000000000000000, -0.000000000000000000, -0.000000000000000000 ) ) ;
#42166 = CARTESIAN_POINT ( 'NONE',  ( -10.00000000000000178, 0.000000000000000000, 0.000000000000000000 ) ) ;
#42167 = ORIENTED_EDGE ( 'NONE', *, *, #43297, .T. ) ;
#42168 = ORIENTED_EDGE ( 'NONE', *, *, #29050, .F. ) ;
#42169 = CARTESIAN_POINT ( 'NONE',  ( -17.19056858472900728, 2.658600115333384917, -11.70257571668042296 ) ) ;
#42170 = ORIENTED_EDGE ( 'NONE', *, *, #12140, .F. ) ;
#42171 = EDGE_CURVE ( 'NONE', #12997, #34948, #63116, .T. ) ;
#42172 = VERTEX_POINT ( 'NONE', #16154 ) ;
#42173 = ORIENTED_EDGE ( 'NONE', *, *, #63883, .T. ) ;
#42174 = ORIENTED_EDGE ( 'NONE', *, *, #63248, .F. ) ;
#42175 = CARTESIAN_POINT ( 'NONE',  ( -22.27706485742869091, -2.625261754997692876, 2.580541389029905819 ) ) ;
#42176 = EDGE_CURVE ( 'NONE', #46588, #35243, #36938, .T. ) ;
#42177 = CARTESIAN_POINT ( 'NONE',  ( -37.00000000000000711, -5.391785509270885512, -10.43555801961481677 ) ) ;
#42178 = DIRECTION ( 'NONE',  ( -1.000000000000000000, 0.000000000000000000, 0.000000000000000000 ) ) ;
#42179 = CARTESIAN_POINT ( 'NONE',  ( 5.520433897694421610, -0.01397038704729910638, 0.005630909886753099683 ) ) ;
#42180 = FACE_OUTER_BOUND ( 'NONE', #37935, .T. ) ;
#42182 = ORIENTED_EDGE ( 'NONE', *, *, #47973, .T. ) ;
#42181 = B_SPLINE_CURVE_WITH_KNOTS ( 'NONE', 3,
 ( #5718, #52250, #1377, #21662, #35925, #11015, #46584, #36270, #7008, #47264, #46273, #56913, #41916, #6690, #62515, #27278, #2017, #26303, #41588, #51598, #1704, #41253 ),
 .UNSPECIFIED., .F., .F.,
 ( 4, 3, 3, 3, 3, 3, 3, 4 ),
 ( 8.741117365843378158E-19, 4.449119708436956745E-05, 6.626296329540612624E-05, 8.803456484962883955E-05, 0.0001098060367612828321, 0.0001315774408628544599, 0.0001760698110411208165, 0.0001829697163287820740 ),
 .UNSPECIFIED. ) ;
#42183 = CARTESIAN_POINT ( 'NONE',  ( -35.00000000000000000, -7.110831038798204773, -9.896810808925470937 ) ) ;
#42184 = ORIENTED_EDGE ( 'NONE', *, *, #52480, .T. ) ;
#42185 = CARTESIAN_POINT ( 'NONE',  ( -35.00000000000000000, 7.474872387601008583, 9.060822531526074641 ) ) ;
#42186 = CARTESIAN_POINT ( 'NONE',  ( 2.994568964204062489, 4.756002438591091064, 6.289764245798157738 ) ) ;
#42187 = CARTESIAN_POINT ( 'NONE',  ( 2.244591118396912055, 3.724266936772022696, -6.665613643997293281 ) ) ;
#42188 = CARTESIAN_POINT ( 'NONE',  ( 0.3006302518452043104, -8.051021221755712887, -9.243299516615106626 ) ) ;
#42189 = CARTESIAN_POINT ( 'NONE',  ( 20.00005080000000035, 0.000000000000000000, 1.000000000000000000 ) ) ;
#42190 = CARTESIAN_POINT ( 'NONE',  ( 35.00000000000000000, -4.983891302653661093, -11.73555825188274504 ) ) ;
#42191 = ADVANCED_FACE ( 'NONE', ( #41082 ), #61360, .T. ) ;
#42192 = VECTOR ( 'NONE', #32284, 1000.000000000000000 ) ;
#42193 = ORIENTED_EDGE ( 'NONE', *, *, #21455, .T. ) ;
#42194 = CARTESIAN_POINT ( 'NONE',  ( 0.2646305136544072623, 12.08286001766538398, -1.996350543472872996 ) ) ;
#42195 = AXIS2_PLACEMENT_3D ( 'NONE', #44170, #49186, #47860 ) ;
#42196 = ORIENTED_EDGE ( 'NONE', *, *, #13468, .T. ) ;
#42197 = DIRECTION ( 'NONE',  ( 0.000000000000000000, -0.01356324068817991828, 0.9999080150203990547 ) ) ;
#42198 = CARTESIAN_POINT ( 'NONE',  ( 2.350038591457881409, 10.18214835919976302, -3.024612895785611766 ) ) ;
#42199 = FACE_OUTER_BOUND ( 'NONE', #35870, .T. ) ;
#42200 = DIRECTION ( 'NONE',  ( 0.000000000000000000, 0.000000000000000000, 1.000000000000000000 ) ) ;
#42201 = EDGE_LOOP ( 'NONE', ( #21560, #25605, #14509, #58583 ) ) ;
#42202 = CARTESIAN_POINT ( 'NONE',  ( 35.00000000000000000, -8.766823244861932096, 7.817610399097601359 ) ) ;
#42203 = CARTESIAN_POINT ( 'NONE',  ( 0.3537226245948345005, 2.388187631842678016, -12.04110684114370677 ) ) ;
#42204 = CARTESIAN_POINT ( 'NONE',  ( 2.000000000000001776, 0.000000000000000000, 0.000000000000000000 ) ) ;
#42205 = AXIS2_PLACEMENT_3D ( 'NONE', #14462, #20123, #4852 ) ;
#42206 = CARTESIAN_POINT ( 'NONE',  ( -3.649648704207571814, 12.48837185217044166, 5.141182941002472973 ) ) ;
#42207 = B_SPLINE_CURVE_WITH_KNOTS ( 'NONE', 3,
 ( #44820, #10224, #55460, #45810, #25193, #49821, #30502, #50799, #39834, #9550, #34818, #60439, #5252, #35803, #35150, #19570, #25518, #54817, #45466, #15212, #65734, #20203, #24881, #40480, #60777, #64758 ),
 .UNSPECIFIED., .F., .F.,
 ( 4, 2, 2, 2, 2, 2, 2, 2, 2, 2, 2, 2, 4 ),
 ( 3.004629197474318463E-18, 0.001181670535257466504, 0.001772505802886197371, 0.002363341070514927804, 0.003545011605772387803, 0.004726682141029846934, 0.005317517408658578235, 0.005908352676287307800, 0.007090023211544771269, 0.007680858479173503436, 0.008271693746802234737, 0.008862529014430967772, 0.009453364282059699072 ),
 .UNSPECIFIED. ) ;
#42208 = EDGE_CURVE ( 'NONE', #20627, #27642, #4075, .T. ) ;
#42209 = AXIS2_PLACEMENT_3D ( 'NONE', #12961, #3338, #48555 ) ;
#42210 = CARTESIAN_POINT ( 'NONE',  ( -37.00000000000000711, 0.000000000000000000, 0.000000000000000000 ) ) ;
#42211 = VERTEX_POINT ( 'NONE', #1197 ) ;
#42212 = CARTESIAN_POINT ( 'NONE',  ( 3.031336079628962121, -0.4165536638489777954, -7.886784934834683014 ) ) ;
#42213 = CARTESIAN_POINT ( 'NONE',  ( 1.462291587750754296, -5.766456054323672475, -11.25382118863359260 ) ) ;
#42214 = ORIENTED_EDGE ( 'NONE', *, *, #17491, .F. ) ;
#42216 = ORIENTED_EDGE ( 'NONE', *, *, #65428, .T. ) ;
#42215 = EDGE_CURVE ( 'NONE', #43782, #29713, #2633, .T. ) ;
#42217 = CARTESIAN_POINT ( 'NONE',  ( -37.00000000000000711, 8.573591947375437172, -8.029056188533592930 ) ) ;
#42218 = LINE ( 'NONE', #3016, #35338 ) ;
#42219 = CARTESIAN_POINT ( 'NONE',  ( -29.68541646480307250, -1.792450633335325616, 13.38582821403480771 ) ) ;
#42220 = FACE_OUTER_BOUND ( 'NONE', #17388, .T. ) ;
#42221 = EDGE_CURVE ( 'NONE', #46041, #23282, #21128, .T. ) ;
#42222 = VERTEX_POINT ( 'NONE', #21817 ) ;
#42223 = ORIENTED_EDGE ( 'NONE', *, *, #12115, .T. ) ;
#42224 = ORIENTED_EDGE ( 'NONE', *, *, #56280, .F. ) ;
#42225 = CYLINDRICAL_SURFACE ( 'NONE', #48273, 4.999999999999999112 ) ;
#42226 = CIRCLE ( 'NONE', #12479, 12.75000000000000178 ) ;
#42227 = DIRECTION ( 'NONE',  ( -1.000000000000000000, -0.000000000000000000, 0.000000000000000000 ) ) ;
#42228 = EDGE_CURVE ( 'NONE', #12898, #11089, #12323, .T. ) ;
#42229 = ORIENTED_EDGE ( 'NONE', *, *, #18876, .T. ) ;
#42230 = CARTESIAN_POINT ( 'NONE',  ( 3.152665057734079568, -2.258875078502220024, -7.609997527621126245 ) ) ;
#42231 = CYLINDRICAL_SURFACE ( 'NONE', #27883, 5.000000000000000000 ) ;
#42233 = ORIENTED_EDGE ( 'NONE', *, *, #8004, .F. ) ;
#42232 = AXIS2_PLACEMENT_3D ( 'NONE', #12502, #63699, #53757 ) ;
#42234 = CARTESIAN_POINT ( 'NONE',  ( 0.2651627682582922141, 11.47719223137565869, -4.271106202749156644 ) ) ;
#42235 = CARTESIAN_POINT ( 'NONE',  ( 15.30590914263659386, -29.00884126188377365, -11.24874127360776654 ) ) ;
#42236 = CARTESIAN_POINT ( 'NONE',  ( -37.25000000000000711, -1.853910857666116187E-16, -1.500000000000000222 ) ) ;
#42237 = VERTEX_POINT ( 'NONE', #11479 ) ;
#42238 = CIRCLE ( 'NONE', #18924, 4.999999999999999112 ) ;
#42239 = CARTESIAN_POINT ( 'NONE',  ( 17.05023968204110574, -34.50000000000000000, -4.356789313881336057 ) ) ;
#42240 = EDGE_LOOP ( 'NONE', ( #20777, #53211, #7587, #56370 ) ) ;
#42241 = EDGE_CURVE ( 'NONE', #53890, #8677, #58398, .T. ) ;
#42242 = DIRECTION ( 'NONE',  ( 0.000000000000000000, 0.01356324068817992175, -0.9999080150203990547 ) ) ;
#42243 = AXIS2_PLACEMENT_3D ( 'NONE', #18757, #22763, #43340 ) ;
#42244 = LINE ( 'NONE', #11674, #19186 ) ;
#42245 = CARTESIAN_POINT ( 'NONE',  ( 1.719304012340734822, -3.626341562669572305, -12.20344780066098345 ) ) ;
#42246 = LINE ( 'NONE', #41939, #30445 ) ;
#42247 = DIRECTION ( 'NONE',  ( 0.000000000000000000, -0.01356324068817992175, 0.9999080150203990547 ) ) ;
#42248 = CARTESIAN_POINT ( 'NONE',  ( 24.90079489126681977, -10.54408982692481977, -8.432554294912243620 ) ) ;
#42249 = DIRECTION ( 'NONE',  ( 0.000000000000000000, 0.01356324068818000848, -0.9999080150203990547 ) ) ;
#42250 = DIRECTION ( 'NONE',  ( 0.000000000000000000, 0.01356324068817998940, -0.9999080150203990547 ) ) ;
#42251 = ORIENTED_EDGE ( 'NONE', *, *, #35784, .F. ) ;
#42252 = EDGE_CURVE ( 'NONE', #31959, #65704, #9559, .T. ) ;
#42253 = DIRECTION ( 'NONE',  ( 0.000000000000000000, -0.3193015301359669600, -0.9476531711828067861 ) ) ;
#42254 = ORIENTED_EDGE ( 'NONE', *, *, #58754, .F. ) ;
#42255 = CARTESIAN_POINT ( 'NONE',  ( 5.530133899448235191, 0.01550764871776215935, 0.003876417824003496135 ) ) ;
#42256 = CARTESIAN_POINT ( 'NONE',  ( 2.263328370259784172, 6.687792802425356342, 3.697218830765363951 ) ) ;
#42257 = ORIENTED_EDGE ( 'NONE', *, *, #31788, .F. ) ;
#42258 = CARTESIAN_POINT ( 'NONE',  ( 1.633930747251838511, -12.68212725188740286, 0.7186603069036878733 ) ) ;
#42259 = CARTESIAN_POINT ( 'NONE',  ( 22.61491127797214062, 25.00000000000000000, 9.376349503825034404 ) ) ;
#42260 = DIRECTION ( 'NONE',  ( -1.000000000000000000, 0.000000000000000000, 0.000000000000000000 ) ) ;
#42261 = B_SPLINE_CURVE_WITH_KNOTS ( 'NONE', 3,
 ( #57533, #53537, #53850, #23251, #7980, #28246, #47872, #48540, #2990, #28561, #48863, #32237, #62822, #22259, #3318, #52554, #40157, #44491, #54169 ),
 .UNSPECIFIED., .F., .F.,
 ( 4, 3, 3, 3, 3, 3, 4 ),
 ( 7.884170296961029399E-18, 4.457896483014810721E-05, 6.639290541542139964E-05, 8.820687556478942857E-05, 0.0001100173248778936035, 0.0001545671401658124818, 0.0001830328308068588749 ),
 .UNSPECIFIED. ) ;
#42262 = ORIENTED_EDGE ( 'NONE', *, *, #18101, .T. ) ;
#42263 = EDGE_LOOP ( 'NONE', ( #36290, #28717, #55261, #45030 ) ) ;
#42264 = FACE_OUTER_BOUND ( 'NONE', #33469, .T. ) ;
#42265 = AXIS2_PLACEMENT_3D ( 'NONE', #58404, #47448, #62707 ) ;
#42266 = ORIENTED_EDGE ( 'NONE', *, *, #26475, .T. ) ;
#42267 = CARTESIAN_POINT ( 'NONE',  ( 3.152665057735657861, -7.609997527621795932, -2.258875078500884204 ) ) ;
#42268 = CARTESIAN_POINT ( 'NONE',  ( 35.00000000000000000, 4.705694406421931860E-17, -3.469127814946512892E-15 ) ) ;
#42269 = CARTESIAN_POINT ( 'NONE',  ( -35.00000000000000000, -2.968224442958318665, -11.81949347079750012 ) ) ;
#42270 = FACE_OUTER_BOUND ( 'NONE', #15463, .T. ) ;
#42271 = CARTESIAN_POINT ( 'NONE',  ( 2.889800649504073782, 6.039722463373554007, -0.9965440656173106815 ) ) ;
#42272 = VERTEX_POINT ( 'NONE', #47725 ) ;
#42273 = CARTESIAN_POINT ( 'NONE',  ( 5.514970785353741078, -0.004324946436530292468, 0.001897634820904997880 ) ) ;
#42274 = AXIS2_PLACEMENT_3D ( 'NONE', #50481, #4924, #64749 ) ;
#42275 = EDGE_CURVE ( 'NONE', #3924, #43734, #21301, .T. ) ;
#42276 = AXIS2_PLACEMENT_3D ( 'NONE', #9447, #15104, #45694 ) ;
#42277 = CARTESIAN_POINT ( 'NONE',  ( 1.719304012338836563, 0.7661785589583339773, 12.70777170743865980 ) ) ;
#42278 = DIRECTION ( 'NONE',  ( 0.000000000000000000, 0.9718671068226466536, -0.2355298848897482422 ) ) ;
#42280 = AXIS2_PLACEMENT_3D ( 'NONE', #59230, #20289, #19317 ) ;
#42279 = CARTESIAN_POINT ( 'NONE',  ( 37.00000000000000711, 12.18632975068352664, 0.06441628369840225743 ) ) ;
#42281 = CARTESIAN_POINT ( 'NONE',  ( 5.514624014163232779, -0.002216125254993689137, -0.003498325728817801728 ) ) ;
#42282 = CARTESIAN_POINT ( 'NONE',  ( 1.104777566491138785, 4.729982681549531165, 11.59867774809546148 ) ) ;
#42283 = LINE ( 'NONE', #58954, #34301 ) ;
#42284 = AXIS2_PLACEMENT_3D ( 'NONE', #38865, #38530, #8593 ) ;
#42285 = ADVANCED_FACE ( 'NONE', ( #53380 ), #7470, .T. ) ;
#42286 = ORIENTED_EDGE ( 'NONE', *, *, #18498, .F. ) ;
#42287 = CARTESIAN_POINT ( 'NONE',  ( 35.00000000000000000, 1.039216533672905785, -11.70009620280412221 ) ) ;
#42288 = CARTESIAN_POINT ( 'NONE',  ( 3.711556079772022176, -10.52777116167494675, 8.451878016623856738 ) ) ;
#42289 =( BOUNDED_CURVE ( )  B_SPLINE_CURVE ( 3, ( #23549, #24510, #19544, #33826 ),
 .UNSPECIFIED., .F., .F. ) 
 B_SPLINE_CURVE_WITH_KNOTS ( ( 4, 4 ),
 ( 3.747275043436211650, 3.808054268073822524 ),
 .UNSPECIFIED. ) 
 CURVE ( )  GEOMETRIC_REPRESENTATION_ITEM ( )  RATIONAL_B_SPLINE_CURVE ( ( 1.000000000000000000, 0.9996921808454459768, 0.9996921808454459768, 1.000000000000000000 ) ) 
 REPRESENTATION_ITEM ( '' )  );
#42290 = ORIENTED_EDGE ( 'NONE', *, *, #44484, .T. ) ;
#42291 = EDGE_CURVE ( 'NONE', #28521, #58714, #30830, .T. ) ;
#42292 = CARTESIAN_POINT ( 'NONE',  ( 1.719304012339819332, -7.581471372739574832, 10.22720798541442555 ) ) ;
#42293 = CARTESIAN_POINT ( 'NONE',  ( 1.020182472824409547, -9.280950437305058642, -8.370187102470554308 ) ) ;
#42294 = ORIENTED_EDGE ( 'NONE', *, *, #33182, .F. ) ;
#42295 = CARTESIAN_POINT ( 'NONE',  ( -35.00000000000000000, 7.718225330433806874, 9.430788938294076829 ) ) ;
#42296 = EDGE_CURVE ( 'NONE', #57422, #19640, #27427, .T. ) ;
#42297 = ORIENTED_EDGE ( 'NONE', *, *, #26904, .F. ) ;
#42298 = LINE ( 'NONE', #17053, #43377 ) ;
#42299 = VERTEX_POINT ( 'NONE', #43370 ) ;
#42300 = VERTEX_POINT ( 'NONE', #39049 ) ;
#42301 = DIRECTION ( 'NONE',  ( 1.000000000000000000, 0.000000000000000000, 0.000000000000000000 ) ) ;
#42302 = CIRCLE ( 'NONE', #3104, 5.000000000000000000 ) ;
#42303 = ADVANCED_FACE ( 'NONE', ( #42713 ), #22795, .T. ) ;
#42304 = EDGE_LOOP ( 'NONE', ( #1667, #13739, #58819, #43372 ) ) ;
#42305 = FACE_OUTER_BOUND ( 'NONE', #26379, .T. ) ;
#42306 = CARTESIAN_POINT ( 'NONE',  ( 0.000000000000000000, 5.860254403322073813, -3.474373880649762381 ) ) ;
#42307 = CYLINDRICAL_SURFACE ( 'NONE', #55652, 4.999999999999999112 ) ;
#42308 = DIRECTION ( 'NONE',  ( 0.000000000000000000, 0.000000000000000000, 1.000000000000000000 ) ) ;
#42309 = EDGE_LOOP ( 'NONE', ( #46029, #59271, #10708, #28674 ) ) ;
#42310 = CARTESIAN_POINT ( 'NONE',  ( 0.3675815128205894289, -7.689697408877338880, 9.574637318041938627 ) ) ;
#42311 = AXIS2_PLACEMENT_3D ( 'NONE', #512, #824, #26104 ) ;
#42312 = EDGE_CURVE ( 'NONE', #12370, #1280, #18123, .T. ) ;
#42313 = CARTESIAN_POINT ( 'NONE',  ( 7.919433923537877895, -32.26502814485947823, 12.92562328492908286 ) ) ;
#42314 = CARTESIAN_POINT ( 'NONE',  ( 1.937114397841932290, -7.182898292393840478, 10.63710405811931459 ) ) ;
#42316 = VERTEX_POINT ( 'NONE', #23434 ) ;
#42315 = CARTESIAN_POINT ( 'NONE',  ( -25.60894296954852223, 10.48177738153426830, 5.844539321404759846 ) ) ;
#42317 = DIRECTION ( 'NONE',  ( -1.000000000000000000, 0.000000000000000000, 0.000000000000000000 ) ) ;
#42318 = VERTEX_POINT ( 'NONE', #32414 ) ;
#42319 = CARTESIAN_POINT ( 'NONE',  ( 0.2652384529303148941, 9.338494547402500956, -7.922180393770576146 ) ) ;
#42320 = ORIENTED_EDGE ( 'NONE', *, *, #2793, .F. ) ;
#42321 = CARTESIAN_POINT ( 'NONE',  ( 21.46003464439880659, -11.46841712088275322, -3.538095200798918594 ) ) ;
#42322 = CARTESIAN_POINT ( 'NONE',  ( -35.00000000000000000, 10.43555801961483098, -5.391785509270847321 ) ) ;
#42323 = CIRCLE ( 'NONE', #49758, 4.999999999999999112 ) ;
#42324 = CARTESIAN_POINT ( 'NONE',  ( 35.00000000000000000, -11.16627499335657703, -3.645068577059991988 ) ) ;
#42325 = VERTEX_POINT ( 'NONE', #13129 ) ;
#42326 = CARTESIAN_POINT ( 'NONE',  ( 1.283627346226357879, 8.503905436511839611, 9.278077665801896856 ) ) ;
#42327 = CARTESIAN_POINT ( 'NONE',  ( 35.00000000000000000, 10.75351884295727345, -4.725891942574794058 ) ) ;
#42328 = LINE ( 'NONE', #28064, #24650 ) ;
#42330 = ORIENTED_EDGE ( 'NONE', *, *, #53517, .T. ) ;
#42329 = EDGE_CURVE ( 'NONE', #33526, #57232, #52069, .T. ) ;
#42331 = CIRCLE ( 'NONE', #9397, 12.18649999999999878 ) ;
#42332 = ORIENTED_EDGE ( 'NONE', *, *, #23821, .F. ) ;
#42333 = CARTESIAN_POINT ( 'NONE',  ( 0.2706063244538028933, 12.03021891034991064, 2.299194104693123020 ) ) ;
#42334 = VERTEX_POINT ( 'NONE', #59339 ) ;
#42335 = EDGE_CURVE ( 'NONE', #42786, #24439, #15970, .T. ) ;
#42336 = VECTOR ( 'NONE', #34181, 1000.000000000000000 ) ;
#42337 = ORIENTED_EDGE ( 'NONE', *, *, #46016, .F. ) ;
#42338 = DIRECTION ( 'NONE',  ( -1.000000000000000000, 0.000000000000000000, 0.000000000000000000 ) ) ;
#42339 = CARTESIAN_POINT ( 'NONE',  ( 1.104777566491149221, -10.60111489796739193, 6.672212870706169419 ) ) ;
#42340 = CARTESIAN_POINT ( 'NONE',  ( 2.241449424704145876, -7.194804211893830015, -2.553400830064051164 ) ) ;
#42341 = CARTESIAN_POINT ( 'NONE',  ( 35.00000000000000000, -1.903127969211267700, -11.59095880812007628 ) ) ;
#42342 = DIRECTION ( 'NONE',  ( -1.000000000000000000, 0.000000000000000000, 0.000000000000000000 ) ) ;
#42343 = FACE_OUTER_BOUND ( 'NONE', #9223, .T. ) ;
#42344 = CARTESIAN_POINT ( 'NONE',  ( -22.27722019117889474, -0.6494988092404023750, -3.623917154020615428 ) ) ;
#42345 = VERTEX_POINT ( 'NONE', #59033 ) ;
#42346 = CARTESIAN_POINT ( 'NONE',  ( 2.000000000000001776, -5.662015959325215952, 4.918493191653933394 ) ) ;
#42347 = EDGE_CURVE ( 'NONE', #21730, #46798, #55207, .T. ) ;
#42348 = CARTESIAN_POINT ( 'NONE',  ( 0.2676618633000484859, 4.339362305359601990, -11.45242956837282655 ) ) ;
#42349 = EDGE_CURVE ( 'NONE', #44279, #2026, #17033, .T. ) ;
#42350 = DIRECTION ( 'NONE',  ( 1.000000000000000000, -0.000000000000000000, 0.000000000000000000 ) ) ;
#42351 = CIRCLE ( 'NONE', #46609, 12.18650000000000233 ) ;
#42352 = CARTESIAN_POINT ( 'NONE',  ( -47.00000000000000711, 0.000000000000000000, 0.000000000000000000 ) ) ;
#42353 = VECTOR ( 'NONE', #2668, 999.9999999999998863 ) ;
#42354 = CARTESIAN_POINT ( 'NONE',  ( 0.2652384529303158933, 12.04846370803831412, -2.191562200667060978 ) ) ;
#42355 = CARTESIAN_POINT ( 'NONE',  ( 11.12233887262441279, 0.3490535524848530358, -11.99560895363750923 ) ) ;
#42356 = ORIENTED_EDGE ( 'NONE', *, *, #29940, .T. ) ;
#42357 = DIRECTION ( 'NONE',  ( 0.000000000000000000, 0.9970832820307041766, 0.07632122047556143263 ) ) ;
#42358 = CARTESIAN_POINT ( 'NONE',  ( 0.2648978790185584908, -1.996248716311547433, -12.08224454301450734 ) ) ;
#42359 = CARTESIAN_POINT ( 'NONE',  ( 35.00000000000000000, 1.591260454995240714, -12.08216339958901564 ) ) ;
#42360 = ADVANCED_FACE ( 'NONE', ( #60642 ), #59673, .T. ) ;
#42361 = CARTESIAN_POINT ( 'NONE',  ( 2.305787727787084407, -1.493241775258372872, -7.508843116234172221 ) ) ;
#42362 = CIRCLE ( 'NONE', #60428, 5.000000000000000888 ) ;
#42363 = ADVANCED_FACE ( 'NONE', ( #20411 ), #29397, .T. ) ;
#42364 = CARTESIAN_POINT ( 'NONE',  ( -36.00000000000000711, -6.950793414699719008, -10.68873102412850074 ) ) ;
#42365 = CARTESIAN_POINT ( 'NONE',  ( 35.00000000000000000, 4.705694406421931860E-17, -3.469127814946512892E-15 ) ) ;
#42366 = AXIS2_PLACEMENT_3D ( 'NONE', #3005, #18295, #63813 ) ;
#42367 = VERTEX_POINT ( 'NONE', #4481 ) ;
#42368 = DIRECTION ( 'NONE',  ( 0.000000000000000000, 0.01356324068817998940, -0.9999080150203990547 ) ) ;
#42369 = CARTESIAN_POINT ( 'NONE',  ( -35.00000000000000000, 0.000000000000000000, 0.000000000000000000 ) ) ;
#42370 = LINE ( 'NONE', #57715, #59716 ) ;
#42371 = CARTESIAN_POINT ( 'NONE',  ( 1.459561108993789880, -12.54631635028882286, -1.570807238540975037 ) ) ;
#42372 = ORIENTED_EDGE ( 'NONE', *, *, #4121, .F. ) ;
#42373 = CARTESIAN_POINT ( 'NONE',  ( -37.00000000000000711, 0.000000000000000000, 0.000000000000000000 ) ) ;
#42374 = CARTESIAN_POINT ( 'NONE',  ( 0.2646305136544072623, -10.67138229758225343, -6.008537389229529957 ) ) ;
#42375 = EDGE_CURVE ( 'NONE', #33979, #11407, #23406, .T. ) ;
#42376 = CIRCLE ( 'NONE', #53038, 12.74999999999999822 ) ;
#42378 = VERTEX_POINT ( 'NONE', #45674 ) ;
#42377 = CARTESIAN_POINT ( 'NONE',  ( -35.00000000000000000, 11.29812557209476864, 3.213188559034282132 ) ) ;
#42379 = DIRECTION ( 'NONE',  ( -1.000000000000000000, -0.000000000000000000, -0.000000000000000000 ) ) ;
#42380 = CARTESIAN_POINT ( 'NONE',  ( 2.000000000000001776, -1.865193240757140991, 6.552473556515165498 ) ) ;
#42381 = VERTEX_POINT ( 'NONE', #40345 ) ;
#42382 = CARTESIAN_POINT ( 'NONE',  ( -35.00000000000000000, 6.102719229070827645, -10.54834585426213422 ) ) ;
#42383 = DIRECTION ( 'NONE',  ( 1.000000000000000000, -0.000000000000000000, 0.000000000000000000 ) ) ;
#42384 = CARTESIAN_POINT ( 'NONE',  ( 2.241537034860907607, 7.519304283075095796, -1.321063441155912788 ) ) ;
#42385 = CARTESIAN_POINT ( 'NONE',  ( 2.941278708680199916, -1.972702289976042023, 5.814102272488581136 ) ) ;
#42386 = FACE_OUTER_BOUND ( 'NONE', #64661, .T. ) ;
#42387 = EDGE_CURVE ( 'NONE', #11516, #48650, #49396, .T. ) ;
#42388 = DIRECTION ( 'NONE',  ( 0.000000000000000000, 0.5472293298355273006, -0.8369827122275343978 ) ) ;
#42390 = VERTEX_POINT ( 'NONE', #45028 ) ;
#42389 = DIRECTION ( 'NONE',  ( -1.000000000000000000, 0.000000000000000000, 0.000000000000000000 ) ) ;
#42391 = CARTESIAN_POINT ( 'NONE',  ( -22.27722015946439171, 2.356370737780168589, 2.828901469906451194 ) ) ;
#42392 = EDGE_CURVE ( 'NONE', #49156, #40383, #35016, .T. ) ;
#42393 = ORIENTED_EDGE ( 'NONE', *, *, #49302, .T. ) ;
#42394 = DIRECTION ( 'NONE',  ( 0.000000000000000000, 0.1387779952735818945, -0.9903235168508549569 ) ) ;
#42395 = EDGE_LOOP ( 'NONE', ( #19472, #65193, #49375, #43832 ) ) ;
#42396 = SHAPE_DEFINITION_REPRESENTATION ( #18496, #63658 ) ;
#42397 = FACE_OUTER_BOUND ( 'NONE', #21923, .T. ) ;
#42398 = EDGE_CURVE ( 'NONE', #15301, #42144, #2179, .T. ) ;
#42399 = CARTESIAN_POINT ( 'NONE',  ( 2.889800649504073782, 3.882893708502110908, -4.732281052280274736 ) ) ;
#42400 = AXIS2_PLACEMENT_3D ( 'NONE', #21876, #38120, #2245 ) ;
#42401 = DIRECTION ( 'NONE',  ( -1.000000000000000000, -0.000000000000000000, -0.000000000000000000 ) ) ;
#42402 = EDGE_CURVE ( 'NONE', #43073, #32242, #15083, .T. ) ;
#42403 = CARTESIAN_POINT ( 'NONE',  ( -27.08429572838383947, 0.9410937941434112108, -2.089332284968719922 ) ) ;
#42404 = VERTEX_POINT ( 'NONE', #25079 ) ;
#42405 = CARTESIAN_POINT ( 'NONE',  ( -24.89073217517900360, -5.758728772039412469, 10.56290472577202522 ) ) ;
#42406 = AXIS2_PLACEMENT_3D ( 'NONE', #50341, #10390, #56628 ) ;
#42407 = CARTESIAN_POINT ( 'NONE',  ( 0.2851083653049530375, -0.4107471485392680810, -13.49374991542258151 ) ) ;
#42408 = EDGE_LOOP ( 'NONE', ( #22091, #34705, #56183, #33989 ) ) ;
#42409 = ORIENTED_EDGE ( 'NONE', *, *, #28085, .T. ) ;
#42410 = ADVANCED_FACE ( 'NONE', ( #44354 ), #19101, .T. ) ;
#42411 = DIRECTION ( 'NONE',  ( -1.000000000000000000, 0.000000000000000000, 0.000000000000000000 ) ) ;
#42412 = EDGE_LOOP ( 'NONE', ( #63143, #53487, #12307, #23695, #46815, #48897 ) ) ;
#42413 = DIRECTION ( 'NONE',  ( 1.000000000000000000, 0.000000000000000000, 0.000000000000000000 ) ) ;
#42414 = CARTESIAN_POINT ( 'NONE',  ( 12.49336350054390365, 0.1658493928153598473, 11.99999999999999645 ) ) ;
#42416 = AXIS2_PLACEMENT_3D ( 'NONE', #29898, #30236, #50851 ) ;
#42415 = FACE_OUTER_BOUND ( 'NONE', #12740, .T. ) ;
#42417 = DIRECTION ( 'NONE',  ( 1.000000000000000000, 0.000000000000000000, 0.000000000000000000 ) ) ;
#42418 = DIRECTION ( 'NONE',  ( 1.000000000000000000, -0.000000000000000000, -0.000000000000000000 ) ) ;
#42419 = CARTESIAN_POINT ( 'NONE',  ( 35.00000000000000000, 4.705694406421931860E-17, -3.469127814946512892E-15 ) ) ;
#42420 = CIRCLE ( 'NONE', #13757, 2.899999999999995470 ) ;
#42421 = ORIENTED_EDGE ( 'NONE', *, *, #14981, .F. ) ;
#42422 = CARTESIAN_POINT ( 'NONE',  ( 1.719304012338199517, 0.000000000000000000, 0.000000000000000000 ) ) ;
#42423 = ORIENTED_EDGE ( 'NONE', *, *, #29284, .F. ) ;
#42424 = FACE_OUTER_BOUND ( 'NONE', #8871, .T. ) ;
#42425 = CARTESIAN_POINT ( 'NONE',  ( -9.129631415690074192, -12.73028175706349430, -4.506864653171657409 ) ) ;
#42426 = CARTESIAN_POINT ( 'NONE',  ( 2.242819959140646802, -3.905785747113969641, 6.560218843829765056 ) ) ;
#42427 = B_SPLINE_CURVE_WITH_KNOTS ( 'NONE', 3,
 ( #60792, #9566, #65432, #45482, #65747, #20219, #40496, #15229, #35512, #55811, #10237, #30514, #40841, #50817, #25533, #21875 ),
 .UNSPECIFIED., .F., .F.,
 ( 4, 3, 3, 3, 3, 4 ),
 ( 2.346432215325189512E-15, 0.0002126834539179932228, 0.0004253519300366710764, 0.0006380165497224839352, 0.0007442707582429045543, 0.0009453531351412929181 ),
 .UNSPECIFIED. ) ;
#42428 = CIRCLE ( 'NONE', #40349, 6.936499999999989896 ) ;
#42429 = DIRECTION ( 'NONE',  ( -1.000000000000000000, 0.000000000000000000, 0.000000000000000000 ) ) ;
#42430 = ORIENTED_EDGE ( 'NONE', *, *, #16819, .T. ) ;
#42431 = EDGE_CURVE ( 'NONE', #16656, #57717, #4463, .T. ) ;
#42432 = ORIENTED_EDGE ( 'NONE', *, *, #45930, .T. ) ;
#42433 = CARTESIAN_POINT ( 'NONE',  ( -2.952869152607107139, 12.96714474214482138, 3.755417052241487585 ) ) ;
#42434 = EDGE_CURVE ( 'NONE', #57088, #61909, #45247, .T. ) ;
#42435 = VERTEX_POINT ( 'NONE', #32571 ) ;
#42436 = FACE_OUTER_BOUND ( 'NONE', #61000, .T. ) ;
#42437 = DIRECTION ( 'NONE',  ( -1.000000000000000000, -0.000000000000000000, 0.000000000000000000 ) ) ;
#42438 = CARTESIAN_POINT ( 'NONE',  ( 5.515539859299206427, 0.005751553894235443033, 0.001886660928063796675 ) ) ;
#42439 = CARTESIAN_POINT ( 'NONE',  ( 2.259830038564998755, 1.462175769136944581, -7.499347412930710277 ) ) ;
#42440 = ORIENTED_EDGE ( 'NONE', *, *, #11273, .F. ) ;
#42441 = CARTESIAN_POINT ( 'NONE',  ( 0.2647959493198550618, 12.08462848595695149, 1.981611532097588446 ) ) ;
#42442 = CARTESIAN_POINT ( 'NONE',  ( 2.000000000000001776, 0.000000000000000000, 0.000000000000000000 ) ) ;
#42443 = ADVANCED_FACE ( 'NONE', ( #53212 ), #13011, .F. ) ;
#42444 = CARTESIAN_POINT ( 'NONE',  ( -26.74023318801843985, 0.2829279580742273259, -3.342010596062600758 ) ) ;
#42445 = LINE ( 'NONE', #57793, #62472 ) ;
#42446 = AXIS2_PLACEMENT_3D ( 'NONE', #42210, #16963, #7300 ) ;
#42447 = CIRCLE ( 'NONE', #13788, 5.000000000000000888 ) ;
#42448 = CARTESIAN_POINT ( 'NONE',  ( -35.00000000000000000, 0.000000000000000000, 0.000000000000000000 ) ) ;
#42449 = CARTESIAN_POINT ( 'NONE',  ( -35.00000000000000000, 0.000000000000000000, 0.000000000000000000 ) ) ;
#42450 = VERTEX_POINT ( 'NONE', #46344 ) ;
#42451 = CARTESIAN_POINT ( 'NONE',  ( -16.37486794060187734, -28.33944867960597236, -9.978426449060183501 ) ) ;
#42452 = ORIENTED_EDGE ( 'NONE', *, *, #14596, .T. ) ;
#42453 = CARTESIAN_POINT ( 'NONE',  ( -37.00000000000000711, -1.771820996347237331, 11.61175578952785692 ) ) ;
#42454 = CARTESIAN_POINT ( 'NONE',  ( 2.034671305880519476, 11.35598636043232190, 2.716450156983679420 ) ) ;
#42455 = CARTESIAN_POINT ( 'NONE',  ( -35.00000000000000000, 0.000000000000000000, 0.000000000000000000 ) ) ;
#42456 = EDGE_CURVE ( 'NONE', #5624, #35473, #36, .T. ) ;
#42457 = CARTESIAN_POINT ( 'NONE',  ( 1.462291587748163257, 12.62932306616532152, 0.6330131614645532201 ) ) ;
#42458 = ADVANCED_FACE ( 'NONE', ( #2359 ), #37201, .T. ) ;
#42459 = CARTESIAN_POINT ( 'NONE',  ( 0.2759803524722214130, -11.57441428600635902, 4.011137970318905843 ) ) ;
#42460 = AXIS2_PLACEMENT_3D ( 'NONE', #34148, #19850, #29184 ) ;
#42461 = B_SPLINE_CURVE_WITH_KNOTS ( 'NONE', 3,
 ( #42800, #17552, #46573, #43123, #58790, #18205, #2608, #36256, #41240, #3246, #8218, #61524, #13209, #37822, #7905, #6349 ),
 .UNSPECIFIED., .F., .F.,
 ( 4, 3, 3, 3, 3, 4 ),
 ( 0.000000000000000000, 6.991367980366399674E-05, 0.0001398269368981363962, 0.0002097400188389094984, 0.0002811534801551362150, 0.0003526297678872492578 ),
 .UNSPECIFIED. ) ;
#42462 = ORIENTED_EDGE ( 'NONE', *, *, #6213, .F. ) ;
#42463 = VERTEX_POINT ( 'NONE', #31369 ) ;
#42464 = CARTESIAN_POINT ( 'NONE',  ( -35.00000000000000000, 0.000000000000000000, 0.000000000000000000 ) ) ;
#42465 = ORIENTED_EDGE ( 'NONE', *, *, #20060, .T. ) ;
#42466 = AXIS2_PLACEMENT_3D ( 'NONE', #44769, #3604, #34774 ) ;
#42467 = CARTESIAN_POINT ( 'NONE',  ( 3.243709820962341617, 4.721130720727682473, 11.04021256742971069 ) ) ;
#42468 = CARTESIAN_POINT ( 'NONE',  ( -22.27384469013076185, 3.358914544760244869, 1.508555848190743287 ) ) ;
#42469 = CARTESIAN_POINT ( 'NONE',  ( 1.719304012342639965, 12.38166659047149487, -2.961219984262613458 ) ) ;
#42470 = CARTESIAN_POINT ( 'NONE',  ( 35.00000000000000000, 4.705694406421931860E-17, -3.469127814946512892E-15 ) ) ;
#42471 = DIRECTION ( 'NONE',  ( -1.000000000000000000, 0.000000000000000000, -0.000000000000000000 ) ) ;
#42472 = CARTESIAN_POINT ( 'NONE',  ( 2.266490820343226797, 7.550546162186920540, 1.183790889241755018 ) ) ;
#42473 = CARTESIAN_POINT ( 'NONE',  ( -37.00000000000000711, 10.80631716521666874, 4.603882218679588689 ) ) ;
#42474 = ORIENTED_EDGE ( 'NONE', *, *, #25581, .T. ) ;
#42475 = ORIENTED_EDGE ( 'NONE', *, *, #63768, .F. ) ;
#42476 = CARTESIAN_POINT ( 'NONE',  ( 3.152665057734113319, -5.461013642405577073, 5.761241965769066553 ) ) ;
#42477 = AXIS2_PLACEMENT_3D ( 'NONE', #59066, #13474, #33757 ) ;
#42478 = ORIENTED_EDGE ( 'NONE', *, *, #23791, .T. ) ;
#42479 =( LENGTH_UNIT ( ) NAMED_UNIT ( * ) SI_UNIT ( .MILLI., .METRE. ) );
#42480 = EDGE_CURVE ( 'NONE', #33417, #49413, #45705, .T. ) ;
#42481 = CARTESIAN_POINT ( 'NONE',  ( 24.16730227909621220, -10.72488973065076223, -8.203994665790906637 ) ) ;
#42482 = CYLINDRICAL_SURFACE ( 'NONE', #64015, 4.999999999999999112 ) ;
#42483 = EDGE_CURVE ( 'NONE', #24280, #19299, #9149, .T. ) ;
#42484 = CARTESIAN_POINT ( 'NONE',  ( -35.00000000000000000, 0.000000000000000000, 0.000000000000000000 ) ) ;
#42485 = VERTEX_POINT ( 'NONE', #15418 ) ;
#42487 = CARTESIAN_POINT ( 'NONE',  ( 0.3665391374699465965, -0.2638605131386297376, -12.27992639892678639 ) ) ;
#42486 = AXIS2_PLACEMENT_3D ( 'NONE', #50300, #43643, #59607 ) ;
#42488 = CARTESIAN_POINT ( 'NONE',  ( -13.40508024069041326, -30.08919203117021368, -6.920461462856672519 ) ) ;
#42489 = CARTESIAN_POINT ( 'NONE',  ( 2.080613030138687147, 0.000000000000000000, -7.580821595991582562 ) ) ;
#42490 = ORIENTED_EDGE ( 'NONE', *, *, #17201, .F. ) ;
#42491 = EDGE_LOOP ( 'NONE', ( #56482, #33681, #49079, #14578 ) ) ;
#42492 = EDGE_CURVE ( 'NONE', #58003, #14898, #39291, .T. ) ;
#42493 = VERTEX_POINT ( 'NONE', #477 ) ;
#42494 = ORIENTED_EDGE ( 'NONE', *, *, #57016, .F. ) ;
#42495 = CARTESIAN_POINT ( 'NONE',  ( 25.05309951391468459, -10.77522019223763827, -8.132934882857099979 ) ) ;
#42496 = ORIENTED_EDGE ( 'NONE', *, *, #19598, .T. ) ;
#42497 = EDGE_LOOP ( 'NONE', ( #41911, #41268, #29276, #696 ) ) ;
#42498 = PLANE ( 'NONE',  #32000 ) ;
#42499 = CARTESIAN_POINT ( 'NONE',  ( -1.318817192132426526E-11, -30.53649492335491544, -15.30974548841782834 ) ) ;
#42500 = AXIS2_PLACEMENT_3D ( 'NONE', #42449, #37817, #62748 ) ;
#42502 = CIRCLE ( 'NONE', #51034, 5.000000000000000888 ) ;
#42501 = DIRECTION ( 'NONE',  ( -1.000000000000000000, 0.000000000000000000, 0.000000000000000000 ) ) ;
#42503 = CIRCLE ( 'NONE', #22338, 12.75000000000000178 ) ;
#42504 = CARTESIAN_POINT ( 'NONE',  ( 2.241311220309555985, 2.698144003944889846, -7.141707286456099091 ) ) ;
#42505 = CARTESIAN_POINT ( 'NONE',  ( -35.00000000000000000, 3.645068577060182946, -11.16627499335651130 ) ) ;
#42506 = CARTESIAN_POINT ( 'NONE',  ( -37.00000000000000711, 12.05416472667165806, 1.791059740004466994 ) ) ;
#42507 = ORIENTED_EDGE ( 'NONE', *, *, #35778, .F. ) ;
#42508 =( BOUNDED_SURFACE ( )  B_SPLINE_SURFACE ( 3, 1, ( 
 ( #13177, #13481 ),
 ( #8184, #38098 ),
 ( #39412, #28456 ),
 ( #28146, #54068 ) ),
 .UNSPECIFIED., .F., .F., .F. ) 
 B_SPLINE_SURFACE_WITH_KNOTS ( ( 4, 4 ),
 ( 2, 2 ),
 ( 0.000000000000000000, 1.000000000000000000 ),
 ( 0.000000000000000000, 1.000000000000000000 ),
 .UNSPECIFIED. ) 
 GEOMETRIC_REPRESENTATION_ITEM ( )  RATIONAL_B_SPLINE_SURFACE ( (
 ( 1.000000000000000000, 1.000000000000000000),
 ( 0.9942764183789327692, 0.8450855930916585379),
 ( 0.9942764183789327692, 0.8450855930916585379),
 ( 1.000000000000000000, 1.000000000000000000) ) ) 
 REPRESENTATION_ITEM ( '' )  SURFACE ( )  );
#42509 = CARTESIAN_POINT ( 'NONE',  ( -35.00000000000000000, 0.4993900848167411310, 12.17626345777664021 ) ) ;
#42510 = CARTESIAN_POINT ( 'NONE',  ( 2.770579946183230113, 4.784693811915898820, 6.173813901927509562 ) ) ;
#42511 = DIRECTION ( 'NONE',  ( -1.000000000000000000, 0.000000000000000000, 0.000000000000000000 ) ) ;
#42512 = CARTESIAN_POINT ( 'NONE',  ( 2.000000000000001776, 0.000000000000000000, 0.000000000000000000 ) ) ;
#42513 = LINE ( 'NONE', #58855, #54164 ) ;
#42514 = CARTESIAN_POINT ( 'NONE',  ( 0.3341166715381381214, -11.61315925169691177, -3.958014133396720702 ) ) ;
#42515 = CIRCLE ( 'NONE', #13840, 2.899999999999995026 ) ;
#42516 = VERTEX_POINT ( 'NONE', #20744 ) ;
#42517 = DIRECTION ( 'NONE',  ( 0.000000000000000000, 0.1740410799127543318, 0.9847383929261630531 ) ) ;
#42518 = VECTOR ( 'NONE', #46158, 1000.000000000000000 ) ;
#42519 = AXIS2_PLACEMENT_3D ( 'NONE', #48158, #44427, #7565 ) ;
#42520 = ADVANCED_FACE ( 'NONE', ( #41013 ), #29137, .F. ) ;
#42521 = ORIENTED_EDGE ( 'NONE', *, *, #60686, .T. ) ;
#42522 = CARTESIAN_POINT ( 'NONE',  ( 1.948354844646956963, 4.761851831282559289, 10.97658859989492086 ) ) ;
#42523 = CARTESIAN_POINT ( 'NONE',  ( 2.284126774967658147, 5.959830409747719493, -4.793997684221303679 ) ) ;
#42524 = CARTESIAN_POINT ( 'NONE',  ( 9.575800908719084958, -13.45729701195359240, -1.072919909436246266 ) ) ;
#42525 = CARTESIAN_POINT ( 'NONE',  ( -27.09229696323320624, -0.6397626223479085938, -2.225368503508858620 ) ) ;
#42526 = CARTESIAN_POINT ( 'NONE',  ( 2.276198483117258586, -6.697332984100285991, 3.688810392808530736 ) ) ;
#42527 = ORIENTED_EDGE ( 'NONE', *, *, #46278, .F. ) ;
#42528 = DIRECTION ( 'NONE',  ( -1.000000000000000000, 0.000000000000000000, 0.000000000000000000 ) ) ;
#42530 = CIRCLE ( 'NONE', #2217, 5.000000000000000000 ) ;
#42529 = DIRECTION ( 'NONE',  ( 0.000000000000000000, 0.3218879778915904044, -0.9467777615094594701 ) ) ;
#42531 = DIRECTION ( 'NONE',  ( 0.000000000000000000, 0.000000000000000000, 1.000000000000000000 ) ) ;
#42532 = DIRECTION ( 'NONE',  ( 0.000000000000000000, -0.01356324068817999114, 0.9999080150203989437 ) ) ;
#42533 = DIRECTION ( 'NONE',  ( -1.000000000000000000, 0.000000000000000000, -0.000000000000000000 ) ) ;
#42534 = VERTEX_POINT ( 'NONE', #53559 ) ;
#42535 = DIRECTION ( 'NONE',  ( 0.3865475372811021382, 0.7888450329201709410, 0.4778122177792122338 ) ) ;
#42536 = CIRCLE ( 'NONE', #27650, 5.000000000000001776 ) ;
#42538 = ADVANCED_FACE ( 'NONE', ( #24250 ), #8639, .T. ) ;
#42537 = FACE_OUTER_BOUND ( 'NONE', #59493, .T. ) ;
#42539 = EDGE_CURVE ( 'NONE', #49728, #57334, #10659, .T. ) ;
#42540 = AXIS2_PLACEMENT_3D ( 'NONE', #60378, #55399, #45747 ) ;
#42541 = AXIS2_PLACEMENT_3D ( 'NONE', #59480, #34830, #3962 ) ;
#42542 = CIRCLE ( 'NONE', #54268, 12.73084802173761787 ) ;
#42543 = ORIENTED_EDGE ( 'NONE', *, *, #54505, .F. ) ;
#42544 = ORIENTED_EDGE ( 'NONE', *, *, #7352, .F. ) ;
#42545 = CARTESIAN_POINT ( 'NONE',  ( 5.516018279890452902, -0.005042957932159101465, -0.004525000489649917343 ) ) ;
#42546 = VECTOR ( 'NONE', #33034, 1000.000000000000000 ) ;
#42547 = LINE ( 'NONE', #58890, #40665 ) ;
#42548 = CARTESIAN_POINT ( 'NONE',  ( 1.014383007554957139, -7.686901933424216793, 9.851867765302158020 ) ) ;
#42549 = DIRECTION ( 'NONE',  ( 1.000000000000000000, 0.000000000000000000, 0.000000000000000000 ) ) ;
#42550 = ORIENTED_EDGE ( 'NONE', *, *, #52846, .T. ) ;
#42551 = ORIENTED_EDGE ( 'NONE', *, *, #39453, .T. ) ;
#42552 = ORIENTED_EDGE ( 'NONE', *, *, #50573, .T. ) ;
#42553 = CARTESIAN_POINT ( 'NONE',  ( 2.305787727787084407, 7.654065630109506913, 0.1666591538752955071 ) ) ;
#42554 = AXIS2_PLACEMENT_3D ( 'NONE', #21590, #16596, #57164 ) ;
#42555 = EDGE_CURVE ( 'NONE', #36274, #44559, #49677, .T. ) ;
#42556 = AXIS2_PLACEMENT_3D ( 'NONE', #7353, #27636, #63219 ) ;
#42557 = CARTESIAN_POINT ( 'NONE',  ( -27.45775109278350712, 13.35262336282554152, -1.989333891161978674 ) ) ;
#42558 = ORIENTED_EDGE ( 'NONE', *, *, #64051, .T. ) ;
#42559 = CYLINDRICAL_SURFACE ( 'NONE', #32566, 12.18650000000000055 ) ;
#42560 = VECTOR ( 'NONE', #20132, 1000.000000000000000 ) ;
#42561 = CARTESIAN_POINT ( 'NONE',  ( -22.30078715814471835, -0.2606204736986897363, -3.743307663037647615 ) ) ;
#42562 = ORIENTED_EDGE ( 'NONE', *, *, #17215, .F. ) ;
#42563 = CARTESIAN_POINT ( 'NONE',  ( -27.08419797710328680, -0.3221715127607973628, -2.268561579780439708 ) ) ;
#42564 = CARTESIAN_POINT ( 'NONE',  ( 35.00000000000000000, 1.030638227056565048, -12.14284015767850278 ) ) ;
#42565 = CARTESIAN_POINT ( 'NONE',  ( 35.00000000000000000, -11.68758509253247091, 1.171570255487570655 ) ) ;
#42566 = ORIENTED_EDGE ( 'NONE', *, *, #7281, .F. ) ;
#42567 = CIRCLE ( 'NONE', #18206, 2.899999999999994582 ) ;
#42568 = ORIENTED_EDGE ( 'NONE', *, *, #63706, .F. ) ;
#42569 = DIRECTION ( 'NONE',  ( 0.000000000000000000, 0.000000000000000000, 1.000000000000000000 ) ) ;
#42570 = VERTEX_POINT ( 'NONE', #63491 ) ;
#42571 = CARTESIAN_POINT ( 'NONE',  ( 2.000000000000001776, 2.562706407243636075, 6.312399813420339179 ) ) ;
#42572 = CIRCLE ( 'NONE', #55366, 5.000000000000000000 ) ;
#42573 = CARTESIAN_POINT ( 'NONE',  ( -35.00000000000000000, 0.000000000000000000, 0.000000000000000000 ) ) ;
#42574 = DIRECTION ( 'NONE',  ( 0.000000000000000000, 0.01356324068817998940, -0.9999080150203990547 ) ) ;
#42575 = ADVANCED_FACE ( 'NONE', ( #43217 ), #3986, .T. ) ;
#42576 = LINE ( 'NONE', #1726, #58092 ) ;
#42577 = CARTESIAN_POINT ( 'NONE',  ( 19.56743653832047158, -33.00000000000000000, -5.000000000000017764 ) ) ;
#42578 = DIRECTION ( 'NONE',  ( -1.000000000000000000, 0.000000000000000000, 0.000000000000000000 ) ) ;
#42579 = CARTESIAN_POINT ( 'NONE',  ( -29.92777678363736626, -3.750539801530011985, -12.96855624952674724 ) ) ;
#42580 = CARTESIAN_POINT ( 'NONE',  ( 6.432001473550251092, -8.074322192336737203, -8.885343091696837448 ) ) ;
#42581 = ORIENTED_EDGE ( 'NONE', *, *, #50672, .T. ) ;
#42582 = FACE_OUTER_BOUND ( 'NONE', #44575, .T. ) ;
#42583 = VECTOR ( 'NONE', #4344, 1000.000000000000000 ) ;
#42584 = ORIENTED_EDGE ( 'NONE', *, *, #47962, .F. ) ;
#42585 = DIRECTION ( 'NONE',  ( 0.000000000000000000, 0.000000000000000000, 1.000000000000000000 ) ) ;
#42586 = CARTESIAN_POINT ( 'NONE',  ( 2.259025283526324479, 6.683966451871405035, 3.701170455112714475 ) ) ;
#42587 = AXIS2_PLACEMENT_3D ( 'NONE', #47415, #37411, #62346 ) ;
#42588 = ORIENTED_EDGE ( 'NONE', *, *, #53900, .T. ) ;
#42589 = DIRECTION ( 'NONE',  ( -1.000000000000000000, 0.000000000000000000, 0.000000000000000000 ) ) ;
#42590 = CARTESIAN_POINT ( 'NONE',  ( 0.3164563675027631806, 12.03284811452140346, -2.365891945210687020 ) ) ;
#42591 = CARTESIAN_POINT ( 'NONE',  ( -35.00000000000000000, 8.352657516904674395, 8.258652103341463047 ) ) ;
#42592 = ORIENTED_EDGE ( 'NONE', *, *, #17599, .F. ) ;
#42593 = AXIS2_PLACEMENT_3D ( 'NONE', #40765, #34761, #55063 ) ;
#42594 = ORIENTED_EDGE ( 'NONE', *, *, #8566, .T. ) ;
#42595 = DIRECTION ( 'NONE',  ( -1.000000000000000000, 0.000000000000000000, 0.000000000000000000 ) ) ;
#42596 = EDGE_CURVE ( 'NONE', #49507, #55512, #19276, .T. ) ;
#42597 = ORIENTED_EDGE ( 'NONE', *, *, #3335, .T. ) ;
#42598 = CARTESIAN_POINT ( 'NONE',  ( 2.931247277082670077, -6.255823895766985387, 4.765826751677415984 ) ) ;
#42599 = CARTESIAN_POINT ( 'NONE',  ( -27.08419797710328325, 2.125717714519606449, 0.8552720754636790046 ) ) ;
#42600 = ADVANCED_FACE ( 'NONE', ( #12970 ), #23276, .T. ) ;
#42601 = CARTESIAN_POINT ( 'NONE',  ( 35.00000000000000000, -11.73808581813437613, 0.4353888892049613824 ) ) ;
#42602 = DIRECTION ( 'NONE',  ( 0.000000000000000000, 0.01356324068817992175, -0.9999080150203990547 ) ) ;
#42603 = VERTEX_POINT ( 'NONE', #13302 ) ;
#42604 = CARTESIAN_POINT ( 'NONE',  ( 0.2638984909335716500, 12.02508546958696911, 2.322601104020707741 ) ) ;
#42605 = AXIS2_PLACEMENT_3D ( 'NONE', #6800, #1810, #8106 ) ;
#42606 = AXIS2_PLACEMENT_3D ( 'NONE', #24318, #9333, #14338 ) ;
#42607 = EDGE_CURVE ( 'NONE', #1074, #63071, #11705, .T. ) ;
#42608 = CIRCLE ( 'NONE', #31986, 4.999999999999999112 ) ;
#42609 = CARTESIAN_POINT ( 'NONE',  ( 11.20797324838622444, -27.95044230146133302, -13.82289656124156885 ) ) ;
#42610 = FACE_OUTER_BOUND ( 'NONE', #16271, .T. ) ;
#42611 = AXIS2_PLACEMENT_3D ( 'NONE', #33742, #54045, #8480 ) ;
#42612 = CARTESIAN_POINT ( 'NONE',  ( 1.719304012338836563, -3.626341562670527985, 12.20344780066003487 ) ) ;
#42613 = CARTESIAN_POINT ( 'NONE',  ( -27.08419797710328325, -0.8552720754637003209, 2.125717714519622881 ) ) ;
#42614 = FACE_OUTER_BOUND ( 'NONE', #16465, .T. ) ;
#42615 = EDGE_CURVE ( 'NONE', #37563, #43734, #54211, .T. ) ;
#42616 = CARTESIAN_POINT ( 'NONE',  ( 2.260457164927182738, -5.763213574030888964, 5.016645293558183560 ) ) ;
#42617 = CARTESIAN_POINT ( 'NONE',  ( -22.31328051695926007, -2.748895659348118858, -2.608921479762132734 ) ) ;
#42618 = AXIS2_PLACEMENT_3D ( 'NONE', #13803, #65011, #59715 ) ;
#42619 = VERTEX_POINT ( 'NONE', #28586 ) ;
#42620 = CARTESIAN_POINT ( 'NONE',  ( -23.41523303002442091, 1.997501275420757949, 4.252418708693335603 ) ) ;
#42621 = CARTESIAN_POINT ( 'NONE',  ( 0.2956976708475462234, -12.25433786972505779, -0.2200030809426881950 ) ) ;
#42622 = AXIS2_PLACEMENT_3D ( 'NONE', #13876, #33842, #54144 ) ;
#42623 = ORIENTED_EDGE ( 'NONE', *, *, #15645, .T. ) ;
#42624 = CARTESIAN_POINT ( 'NONE',  ( 35.00000000000000000, -5.636262487437393887, -10.80478261802180207 ) ) ;
#42625 = CARTESIAN_POINT ( 'NONE',  ( 1.462291587751586297, -9.267729738232038272, -8.602888600422598842 ) ) ;
#42626 = VERTEX_POINT ( 'NONE', #54849 ) ;
#42627 = CIRCLE ( 'NONE', #46892, 5.000000000000000000 ) ;
#42628 = CIRCLE ( 'NONE', #58591, 6.936499999999990784 ) ;
#42629 = DIRECTION ( 'NONE',  ( 0.000000000000000000, 0.01356324068817998940, -0.9999080150203990547 ) ) ;
#42630 = ORIENTED_EDGE ( 'NONE', *, *, #5938, .T. ) ;
#42631 = CARTESIAN_POINT ( 'NONE',  ( 0.000000000000000000, 4.409940824963425321, 5.354199675985255702 ) ) ;
#42632 = EDGE_LOOP ( 'NONE', ( #5450, #61086, #47121, #16976 ) ) ;
#42633 = EDGE_LOOP ( 'NONE', ( #50436, #37820, #15057, #41420 ) ) ;
#42634 = AXIS2_PLACEMENT_3D ( 'NONE', #51751, #36766, #10180 ) ;
#42635 = CARTESIAN_POINT ( 'NONE',  ( -22.30527770659433173, -3.381761229713378558, -1.656864125491266604 ) ) ;
#42636 = ORIENTED_EDGE ( 'NONE', *, *, #26045, .F. ) ;
#42637 = DIRECTION ( 'NONE',  ( 0.000000000000000000, 0.4698238015817365332, 0.8827602140260315533 ) ) ;
#42638 = CARTESIAN_POINT ( 'NONE',  ( 3.047904605210309814, -3.098478597269290535, 7.270585891216595265 ) ) ;
#42639 = FACE_OUTER_BOUND ( 'NONE', #45613, .T. ) ;
#42640 = FACE_OUTER_BOUND ( 'NONE', #2094, .T. ) ;
#42641 = EDGE_LOOP ( 'NONE', ( #33374, #65028, #17734, #34491 ) ) ;
#42642 = CARTESIAN_POINT ( 'NONE',  ( 35.00000000000000000, 4.705694406421931860E-17, -3.469127814946512892E-15 ) ) ;
#42643 = CARTESIAN_POINT ( 'NONE',  ( -0.4156926711315701573, -31.03628804997841684, 14.44394305974772408 ) ) ;
#42644 = CARTESIAN_POINT ( 'NONE',  ( 2.305787727787084407, -7.654065630109508689, 0.1666591538752418555 ) ) ;
#42646 = ORIENTED_EDGE ( 'NONE', *, *, #52308, .F. ) ;
#42645 = CARTESIAN_POINT ( 'NONE',  ( 37.00000000000000711, 6.018036132182163378, -11.24036214326523009 ) ) ;
#42647 = DIRECTION ( 'NONE',  ( 0.000000000000000000, -0.01356324068818000328, 0.9999080150203990547 ) ) ;
#42648 = ORIENTED_EDGE ( 'NONE', *, *, #23485, .T. ) ;
#42650 = EDGE_CURVE ( 'NONE', #21734, #55560, #3347, .T. ) ;
#42649 = DIRECTION ( 'NONE',  ( 0.000000000000000000, 0.8515178078024886466, -0.5243256840888532722 ) ) ;
#42651 = ORIENTED_EDGE ( 'NONE', *, *, #48613, .T. ) ;
#42652 = CARTESIAN_POINT ( 'NONE',  ( 21.83529864932240017, -10.79899791687600619, -5.236407238049663349 ) ) ;
#42653 = DIRECTION ( 'NONE',  ( 0.000000000000000000, 0.01356324068817992175, -0.9999080150203990547 ) ) ;
#42654 = DIRECTION ( 'NONE',  ( 1.000000000000000000, 0.000000000000000000, 0.000000000000000000 ) ) ;
#42655 = EDGE_CURVE ( 'NONE', #20112, #48583, #34024, .T. ) ;
#42656 = AXIS2_PLACEMENT_3D ( 'NONE', #15566, #62119, #16572 ) ;
#42657 = ORIENTED_EDGE ( 'NONE', *, *, #39861, .F. ) ;
#42658 = DIRECTION ( 'NONE',  ( 1.000000000000000000, 0.000000000000000000, -0.000000000000000000 ) ) ;
#42659 = LINE ( 'NONE', #12738, #49485 ) ;
#42660 = CARTESIAN_POINT ( 'NONE',  ( 13.17631928000994712, 11.70382209058883483, -6.731835258288742629 ) ) ;
#42662 = VERTEX_POINT ( 'NONE', #14902 ) ;
#42661 = CIRCLE ( 'NONE', #27828, 1.399999999999999911 ) ;
#42663 = EDGE_LOOP ( 'NONE', ( #31347, #15439, #39651, #1354 ) ) ;
#42664 = CARTESIAN_POINT ( 'NONE',  ( -37.00000000000000711, -6.564808257521847601, 10.93004082984016634 ) ) ;
#42665 = ORIENTED_EDGE ( 'NONE', *, *, #7835, .F. ) ;
#42666 = CIRCLE ( 'NONE', #5541, 12.75000000000000178 ) ;
#42667 = ORIENTED_EDGE ( 'NONE', *, *, #31732, .F. ) ;
#42668 = AXIS2_PLACEMENT_3D ( 'NONE', #13272, #44176, #13574 ) ;
#42669 = CYLINDRICAL_SURFACE ( 'NONE', #55102, 5.594511299047803199 ) ;
#42670 = DIRECTION ( 'NONE',  ( -1.000000000000000000, -1.836970198721029688E-16, 0.000000000000000000 ) ) ;
#42671 = CARTESIAN_POINT ( 'NONE',  ( -37.00000000000000711, -7.474872387600942858, -9.060822531526127932 ) ) ;
#42672 = CARTESIAN_POINT ( 'NONE',  ( -22.29195009621226831, 1.030739959031474973, 3.580440466953051626 ) ) ;
#42673 = CARTESIAN_POINT ( 'NONE',  ( 2.000000000000001776, 6.470132594555847660, -2.133363481234036296 ) ) ;
#42674 = CYLINDRICAL_SURFACE ( 'NONE', #16111, 4.999999999999999112 ) ;
#42675 = EDGE_CURVE ( 'NONE', #32268, #57074, #19920, .T. ) ;
#42676 = DIRECTION ( 'NONE',  ( 0.000000000000000000, 0.000000000000000000, -1.000000000000000000 ) ) ;
#42677 = CIRCLE ( 'NONE', #61773, 5.000000000000000888 ) ;
#42678 = EDGE_CURVE ( 'NONE', #8992, #60025, #20212, .T. ) ;
#42679 = EDGE_CURVE ( 'NONE', #59695, #62587, #51037, .T. ) ;
#42680 = ORIENTED_EDGE ( 'NONE', *, *, #9463, .T. ) ;
#42681 = CARTESIAN_POINT ( 'NONE',  ( -36.00000000000000711, 4.561791185930588632, -11.90598845858528776 ) ) ;
#42682 = EDGE_CURVE ( 'NONE', #4661, #51925, #53170, .T. ) ;
#42683 = CARTESIAN_POINT ( 'NONE',  ( -22.29115169517546136, -3.075985640626798023, 2.098196790595514560 ) ) ;
#42684 = CIRCLE ( 'NONE', #31029, 5.000000000000000888 ) ;
#42685 = VECTOR ( 'NONE', #8368, 1000.000000000000000 ) ;
#42686 = CARTESIAN_POINT ( 'NONE',  ( -22.27384469013076185, 0.9224151068931638608, 3.564715702084478632 ) ) ;
#42687 = CARTESIAN_POINT ( 'NONE',  ( 0.000000000000000000, 0.000000000000000000, 0.000000000000000000 ) ) ;
#42688 = VECTOR ( 'NONE', #16796, 1000.000000000000000 ) ;
#42689 = DIRECTION ( 'NONE',  ( -1.000000000000000000, 0.000000000000000000, 0.000000000000000000 ) ) ;
#42690 = EDGE_CURVE ( 'NONE', #64984, #39958, #20339, .T. ) ;
#42691 =( BOUNDED_SURFACE ( )  B_SPLINE_SURFACE ( 3, 2, ( 
 ( #62452, #12252, #7254 ),
 ( #11280, #37184, #11595 ),
 ( #6299, #6951, #52184 ),
 ( #31549, #6631, #11920 ),
 ( #36550, #58146, #41517 ),
 ( #62786, #32197, #22228 ),
 ( #2295, #42488, #17254 ),
 ( #37528, #22572, #42834 ),
 ( #57833, #61810, #63125 ),
 ( #12561, #32842, #5990 ),
 ( #26246, #46520, #34639 ),
 ( #24686, #39646, #14673 ),
 ( #24345, #25663, #20681 ),
 ( #15011, #29650, #29990 ),
 ( #45957, #9060, #9701 ),
 ( #60576, #14037, #54642 ),
 ( #29340, #64900, #49637 ),
 ( #45606, #4077, #65244 ),
 ( #55924, #412, #40625 ),
 ( #34956, #20341, #50302 ),
 ( #35630, #55262, #35297 ),
 ( #59946, #44963, #65547 ),
 ( #10355, #19712, #4755 ),
 ( #5391, #44610, #50943 ),
 ( #39967, #60249, #25017 ),
 ( #45289, #59608, #57 ),
 ( #34328, #19379, #20017 ),
 ( #55610, #14367, #54935 ),
 ( #40283, #10046, #9365 ),
 ( #30327, #49956, #50620 ),
 ( #4416, #60920, #5066 ),
 ( #25329, #15357, #30632 ),
 ( #5735, #40956, #52596 ),
 ( #61892, #7021, #47585 ),
 ( #2031, #46598, #26002 ),
 ( #1054, #21323, #35938 ),
 ( #1718, #21983, #26982 ),
 ( #20985, #36623, #36283 ),
 ( #27291, #56240, #15662 ),
 ( #46286, #61549, #42235 ),
 ( #51612, #41605, #6058 ),
 ( #26316, #41930, #16351 ),
 ( #61236, #47277, #56929 ),
 ( #15995, #41266, #21676 ),
 ( #11348, #10682, #62528 ),
 ( #56589, #31618, #727 ),
 ( #30969, #51285, #51931 ),
 ( #11031, #6373, #31310 ),
 ( #26641, #46934, #1395 ),
 ( #62215, #16666, #36939 ) ),
 .UNSPECIFIED., .F., .F., .F. ) 
 B_SPLINE_SURFACE_WITH_KNOTS ( ( 4, 2, 2, 2, 2, 2, 2, 2, 2, 2, 2, 2, 2, 2, 2, 2, 2, 2, 2, 2, 2, 2, 2, 2, 4 ),
 ( 3, 3 ),
 ( 0.06047842900482980344, 0.06367705432712368607, 0.06527636698827063433, 0.06687567964941756871, 0.06847499231056451696, 0.07007430497171146522, 0.07327293029400534785, 0.07647155561629923048, 0.07807086827744617874, 0.07967018093859312700, 0.08286880626088700963, 0.08446811892203395788, 0.08606743158318089226, 0.08926605690547478877, 0.09086536956662172315, 0.09246468222776867141, 0.09566330755006255404, 0.09726262021120950230, 0.09886193287235645055, 0.1020605581946503332, 0.1052591835169442158, 0.1068584961780911641, 0.1084578088392381123, 0.1100571215003850467, 0.1116564341615319950 ),
 ( 0.000000000000000000, 1.000000000000000000 ),
 .UNSPECIFIED. ) 
 GEOMETRIC_REPRESENTATION_ITEM ( )  RATIONAL_B_SPLINE_SURFACE ( (
 ( 1.000000000000000000, 0.4999999999999997224, 1.000000000000000000),
 ( 1.000000000000000000, 0.5048840838053595403, 1.000000000000000000),
 ( 1.000000000000000000, 0.5132072642500214998, 1.000000000000000000),
 ( 1.000000000000000000, 0.5290214861663712353, 1.000000000000000000),
 ( 1.000000000000000000, 0.5348648783786204008, 1.000000000000000000),
 ( 1.000000000000000000, 0.5473516051742154387, 1.000000000000000000),
 ( 1.000000000000000000, 0.5539126387907835625, 1.000000000000000000),
 ( 1.000000000000000000, 0.5674101295480111773, 1.000000000000000000),
 ( 1.000000000000000000, 0.5743474342085095330, 1.000000000000000000),
 ( 1.000000000000000000, 0.5883951384280732277, 1.000000000000000000),
 ( 1.000000000000000000, 0.5955302209472060904, 1.000000000000000000),
 ( 1.000000000000000000, 0.6167715304226100148, 1.000000000000000000),
 ( 1.000000000000000000, 0.6305661306844096980, 1.000000000000000000),
 ( 1.000000000000000000, 0.6565125894475725143, 1.000000000000000000),
 ( 1.000000000000000000, 0.6686743926052454157, 1.000000000000000000),
 ( 1.000000000000000000, 0.6851014456086110815, 1.000000000000000000),
 ( 1.000000000000000000, 0.6902475665163220198, 1.000000000000000000),
 ( 1.000000000000000000, 0.6997062435424069582, 1.000000000000000000),
 ( 1.000000000000000000, 0.7040363771868437537, 1.000000000000000000),
 ( 1.000000000000000000, 0.7157418617800307414, 1.000000000000000000),
 ( 1.000000000000000000, 0.7218341033859928535, 1.000000000000000000),
 ( 1.000000000000000000, 0.7280280015705831165, 1.000000000000000000),
 ( 1.000000000000000000, 0.7296036051600910399, 1.000000000000000000),
 ( 1.000000000000000000, 0.7316818214127936981, 1.000000000000000000),
 ( 1.000000000000000000, 0.7321927565546040295, 1.000000000000000000),
 ( 1.000000000000000000, 0.7321641879719948953, 1.000000000000000000),
 ( 1.000000000000000000, 0.7300624469249552551, 1.000000000000000000),
 ( 1.000000000000000000, 0.7238943330025175982, 1.000000000000000000),
 ( 1.000000000000000000, 0.7213359435419578469, 1.000000000000000000),
 ( 1.000000000000000000, 0.7152343487864250005, 1.000000000000000000),
 ( 1.000000000000000000, 0.7117056589944237288, 1.000000000000000000),
 ( 1.000000000000000000, 0.6999072021060018800, 1.000000000000000000),
 ( 1.000000000000000000, 0.6903911339385546686, 1.000000000000000000),
 ( 1.000000000000000000, 0.6741089150888935899, 1.000000000000000000),
 ( 1.000000000000000000, 0.6683461163769471858, 1.000000000000000000),
 ( 1.000000000000000000, 0.6562237482356158003, 1.000000000000000000),
 ( 1.000000000000000000, 0.6498375142660285375, 1.000000000000000000),
 ( 1.000000000000000000, 0.6302143011363016134, 1.000000000000000000),
 ( 1.000000000000000000, 0.6164540672887561801, 1.000000000000000000),
 ( 1.000000000000000000, 0.5885848209491306715, 1.000000000000000000),
 ( 1.000000000000000000, 0.5744580946949985334, 1.000000000000000000),
 ( 1.000000000000000000, 0.5540565490002123950, 1.000000000000000000),
 ( 1.000000000000000000, 0.5474350731751662646, 1.000000000000000000),
 ( 1.000000000000000000, 0.5350293539660013753, 1.000000000000000000),
 ( 1.000000000000000000, 0.5292092555093375061, 1.000000000000000000),
 ( 1.000000000000000000, 0.5186171472262197657, 1.000000000000000000),
 ( 1.000000000000000000, 0.5138445523878424348, 1.000000000000000000),
 ( 1.000000000000000000, 0.5056909436241939781, 1.000000000000000000),
 ( 1.000000000000000000, 0.5023956439952818043, 1.000000000000000000),
 ( 1.000000000000000000, 0.4999999999999995004, 1.000000000000000000) ) ) 
 REPRESENTATION_ITEM ( '' )  SURFACE ( )  );
#42692 = CARTESIAN_POINT ( 'NONE',  ( 16.78263030916553333, -12.17295508002144011, 5.836879698929882565 ) ) ;
#42693 = EDGE_CURVE ( 'NONE', #5798, #15336, #32966, .T. ) ;
#42694 = CARTESIAN_POINT ( 'NONE',  ( 8.957021277343063304, 4.012943098840286105, -11.31181617744290158 ) ) ;
#42695 = ORIENTED_EDGE ( 'NONE', *, *, #29079, .F. ) ;
#42696 = DIRECTION ( 'NONE',  ( 1.000000000000000000, -0.000000000000000000, 0.000000000000000000 ) ) ;
#42697 = CARTESIAN_POINT ( 'NONE',  ( 0.2648321136542697296, -1.986804758684036276, -12.08378267055567434 ) ) ;
#42698 = DIRECTION ( 'NONE',  ( 0.000000000000000000, -1.000000000000000000, 0.000000000000000000 ) ) ;
#42699 = CARTESIAN_POINT ( 'NONE',  ( 2.941278708680199916, -6.138172921908580548, -0.1348063076487592271 ) ) ;
#42700 = CIRCLE ( 'NONE', #14046, 2.899999999999994582 ) ;
#42701 = AXIS2_PLACEMENT_3D ( 'NONE', #38650, #43622, #3431 ) ;
#42702 = EDGE_CURVE ( 'NONE', #46041, #42334, #56337, .T. ) ;
#42703 = FACE_OUTER_BOUND ( 'NONE', #129, .T. ) ;
#42704 = CYLINDRICAL_SURFACE ( 'NONE', #14975, 2.899999999999994582 ) ;
#42705 = AXIS2_PLACEMENT_3D ( 'NONE', #15992, #56585, #11026 ) ;
#42706 = VERTEX_POINT ( 'NONE', #44862 ) ;
#42707 = CARTESIAN_POINT ( 'NONE',  ( 19.21195920369069299, -2.638879775956874507, 11.74464917922519547 ) ) ;
#42708 = CARTESIAN_POINT ( 'NONE',  ( -17.32245137130363943, 3.212379320876176170, 13.11341242674679286 ) ) ;
#42709 = CARTESIAN_POINT ( 'NONE',  ( 2.298277635560095788, -4.791911337974128493, -5.967558917212117287 ) ) ;
#42710 = CIRCLE ( 'NONE', #50204, 5.000000000000000000 ) ;
#42711 = CARTESIAN_POINT ( 'NONE',  ( 0.6473888112830246122, -12.23851338376148590, -1.823007254467082339 ) ) ;
#42712 = EDGE_LOOP ( 'NONE', ( #17743, #33761, #61030, #65465 ) ) ;
#42713 = FACE_OUTER_BOUND ( 'NONE', #17051, .T. ) ;
#42714 = CARTESIAN_POINT ( 'NONE',  ( 0.2652384529303120075, -4.250461213012467709, -11.48485968917278299 ) ) ;
#42715 = VERTEX_POINT ( 'NONE', #55164 ) ;
#42716 = ORIENTED_EDGE ( 'NONE', *, *, #38039, .T. ) ;
#42717 = B_SPLINE_CURVE_WITH_KNOTS ( 'NONE', 3,
 ( #22681, #62892, #53605, #38272, #17359, #58932, #63223, #27994, #48938, #48300, #8047, #48606, #23323, #43587, #33630, #38618, #18355, #53918, #28633, #3394, #23664, #64846 ),
 .UNSPECIFIED., .F., .F.,
 ( 4, 3, 3, 3, 3, 3, 3, 4 ),
 ( 8.824766327896537836E-19, 4.449119708436899146E-05, 6.626296329540649216E-05, 8.803456484963045230E-05, 0.0001098060367612840654, 0.0001315774408628553544, 0.0001760698110411230662, 0.0001829697163287824805 ),
 .UNSPECIFIED. ) ;
#42718 = FACE_OUTER_BOUND ( 'NONE', #719, .T. ) ;
#42719 = DIRECTION ( 'NONE',  ( -1.000000000000000000, -0.000000000000000000, 0.000000000000000000 ) ) ;
#42720 = ORIENTED_EDGE ( 'NONE', *, *, #58535, .F. ) ;
#42721 = CARTESIAN_POINT ( 'NONE',  ( 0.2911222467163543381, -9.524109243548023684, 7.711756541611659799 ) ) ;
#42722 = VECTOR ( 'NONE', #31888, 1000.000000000000000 ) ;
#42723 = CARTESIAN_POINT ( 'NONE',  ( -37.00000000000000711, 0.000000000000000000, 0.000000000000000000 ) ) ;
#42724 = DIRECTION ( 'NONE',  ( 0.000000000000000000, 0.1081190184239417817, -0.9941379571543595972 ) ) ;
#42725 = PLANE ( 'NONE',  #56324 ) ;
#42726 = DIRECTION ( 'NONE',  ( 0.000000000000000000, -0.1740410799127471153, -0.9847383929261642743 ) ) ;
#42727 = CARTESIAN_POINT ( 'NONE',  ( 0.2911222467163552263, 5.940753417478925158, 10.71854909364320463 ) ) ;
#42729 = ORIENTED_EDGE ( 'NONE', *, *, #37899, .F. ) ;
#42728 = CARTESIAN_POINT ( 'NONE',  ( -2.532614230583023041, 12.88560382747354005, 4.026315189028235153 ) ) ;
#42730 = CARTESIAN_POINT ( 'NONE',  ( 1.287602823388335427, 4.819820779360716401, -11.62763122280001582 ) ) ;
#42731 = ORIENTED_EDGE ( 'NONE', *, *, #33430, .T. ) ;
#42732 = CIRCLE ( 'NONE', #44892, 12.18649999999999878 ) ;
#42733 = CARTESIAN_POINT ( 'NONE',  ( 2.241528039335008327, -0.01573255094247159869, 7.634443721858077403 ) ) ;
#42734 = VERTEX_POINT ( 'NONE', #10261 ) ;
#42735 = VECTOR ( 'NONE', #14591, 1000.000000000000000 ) ;
#42736 = VERTEX_POINT ( 'NONE', #40184 ) ;
#42737 = APPLICATION_PROTOCOL_DEFINITION ( 'draft international standard', 'automotive_design', 1998, #9387 ) ;
#42738 = CARTESIAN_POINT ( 'NONE',  ( 1.719304012339893051, -12.70777170743897422, -0.7661785589590540679 ) ) ;
#42739 = CARTESIAN_POINT ( 'NONE',  ( -22.27720387087365239, 3.639274226782813315, -0.5572161790459750907 ) ) ;
#42741 = CARTESIAN_POINT ( 'NONE',  ( -3.386137662399145487, 11.13011477932007232, 4.505408349134588875 ) ) ;
#42740 = CIRCLE ( 'NONE', #7735, 12.74999999999999822 ) ;
#42742 = EDGE_CURVE ( 'NONE', #12098, #14609, #7478, .T. ) ;
#42743 = VECTOR ( 'NONE', #31366, 1000.000000000000000 ) ;
#42744 = CARTESIAN_POINT ( 'NONE',  ( -46.51586683006346590, -0.6857498399870952666, 10.66240463596387578 ) ) ;
#42745 = CARTESIAN_POINT ( 'NONE',  ( -27.08426504710140392, 0.6326154899769418360, -2.202478235133286333 ) ) ;
#42746 = ORIENTED_EDGE ( 'NONE', *, *, #7307, .T. ) ;
#42747 = CARTESIAN_POINT ( 'NONE',  ( -35.00000000000000000, -9.908974237959601084, -6.307491713049132365 ) ) ;
#42748 = ADVANCED_FACE ( 'NONE', ( #34855 ), #15894, .T. ) ;
#42749 = CARTESIAN_POINT ( 'NONE',  ( 2.740575968810160301, 2.123581467810721435, -13.35090380385353548 ) ) ;
#42750 = ORIENTED_EDGE ( 'NONE', *, *, #13296, .T. ) ;
#42751 = ORIENTED_EDGE ( 'NONE', *, *, #33129, .F. ) ;
#42752 = CARTESIAN_POINT ( 'NONE',  ( -1.734723475976807094E-15, -3.469446951953614189E-15, -11.99999999999998934 ) ) ;
#42753 = EDGE_CURVE ( 'NONE', #8323, #55428, #29072, .T. ) ;
#42754 = VERTEX_POINT ( 'NONE', #312 ) ;
#42755 = AXIS2_PLACEMENT_3D ( 'NONE', #57356, #18701, #37727 ) ;
#42756 = CARTESIAN_POINT ( 'NONE',  ( 35.00000000000000000, 4.705694406421931860E-17, -3.469127814946512892E-15 ) ) ;
#42757 = CARTESIAN_POINT ( 'NONE',  ( 0.3665391374699464300, 5.911453292029603013, 10.76665847464314751 ) ) ;
#42758 = DIRECTION ( 'NONE',  ( 0.000000000000000000, -0.6876994588534142139, -0.7259954919231395021 ) ) ;
#42759 = CARTESIAN_POINT ( 'NONE',  ( -47.00000000000000711, 0.000000000000000000, 0.000000000000000000 ) ) ;
#42760 = AXIS2_PLACEMENT_3D ( 'NONE', #8007, #48566, #33588 ) ;
#42761 = DIRECTION ( 'NONE',  ( 1.000000000000000000, 0.000000000000000000, 0.000000000000000000 ) ) ;
#42762 = CARTESIAN_POINT ( 'NONE',  ( -27.10719052120871098, -1.962717903527672059, 1.310802520592011966 ) ) ;
#42763 = EDGE_CURVE ( 'NONE', #13765, #46293, #65141, .T. ) ;
#42764 = CARTESIAN_POINT ( 'NONE',  ( 2.276198483117258586, 3.955655305430065383, -6.543270001966361882 ) ) ;
#42765 = ORIENTED_EDGE ( 'NONE', *, *, #55495, .T. ) ;
#42766 = FACE_OUTER_BOUND ( 'NONE', #63014, .T. ) ;
#42767 = ADVANCED_FACE ( 'NONE', ( #35840 ), #50198, .T. ) ;
#42768 = VERTEX_POINT ( 'NONE', #7235 ) ;
#42769 = VECTOR ( 'NONE', #63686, 1000.000000000000114 ) ;
#42770 = CARTESIAN_POINT ( 'NONE',  ( 0.2653519991613804141, -6.142165520908248411, 10.59450977800980453 ) ) ;
#42771 = EDGE_CURVE ( 'NONE', #26553, #36879, #46830, .T. ) ;
#42772 = CARTESIAN_POINT ( 'NONE',  ( -8.902713192980971968, -10.71502374161934057, -8.218914786477059309 ) ) ;
#42773 = CARTESIAN_POINT ( 'NONE',  ( 2.276198483117258142, -3.955655305430017865, 6.543270001966392080 ) ) ;
#42774 = DIRECTION ( 'NONE',  ( -1.000000000000000000, 0.000000000000000000, 0.000000000000000000 ) ) ;
#42775 = B_SPLINE_CURVE_WITH_KNOTS ( 'NONE', 3,
 ( #23048, #2789, #18728, #54636, #58642, #13383, #43308, #63582, #24338, #19373, #33668, #13699, #28353, #28675, #44603, #58296 ),
 .UNSPECIFIED., .F., .F.,
 ( 4, 3, 3, 3, 3, 4 ),
 ( 4.336808689942017736E-19, 0.0002176109881720207173, 0.0004352086762394531856, 0.0006528017811446789427, 0.0007615147961451612180, 0.0009453342004947423759 ),
 .UNSPECIFIED. ) ;
#42776 = ORIENTED_EDGE ( 'NONE', *, *, #64750, .F. ) ;
#42777 = EDGE_LOOP ( 'NONE', ( #56175, #24281, #29421, #46443 ) ) ;
#42778 = CARTESIAN_POINT ( 'NONE',  ( -36.00000000000000711, -10.49626516989265923, -7.238157050195740183 ) ) ;
#42779 = VERTEX_POINT ( 'NONE', #32822 ) ;
#42780 = CARTESIAN_POINT ( 'NONE',  ( 35.00000000000000000, -10.30098186818245409, 5.644643009979177783 ) ) ;
#42781 = EDGE_CURVE ( 'NONE', #5722, #5002, #6612, .T. ) ;
#42782 = DIRECTION ( 'NONE',  ( 0.000000000000000000, 0.000000000000000000, 1.000000000000000000 ) ) ;
#42783 = CARTESIAN_POINT ( 'NONE',  ( -10.00000000000000178, 0.000000000000000000, 0.000000000000000000 ) ) ;
#42784 = CARTESIAN_POINT ( 'NONE',  ( 2.241352910868908310, 1.407733736974966288, -7.503490710578218703 ) ) ;
#42785 = EDGE_CURVE ( 'NONE', #20437, #57759, #37508, .T. ) ;
#42786 = VERTEX_POINT ( 'NONE', #22205 ) ;
#42787 = AXIS2_PLACEMENT_3D ( 'NONE', #64174, #19615, #39877 ) ;
#42788 = CARTESIAN_POINT ( 'NONE',  ( 0.3654063281920738038, 12.13594617907221540, 1.872466061177124885 ) ) ;
#42789 = LINE ( 'NONE', #13508, #24730 ) ;
#42790 = AXIS2_PLACEMENT_3D ( 'NONE', #49420, #13786, #64020 ) ;
#42791 = FACE_OUTER_BOUND ( 'NONE', #35276, .T. ) ;
#42792 = DIRECTION ( 'NONE',  ( -1.000000000000000000, -1.836970198721029688E-16, -0.000000000000000000 ) ) ;
#42793 = ADVANCED_FACE ( 'NONE', ( #1626 ), #21900, .T. ) ;
#42794 = CIRCLE ( 'NONE', #51329, 5.000000000000000000 ) ;
#42795 = EDGE_CURVE ( 'NONE', #60735, #39298, #63775, .T. ) ;
#42796 = LINE ( 'NONE', #57458, #28804 ) ;
#42797 = CARTESIAN_POINT ( 'NONE',  ( 2.305787727787084407, 1.493241775258423720, 7.508843116234161563 ) ) ;
#42798 = B_SPLINE_CURVE_WITH_KNOTS ( 'NONE', 3,
 ( #12352, #43942, #48942, #38623, #52928, #22324, #23670, #27998, #37957, #64220, #8050, #48612, #48303, #58936, #12028, #58251 ),
 .UNSPECIFIED., .F., .F.,
 ( 4, 3, 3, 3, 3, 4 ),
 ( 2.536682445082988549E-15, 0.0002126834539179670665, 0.0004253519300366167036, 0.0006380165497224025116, 0.0007442707582428092529, 0.0009453531351419345490 ),
 .UNSPECIFIED. ) ;
#42799 = ORIENTED_EDGE ( 'NONE', *, *, #28699, .F. ) ;
#42800 = CARTESIAN_POINT ( 'NONE',  ( -27.08429572838383947, 1.859677275556428810, -1.338867938658195200 ) ) ;
#42801 = AXIS2_PLACEMENT_3D ( 'NONE', #23328, #18015, #58601 ) ;
#42803 = EDGE_CURVE ( 'NONE', #9125, #51886, #1937, .T. ) ;
#42802 = CARTESIAN_POINT ( 'NONE',  ( -15.30016555129190792, -28.05832310202213620, -10.91616026484521385 ) ) ;
#42804 = VERTEX_POINT ( 'NONE', #953 ) ;
#42805 = DIRECTION ( 'NONE',  ( 1.000000000000000000, -0.000000000000000000, -0.000000000000000000 ) ) ;
#42806 = CARTESIAN_POINT ( 'NONE',  ( 1.109979610370630754, -8.414317452282139342, 9.281420052101156060 ) ) ;
#42807 = CARTESIAN_POINT ( 'NONE',  ( -37.00000000000000711, -11.65554240571058031, 1.456211999474302798 ) ) ;
#42808 = CIRCLE ( 'NONE', #5684, 12.74999999999999822 ) ;
#42809 = CARTESIAN_POINT ( 'NONE',  ( 37.00000000000000711, -11.38112321385048631, 2.905556151562744382 ) ) ;
#42810 = CARTESIAN_POINT ( 'NONE',  ( -22.76187086591099984, 1.734723475976807094E-15, -8.673617379884035472E-15 ) ) ;
#42811 = AXIS2_PLACEMENT_3D ( 'NONE', #7576, #38148, #28196 ) ;
#42812 = EDGE_LOOP ( 'NONE', ( #54588, #12907, #7023, #25664 ) ) ;
#42813 = ORIENTED_EDGE ( 'NONE', *, *, #46514, .T. ) ;
#42814 = CARTESIAN_POINT ( 'NONE',  ( 37.00000000000000711, -11.74614673114903596, -0.01609748574441245694 ) ) ;
#42815 = ORIENTED_EDGE ( 'NONE', *, *, #35784, .T. ) ;
#42816 = CARTESIAN_POINT ( 'NONE',  ( 2.000000000000001776, -3.341639490130797530, 6.078525953551414673 ) ) ;
#42817 = CARTESIAN_POINT ( 'NONE',  ( 3.047904605210274731, 7.561255571389346564, -2.299870214474515340 ) ) ;
#42818 = CARTESIAN_POINT ( 'NONE',  ( -35.00000000000000000, -7.110831038798204773, -9.896810808925470937 ) ) ;
#42819 = CARTESIAN_POINT ( 'NONE',  ( -35.00000000000000000, -12.54989509947649751, -2.250029553613891675 ) ) ;
#42820 = CYLINDRICAL_SURFACE ( 'NONE', #65106, 12.18649999999999878 ) ;
#42821 = VECTOR ( 'NONE', #48599, 1000.000000000000000 ) ;
#42822 = CARTESIAN_POINT ( 'NONE',  ( 2.263328370261528555, 7.548992860189821741, 1.186889399881216223 ) ) ;
#42823 = ORIENTED_EDGE ( 'NONE', *, *, #50243, .T. ) ;
#42824 = ORIENTED_EDGE ( 'NONE', *, *, #23948, .F. ) ;
#42825 = DIRECTION ( 'NONE',  ( -1.000000000000000000, 0.000000000000000000, 0.000000000000000000 ) ) ;
#42826 = ORIENTED_EDGE ( 'NONE', *, *, #36983, .F. ) ;
#42827 = CARTESIAN_POINT ( 'NONE',  ( 21.44662240950248133, -13.04912158988539339, -3.483575318819825739 ) ) ;
#42828 = DIRECTION ( 'NONE',  ( -1.000000000000000000, -0.000000000000000000, -0.000000000000000000 ) ) ;
#42829 = EDGE_CURVE ( 'NONE', #38497, #56049, #32921, .T. ) ;
#42830 = AXIS2_PLACEMENT_3D ( 'NONE', #14157, #13817, #34106 ) ;
#42831 = CYLINDRICAL_SURFACE ( 'NONE', #47908, 12.18650000000000055 ) ;
#42832 = VERTEX_POINT ( 'NONE', #21222 ) ;
#42833 = DIRECTION ( 'NONE',  ( -0.4531421102008652557, 0.000000000000000000, -0.8914382917301156839 ) ) ;
#42834 = CARTESIAN_POINT ( 'NONE',  ( -16.37486794060188444, -29.30468282063774765, -10.24044889374801315 ) ) ;
#42835 = CARTESIAN_POINT ( 'NONE',  ( 2.705197763288549329, -1.627208841526513350, 7.617149697727738200 ) ) ;
#42836 = ORIENTED_EDGE ( 'NONE', *, *, #51284, .F. ) ;
#42837 = ORIENTED_EDGE ( 'NONE', *, *, #5809, .F. ) ;
#42838 = CARTESIAN_POINT ( 'NONE',  ( 3.152665057734040488, 0.000000000000000000, 0.000000000000000000 ) ) ;
#42839 = VERTEX_POINT ( 'NONE', #11260 ) ;
#42840 = ORIENTED_EDGE ( 'NONE', *, *, #58121, .T. ) ;
#42842 = DIRECTION ( 'NONE',  ( -1.000000000000000000, -0.000000000000000000, 0.000000000000000000 ) ) ;
#42841 = CIRCLE ( 'NONE', #4662, 12.18650000000000055 ) ;
#42843 = EDGE_CURVE ( 'NONE', #6053, #16234, #26583, .T. ) ;
#42844 = VECTOR ( 'NONE', #61989, 1000.000000000000000 ) ;
#42845 = ORIENTED_EDGE ( 'NONE', *, *, #9463, .F. ) ;
#42846 = VERTEX_POINT ( 'NONE', #13530 ) ;
#42847 = FACE_OUTER_BOUND ( 'NONE', #60952, .T. ) ;
#42848 = CARTESIAN_POINT ( 'NONE',  ( 1.719304012338199517, 0.000000000000000000, 0.000000000000000000 ) ) ;
#42849 = CIRCLE ( 'NONE', #14167, 6.936499999999987232 ) ;
#42850 = CARTESIAN_POINT ( 'NONE',  ( -20.15450366670237869, -11.80221610452082714, -2.191204727034115507 ) ) ;
#42851 = CARTESIAN_POINT ( 'NONE',  ( 0.2648978790185584908, -7.769924372105139199, -9.465406350830686932 ) ) ;
#42852 = DIRECTION ( 'NONE',  ( 1.000000000000000000, 0.000000000000000000, 0.000000000000000000 ) ) ;
#42853 = DIRECTION ( 'NONE',  ( 0.000000000000000000, -0.5472293298355330737, 0.8369827122275305120 ) ) ;
#42854 = ORIENTED_EDGE ( 'NONE', *, *, #21009, .T. ) ;
#42855 = CYLINDRICAL_SURFACE ( 'NONE', #13531, 6.936499999999988120 ) ;
#42857 = CARTESIAN_POINT ( 'NONE',  ( -22.27720387087365239, 2.873095842208905459, -2.302200479844925596 ) ) ;
#42856 = CIRCLE ( 'NONE', #24825, 7.499999999999988454 ) ;
#42859 = CARTESIAN_POINT ( 'NONE',  ( 0.2646305136544072623, -0.1321451301298671999, 12.24595685781654630 ) ) ;
#42858 = B_SPLINE_CURVE_WITH_KNOTS ( 'NONE', 3,
 ( #44172, #13569, #13890, #33857, #28549, #49510, #8592, #48850 ),
 .UNSPECIFIED., .F., .F.,
 ( 4, 2, 2, 4 ),
 ( 0.000000000000000000, 0.002114292923455004559, 0.003171439385182506839, 0.004228585846910009986 ),
 .UNSPECIFIED. ) ;
#42860 = EDGE_CURVE ( 'NONE', #16579, #40797, #28195, .T. ) ;
#42861 = DIRECTION ( 'NONE',  ( 1.000000000000000000, -0.000000000000000000, 0.000000000000000000 ) ) ;
#42862 = DIRECTION ( 'NONE',  ( 0.000000000000000000, 0.000000000000000000, 1.000000000000000000 ) ) ;
#42863 = DIRECTION ( 'NONE',  ( 1.000000000000000000, 0.000000000000000000, -0.000000000000000000 ) ) ;
#42864 = CARTESIAN_POINT ( 'NONE',  ( 0.2717059086739035956, -11.56868249951478589, -4.023283916512541580 ) ) ;
#42865 = CARTESIAN_POINT ( 'NONE',  ( 1.375507693217275840, 5.789143338282538132, 11.20969178069527139 ) ) ;
#42866 = CIRCLE ( 'NONE', #22707, 12.74999999999999822 ) ;
#42867 = ORIENTED_EDGE ( 'NONE', *, *, #40924, .T. ) ;
#42868 = CARTESIAN_POINT ( 'NONE',  ( -37.00000000000000711, -5.556331110570327247, -11.47561260193582910 ) ) ;
#42869 = AXIS2_PLACEMENT_3D ( 'NONE', #59605, #14363, #40278 ) ;
#42870 = ORIENTED_EDGE ( 'NONE', *, *, #1827, .T. ) ;
#42871 = CARTESIAN_POINT ( 'NONE',  ( 0.3164563675027642353, 10.73846246126249149, 5.922187299605671029 ) ) ;
#42872 = CARTESIAN_POINT ( 'NONE',  ( -16.73721172569806015, -28.43318523521388030, -9.619723400408265235 ) ) ;
#42873 = CIRCLE ( 'NONE', #21675, 5.000000000000000888 ) ;
#42874 = CYLINDRICAL_SURFACE ( 'NONE', #3813, 12.18649999999999878 ) ;
#42875 = DIRECTION ( 'NONE',  ( 0.000000000000000000, 0.000000000000000000, 1.000000000000000000 ) ) ;
#42876 = CARTESIAN_POINT ( 'NONE',  ( 2.994568964204213923, -4.756002438591021786, -6.289764245798271425 ) ) ;
#42877 = ORIENTED_EDGE ( 'NONE', *, *, #60809, .F. ) ;
#42878 = CARTESIAN_POINT ( 'NONE',  ( 2.000000000000001776, -3.979254915827401540, 5.681598592373737766 ) ) ;
#42879 = LINE ( 'NONE', #17295, #49293 ) ;
#42880 = CARTESIAN_POINT ( 'NONE',  ( -47.00000000000000711, 0.000000000000000000, 0.000000000000000000 ) ) ;
#42881 = CARTESIAN_POINT ( 'NONE',  ( 35.00000000000000000, 9.240395740215630482, -7.251710744571611578 ) ) ;
#42882 = EDGE_CURVE ( 'NONE', #7766, #30254, #4383, .T. ) ;
#42883 = AXIS2_PLACEMENT_3D ( 'NONE', #59778, #39479, #49167 ) ;
#42884 = EDGE_CURVE ( 'NONE', #4710, #20776, #59121, .T. ) ;
#42885 = DIRECTION ( 'NONE',  ( 0.000000000000000000, 0.01356324068817992175, -0.9999080150203990547 ) ) ;
#42886 = EDGE_LOOP ( 'NONE', ( #21743, #64396, #49959, #49292 ) ) ;
#42888 = EDGE_CURVE ( 'NONE', #1051, #63114, #21356, .T. ) ;
#42887 = LINE ( 'NONE', #62503, #54083 ) ;
#42889 = DIRECTION ( 'NONE',  ( 0.000000000000000000, 0.01356324068817998940, -0.9999080150203990547 ) ) ;
#42890 = AXIS2_PLACEMENT_3D ( 'NONE', #41277, #63442, #6067 ) ;
#42891 = AXIS2_PLACEMENT_3D ( 'NONE', #23430, #37741, #28740 ) ;
#42892 = ORIENTED_EDGE ( 'NONE', *, *, #61134, .T. ) ;
#42893 = LINE ( 'NONE', #63180, #34977 ) ;
#42894 = B_SPLINE_CURVE_WITH_KNOTS ( 'NONE', 3,
 ( #3955, #24215, #14544, #4616, #59801, #14234 ),
 .UNSPECIFIED., .F., .F.,
 ( 4, 2, 4 ),
 ( 0.000000000000000000, 0.0004528561986909231053, 0.0009057123973818462107 ),
 .UNSPECIFIED. ) ;
#42895 =( BOUNDED_SURFACE ( )  B_SPLINE_SURFACE ( 3, 1, ( 
 ( #50282, #25000 ),
 ( #45273, #20667 ),
 ( #15341, #35922 ),
 ( #45936, #11333 ) ),
 .UNSPECIFIED., .F., .F., .F. ) 
 B_SPLINE_SURFACE_WITH_KNOTS ( ( 4, 4 ),
 ( 2, 2 ),
 ( 0.000000000000000000, 1.000000000000000000 ),
 ( 0.000000000000000000, 1.000000000000000000 ),
 .UNSPECIFIED. ) 
 GEOMETRIC_REPRESENTATION_ITEM ( )  RATIONAL_B_SPLINE_SURFACE ( (
 ( 1.000000000000000000, 1.000000000000000000),
 ( 0.9942764183789327692, 0.8450855930916585379),
 ( 0.9942764183789327692, 0.8450855930916585379),
 ( 1.000000000000000000, 1.000000000000000000) ) ) 
 REPRESENTATION_ITEM ( '' )  SURFACE ( )  );
#42896 = ORIENTED_EDGE ( 'NONE', *, *, #13505, .F. ) ;
#42897 = CARTESIAN_POINT ( 'NONE',  ( 2.251152103363646795, -6.550893877460178594, 3.926807817126177547 ) ) ;
#42899 = AXIS2_PLACEMENT_3D ( 'NONE', #56382, #15154, #40769 ) ;
#42898 = CARTESIAN_POINT ( 'NONE',  ( 2.639814597422736941, -3.659458430304299181, -6.851176153958514981 ) ) ;
#42900 = LINE ( 'NONE', #53216, #338 ) ;
#42901 = CARTESIAN_POINT ( 'NONE',  ( -37.00000000000000711, -11.70009620280410978, -1.039216533673027243 ) ) ;
#42902 = CARTESIAN_POINT ( 'NONE',  ( 0.000000000000000000, 5.396716205731433291, 4.158041573745082431 ) ) ;
#42903 = ORIENTED_EDGE ( 'NONE', *, *, #4375, .F. ) ;
#42904 = AXIS2_PLACEMENT_3D ( 'NONE', #63619, #2140, #42676 ) ;
#42905 = ORIENTED_EDGE ( 'NONE', *, *, #8273, .F. ) ;
#42906 = ORIENTED_EDGE ( 'NONE', *, *, #31364, .F. ) ;
#42907 = CARTESIAN_POINT ( 'NONE',  ( 5.515539859299206427, -0.005142293699651617929, -0.003193223631738859817 ) ) ;
#42908 = VECTOR ( 'NONE', #52049, 1000.000000000000114 ) ;
#42909 = CARTESIAN_POINT ( 'NONE',  ( -19.47984447937493613, -1.416020129149132334, 25.00000000000000000 ) ) ;
#42910 = EDGE_CURVE ( 'NONE', #51465, #41912, #48810, .T. ) ;
#42911 = VERTEX_POINT ( 'NONE', #53132 ) ;
#42912 = CARTESIAN_POINT ( 'NONE',  ( -35.00000000000000000, 0.4353888892048373149, 11.73808581813438323 ) ) ;
#42913 = CARTESIAN_POINT ( 'NONE',  ( -22.28350523959500862, -0.3047406164877233814, -3.687952016964573421 ) ) ;
#42914 = ADVANCED_FACE ( 'NONE', ( #22886 ), #8348, .F. ) ;
#42915 = VERTEX_POINT ( 'NONE', #3261 ) ;
#42916 = CARTESIAN_POINT ( 'NONE',  ( -35.00000000000000000, -10.07641281632181673, 6.036400161834530209 ) ) ;
#42917 =( BOUNDED_SURFACE ( )  B_SPLINE_SURFACE ( 3, 1, ( 
 ( #18351, #18005 ),
 ( #17007, #38266 ),
 ( #58927, #53912 ),
 ( #13014, #33297 ) ),
 .UNSPECIFIED., .F., .F., .F. ) 
 B_SPLINE_SURFACE_WITH_KNOTS ( ( 4, 4 ),
 ( 2, 2 ),
 ( 0.000000000000000000, 1.000000000000000000 ),
 ( 0.000000000000000000, 1.000000000000000000 ),
 .UNSPECIFIED. ) 
 GEOMETRIC_REPRESENTATION_ITEM ( )  RATIONAL_B_SPLINE_SURFACE ( (
 ( 1.000000000000000000, 1.000000000000000000),
 ( 0.6933888150995267674, 0.9895912004443193632),
 ( 0.6933888150995267674, 0.9895912004443193632),
 ( 1.000000000000000000, 1.000000000000000000) ) ) 
 REPRESENTATION_ITEM ( '' )  SURFACE ( )  );
#42918 = CIRCLE ( 'NONE', #52541, 3.000000000000000444 ) ;
#42919 = DIRECTION ( 'NONE',  ( 0.000000000000000000, 0.01356324068817998940, -0.9999080150203990547 ) ) ;
#42920 = LINE ( 'NONE', #49568, #43040 ) ;
#42921 = ORIENTED_EDGE ( 'NONE', *, *, #8111, .T. ) ;
#42922 = ORIENTED_EDGE ( 'NONE', *, *, #42492, .F. ) ;
#42923 = LINE ( 'NONE', #17337, #22523 ) ;
#42924 = ORIENTED_EDGE ( 'NONE', *, *, #59806, .F. ) ;
#42925 = CARTESIAN_POINT ( 'NONE',  ( -20.31672697212907508, 11.54175897114123117, -3.341373981289996298 ) ) ;
#42926 = ORIENTED_EDGE ( 'NONE', *, *, #10363, .F. ) ;
#42927 = EDGE_CURVE ( 'NONE', #136, #14909, #35087, .T. ) ;
#42928 = CARTESIAN_POINT ( 'NONE',  ( 5.515539859299206427, 0.004759416711442177560, 0.003740028639278364028 ) ) ;
#42929 = CARTESIAN_POINT ( 'NONE',  ( 1.744217550858792265, -31.08480052993691345, -14.39239673296543920 ) ) ;
#42930 = CARTESIAN_POINT ( 'NONE',  ( -27.10719052120871098, -0.6736837626858844796, -2.261993590776034235 ) ) ;
#42931 = AXIS2_PLACEMENT_3D ( 'NONE', #5340, #9998, #30585 ) ;
#42932 = DIRECTION ( 'NONE',  ( -1.000000000000000000, 0.000000000000000000, 0.000000000000000000 ) ) ;
#42933 = FACE_OUTER_BOUND ( 'NONE', #40214, .T. ) ;
#42934 = CARTESIAN_POINT ( 'NONE',  ( 1.462291587751620714, 6.862867011842961773, -10.62080802716768524 ) ) ;
#42935 = CARTESIAN_POINT ( 'NONE',  ( 4.889044754487288813, -9.933478907102429645, -6.734253674175185722 ) ) ;
#42936 = ORIENTED_EDGE ( 'NONE', *, *, #11173, .T. ) ;
#42937 = CARTESIAN_POINT ( 'NONE',  ( -35.04834644901396956, 0.009049049589496429083, -0.01046409687785401256 ) ) ;
#42938 = VERTEX_POINT ( 'NONE', #33168 ) ;
#42939 = CARTESIAN_POINT ( 'NONE',  ( 2.245754705088393255, -2.715960966012146649, 7.136529175883355336 ) ) ;
#42940 = CARTESIAN_POINT ( 'NONE',  ( 35.00000000000000000, 3.511814412392283646, 11.66953048682395355 ) ) ;
#42941 = EDGE_CURVE ( 'NONE', #44564, #44595, #45745, .T. ) ;
#42942 = EDGE_CURVE ( 'NONE', #11977, #29813, #58540, .T. ) ;
#42943 = ORIENTED_EDGE ( 'NONE', *, *, #21685, .T. ) ;
#42944 = CARTESIAN_POINT ( 'NONE',  ( 2.781367136452501221, 7.442815111163411324, 2.381060477055354507 ) ) ;
#42945 = CARTESIAN_POINT ( 'NONE',  ( 0.3632410797595206353, 6.365652464380907816, 10.49990774419904227 ) ) ;
#42946 = CARTESIAN_POINT ( 'NONE',  ( 0.2653519890518172830, -9.381137101569615666, -7.871697161810781829 ) ) ;
#42947 = EDGE_CURVE ( 'NONE', #12619, #2058, #38036, .T. ) ;
#42948 = ORIENTED_EDGE ( 'NONE', *, *, #20860, .F. ) ;
#42949 = EDGE_LOOP ( 'NONE', ( #49885, #58198, #16857, #45909 ) ) ;
#42950 = CYLINDRICAL_SURFACE ( 'NONE', #57691, 19.00000000000000000 ) ;
#42951 = ORIENTED_EDGE ( 'NONE', *, *, #50892, .T. ) ;
#42952 = DIRECTION ( 'NONE',  ( 0.000000000000000000, -0.01356324068817998940, 0.9999080150203990547 ) ) ;
#42953 = CARTESIAN_POINT ( 'NONE',  ( -37.00000000000000711, 0.000000000000000000, 0.000000000000000000 ) ) ;
#42954 = LINE ( 'NONE', #63234, #12866 ) ;
#42955 = CARTESIAN_POINT ( 'NONE',  ( -17.74495101254168716, -6.568451298135349781, 10.04738369426859279 ) ) ;
#42956 = ORIENTED_EDGE ( 'NONE', *, *, #29237, .T. ) ;
#42957 = CARTESIAN_POINT ( 'NONE',  ( 5.515188684475870851, -0.004442604682416595625, 0.002983184900675373528 ) ) ;
#42958 = EDGE_CURVE ( 'NONE', #64815, #11282, #43137, .T. ) ;
#42960 = CIRCLE ( 'NONE', #40833, 5.000000000000000888 ) ;
#42959 = CIRCLE ( 'NONE', #57848, 5.000000000000000000 ) ;
#42961 = ADVANCED_FACE ( 'NONE', ( #63416 ), #15131, .F. ) ;
#42962 = CARTESIAN_POINT ( 'NONE',  ( 7.002886717044651377, -27.11012757947470320, -15.35900505431295926 ) ) ;
#42963 = CARTESIAN_POINT ( 'NONE',  ( -28.85619398320021745, 3.750539801530000439, 11.39883551934754280 ) ) ;
#42964 = LINE ( 'NONE', #17037, #6246 ) ;
#42965 = CYLINDRICAL_SURFACE ( 'NONE', #62799, 2.899999999999994582 ) ;
#42966 = DIRECTION ( 'NONE',  ( 0.000000000000000000, -1.000000000000000000, 0.000000000000000000 ) ) ;
#42967 = CARTESIAN_POINT ( 'NONE',  ( -22.28169757117798611, -2.633129923220811630, -2.592369810060399793 ) ) ;
#42968 = CIRCLE ( 'NONE', #62067, 12.18649999999999878 ) ;
#42969 = ORIENTED_EDGE ( 'NONE', *, *, #26962, .T. ) ;
#42970 = CARTESIAN_POINT ( 'NONE',  ( 2.245754705088395475, -0.1113317465207330631, 7.635057163463321750 ) ) ;
#42971 = CARTESIAN_POINT ( 'NONE',  ( 0.2648321136542695631, -12.24520788540325711, -0.1417061099916042954 ) ) ;
#42972 = ORIENTED_EDGE ( 'NONE', *, *, #17599, .T. ) ;
#42973 = FACE_OUTER_BOUND ( 'NONE', #2727, .T. ) ;
#42974 = CARTESIAN_POINT ( 'NONE',  ( -22.28482751661422867, 3.692400780723907872, -0.2989970708918196496 ) ) ;
#42975 = CARTESIAN_POINT ( 'NONE',  ( -22.31328051695926007, 2.748895659348141507, 2.608921479762082551 ) ) ;
#42976 = ORIENTED_EDGE ( 'NONE', *, *, #28228, .T. ) ;
#42977 = UNCERTAINTY_MEASURE_WITH_UNIT (LENGTH_MEASURE( 1.000000000000000082E-05 ), #58470, 'distance_accuracy_value', 'NONE');
#42978 = DIRECTION ( 'NONE',  ( 0.000000000000000000, 0.9847383929261624980, -0.1740410799127578012 ) ) ;
#42979 = ORIENTED_EDGE ( 'NONE', *, *, #19629, .T. ) ;
#42980 = COLOUR_RGB ( '', 0.31764706, 0.68627451, 0.89019608) ;
#42981 = CARTESIAN_POINT ( 'NONE',  ( 35.00000000000000000, 2.968224442958566911, 11.81949347079743440 ) ) ;
#42982 = EDGE_LOOP ( 'NONE', ( #21078, #578, #3360, #24436 ) ) ;
#42983 = VERTEX_POINT ( 'NONE', #59760 ) ;
#42984 = DIRECTION ( 'NONE',  ( -1.000000000000000000, 0.000000000000000000, 0.000000000000000000 ) ) ;
#42985 = CARTESIAN_POINT ( 'NONE',  ( 0.3218525148189839702, -12.03385614540603044, -2.370084734146341798 ) ) ;
#42986 = ORIENTED_EDGE ( 'NONE', *, *, #58501, .T. ) ;
#42987 = DIRECTION ( 'NONE',  ( 0.000000000000000000, 0.000000000000000000, 1.000000000000000000 ) ) ;
#42988 = LINE ( 'NONE', #7087, #29373 ) ;
#42989 = DIRECTION ( 'NONE',  ( 0.000000000000000000, -1.000000000000000000, 0.000000000000000000 ) ) ;
#42990 = CARTESIAN_POINT ( 'NONE',  ( 18.53913913034530125, 6.074311044188305253, 10.35926595326936628 ) ) ;
#42991 = EDGE_CURVE ( 'NONE', #38246, #3342, #38343, .T. ) ;
#42992 = ORIENTED_EDGE ( 'NONE', *, *, #22683, .T. ) ;
#42993 = VECTOR ( 'NONE', #23414, 1000.000000000000000 ) ;
#42994 = CARTESIAN_POINT ( 'NONE',  ( 0.2647959493198549508, -7.758440170207231645, 9.474789498086966688 ) ) ;
#42995 = CARTESIAN_POINT ( 'NONE',  ( -36.00000000000000711, 7.882940143791919319, -10.02106554660700333 ) ) ;
#42996 = FACE_OUTER_BOUND ( 'NONE', #44618, .T. ) ;
#42998 = EDGE_LOOP ( 'NONE', ( #35181, #18868, #26000, #27346 ) ) ;
#42997 = CARTESIAN_POINT ( 'NONE',  ( -25.54417658651491863, 4.240019242199842608, 11.22596262356930197 ) ) ;
#42999 = DIRECTION ( 'NONE',  ( 0.000000000000000000, 0.000000000000000000, 1.000000000000000000 ) ) ;
#43000 = ORIENTED_EDGE ( 'NONE', *, *, #41730, .T. ) ;
#43001 = VECTOR ( 'NONE', #40902, 1000.000000000000000 ) ;
#43002 = CARTESIAN_POINT ( 'NONE',  ( 37.00000000000000711, -5.556331110570486231, -11.47561260193575272 ) ) ;
#43003 = EDGE_LOOP ( 'NONE', ( #47784, #51853, #10387, #50904 ) ) ;
#43004 = CARTESIAN_POINT ( 'NONE',  ( 2.241526690369556984, 7.168108047190872689, -2.627393882429245320 ) ) ;
#43005 = CARTESIAN_POINT ( 'NONE',  ( 0.2647959493198541736, 4.049980114636526629, -11.55693259385002492 ) ) ;
#43006 = CIRCLE ( 'NONE', #15388, 5.000000000000000888 ) ;
#43007 = DIRECTION ( 'NONE',  ( 0.000000000000000000, 0.000000000000000000, 1.000000000000000000 ) ) ;
#43008 = CARTESIAN_POINT ( 'NONE',  ( 0.2834382757448030699, -3.999440312567289713, 11.58108645293229166 ) ) ;
#43009 = EDGE_CURVE ( 'NONE', #24268, #2113, #6012, .T. ) ;
#43010 = CARTESIAN_POINT ( 'NONE',  ( 1.372161826075867230, 8.551811013234416947, 9.274145586376221218 ) ) ;
#43011 = CARTESIAN_POINT ( 'NONE',  ( 2.000000000000001776, 4.976357229393922665, -4.652926418895522609 ) ) ;
#43012 = CARTESIAN_POINT ( 'NONE',  ( 13.37150665029400542, 12.72374181243443303, -4.532386660038074666 ) ) ;
#43013 = ORIENTED_EDGE ( 'NONE', *, *, #44428, .F. ) ;
#43014 = VERTEX_POINT ( 'NONE', #14823 ) ;
#43015 = CARTESIAN_POINT ( 'NONE',  ( 2.000000000000001776, -1.779948802829750543, -6.576141558201276993 ) ) ;
#43016 = ORIENTED_EDGE ( 'NONE', *, *, #55095, .F. ) ;
#43017 = ORIENTED_EDGE ( 'NONE', *, *, #27568, .T. ) ;
#43018 = CARTESIAN_POINT ( 'NONE',  ( 37.00000000000000711, 4.705694406421931860E-17, -3.469127814946512892E-15 ) ) ;
#43019 = CARTESIAN_POINT ( 'NONE',  ( -22.28776923226071460, 3.350304995653733187, 1.601293944844088823 ) ) ;
#43020 = CARTESIAN_POINT ( 'NONE',  ( 0.9232058338315058954, -2.536181247095282476, -12.21058493388775901 ) ) ;
#43021 = CARTESIAN_POINT ( 'NONE',  ( 5.516018279890452902, -0.002104829434640716982, 0.006440244342253021413 ) ) ;
#43022 = LINE ( 'NONE', #53679, #15716 ) ;
#43023 = DIRECTION ( 'NONE',  ( -1.000000000000000000, 0.000000000000000000, 0.000000000000000000 ) ) ;
#43024 = AXIS2_PLACEMENT_3D ( 'NONE', #32389, #1825, #35501 ) ;
#43025 = DIRECTION ( 'NONE',  ( 1.000000000000000000, 0.000000000000000000, -0.000000000000000000 ) ) ;
#43026 = ORIENTED_EDGE ( 'NONE', *, *, #52372, .T. ) ;
#43027 = CARTESIAN_POINT ( 'NONE',  ( 2.000000000000001776, 7.248432822490290306, -1.926193556692970876 ) ) ;
#43028 = CARTESIAN_POINT ( 'NONE',  ( -35.04709527796842394, -0.01232256164996302361, -0.001003525937983557048 ) ) ;
#43029 = AXIS2_PLACEMENT_3D ( 'NONE', #11507, #11192, #30788 ) ;
#43030 = EDGE_CURVE ( 'NONE', #60601, #37253, #17870, .T. ) ;
#43031 = DIRECTION ( 'NONE',  ( 0.000000000000000000, -0.8276889981568841259, -0.5611870653623918237 ) ) ;
#43032 = DIRECTION ( 'NONE',  ( -1.000000000000000000, 0.000000000000000000, 0.000000000000000000 ) ) ;
#43033 = FACE_OUTER_BOUND ( 'NONE', #11774, .T. ) ;
#43034 = DIRECTION ( 'NONE',  ( 0.000000000000000000, 0.4380125133593974485, -0.8989688749565157844 ) ) ;
#43035 = CARTESIAN_POINT ( 'NONE',  ( 5.530133899448235191, -0.001661287012793933454, -0.01589823604557703135 ) ) ;
#43036 = VERTEX_POINT ( 'NONE', #25480 ) ;
#43037 = CYLINDRICAL_SURFACE ( 'NONE', #46112, 5.000000000000000888 ) ;
#43038 = CARTESIAN_POINT ( 'NONE',  ( -29.43980975494970309, -3.641506875706030488, 11.43413432115373318 ) ) ;
#43039 = CARTESIAN_POINT ( 'NONE',  ( 0.000000000000000000, 3.786546189469178092, 5.663561025469147303 ) ) ;
#43040 = VECTOR ( 'NONE', #53893, 1000.000000000000000 ) ;
#43041 = EDGE_CURVE ( 'NONE', #24391, #16668, #29476, .T. ) ;
#43042 = FACE_OUTER_BOUND ( 'NONE', #22121, .T. ) ;
#43043 = CARTESIAN_POINT ( 'NONE',  ( 0.3675815128205912052, 3.951233083390468526, 11.62724744438066971 ) ) ;
#43044 = ORIENTED_EDGE ( 'NONE', *, *, #26026, .T. ) ;
#43045 = LINE ( 'NONE', #17790, #29103 ) ;
#43046 = DIRECTION ( 'NONE',  ( 0.000000000000000000, 0.000000000000000000, 1.000000000000000000 ) ) ;
#43047 = CARTESIAN_POINT ( 'NONE',  ( 0.3160775863651122397, 9.237902461149245070, 8.065044686487343739 ) ) ;
#43048 = CARTESIAN_POINT ( 'NONE',  ( 2.290907136833257862, 1.168459104840932961, 7.561169784528408933 ) ) ;
#43049 = ORIENTED_EDGE ( 'NONE', *, *, #37172, .F. ) ;
#43050 = DIRECTION ( 'NONE',  ( 0.000000000000000000, 0.000000000000000000, -1.000000000000000000 ) ) ;
#43051 = FACE_OUTER_BOUND ( 'NONE', #40192, .T. ) ;
#43052 = ORIENTED_EDGE ( 'NONE', *, *, #43239, .T. ) ;
#43053 = ORIENTED_EDGE ( 'NONE', *, *, #5397, .T. ) ;
#43054 = CYLINDRICAL_SURFACE ( 'NONE', #3396, 4.999999999999999112 ) ;
#43055 = CIRCLE ( 'NONE', #22917, 5.000000000000001776 ) ;
#43056 = DIRECTION ( 'NONE',  ( -1.000000000000000000, -0.000000000000000000, -0.000000000000000000 ) ) ;
#43057 = ORIENTED_EDGE ( 'NONE', *, *, #26930, .T. ) ;
#43058 = DIRECTION ( 'NONE',  ( 1.000000000000000000, 0.000000000000000000, 0.000000000000000000 ) ) ;
#43059 = CARTESIAN_POINT ( 'NONE',  ( 41.00000000000000711, -45.00200000000000244, 4.499999999999997335 ) ) ;
#43060 = LINE ( 'NONE', #53389, #30100 ) ;
#43061 = DIRECTION ( 'NONE',  ( 0.000000000000000000, 0.000000000000000000, 1.000000000000000000 ) ) ;
#43062 = ADVANCED_FACE ( 'NONE', ( #45429, #10186 ), #19222, .F. ) ;
#43063 = CARTESIAN_POINT ( 'NONE',  ( -27.47732806285103990, 11.55817606591125646, -3.277555523800877779 ) ) ;
#43064 = CARTESIAN_POINT ( 'NONE',  ( 2.241352910868909643, -0.08337961031709527349, 7.633946224498472155 ) ) ;
#43067 = ORIENTED_EDGE ( 'NONE', *, *, #57375, .T. ) ;
#43066 = CARTESIAN_POINT ( 'NONE',  ( 35.00000000000000000, 3.473736367725426266, 12.26766708251987481 ) ) ;
#43065 = B_SPLINE_CURVE_WITH_KNOTS ( 'NONE', 3,
 ( #58219, #32922, #37927, #53578, #57910, #49250, #53234, #12990, #43561, #2377, #7680, #28287, #8329, #18663, #27965, #38243, #22295, #33915, #12324 ),
 .UNSPECIFIED., .F., .F.,
 ( 4, 3, 3, 3, 3, 3, 4 ),
 ( 6.269651592512720910E-18, 2.825908398831147194E-05, 4.208813692483879805E-05, 5.591713746943844775E-05, 6.279584083231875386E-05, 9.105792820296639836E-05, 0.0001153131102488859876 ),
 .UNSPECIFIED. ) ;
#43068 = EDGE_CURVE ( 'NONE', #54831, #29266, #24858, .T. ) ;
#43069 = CARTESIAN_POINT ( 'NONE',  ( 0.8375941296815332393, 4.612912274496897780, -11.54987202580294969 ) ) ;
#43070 = ORIENTED_EDGE ( 'NONE', *, *, #48526, .T. ) ;
#43071 = CARTESIAN_POINT ( 'NONE',  ( 24.85883792449336838, 0.06046942610558726783, -12.00622078180220953 ) ) ;
#43072 = ORIENTED_EDGE ( 'NONE', *, *, #8067, .F. ) ;
#43073 = VERTEX_POINT ( 'NONE', #24497 ) ;
#43074 = CARTESIAN_POINT ( 'NONE',  ( -26.47549526795953767, 12.14959199744532192, 5.886054789876417281 ) ) ;
#43075 = CARTESIAN_POINT ( 'NONE',  ( -22.27721701579900682, 3.615531902032099065, -0.6950008646884262564 ) ) ;
#43076 = CARTESIAN_POINT ( 'NONE',  ( -24.53407633983860947, 11.34666137335572778, 7.317014004570370211 ) ) ;
#43077 = EDGE_CURVE ( 'NONE', #9614, #61242, #34778, .T. ) ;
#43078 = CARTESIAN_POINT ( 'NONE',  ( -48.61333473403968952, -0.2789806315675443793, -4.308813575818139618 ) ) ;
#43079 = FACE_OUTER_BOUND ( 'NONE', #31945, .T. ) ;
#43080 = ORIENTED_EDGE ( 'NONE', *, *, #47591, .T. ) ;
#43081 = CIRCLE ( 'NONE', #623, 17.19615242270663558 ) ;
#43082 = CARTESIAN_POINT ( 'NONE',  ( -22.27718112499583469, -0.5110808820053321933, -3.645895996548667917 ) ) ;
#43083 = FACE_OUTER_BOUND ( 'NONE', #47870, .T. ) ;
#43085 = ORIENTED_EDGE ( 'NONE', *, *, #64847, .F. ) ;
#43084 = CARTESIAN_POINT ( 'NONE',  ( 35.00000000000000000, 11.68758509253246558, -1.171570255487653700 ) ) ;
#43086 = ORIENTED_EDGE ( 'NONE', *, *, #30526, .T. ) ;
#43087 = CARTESIAN_POINT ( 'NONE',  ( 0.3665391374699467075, -4.447929964102923961, 11.44911061034385291 ) ) ;
#43088 = ORIENTED_EDGE ( 'NONE', *, *, #10726, .F. ) ;
#43089 = CARTESIAN_POINT ( 'NONE',  ( -37.00000000000000711, 7.379373053629018742, -10.39746860227882763 ) ) ;
#43090 = CARTESIAN_POINT ( 'NONE',  ( 0.2911222467163554484, 0.2144311696657358324, -12.25291251554514815 ) ) ;
#43091 = CARTESIAN_POINT ( 'NONE',  ( 9.632875692954998570, 2.208857168211140642, 13.31978269373658641 ) ) ;
#43092 = CARTESIAN_POINT ( 'NONE',  ( -22.28776923226071460, 3.061913732988073011, -2.100802264239969297 ) ) ;
#43093 = CARTESIAN_POINT ( 'NONE',  ( -37.25000000000001421, -27.53407839942726554, 1.504154570186529760 ) ) ;
#43094 = CARTESIAN_POINT ( 'NONE',  ( -27.09483304420799143, -1.923212037696908627, 1.303111346475729126 ) ) ;
#43095 = EDGE_CURVE ( 'NONE', #42211, #51152, #42542, .T. ) ;
#43096 = CARTESIAN_POINT ( 'NONE',  ( 2.268878695253353950, 3.949362208797156271, -6.544222817598178032 ) ) ;
#43097 = VERTEX_POINT ( 'NONE', #24839 ) ;
#43098 =( BOUNDED_SURFACE ( )  B_SPLINE_SURFACE ( 3, 1, ( 
 ( #37631, #11052 ),
 ( #42255, #62546 ),
 ( #21006, #11365 ),
 ( #41949, #57598 ) ),
 .UNSPECIFIED., .F., .F., .F. ) 
 B_SPLINE_SURFACE_WITH_KNOTS ( ( 4, 4 ),
 ( 2, 2 ),
 ( 0.000000000000000000, 1.000000000000000000 ),
 ( 0.000000000000000000, 1.000000000000000000 ),
 .UNSPECIFIED. ) 
 GEOMETRIC_REPRESENTATION_ITEM ( )  RATIONAL_B_SPLINE_SURFACE ( (
 ( 1.000000000000000000, 1.000000000000000000),
 ( 0.6933888150995267674, 0.9895912004443193632),
 ( 0.6933888150995267674, 0.9895912004443193632),
 ( 1.000000000000000000, 1.000000000000000000) ) ) 
 REPRESENTATION_ITEM ( '' )  SURFACE ( )  );
#43099 = FACE_OUTER_BOUND ( 'NONE', #25698, .T. ) ;
#43100 = ORIENTED_EDGE ( 'NONE', *, *, #64340, .F. ) ;
#43101 = CARTESIAN_POINT ( 'NONE',  ( -8.891032880924175430, -12.93614229090407974, -3.860857758255645589 ) ) ;
#43102 = CARTESIAN_POINT ( 'NONE',  ( 2.781367136452001620, -2.960151187464810540, -7.232043329634134210 ) ) ;
#43103 = LINE ( 'NONE', #2902, #46811 ) ;
#43104 = ORIENTED_EDGE ( 'NONE', *, *, #63676, .T. ) ;
#43105 = ORIENTED_EDGE ( 'NONE', *, *, #28790, .T. ) ;
#43106 = CARTESIAN_POINT ( 'NONE',  ( -27.09602251845210930, 0.1644056400645444449, 2.320865065108503433 ) ) ;
#43107 = VERTEX_POINT ( 'NONE', #45119 ) ;
#43108 = DIRECTION ( 'NONE',  ( -1.000000000000000000, 0.000000000000000000, 0.000000000000000000 ) ) ;
#43109 = CARTESIAN_POINT ( 'NONE',  ( 10.48620311856346454, 8.250315036047107142, 8.713914264323181058 ) ) ;
#43110 = DIRECTION ( 'NONE',  ( 0.9582930651793755139, 0.1254087680151186046, -0.2568015617827263397 ) ) ;
#43111 = CARTESIAN_POINT ( 'NONE',  ( 2.255723233588950549, 1.456523090672709797, -7.499053486174006800 ) ) ;
#43112 = ORIENTED_EDGE ( 'NONE', *, *, #3153, .F. ) ;
#43113 = FACE_OUTER_BOUND ( 'NONE', #31401, .T. ) ;
#43114 = DIRECTION ( 'NONE',  ( 0.000000000000000000, -0.01356324068817992175, 0.9999080150203990547 ) ) ;
#43115 = DIRECTION ( 'NONE',  ( -1.000000000000000000, 0.000000000000000000, -0.000000000000000000 ) ) ;
#43116 = CARTESIAN_POINT ( 'NONE',  ( -35.00000000000000000, 0.000000000000000000, 0.000000000000000000 ) ) ;
#43117 = EDGE_CURVE ( 'NONE', #53955, #40199, #40415, .T. ) ;
#43118 = AXIS2_PLACEMENT_3D ( 'NONE', #10367, #54948, #29663 ) ;
#43119 = CARTESIAN_POINT ( 'NONE',  ( 2.969415267404411196, -3.597837242549799974, 7.007431655063433240 ) ) ;
#43120 = DIRECTION ( 'NONE',  ( 1.000000000000000000, 0.000000000000000000, 0.000000000000000000 ) ) ;
#43121 = AXIS2_PLACEMENT_3D ( 'NONE', #61946, #2426, #1769 ) ;
#43122 = ORIENTED_EDGE ( 'NONE', *, *, #25027, .F. ) ;
#43123 = CARTESIAN_POINT ( 'NONE',  ( -27.08421860617808008, 1.817782142550201208, -1.394838596205214332 ) ) ;
#43124 = CARTESIAN_POINT ( 'NONE',  ( 5.536195898058073439, 0.006672323185952712399, -0.005266167600747622204 ) ) ;
#43125 = CARTESIAN_POINT ( 'NONE',  ( -11.18139917412363182, -29.23077454460525360, -7.530122743832658117 ) ) ;
#43126 = ORIENTED_EDGE ( 'NONE', *, *, #61473, .F. ) ;
#43127 = CARTESIAN_POINT ( 'NONE',  ( -10.95212338237647920, -9.902220863987562183, -6.778349501228825069 ) ) ;
#43128 = CARTESIAN_POINT ( 'NONE',  ( 1.549075743845145015, -8.652116335901308020, 9.261503792573748228 ) ) ;
#43129 = DIRECTION ( 'NONE',  ( 0.000000000000000000, 0.01356324068817991828, -0.9999080150203990547 ) ) ;
#43130 = FACE_OUTER_BOUND ( 'NONE', #7475, .T. ) ;
#43131 = DIRECTION ( 'NONE',  ( 1.000000000000000000, 0.000000000000000000, 0.000000000000000000 ) ) ;
#43132 = EDGE_CURVE ( 'NONE', #29075, #16670, #46847, .T. ) ;
#43133 = VERTEX_POINT ( 'NONE', #30466 ) ;
#43134 = ORIENTED_EDGE ( 'NONE', *, *, #14048, .F. ) ;
#43135 = CARTESIAN_POINT ( 'NONE',  ( 0.2648321136542695076, 1.986804758684115990, 12.08378267055565658 ) ) ;
#43136 = EDGE_LOOP ( 'NONE', ( #45117, #62983, #31654, #61240 ) ) ;
#43137 = LINE ( 'NONE', #58806, #17083 ) ;
#43138 = CARTESIAN_POINT ( 'NONE',  ( 0.2717059086739027629, -9.494961435243642001, -7.737372654246677861 ) ) ;
#43139 = CARTESIAN_POINT ( 'NONE',  ( 22.05617246934747300, -13.47655295422364041, -0.7978008018308943017 ) ) ;
#43140 = CARTESIAN_POINT ( 'NONE',  ( 35.00000000000000000, 4.705694406421931860E-17, -3.469127814946512892E-15 ) ) ;
#43141 = CARTESIAN_POINT ( 'NONE',  ( 35.00000000000000000, 2.936739658819871313, -11.37311665002364869 ) ) ;
#43142 = EDGE_CURVE ( 'NONE', #16581, #25502, #18186, .T. ) ;
#43143 = CARTESIAN_POINT ( 'NONE',  ( 0.3040950598368152291, 0.2511348647275649659, 12.25911170648142701 ) ) ;
#43144 = DIRECTION ( 'NONE',  ( 0.000000000000000000, -1.000000000000000000, 0.000000000000000000 ) ) ;
#43145 = VERTEX_POINT ( 'NONE', #1860 ) ;
#43146 = EDGE_CURVE ( 'NONE', #48363, #8671, #6463, .T. ) ;
#43147 = ORIENTED_EDGE ( 'NONE', *, *, #4608, .F. ) ;
#43148 = DIRECTION ( 'NONE',  ( 1.000000000000000000, 0.000000000000000000, 0.000000000000000000 ) ) ;
#43149 = VERTEX_POINT ( 'NONE', #26151 ) ;
#43150 = SHAPE_REPRESENTATION_RELATIONSHIP ( 'NONE' , 'NONE' ,  #25052, #37239 ) ;
#43151 = DIRECTION ( 'NONE',  ( 1.000000000000000000, 0.000000000000000000, 0.000000000000000000 ) ) ;
#43152 = LINE ( 'NONE', #31542, #18379 ) ;
#43153 = EDGE_CURVE ( 'NONE', #47268, #26437, #51078, .T. ) ;
#43154 = B_SPLINE_CURVE_WITH_KNOTS ( 'NONE', 3,
 ( #40234, #34903, #60523, #35245, #3734, #23990, #41216, #5685, #50576, #30584, #60867, #8, #36577, #61501, #51567, #51234, #6016, #356 ),
 .UNSPECIFIED., .F., .F.,
 ( 4, 2, 2, 2, 2, 2, 2, 2, 4 ),
 ( 4.336808689942017736E-19, 0.001378279384175299478, 0.002756558768350598522, 0.004134838152525898217, 0.005513117536701197044, 0.006891396920876495871, 0.008269676305051794699, 0.009647955689227093526, 0.01102623507340239235 ),
 .UNSPECIFIED. ) ;
#43155 = CARTESIAN_POINT ( 'NONE',  ( -9.351388602708162523, -12.99278190472486827, -3.665735721005250358 ) ) ;
#43156 = ORIENTED_EDGE ( 'NONE', *, *, #9586, .T. ) ;
#43157 = DIRECTION ( 'NONE',  ( 0.000000000000000000, -0.01356324068817998940, 0.9999080150203990547 ) ) ;
#43158 = CARTESIAN_POINT ( 'NONE',  ( 5.530133899448235191, -0.006510401266731719039, 0.01459891979722816729 ) ) ;
#43160 = ADVANCED_FACE ( 'NONE', ( #51443 ), #26462, .T. ) ;
#43159 = DIRECTION ( 'NONE',  ( -0.9688695217174487784, 0.000000000000000000, 0.2475719085175093481 ) ) ;
#43161 = EDGE_LOOP ( 'NONE', ( #58226, #31538, #65171, #20620 ) ) ;
#43162 = ORIENTED_EDGE ( 'NONE', *, *, #15248, .T. ) ;
#43163 = LINE ( 'NONE', #63440, #24710 ) ;
#43164 = ORIENTED_EDGE ( 'NONE', *, *, #40392, .T. ) ;
#43165 = CARTESIAN_POINT ( 'NONE',  ( 2.280717697723837922, 3.958470850374305350, 6.543326285614636362 ) ) ;
#43166 = ORIENTED_EDGE ( 'NONE', *, *, #48042, .F. ) ;
#43167 = CIRCLE ( 'NONE', #4981, 5.000000000000000888 ) ;
#43169 = EDGE_CURVE ( 'NONE', #12741, #26603, #26619, .T. ) ;
#43168 = ORIENTED_EDGE ( 'NONE', *, *, #38918, .F. ) ;
#43170 = CARTESIAN_POINT ( 'NONE',  ( 0.2801149460245140888, 4.374013318106550585, 11.44368419510487378 ) ) ;
#43171 = CARTESIAN_POINT ( 'NONE',  ( 2.253265082352144955, 5.007416537586165006, -5.768060979107731967 ) ) ;
#43172 = CARTESIAN_POINT ( 'NONE',  ( 0.2648978790185593790, 12.08224454301451445, -1.996248716311504801 ) ) ;
#43173 = CARTESIAN_POINT ( 'NONE',  ( 0.2869720083484385009, 8.034871682535227322, -9.251312689958684388 ) ) ;
#43174 = CARTESIAN_POINT ( 'NONE',  ( 0.2646305136544072623, -2.256625640822234047, -12.03696649559617171 ) ) ;
#43175 = CIRCLE ( 'NONE', #26197, 12.18649999999999878 ) ;
#43176 = EDGE_CURVE ( 'NONE', #46663, #23557, #11753, .T. ) ;
#43177 = DIRECTION ( 'NONE',  ( 0.000000000000000000, 0.8989688749565172277, 0.4380125133593943398 ) ) ;
#43178 = ORIENTED_EDGE ( 'NONE', *, *, #10015, .T. ) ;
#43179 = DIRECTION ( 'NONE',  ( 0.000000000000000000, 0.000000000000000000, 1.000000000000000000 ) ) ;
#43180 = CARTESIAN_POINT ( 'NONE',  ( -22.27716857039623477, 2.705892286796408364, -2.496432241075900560 ) ) ;
#43181 = EDGE_CURVE ( 'NONE', #60526, #63812, #62679, .T. ) ;
#43182 = LINE ( 'NONE', #63147, #17272 ) ;
#43183 = DIRECTION ( 'NONE',  ( -1.000000000000000000, 0.000000000000000000, -0.000000000000000000 ) ) ;
#43184 = CARTESIAN_POINT ( 'NONE',  ( 29.72982303775677337, 7.929557435711985569, 9.020309769402173217 ) ) ;
#43185 = CARTESIAN_POINT ( 'NONE',  ( 1.634816307077576081, 0.7191532042408318448, -12.68239325670243822 ) ) ;
#43186 = CARTESIAN_POINT ( 'NONE',  ( 2.491965175174250202, -4.041154086925277333, -6.575382551509628470 ) ) ;
#43187 = CARTESIAN_POINT ( 'NONE',  ( 0.2648978790185602672, -11.55204314799261311, -4.063980959785162383 ) ) ;
#43188 = DIRECTION ( 'NONE',  ( -1.000000000000000000, 0.000000000000000000, 0.000000000000000000 ) ) ;
#43189 = EDGE_LOOP ( 'NONE', ( #24363, #7011 ) ) ;
#43190 = DIRECTION ( 'NONE',  ( 0.000000000000000000, 0.01356324068818000328, -0.9999080150203990547 ) ) ;
#43191 = VERTEX_POINT ( 'NONE', #47097 ) ;
#43192 = CARTESIAN_POINT ( 'NONE',  ( 2.034671305880103809, 9.742055912616228497, 6.436604249850454984 ) ) ;
#43193 = CYLINDRICAL_SURFACE ( 'NONE', #44684, 5.000000000000000888 ) ;
#43194 = LINE ( 'NONE', #22609, #64293 ) ;
#43195 = B_SPLINE_CURVE_WITH_KNOTS ( 'NONE', 3,
 ( #63701, #2899, #29140, #64044, #33775, #64365, #8196, #18531, #9162, #3880, #59082, #34096, #38449, #19490, #49742, #18180 ),
 .UNSPECIFIED., .F., .F.,
 ( 4, 3, 3, 3, 3, 4 ),
 ( 0.000000000000000000, 0.0002999043160757258481, 0.0005998071753050843039, 0.0008997092107374322261, 0.001204458948194995658, 0.001510329163475229806 ),
 .UNSPECIFIED. ) ;
#43196 = CARTESIAN_POINT ( 'NONE',  ( 0.2651627923886314409, 9.324231535593115794, 7.938954356958122460 ) ) ;
#43197 = CARTESIAN_POINT ( 'NONE',  ( 2.241352910868908754, -6.652881166698538351, 3.744764251556969903 ) ) ;
#43198 = ORIENTED_EDGE ( 'NONE', *, *, #28656, .T. ) ;
#43199 = CARTESIAN_POINT ( 'NONE',  ( 35.00000000000000000, 10.62137734850267989, 5.015831474386340361 ) ) ;
#43200 = CARTESIAN_POINT ( 'NONE',  ( 37.00000000000000711, 11.98254675519227952, -2.220215194441947482 ) ) ;
#43201 = LINE ( 'NONE', #37895, #16297 ) ;
#43202 = CARTESIAN_POINT ( 'NONE',  ( -3.764911300353465329, 12.33769845550319921, 5.494011308154752804 ) ) ;
#43203 = EDGE_CURVE ( 'NONE', #37463, #18737, #56397, .T. ) ;
#43204 = ADVANCED_FACE ( 'NONE', ( #1210 ), #54182, .F. ) ;
#43205 = DIRECTION ( 'NONE',  ( -1.000000000000000000, 0.000000000000000000, 0.000000000000000000 ) ) ;
#43206 = CIRCLE ( 'NONE', #50676, 12.18649999999999878 ) ;
#43207 = ORIENTED_EDGE ( 'NONE', *, *, #17762, .F. ) ;
#43208 = FACE_OUTER_BOUND ( 'NONE', #51602, .T. ) ;
#43209 = DIRECTION ( 'NONE',  ( -1.000000000000000000, 0.000000000000000000, 0.000000000000000000 ) ) ;
#43210 = LINE ( 'NONE', #3677, #52197 ) ;
#43211 = EDGE_CURVE ( 'NONE', #9488, #51996, #57065, .T. ) ;
#43212 = EDGE_CURVE ( 'NONE', #59561, #57508, #57437, .T. ) ;
#43213 = VECTOR ( 'NONE', #11664, 1000.000000000000000 ) ;
#43214 = EDGE_LOOP ( 'NONE', ( #32615, #56985, #63540, #21625 ) ) ;
#43215 = CARTESIAN_POINT ( 'NONE',  ( -27.08430792439081003, 2.215465963318196785, -0.5856059198894554285 ) ) ;
#43216 = ORIENTED_EDGE ( 'NONE', *, *, #7030, .F. ) ;
#43217 = FACE_OUTER_BOUND ( 'NONE', #25568, .T. ) ;
#43218 = CARTESIAN_POINT ( 'NONE',  ( 2.241537034860906275, -5.845308934728745243, -4.910958050585496615 ) ) ;
#43219 = CARTESIAN_POINT ( 'NONE',  ( -27.08639648637142017, -1.635407781266639660, -1.614109828502286570 ) ) ;
#43220 = CARTESIAN_POINT ( 'NONE',  ( 0.4613984246114889998, -7.694922453052204681, 9.610550265395824354 ) ) ;
#43221 = CARTESIAN_POINT ( 'NONE',  ( -22.28939870658739864, -2.099199915896300173, -3.068935452695167321 ) ) ;
#43222 = EDGE_LOOP ( 'NONE', ( #8996, #30084, #31360, #11992 ) ) ;
#43223 = EDGE_CURVE ( 'NONE', #22151, #51572, #62729, .T. ) ;
#43224 = VERTEX_POINT ( 'NONE', #5891 ) ;
#43225 = EDGE_LOOP ( 'NONE', ( #11982, #5914, #6389, #58288 ) ) ;
#43226 = CARTESIAN_POINT ( 'NONE',  ( 2.290907136833254309, 7.243397831411281906, -2.463690939638600419 ) ) ;
#43227 = CARTESIAN_POINT ( 'NONE',  ( -27.30975859563925212, 13.34112994997249757, -2.066478916269103294 ) ) ;
#43228 = VERTEX_POINT ( 'NONE', #31456 ) ;
#43229 = DIRECTION ( 'NONE',  ( 0.000000000000000000, -1.000000000000000000, 0.000000000000000000 ) ) ;
#43230 = CARTESIAN_POINT ( 'NONE',  ( -35.00000000000000000, 11.23004253107764505, 4.732539170486304236 ) ) ;
#43231 = ORIENTED_EDGE ( 'NONE', *, *, #30529, .T. ) ;
#43232 = CARTESIAN_POINT ( 'NONE',  ( 0.2650492594609233366, 11.54478160586242907, -4.084774262245968401 ) ) ;
#43234 = EDGE_CURVE ( 'NONE', #20539, #64321, #51757, .T. ) ;
#43233 = CARTESIAN_POINT ( 'NONE',  ( -37.00000000000000711, -10.80478261802186246, 5.636262487437281976 ) ) ;
#43235 = CARTESIAN_POINT ( 'NONE',  ( 2.000000000000001776, 5.662015959325269243, -4.918493191653929841 ) ) ;
#43236 = ORIENTED_EDGE ( 'NONE', *, *, #44870, .T. ) ;
#43237 = VERTEX_POINT ( 'NONE', #21139 ) ;
#43238 = CARTESIAN_POINT ( 'NONE',  ( 0.2851083653049504285, -0.4107471485392698018, 11.99296822225285730 ) ) ;
#43240 = EDGE_LOOP ( 'NONE', ( #12015, #37987, #36543, #12631 ) ) ;
#43239 = EDGE_CURVE ( 'NONE', #7090, #57074, #56377, .T. ) ;
#43241 = CARTESIAN_POINT ( 'NONE',  ( 8.626688775007931298, 3.155910342056009732, -13.12853318357805676 ) ) ;
#43242 = ORIENTED_EDGE ( 'NONE', *, *, #42947, .T. ) ;
#43243 = CARTESIAN_POINT ( 'NONE',  ( -35.00000000000000000, 11.42599468261435192, -4.237620530777677530 ) ) ;
#43244 = EDGE_CURVE ( 'NONE', #14627, #217, #21827, .T. ) ;
#43245 = CARTESIAN_POINT ( 'NONE',  ( 0.000000000000000000, 0.000000000000000000, 0.000000000000000000 ) ) ;
#43246 = CARTESIAN_POINT ( 'NONE',  ( -35.00000000000000000, 4.603882218679707705, -10.80631716521661900 ) ) ;
#43247 = DIRECTION ( 'NONE',  ( 0.000000000000000000, 0.000000000000000000, -1.000000000000000000 ) ) ;
#43248 = CARTESIAN_POINT ( 'NONE',  ( 0.8320506296491577691, 11.54877388447410702, -4.610676791972224464 ) ) ;
#43249 = CARTESIAN_POINT ( 'NONE',  ( -22.71097035706202405, -4.965150228107763297, -0.4203397252017324615 ) ) ;
#43250 = CARTESIAN_POINT ( 'NONE',  ( -27.01437459610461644, -11.79277645698183186, -2.220455681983952267 ) ) ;
#43251 = EDGE_LOOP ( 'NONE', ( #4005, #64524, #4033, #19628 ) ) ;
#43252 = ADVANCED_FACE ( 'NONE', ( #57388 ), #11814, .T. ) ;
#43253 = CYLINDRICAL_SURFACE ( 'NONE', #27989, 12.75000000000000178 ) ;
#43254 = VERTEX_POINT ( 'NONE', #49071 ) ;
#43255 = DIRECTION ( 'NONE',  ( 0.000000000000000000, -0.01356324068817998940, 0.9999080150203990547 ) ) ;
#43256 = CARTESIAN_POINT ( 'NONE',  ( -37.00000000000000711, 9.076753354954126607, -8.954052073409506818 ) ) ;
#43257 = ADVANCED_FACE ( 'NONE', ( #59348 ), #53388, .T. ) ;
#43258 = VERTEX_POINT ( 'NONE', #3846 ) ;
#43259 = DIRECTION ( 'NONE',  ( 0.000000000000000000, 0.1764146379942750087, 0.9843159429275484262 ) ) ;
#43260 = CARTESIAN_POINT ( 'NONE',  ( 0.3057689695767449312, 6.328747727191191608, 10.49983108339462845 ) ) ;
#43261 = LINE ( 'NONE', #64217, #32289 ) ;
#43262 = AXIS2_PLACEMENT_3D ( 'NONE', #61402, #51475, #20852 ) ;
#43263 = VERTEX_POINT ( 'NONE', #58049 ) ;
#43264 = VERTEX_POINT ( 'NONE', #23792 ) ;
#43265 = VECTOR ( 'NONE', #35776, 1000.000000000000000 ) ;
#43266 = DIRECTION ( 'NONE',  ( 0.000000000000000000, -0.6943713148249532896, 0.7196168960969895334 ) ) ;
#43267 = VERTEX_POINT ( 'NONE', #48077 ) ;
#43268 = LINE ( 'NONE', #24304, #52965 ) ;
#43269 = DIRECTION ( 'NONE',  ( 1.000000000000000000, 0.000000000000000000, 0.000000000000000000 ) ) ;
#43270 = CARTESIAN_POINT ( 'NONE',  ( 2.241352910868908754, -1.243507963608043498, -7.532448145350521429 ) ) ;
#43271 = CARTESIAN_POINT ( 'NONE',  ( 35.00000000000000000, 9.390600770288113353, 8.624332853795948495 ) ) ;
#43272 = CARTESIAN_POINT ( 'NONE',  ( 2.000000000000001776, -3.073484823194281290, -6.841322316745092280 ) ) ;
#43273 = VERTEX_POINT ( 'NONE', #18134 ) ;
#43274 = FACE_OUTER_BOUND ( 'NONE', #10403, .T. ) ;
#43275 = ADVANCED_FACE ( 'NONE', ( #63021 ), #17482, .F. ) ;
#43276 = EDGE_CURVE ( 'NONE', #55375, #32360, #7837, .T. ) ;
#43277 =( BOUNDED_SURFACE ( )  B_SPLINE_SURFACE ( 3, 1, ( 
 ( #43124, #38808 ),
 ( #49462, #3247 ),
 ( #28183, #18853 ),
 ( #63402, #59106 ) ),
 .UNSPECIFIED., .F., .F., .F. ) 
 B_SPLINE_SURFACE_WITH_KNOTS ( ( 4, 4 ),
 ( 2, 2 ),
 ( 0.000000000000000000, 1.000000000000000000 ),
 ( 0.000000000000000000, 1.000000000000000000 ),
 .UNSPECIFIED. ) 
 GEOMETRIC_REPRESENTATION_ITEM ( )  RATIONAL_B_SPLINE_SURFACE ( (
 ( 1.000000000000000000, 1.000000000000000000),
 ( 0.6933888150995267674, 0.9895912004443193632),
 ( 0.6933888150995267674, 0.9895912004443193632),
 ( 1.000000000000000000, 1.000000000000000000) ) ) 
 REPRESENTATION_ITEM ( '' )  SURFACE ( )  );
#43278 = CARTESIAN_POINT ( 'NONE',  ( 1.014403380171158497, -26.55354399125275577, -16.22408933255776731 ) ) ;
#43279 = DIRECTION ( 'NONE',  ( 1.000000000000000000, 0.000000000000000000, 0.000000000000000000 ) ) ;
#43280 = CARTESIAN_POINT ( 'NONE',  ( 0.2646305136544065406, -1.996350543473074390, 12.08286001766534667 ) ) ;
#43281 = DIRECTION ( 'NONE',  ( -1.000000000000000000, -1.836970198721029688E-16, 0.000000000000000000 ) ) ;
#43282 = LINE ( 'NONE', #38967, #60129 ) ;
#43283 = CARTESIAN_POINT ( 'NONE',  ( 2.000000000000001776, -6.777474576704061171, -0.6925993764991672519 ) ) ;
#43284 = EDGE_CURVE ( 'NONE', #4396, #57223, #7482, .T. ) ;
#43285 = CIRCLE ( 'NONE', #49673, 5.000000000000000000 ) ;
#43286 = VERTEX_POINT ( 'NONE', #48408 ) ;
#43287 = CARTESIAN_POINT ( 'NONE',  ( 2.261269890822071194, -0.1394916642590379452, 7.639767381742377239 ) ) ;
#43288 = CIRCLE ( 'NONE', #57133, 5.000000000000001776 ) ;
#43289 = EDGE_LOOP ( 'NONE', ( #46515, #26784, #57409, #29044 ) ) ;
#43291 =( BOUNDED_CURVE ( )  B_SPLINE_CURVE ( 3, ( #23901, #13257, #18898, #39159 ),
 .UNSPECIFIED., .F., .F. ) 
 B_SPLINE_CURVE_WITH_KNOTS ( ( 4, 4 ),
 ( 1.570796326794895892, 1.607646890824687924 ),
 .UNSPECIFIED. ) 
 CURVE ( )  GEOMETRIC_REPRESENTATION_ITEM ( )  RATIONAL_B_SPLINE_CURVE ( ( 1.000000000000000000, 0.9998868395290251287, 0.9998868395290251287, 1.000000000000000000 ) ) 
 REPRESENTATION_ITEM ( '' )  );
#43290 = CARTESIAN_POINT ( 'NONE',  ( 0.3057689695767459304, 1.901059295891078804, -12.11137787899271245 ) ) ;
#43292 = CARTESIAN_POINT ( 'NONE',  ( -37.00000000000000711, 6.415447294506705589, 11.01837265713075631 ) ) ;
#43293 = CARTESIAN_POINT ( 'NONE',  ( -37.00000000000000711, 5.636262487437317503, 10.80478261802183937 ) ) ;
#43294 = ORIENTED_EDGE ( 'NONE', *, *, #30462, .F. ) ;
#43295 = DIRECTION ( 'NONE',  ( -1.000000000000000000, -0.000000000000000000, 0.000000000000000000 ) ) ;
#43296 = ORIENTED_EDGE ( 'NONE', *, *, #49533, .F. ) ;
#43297 = EDGE_CURVE ( 'NONE', #42115, #41622, #35713, .T. ) ;
#43298 = CARTESIAN_POINT ( 'NONE',  ( -17.19056858472901084, 2.658600115333382252, 11.70257571668042473 ) ) ;
#43299 = ORIENTED_EDGE ( 'NONE', *, *, #43531, .F. ) ;
#43300 = CIRCLE ( 'NONE', #22096, 7.499999999999988454 ) ;
#43301 = VERTEX_POINT ( 'NONE', #12464 ) ;
#43302 = CARTESIAN_POINT ( 'NONE',  ( -10.82054232775603708, -8.517672224558221927, -8.456986271403620137 ) ) ;
#43303 = ADVANCED_FACE ( 'NONE', ( #8813 ), #28423, .T. ) ;
#43304 = CARTESIAN_POINT ( 'NONE',  ( 2.269879328256731554, -7.130835954829864320, 2.753278809616085177 ) ) ;
#43305 = B_SPLINE_CURVE_WITH_KNOTS ( 'NONE', 3,
 ( #1536, #22112, #12449, #7146, #21812, #17467, #57371 ),
 .UNSPECIFIED., .F., .F.,
 ( 4, 3, 4 ),
 ( 8.074120965598165776E-15, 0.002398160485434909592, 0.005002426799384971333 ),
 .UNSPECIFIED. ) ;
#43306 = AXIS2_PLACEMENT_3D ( 'NONE', #41107, #9531, #61391 ) ;
#43307 = VERTEX_POINT ( 'NONE', #28115 ) ;
#43308 = CARTESIAN_POINT ( 'NONE',  ( 2.705197763288543111, 5.783040721897930503, 5.217779042888458285 ) ) ;
#43309 = CARTESIAN_POINT ( 'NONE',  ( 2.963017218115624463, -3.051711603120581984, 7.259628195185923616 ) ) ;
#43310 = CARTESIAN_POINT ( 'NONE',  ( 2.000000000000001776, 0.000000000000000000, 0.000000000000000000 ) ) ;
#43311 = CARTESIAN_POINT ( 'NONE',  ( 2.000000000000001776, -3.786546189469129686, -5.663561025469209476 ) ) ;
#43312 = ORIENTED_EDGE ( 'NONE', *, *, #1302, .T. ) ;
#43313 = CARTESIAN_POINT ( 'NONE',  ( 0.3109076770649005228, -7.699281309344391921, 9.542672295796789328 ) ) ;
#43314 = CARTESIAN_POINT ( 'NONE',  ( -35.00000000000000000, 5.644643009979071202, 10.30098186818251982 ) ) ;
#43315 = FACE_OUTER_BOUND ( 'NONE', #34259, .T. ) ;
#43317 = ORIENTED_EDGE ( 'NONE', *, *, #25382, .F. ) ;
#43316 = DIRECTION ( 'NONE',  ( -1.000000000000000000, 0.000000000000000000, 0.000000000000000000 ) ) ;
#43318 = CARTESIAN_POINT ( 'NONE',  ( 0.2638984909335720941, 4.001111175853898416, -11.57533005135174875 ) ) ;
#43319 = ORIENTED_EDGE ( 'NONE', *, *, #40282, .T. ) ;
#43320 = CARTESIAN_POINT ( 'NONE',  ( -35.00000000000000000, 0.000000000000000000, 0.000000000000000000 ) ) ;
#43321 = VERTEX_POINT ( 'NONE', #48725 ) ;
#43322 = CARTESIAN_POINT ( 'NONE',  ( -10.00000000000000178, 0.000000000000000000, 0.000000000000000000 ) ) ;
#43323 = CARTESIAN_POINT ( 'NONE',  ( 47.00000000000000711, 4.705694406421931860E-17, -3.469127814946512892E-15 ) ) ;
#43324 = ADVANCED_FACE ( 'NONE', ( #32736 ), #53046, .T. ) ;
#43325 = DIRECTION ( 'NONE',  ( -1.000000000000000000, 0.000000000000000000, 0.000000000000000000 ) ) ;
#43326 = DIRECTION ( 'NONE',  ( 0.000000000000000000, 0.01356324068817992175, -0.9999080150203990547 ) ) ;
#43327 = CARTESIAN_POINT ( 'NONE',  ( 0.3223008802179294641, 9.550960164375604577, 7.695050880595522003 ) ) ;
#43328 = CARTESIAN_POINT ( 'NONE',  ( 37.00000000000000711, -1.903127969211267700, -11.59095880812007628 ) ) ;
#43329 = CARTESIAN_POINT ( 'NONE',  ( -37.00000000000000711, 6.564808257521928425, -10.93004082984011482 ) ) ;
#43330 = EDGE_CURVE ( 'NONE', #48271, #39541, #49562, .T. ) ;
#43331 = VERTEX_POINT ( 'NONE', #22805 ) ;
#43332 = LINE ( 'NONE', #64282, #4061 ) ;
#43333 = ORIENTED_EDGE ( 'NONE', *, *, #41675, .T. ) ;
#43334 = ADVANCED_FACE ( 'NONE', ( #49406 ), #58876, .F. ) ;
#43335 = ORIENTED_EDGE ( 'NONE', *, *, #615, .T. ) ;
#43336 = CARTESIAN_POINT ( 'NONE',  ( 1.104777566491144558, 1.703053712365489858, -12.40974092093470382 ) ) ;
#43337 = CARTESIAN_POINT ( 'NONE',  ( -22.30078715814471835, 3.372109767220915266, 1.645949880549380850 ) ) ;
#43338 = CARTESIAN_POINT ( 'NONE',  ( 5.516018279890452902, -0.005042957932158615743, 0.004525000489649755146 ) ) ;
#43339 = CARTESIAN_POINT ( 'NONE',  ( -22.28629837673888048, 2.102970853432577059, 3.055064048018781175 ) ) ;
#43340 = DIRECTION ( 'NONE',  ( 0.000000000000000000, 0.000000000000000000, 1.000000000000000000 ) ) ;
#43341 = TOROIDAL_SURFACE ( 'NONE', #11487, 5.000000000000000888, 19.00000000000000000 ) ;
#43342 = CARTESIAN_POINT ( 'NONE',  ( 1.452237505248555660, 12.08199618361513039, 3.767214359061165307 ) ) ;
#43343 = EDGE_CURVE ( 'NONE', #14197, #27631, #52045, .T. ) ;
#43344 = DIRECTION ( 'NONE',  ( 0.000000000000000000, 0.3218879778915905709, -0.9467777615094595811 ) ) ;
#43345 = AXIS2_PLACEMENT_3D ( 'NONE', #7214, #42129, #11881 ) ;
#43346 = ORIENTED_EDGE ( 'NONE', *, *, #12221, .T. ) ;
#43347 = CARTESIAN_POINT ( 'NONE',  ( 0.2646305136544065406, 2.256625640822475631, -12.03696649559612375 ) ) ;
#43348 = CARTESIAN_POINT ( 'NONE',  ( -35.00000000000000000, -3.704519465651227694, -11.60979404548638705 ) ) ;
#43349 = CIRCLE ( 'NONE', #40112, 12.18649999999999878 ) ;
#43350 = CARTESIAN_POINT ( 'NONE',  ( 6.361445718264521432, -4.355102044641763648, -11.18181944858513077 ) ) ;
#43351 = AXIS2_PLACEMENT_3D ( 'NONE', #27395, #16461, #47050 ) ;
#43352 = CARTESIAN_POINT ( 'NONE',  ( 2.247112776671472467, -4.818685025480685447, 5.923998863713047847 ) ) ;
#43353 = DIRECTION ( 'NONE',  ( -1.000000000000000000, 0.000000000000000000, 0.000000000000000000 ) ) ;
#43354 = EDGE_CURVE ( 'NONE', #13777, #9473, #32101, .T. ) ;
#43355 = LINE ( 'NONE', #27741, #27750 ) ;
#43356 = CARTESIAN_POINT ( 'NONE',  ( -10.90165637462999904, -7.508992741355384304, 11.21895841913464587 ) ) ;
#43357 = ORIENTED_EDGE ( 'NONE', *, *, #32732, .F. ) ;
#43358 = DIRECTION ( 'NONE',  ( 1.000000000000000000, 0.000000000000000000, 0.000000000000000000 ) ) ;
#43359 = CARTESIAN_POINT ( 'NONE',  ( -37.00000000000000711, 0.000000000000000000, 0.000000000000000000 ) ) ;
#43360 = CARTESIAN_POINT ( 'NONE',  ( -22.27834755396594346, -0.5583491773602533570, -3.643689482009672798 ) ) ;
#43361 = AXIS2_PLACEMENT_3D ( 'NONE', #43945, #8698, #39601 ) ;
#43362 = CARTESIAN_POINT ( 'NONE',  ( -25.69594172210742045, 5.442502809504032868, 10.70006412471200719 ) ) ;
#43363 = DIRECTION ( 'NONE',  ( 0.000000000000000000, -0.01356324068817998940, 0.9999080150203990547 ) ) ;
#43364 = ORIENTED_EDGE ( 'NONE', *, *, #26432, .F. ) ;
#43365 = AXIS2_PLACEMENT_3D ( 'NONE', #33114, #22834, #26823 ) ;
#43366 = DIRECTION ( 'NONE',  ( 0.000000000000000000, 0.000000000000000000, 1.000000000000000000 ) ) ;
#43367 = CARTESIAN_POINT ( 'NONE',  ( 25.00000000000000355, -9.999999999999998224, -5.000000000000000888 ) ) ;
#43368 = DIRECTION ( 'NONE',  ( -0.000000000000000000, -0.000000000000000000, -1.000000000000000000 ) ) ;
#43369 = ORIENTED_EDGE ( 'NONE', *, *, #49684, .T. ) ;
#43370 = CARTESIAN_POINT ( 'NONE',  ( -35.00000000000000000, 0.4871980014163251327, -12.74068829017553384 ) ) ;
#43371 = CARTESIAN_POINT ( 'NONE',  ( -27.35552965826137140, -1.773915698030568366, 2.548625910254532112 ) ) ;
#43372 = ORIENTED_EDGE ( 'NONE', *, *, #60658, .T. ) ;
#43373 = ADVANCED_FACE ( 'NONE', ( #5136 ), #15092, .T. ) ;
#43374 = ORIENTED_EDGE ( 'NONE', *, *, #54969, .F. ) ;
#43375 = DIRECTION ( 'NONE',  ( -1.000000000000000000, 0.000000000000000000, -0.000000000000000000 ) ) ;
#43376 = ADVANCED_FACE ( 'NONE', ( #50692 ), #4150, .F. ) ;
#43377 = VECTOR ( 'NONE', #62590, 1000.000000000000000 ) ;
#43378 = ORIENTED_EDGE ( 'NONE', *, *, #12198, .T. ) ;
#43379 = CARTESIAN_POINT ( 'NONE',  ( -27.45775109278351067, 25.00000000000000000, -8.471355351200609007 ) ) ;
#43380 = CARTESIAN_POINT ( 'NONE',  ( 5.514970785353741078, 0.001326349372336293846, -0.004532877335078717637 ) ) ;
#43381 = VECTOR ( 'NONE', #20312, 1000.000000000000000 ) ;
#43382 = DIRECTION ( 'NONE',  ( -1.000000000000000000, 0.000000000000000000, 0.000000000000000000 ) ) ;
#43383 = AXIS2_PLACEMENT_3D ( 'NONE', #61315, #19461, #31062 ) ;
#43384 = CARTESIAN_POINT ( 'NONE',  ( 2.000000000000001776, 0.4804830611970945520, -6.919838746524566986 ) ) ;
#43385 = CARTESIAN_POINT ( 'NONE',  ( -2.952869152607106251, -11.39722960915210592, 3.755417052241485365 ) ) ;
#43387 = EDGE_LOOP ( 'NONE', ( #25229, #63748 ) ) ;
#43386 = CARTESIAN_POINT ( 'NONE',  ( -28.67667724226168602, -0.1214114860980438498, -1.888227992976680980 ) ) ;
#43388 = CARTESIAN_POINT ( 'NONE',  ( 0.4626703367448694038, 4.475905684074013458, -11.46957824750464638 ) ) ;
#43389 = EDGE_LOOP ( 'NONE', ( #52079, #48511, #23718, #49030 ) ) ;
#43390 = CARTESIAN_POINT ( 'NONE',  ( -35.00000000000000000, 0.000000000000000000, 0.000000000000000000 ) ) ;
#43391 = ORIENTED_EDGE ( 'NONE', *, *, #26567, .T. ) ;
#43392 = AXIS2_PLACEMENT_3D ( 'NONE', #63783, #18611, #13891 ) ;
#43393 = EDGE_LOOP ( 'NONE', ( #20832, #64180, #57901, #2560 ) ) ;
#43394 = APPLICATION_PROTOCOL_DEFINITION ( 'draft international standard', 'automotive_design', 1998, #36599 ) ;
#43395 = CARTESIAN_POINT ( 'NONE',  ( -17.05443611520388103, 7.955356801464462890, 10.90867276502668659 ) ) ;
#43396 = CARTESIAN_POINT ( 'NONE',  ( -2.264138978095803445, -30.62783502483855358, 15.20150737401304575 ) ) ;
#43397 = ADVANCED_FACE ( 'NONE', ( #10115 ), #60012, .T. ) ;
#43398 = DIRECTION ( 'NONE',  ( -1.000000000000000000, -0.000000000000000000, 0.000000000000000000 ) ) ;
#43399 = CARTESIAN_POINT ( 'NONE',  ( 23.56751799445461870, 2.000530838575146575, 11.83544039284797478 ) ) ;
#43400 = CARTESIAN_POINT ( 'NONE',  ( 35.00000000000000000, 0.7536123767498499326, -11.72195762423410414 ) ) ;
#43401 = DIRECTION ( 'NONE',  ( 1.000000000000000000, 0.000000000000000000, -0.000000000000000000 ) ) ;
#43402 = ORIENTED_EDGE ( 'NONE', *, *, #14446, .F. ) ;
#43403 = CARTESIAN_POINT ( 'NONE',  ( -22.27721038036499834, 0.5802312083658667241, 3.635620891621732298 ) ) ;
#43404 = CARTESIAN_POINT ( 'NONE',  ( 0.000000000000000000, 0.000000000000000000, 0.000000000000000000 ) ) ;
#43405 = CYLINDRICAL_SURFACE ( 'NONE', #37973, 12.18649999999999878 ) ;
#43406 = EDGE_LOOP ( 'NONE', ( #61326, #57011, #21584, #56632 ) ) ;
#43407 = DIRECTION ( 'NONE',  ( 0.000000000000000000, 0.01356324068817992001, -0.9999080150203990547 ) ) ;
#43408 = ORIENTED_EDGE ( 'NONE', *, *, #39106, .T. ) ;
#43409 = CARTESIAN_POINT ( 'NONE',  ( 35.00000000000000000, 9.430788938294046631, -7.718225330433843290 ) ) ;
#43410 = DIRECTION ( 'NONE',  ( -1.000000000000000000, 0.000000000000000000, 0.000000000000000000 ) ) ;
#43411 = DIRECTION ( 'NONE',  ( 1.000000000000000000, 0.000000000000000000, -0.000000000000000000 ) ) ;
#43412 = CARTESIAN_POINT ( 'NONE',  ( -27.32337605527169089, -2.771816950947471714, 1.175835497774979643 ) ) ;
#43413 = EDGE_CURVE ( 'NONE', #20510, #35691, #29723, .T. ) ;
#43414 = CARTESIAN_POINT ( 'NONE',  ( 5.536195898058073439, -0.006344799443923397099, -0.005656495196970955271 ) ) ;
#43415 = CARTESIAN_POINT ( 'NONE',  ( -27.09861164373156228, -1.936722219471109785, 1.303360234155833464 ) ) ;
#43416 = AXIS2_PLACEMENT_3D ( 'NONE', #56551, #30289, #5026 ) ;
#43417 = CARTESIAN_POINT ( 'NONE',  ( -7.287102677926684535, -8.374986170366028659, -10.59034548381062812 ) ) ;
#43418 = ORIENTED_EDGE ( 'NONE', *, *, #57899, .T. ) ;
#43419 = DIRECTION ( 'NONE',  ( -1.000000000000000000, 0.000000000000000000, 0.000000000000000000 ) ) ;
#43420 = CIRCLE ( 'NONE', #54020, 5.000000000000000000 ) ;
#43421 = ORIENTED_EDGE ( 'NONE', *, *, #35035, .F. ) ;
#43422 = CYLINDRICAL_SURFACE ( 'NONE', #53002, 2.899999999999994582 ) ;
#43423 = CARTESIAN_POINT ( 'NONE',  ( 2.430348790457534935, 4.796903114819468072, -6.019963855523847940 ) ) ;
#43424 = CYLINDRICAL_SURFACE ( 'NONE', #64834, 5.000000000000000888 ) ;
#43425 = CIRCLE ( 'NONE', #17958, 12.74999999999999822 ) ;
#43426 = AXIS2_PLACEMENT_3D ( 'NONE', #53471, #22543, #16887 ) ;
#43427 = CARTESIAN_POINT ( 'NONE',  ( 37.00000000000000711, 12.57916205664484188, 2.080187960898425281 ) ) ;
#43428 = CARTESIAN_POINT ( 'NONE',  ( -27.09252613521643127, 0.1722886739160412184, 2.309775830546432651 ) ) ;
#43429 = AXIS2_PLACEMENT_3D ( 'NONE', #20230, #25894, #46489 ) ;
#43430 = EDGE_CURVE ( 'NONE', #57779, #6123, #50599, .T. ) ;
#43431 = ORIENTED_EDGE ( 'NONE', *, *, #31371, .F. ) ;
#43432 = CARTESIAN_POINT ( 'NONE',  ( 0.2834382757448023482, 7.719209397492100777, -9.514772331577340481 ) ) ;
#43433 = CARTESIAN_POINT ( 'NONE',  ( -27.09252613521643127, -2.086468883258537410, -1.005681546877608579 ) ) ;
#43434 = EDGE_CURVE ( 'NONE', #48464, #43665, #44221, .T. ) ;
#43435 = CARTESIAN_POINT ( 'NONE',  ( 35.00000000000000000, -9.321877890560486435, -7.146664589317880178 ) ) ;
#43436 = ORIENTED_EDGE ( 'NONE', *, *, #42392, .T. ) ;
#43437 = CARTESIAN_POINT ( 'NONE',  ( 0.2648978790185602672, -6.237101853238473659, -10.53870023327869987 ) ) ;
#43438 = DIRECTION ( 'NONE',  ( 0.3865475372811021382, 0.8730852074079760161, -0.2971585806051821321 ) ) ;
#43439 = CARTESIAN_POINT ( 'NONE',  ( 37.00000000000000711, 0.1652884326465054732, -12.18537902504609427 ) ) ;
#43440 = AXIS2_PLACEMENT_3D ( 'NONE', #27734, #23758, #48381 ) ;
#43441 = LINE ( 'NONE', #33488, #48726 ) ;
#43442 = EDGE_CURVE ( 'NONE', #12647, #61044, #43175, .T. ) ;
#43443 = CARTESIAN_POINT ( 'NONE',  ( 2.288423627607479194, -0.1612945702821226845, -7.648392725410196213 ) ) ;
#43444 = DIRECTION ( 'NONE',  ( -1.000000000000000000, 0.000000000000000000, 0.000000000000000000 ) ) ;
#43445 = ORIENTED_EDGE ( 'NONE', *, *, #50092, .F. ) ;
#43446 = DIRECTION ( 'NONE',  ( -1.000000000000000000, -1.836970198721029688E-16, 0.000000000000000000 ) ) ;
#43447 = CARTESIAN_POINT ( 'NONE',  ( 29.73007324000527873, 9.884457442835744345, 9.197707082462885708 ) ) ;
#43448 = CARTESIAN_POINT ( 'NONE',  ( -1.729917593620911020, -27.85289612474432275, -12.49635169356267106 ) ) ;
#43449 = ORIENTED_EDGE ( 'NONE', *, *, #61162, .F. ) ;
#43450 = CARTESIAN_POINT ( 'NONE',  ( -17.59645119676047287, 3.550355928000697325, -13.02595742310721150 ) ) ;
#43451 = CARTESIAN_POINT ( 'NONE',  ( 37.00000000000000711, 4.705694406421931860E-17, -3.469127814946512892E-15 ) ) ;
#43452 = CARTESIAN_POINT ( 'NONE',  ( 2.941278708680199916, -5.248410529370246991, 3.185832147968428618 ) ) ;
#43453 = EDGE_CURVE ( 'NONE', #16210, #29920, #45683, .T. ) ;
#43454 = DIRECTION ( 'NONE',  ( 0.000000000000000000, 0.01356324068817998940, -0.9999080150203990547 ) ) ;
#43455 = DIRECTION ( 'NONE',  ( 1.000000000000000000, 0.000000000000000000, -0.000000000000000000 ) ) ;
#43456 = VERTEX_POINT ( 'NONE', #64637 ) ;
#43457 = DIRECTION ( 'NONE',  ( 0.000000000000000000, 0.01356324068817998940, -0.9999080150203990547 ) ) ;
#43458 = B_SPLINE_CURVE_WITH_KNOTS ( 'NONE', 3,
 ( #49886, #24946, #35562, #20613, #51212, #29919, #65480, #30255, #4337, #24610, #55856, #10286, #30565, #45882, #44887, #40891 ),
 .UNSPECIFIED., .F., .F.,
 ( 4, 3, 3, 3, 3, 4 ),
 ( 8.673617379884035472E-19, 0.0002176109881720219099, 0.0004352086762394569803, 0.0006528017811446825205, 0.0007615147961451645790, 0.0009453342004947430264 ),
 .UNSPECIFIED. ) ;
#43459 = ORIENTED_EDGE ( 'NONE', *, *, #16319, .T. ) ;
#43460 = CARTESIAN_POINT ( 'NONE',  ( 1.452237505248552996, -2.778494755359138146, 12.34692280296791189 ) ) ;
#43461 = CARTESIAN_POINT ( 'NONE',  ( 0.2767916011545398236, -9.504925141026303592, -7.727819755721567319 ) ) ;
#43462 = CARTESIAN_POINT ( 'NONE',  ( -35.00000000000000000, -3.307597835713157242, -12.31350058095526734 ) ) ;
#43463 = CARTESIAN_POINT ( 'NONE',  ( 0.9232167919969144210, 3.872606616958433445, -11.84868134597554246 ) ) ;
#43464 = CARTESIAN_POINT ( 'NONE',  ( 35.00000000000000000, 11.65150730582934635, 1.488153103997001514 ) ) ;
#43465 = CARTESIAN_POINT ( 'NONE',  ( 2.273267844204862165, -1.178226273332996898, 7.553702825375862240 ) ) ;
#43466 = CARTESIAN_POINT ( 'NONE',  ( 5.515188684475870851, -0.005320786921497683807, -0.0005703990286339872965 ) ) ;
#43467 = EDGE_LOOP ( 'NONE', ( #49941, #34981, #43335, #22046 ) ) ;
#43468 = ORIENTED_EDGE ( 'NONE', *, *, #48689, .F. ) ;
#43469 = CARTESIAN_POINT ( 'NONE',  ( 5.516018279890452902, -0.002527316374434336339, 0.006286471671802434068 ) ) ;
#43470 = ORIENTED_EDGE ( 'NONE', *, *, #17993, .T. ) ;
#43471 =( NAMED_UNIT ( * ) SI_UNIT ( $, .STERADIAN. ) SOLID_ANGLE_UNIT ( ) );
#43472 = CARTESIAN_POINT ( 'NONE',  ( -22.29018399051993882, 2.585196332786391160, -2.675685774027734887 ) ) ;
#43473 = VECTOR ( 'NONE', #26626, 1000.000000000000000 ) ;
#43474 = CARTESIAN_POINT ( 'NONE',  ( 37.00000000000000711, -2.021542716731485001, -12.01765980939841505 ) ) ;
#43475 = CARTESIAN_POINT ( 'NONE',  ( -18.25006854224444908, -9.443202773001939221, -9.647586298549935435 ) ) ;
#43477 = ORIENTED_EDGE ( 'NONE', *, *, #34159, .F. ) ;
#43476 = CONICAL_SURFACE ( 'NONE', #37121, 7.938172270156617749, 1.280189991382167047 ) ;
#43478 = CARTESIAN_POINT ( 'NONE',  ( 0.3223008802179238019, 5.919638939520732279, -10.74209118105750882 ) ) ;
#43479 =( BOUNDED_CURVE ( )  B_SPLINE_CURVE ( 3, ( #17847, #18535, #44099, #64367 ),
 .UNSPECIFIED., .F., .F. ) 
 B_SPLINE_CURVE_WITH_KNOTS ( ( 4, 4 ),
 ( 5.656652915288876926, 5.682918742766132958 ),
 .UNSPECIFIED. ) 
 CURVE ( )  GEOMETRIC_REPRESENTATION_ITEM ( )  RATIONAL_B_SPLINE_CURVE ( ( 1.000000000000000000, 0.9999425096852141426, 0.9999425096852141426, 1.000000000000000000 ) ) 
 REPRESENTATION_ITEM ( '' )  );
#43480 = CARTESIAN_POINT ( 'NONE',  ( 2.931247277082681180, 1.728824746592373840, -7.672001188570248154 ) ) ;
#43481 = CARTESIAN_POINT ( 'NONE',  ( 35.00000000000000000, 5.814360711498443912, 10.70999494708485678 ) ) ;
#43482 = VERTEX_POINT ( 'NONE', #34403 ) ;
#43483 = ORIENTED_EDGE ( 'NONE', *, *, #5712, .T. ) ;
#43484 = DIRECTION ( 'NONE',  ( 0.000000000000000000, 0.9346839223284554299, -0.3554799084908935036 ) ) ;
#43485 = ORIENTED_EDGE ( 'NONE', *, *, #63129, .T. ) ;
#43486 = FACE_OUTER_BOUND ( 'NONE', #34272, .T. ) ;
#43487 = ORIENTED_EDGE ( 'NONE', *, *, #24965, .T. ) ;
#43488 = AXIS2_PLACEMENT_3D ( 'NONE', #46637, #1431, #37305 ) ;
#43489 = ORIENTED_EDGE ( 'NONE', *, *, #52920, .F. ) ;
#43490 = CARTESIAN_POINT ( 'NONE',  ( 2.000000000000001776, -4.604744433234619017, -5.919993978425545755 ) ) ;
#43491 = DIRECTION ( 'NONE',  ( 0.000000000000000000, 0.9718671068226467646, -0.2355298848897482977 ) ) ;
#43492 = EDGE_CURVE ( 'NONE', #23272, #22824, #14748, .T. ) ;
#43493 = CARTESIAN_POINT ( 'NONE',  ( 0.3006302518452048100, 10.50091819089224288, -6.323626002160976256 ) ) ;
#43494 = DIRECTION ( 'NONE',  ( 0.000000000000000000, -0.01356324068817998940, 0.9999080150203990547 ) ) ;
#43495 = CARTESIAN_POINT ( 'NONE',  ( 0.2655924914740778742, -2.169924872617981393, -12.05257978623656001 ) ) ;
#43496 = CARTESIAN_POINT ( 'NONE',  ( 2.034671305880000336, 6.953089744304945974, 9.380408876023668796 ) ) ;
#43497 = ORIENTED_EDGE ( 'NONE', *, *, #6621, .T. ) ;
#43498 = DIRECTION ( 'NONE',  ( 0.3865475372811021382, -0.1791957239473782881, 0.9046932595863030890 ) ) ;
#43499 = CARTESIAN_POINT ( 'NONE',  ( 2.000000000000001776, -2.480520636974233639, 6.345145617221206180 ) ) ;
#43500 = CARTESIAN_POINT ( 'NONE',  ( 3.152665057734040488, 0.000000000000000000, 0.000000000000000000 ) ) ;
#43501 = CARTESIAN_POINT ( 'NONE',  ( 35.00000000000000000, 4.986700593229853595, 10.63508530065516311 ) ) ;
#43502 = CARTESIAN_POINT ( 'NONE',  ( 29.68692493517211872, 6.340234850405881417, 10.20038037279705456 ) ) ;
#43503 = CARTESIAN_POINT ( 'NONE',  ( 1.375507693220225702, 0.5913006932469592192, -12.60244951981792561 ) ) ;
#43504 = CARTESIAN_POINT ( 'NONE',  ( 2.524535260912557533, -4.054303386867513126, -6.580044328001104503 ) ) ;
#43505 = CARTESIAN_POINT ( 'NONE',  ( 0.3632410797595283514, -11.62558329798848433, -3.951633449031027201 ) ) ;
#43506 = CARTESIAN_POINT ( 'NONE',  ( 35.00000000000000000, -8.352657516904727686, -8.258652103341406203 ) ) ;
#43507 = AXIS2_PLACEMENT_3D ( 'NONE', #59254, #54907, #34924 ) ;
#43508 = EDGE_CURVE ( 'NONE', #18352, #15892, #21932, .T. ) ;
#43509 = CIRCLE ( 'NONE', #48858, 18.99999999999999645 ) ;
#43510 = ORIENTED_EDGE ( 'NONE', *, *, #14472, .F. ) ;
#43511 = CARTESIAN_POINT ( 'NONE',  ( 2.931247277082680736, -7.255238984871605012, -3.034789039497262308 ) ) ;
#43512 = AXIS2_PLACEMENT_3D ( 'NONE', #36813, #41130, #48379 ) ;
#43513 = ORIENTED_EDGE ( 'NONE', *, *, #26424, .F. ) ;
#43514 = ADVANCED_FACE ( 'NONE', ( #4493 ), #26999, .F. ) ;
#43515 = DIRECTION ( 'NONE',  ( -1.000000000000000000, -0.000000000000000000, -0.000000000000000000 ) ) ;
#43516 = FACE_OUTER_BOUND ( 'NONE', #55000, .T. ) ;
#43517 = CARTESIAN_POINT ( 'NONE',  ( 11.77567996792922322, -13.29583568948794792, -2.343173910231071133 ) ) ;
#43518 = CARTESIAN_POINT ( 'NONE',  ( -10.48620311856347875, -9.720786832536937538, 9.367833439828908482 ) ) ;
#43519 = EDGE_CURVE ( 'NONE', #40103, #64752, #63334, .T. ) ;
#43520 = CARTESIAN_POINT ( 'NONE',  ( 2.241311220309555097, -6.657499176698812526, 3.736531646286240793 ) ) ;
#43521 = EDGE_LOOP ( 'NONE', ( #30498, #15465, #41077, #47828 ) ) ;
#43522 = FACE_OUTER_BOUND ( 'NONE', #30441, .T. ) ;
#43523 = DIRECTION ( 'NONE',  ( 1.000000000000000000, 0.000000000000000000, 0.000000000000000000 ) ) ;
#43524 = CARTESIAN_POINT ( 'NONE',  ( -37.00000000000000711, 12.74921544981111232, -0.1414404973752590444 ) ) ;
#43525 = CARTESIAN_POINT ( 'NONE',  ( 1.633930747250948334, 2.909970528250789723, 12.36466318969054790 ) ) ;
#43526 = AXIS2_PLACEMENT_3D ( 'NONE', #23540, #12894, #22892 ) ;
#43527 = ADVANCED_FACE ( 'NONE', ( #4822 ), #27237, .T. ) ;
#43528 = AXIS2_PLACEMENT_3D ( 'NONE', #8548, #28835, #3910 ) ;
#43529 = CYLINDRICAL_SURFACE ( 'NONE', #30775, 2.899999999999994582 ) ;
#43530 = ORIENTED_EDGE ( 'NONE', *, *, #26051, .T. ) ;
#43531 = EDGE_CURVE ( 'NONE', #42516, #51949, #9840, .T. ) ;
#43532 = CARTESIAN_POINT ( 'NONE',  ( 5.514624014163232779, 0.002529391395135005636, -0.003278974416024992272 ) ) ;
#43533 = CARTESIAN_POINT ( 'NONE',  ( 0.6473888112830246122, -8.203438694127592967, -9.263269341114870770 ) ) ;
#43534 = CARTESIAN_POINT ( 'NONE',  ( 2.247112776671468470, -3.918650674719057481, -6.554209700764013213 ) ) ;
#43535 = TOROIDAL_SURFACE ( 'NONE', #38219, 20.19615242270663558, 4.000000000000000000 ) ;
#43536 = B_SPLINE_CURVE_WITH_KNOTS ( 'NONE', 3,
 ( #19047, #58985, #13712, #33998, #54312, #12728, #63596, #8751, #14043, #34335, #15668, #61241, #4764, #14373, #45611, #44616, #9708, #20023, #24351, #15019, #10360, #20347 ),
 .UNSPECIFIED., .F., .F.,
 ( 4, 3, 3, 3, 3, 3, 3, 4 ),
 ( 5.421010862427522170E-20, 4.449119708437038737E-05, 6.626296329540639729E-05, 8.803456484963022191E-05, 0.0001098060367612849870, 0.0001315774408628578751, 0.0001760698110411264815, 0.0001829697163287849471 ),
 .UNSPECIFIED. ) ;
#43537 = ORIENTED_EDGE ( 'NONE', *, *, #20528, .T. ) ;
#43538 = ORIENTED_EDGE ( 'NONE', *, *, #14745, .T. ) ;
#43540 = EDGE_CURVE ( 'NONE', #11296, #29095, #11297, .T. ) ;
#43539 = DIRECTION ( 'NONE',  ( -1.000000000000000000, -0.000000000000000000, 0.000000000000000000 ) ) ;
#43541 = VERTEX_POINT ( 'NONE', #6441 ) ;
#43542 = DIRECTION ( 'NONE',  ( 0.000000000000000000, 0.01356324068817998940, -0.9999080150203989437 ) ) ;
#43543 = CARTESIAN_POINT ( 'NONE',  ( 2.770579946183330478, -3.639932028439770484, -6.910873157406271616 ) ) ;
#43544 = LINE ( 'NONE', #38572, #18378 ) ;
#43545 = CARTESIAN_POINT ( 'NONE',  ( 0.2801149460245141998, 9.257544930777269698, -8.024198546827383538 ) ) ;
#43546 = B_SPLINE_CURVE_WITH_KNOTS ( 'NONE', 3,
 ( #4748, #9692, #25009, #39960, #55255, #12467, #45282, #29982, #60243, #14664, #65540, #50293, #58376, #22808, #8157, #58052 ),
 .UNSPECIFIED., .F., .F.,
 ( 4, 3, 3, 3, 3, 4 ),
 ( 2.923441161686954018E-15, 0.0002126834539179695872, 0.0004253519300366267325, 0.0006380165497224176904, 0.0007442707582428259496, 0.0009453531351417306106 ),
 .UNSPECIFIED. ) ;
#43547 = EDGE_CURVE ( 'NONE', #9429, #16636, #17707, .T. ) ;
#43548 = FACE_OUTER_BOUND ( 'NONE', #5875, .T. ) ;
#43549 = EDGE_LOOP ( 'NONE', ( #32044, #58623, #36687, #54058 ) ) ;
#43550 = ORIENTED_EDGE ( 'NONE', *, *, #37164, .F. ) ;
#43551 = EDGE_LOOP ( 'NONE', ( #24689, #56085, #13025, #31762 ) ) ;
#43552 = DIRECTION ( 'NONE',  ( -1.000000000000000000, 0.000000000000000000, 0.000000000000000000 ) ) ;
#43554 = CARTESIAN_POINT ( 'NONE',  ( 1.000000000000000888, -3.073484823194374993, 6.841322316745024779 ) ) ;
#43553 = AXIS2_PLACEMENT_3D ( 'NONE', #5194, #15481, #25142 ) ;
#43555 = COLOUR_RGB ( '', 0.09019608, 0.27058824, 0.51372549) ;
#43556 = ORIENTED_EDGE ( 'NONE', *, *, #13510, .F. ) ;
#43557 = CARTESIAN_POINT ( 'NONE',  ( -25.54417658651491863, 25.00000000000000000, 11.22596262356930197 ) ) ;
#43558 = CARTESIAN_POINT ( 'NONE',  ( 2.249013661412227361, -7.540851674528683546, 1.207748565003212482 ) ) ;
#43559 = ORIENTED_EDGE ( 'NONE', *, *, #17249, .T. ) ;
#43560 = CARTESIAN_POINT ( 'NONE',  ( -22.94572469358971034, 2.792384151940683346, -4.011883207821665742 ) ) ;
#43561 = CARTESIAN_POINT ( 'NONE',  ( 2.263328370261530775, -2.746620058315247359, -7.131064289852364624 ) ) ;
#43562 = LINE ( 'NONE', #53579, #5922 ) ;
#43563 = ORIENTED_EDGE ( 'NONE', *, *, #28154, .F. ) ;
#43564 = ORIENTED_EDGE ( 'NONE', *, *, #17020, .T. ) ;
#43565 = CARTESIAN_POINT ( 'NONE',  ( -18.25006854224444908, -9.443202773001939221, 7.404452808139724063 ) ) ;
#43566 = VERTEX_POINT ( 'NONE', #25742 ) ;
#43567 = CARTESIAN_POINT ( 'NONE',  ( 9.385593601210327819, 1.699086665242807825, -13.39428285523520401 ) ) ;
#43568 = ORIENTED_EDGE ( 'NONE', *, *, #9994, .F. ) ;
#43569 = CARTESIAN_POINT ( 'NONE',  ( 0.2652384770603659070, -4.250454630553642588, 11.48486213386624755 ) ) ;
#43570 = AXIS2_PLACEMENT_3D ( 'NONE', #21757, #42007, #12394 ) ;
#43571 = DIRECTION ( 'NONE',  ( 0.000000000000000000, 0.000000000000000000, 1.000000000000000000 ) ) ;
#43572 = CARTESIAN_POINT ( 'NONE',  ( -18.83018139755647269, -28.92741097219608903, 6.858339499770058190 ) ) ;
#43573 = EDGE_CURVE ( 'NONE', #10064, #27787, #4332, .T. ) ;
#43574 = CARTESIAN_POINT ( 'NONE',  ( -22.29382655386184808, 3.622626291186084035, 0.8947172055470357099 ) ) ;
#43575 = CARTESIAN_POINT ( 'NONE',  ( 1.547277799340754711, 11.66196709685618416, -4.961646058324859609 ) ) ;
#43576 = DIRECTION ( 'NONE',  ( 0.000000000000000000, 0.000000000000000000, 1.000000000000000000 ) ) ;
#43577 = EDGE_LOOP ( 'NONE', ( #19831, #50627, #133, #3258 ) ) ;
#43578 = FACE_OUTER_BOUND ( 'NONE', #34138, .T. ) ;
#43579 = ORIENTED_EDGE ( 'NONE', *, *, #61789, .F. ) ;
#43580 = FACE_OUTER_BOUND ( 'NONE', #62, .T. ) ;
#43581 = CARTESIAN_POINT ( 'NONE',  ( 2.244591118395372398, 6.665613643994186432, 3.724266936776519987 ) ) ;
#43582 = ORIENTED_EDGE ( 'NONE', *, *, #33814, .T. ) ;
#43583 = ADVANCED_FACE ( 'NONE', ( #32349 ), #5812, .T. ) ;
#43584 = CARTESIAN_POINT ( 'NONE',  ( 35.00000000000000000, 8.029056188533806093, 8.573591947375229338 ) ) ;
#43585 = CARTESIAN_POINT ( 'NONE',  ( 0.3610902822527179978, 6.364812822043165674, 10.49957835860565503 ) ) ;
#43586 = CIRCLE ( 'NONE', #14893, 12.73084802173761787 ) ;
#43587 = CARTESIAN_POINT ( 'NONE',  ( 0.3109076770649110144, -2.361108455562764163, -12.03190317807025700 ) ) ;
#43588 = EDGE_LOOP ( 'NONE', ( #26470, #61584, #5368, #61296 ) ) ;
#43589 = EDGE_CURVE ( 'NONE', #13921, #56844, #24066, .T. ) ;
#43590 = ORIENTED_EDGE ( 'NONE', *, *, #35820, .F. ) ;
#43591 = CARTESIAN_POINT ( 'NONE',  ( 29.51976981715666781, 25.00000000000000000, 11.09513982864076276 ) ) ;
#43592 = AXIS2_PLACEMENT_3D ( 'NONE', #12908, #58826, #29192 ) ;
#43593 = ORIENTED_EDGE ( 'NONE', *, *, #33239, .T. ) ;
#43594 = CARTESIAN_POINT ( 'NONE',  ( 6.812204945636112896, -4.138731716409435712, -12.84993773446340803 ) ) ;
#43595 = CARTESIAN_POINT ( 'NONE',  ( -37.00000000000000711, 8.551552972817082932, 8.052525312709914118 ) ) ;
#43596 = CARTESIAN_POINT ( 'NONE',  ( -27.08421723179412410, 2.188590898430372356, 0.6782017488087717094 ) ) ;
#43598 = AXIS2_PLACEMENT_3D ( 'NONE', #21829, #7161, #62356 ) ;
#43597 = CARTESIAN_POINT ( 'NONE',  ( -2.961933481642279986, 6.427243547134065871, 10.16558664581745930 ) ) ;
#43599 = ADVANCED_FACE ( 'NONE', ( #61303 ), #22313, .F. ) ;
#43600 = LINE ( 'NONE', #42271, #5567 ) ;
#43601 = EDGE_LOOP ( 'NONE', ( #4578, #29812, #7904, #46527 ) ) ;
#43602 = DIRECTION ( 'NONE',  ( 0.000000000000000000, 0.9289767198167924178, -0.3701381553399118451 ) ) ;
#43603 = AXIS2_PLACEMENT_3D ( 'NONE', #57149, #26226, #46502 ) ;
#43604 = CARTESIAN_POINT ( 'NONE',  ( 13.39083528062608330, -28.49171679073736740, -12.64377518253358978 ) ) ;
#43605 = EDGE_CURVE ( 'NONE', #54859, #12885, #51683, .T. ) ;
#43606 = CARTESIAN_POINT ( 'NONE',  ( 22.57855258442564761, -4.427776684447072952, -12.75322679295976691 ) ) ;
#43607 = DIRECTION ( 'NONE',  ( 1.000000000000000000, 0.000000000000000000, 0.000000000000000000 ) ) ;
#43608 = EDGE_CURVE ( 'NONE', #9125, #46774, #3603, .T. ) ;
#43609 = DIRECTION ( 'NONE',  ( 0.000000000000000000, 0.000000000000000000, 1.000000000000000000 ) ) ;
#43610 = DIRECTION ( 'NONE',  ( -1.000000000000000000, 0.000000000000000000, 0.000000000000000000 ) ) ;
#43611 = DIRECTION ( 'NONE',  ( 1.000000000000000000, 0.000000000000000000, 0.000000000000000000 ) ) ;
#43612 = EDGE_CURVE ( 'NONE', #11073, #51152, #45598, .T. ) ;
#43613 = CIRCLE ( 'NONE', #29850, 6.936499999999988120 ) ;
#43614 = AXIS2_PLACEMENT_3D ( 'NONE', #18108, #28732, #3497 ) ;
#43615 = EDGE_LOOP ( 'NONE', ( #30637, #18144, #43559, #20419 ) ) ;
#43616 = ADVANCED_FACE ( 'NONE', ( #32658 ), #32999, .T. ) ;
#43617 = CARTESIAN_POINT ( 'NONE',  ( 2.241352910868909643, -0.08337961031709527349, 7.633946224498472155 ) ) ;
#43619 = EDGE_CURVE ( 'NONE', #43307, #48169, #19796, .T. ) ;
#43618 = AXIS2_PLACEMENT_3D ( 'NONE', #65350, #40074, #60360 ) ;
#43620 = CIRCLE ( 'NONE', #2208, 12.74999999999999822 ) ;
#43621 = VERTEX_POINT ( 'NONE', #2790 ) ;
#43622 = DIRECTION ( 'NONE',  ( 1.000000000000000000, 0.000000000000000000, -0.000000000000000000 ) ) ;
#43623 = B_SPLINE_CURVE_WITH_KNOTS ( 'NONE', 3,
 ( #5769, #21358, #46317, #11065, #47307, #41636, #50978, #1427, #21019, #11378, #56625, #56273, #16029, #6089, #26035, #30665, #16695, #31342, #61925, #16383, #10720, #26676 ),
 .UNSPECIFIED., .F., .F.,
 ( 4, 2, 2, 2, 2, 2, 2, 2, 2, 2, 4 ),
 ( 0.000000000000000000, 0.002098281408793136078, 0.003147422113189705852, 0.004196562817586277361, 0.004721133169784564633, 0.005245703521982852773, 0.005770273874181140045, 0.006294844226379429052, 0.007343984930776007933, 0.007868555282974301276, 0.008393125635172596355 ),
 .UNSPECIFIED. ) ;
#43624 = CARTESIAN_POINT ( 'NONE',  ( -22.28939870658739864, 3.707376022556855499, -0.2834927284407640635 ) ) ;
#43625 = DIRECTION ( 'NONE',  ( -1.000000000000000000, 0.000000000000000000, 0.000000000000000000 ) ) ;
#43626 = ORIENTED_EDGE ( 'NONE', *, *, #52709, .T. ) ;
#43627 = AXIS2_PLACEMENT_3D ( 'NONE', #322, #20600, #49558 ) ;
#43628 = EDGE_CURVE ( 'NONE', #57528, #26284, #3524, .T. ) ;
#43629 = DIRECTION ( 'NONE',  ( -1.000000000000000000, 0.000000000000000000, 0.000000000000000000 ) ) ;
#43630 = CARTESIAN_POINT ( 'NONE',  ( 36.00000000000000711, -12.54989509947652415, -2.250029553613715372 ) ) ;
#43631 = VERTEX_POINT ( 'NONE', #7400 ) ;
#43632 = ORIENTED_EDGE ( 'NONE', *, *, #59977, .T. ) ;
#43633 = ORIENTED_EDGE ( 'NONE', *, *, #45260, .T. ) ;
#43634 = DIRECTION ( 'NONE',  ( 1.000000000000000000, 0.000000000000000000, 0.000000000000000000 ) ) ;
#43635 = CARTESIAN_POINT ( 'NONE',  ( 2.266490820343225909, -7.130860233521867819, 2.750080098241490134 ) ) ;
#43636 = ORIENTED_EDGE ( 'NONE', *, *, #55240, .F. ) ;
#43637 = CARTESIAN_POINT ( 'NONE',  ( -22.27721701579900682, -2.409654355488384692, -2.783642043008656142 ) ) ;
#43638 = CARTESIAN_POINT ( 'NONE',  ( 2.473808721753356643, 1.776017171852686927, 13.38732973840310692 ) ) ;
#43639 = CARTESIAN_POINT ( 'NONE',  ( 0.2648978790185619880, -9.295532325666501450, 7.972372351882998309 ) ) ;
#43640 = AXIS2_PLACEMENT_3D ( 'NONE', #26651, #5744, #35947 ) ;
#43641 = CARTESIAN_POINT ( 'NONE',  ( 18.23172779988076542, 7.217079634543730471, 9.598093013830757414 ) ) ;
#43642 = ORIENTED_EDGE ( 'NONE', *, *, #48382, .F. ) ;
#43643 = DIRECTION ( 'NONE',  ( 1.000000000000000000, 0.000000000000000000, 0.000000000000000000 ) ) ;
#43644 = DIRECTION ( 'NONE',  ( 0.000000000000000000, -0.01356324068817992175, 0.9999080150203990547 ) ) ;
#43645 = CARTESIAN_POINT ( 'NONE',  ( -35.00000000000000000, 0.1414404973752139416, 12.74921544981111232 ) ) ;
#43647 = ORIENTED_EDGE ( 'NONE', *, *, #11976, .F. ) ;
#43646 = CARTESIAN_POINT ( 'NONE',  ( -27.16190680910944621, -11.80725687591872664, -2.143550592226117768 ) ) ;
#43649 = AXIS2_PLACEMENT_3D ( 'NONE', #56748, #57719, #12142 ) ;
#43648 = CARTESIAN_POINT ( 'NONE',  ( 5.514970785353741078, -0.003805873180274332770, 0.002796696073589857289 ) ) ;
#43650 = EDGE_LOOP ( 'NONE', ( #52594, #51500, #51693, #23929 ) ) ;
#43651 = CARTESIAN_POINT ( 'NONE',  ( -17.74124556848530077, 13.28873043644716034, 2.478524752089698246 ) ) ;
#43652 = ORIENTED_EDGE ( 'NONE', *, *, #64847, .T. ) ;
#43653 = CARTESIAN_POINT ( 'NONE',  ( 2.241509619876139059, 7.187074272457187440, -2.575142053947795606 ) ) ;
#43654 = CARTESIAN_POINT ( 'NONE',  ( -22.70624764888619751, 3.282666355490694077, -4.097886656202270217 ) ) ;
#43655 = CARTESIAN_POINT ( 'NONE',  ( 2.000000000000001776, 6.767909380267608022, -0.7805499053121014441 ) ) ;
#43656 = DIRECTION ( 'NONE',  ( 0.000000000000000000, 0.9467777615094583599, 0.3218879778915939016 ) ) ;
#43657 = VECTOR ( 'NONE', #34690, 1000.000000000000000 ) ;
#43658 = EDGE_CURVE ( 'NONE', #14359, #26571, #709, .T. ) ;
#43660 = AXIS2_PLACEMENT_3D ( 'NONE', #51332, #5782, #11080 ) ;
#43659 = DIRECTION ( 'NONE',  ( 0.000000000000000000, 0.000000000000000000, -1.000000000000000000 ) ) ;
#43661 = CYLINDRICAL_SURFACE ( 'NONE', #7949, 2.899999999999994582 ) ;
#43662 = CARTESIAN_POINT ( 'NONE',  ( -22.27756824490284160, -3.555646273932175472, -0.9591204781040369998 ) ) ;
#43663 = VERTEX_POINT ( 'NONE', #59278 ) ;
#43664 = DIRECTION ( 'NONE',  ( 0.000000000000000000, 0.01356324068817991828, -0.9999080150203990547 ) ) ;
#43665 = VERTEX_POINT ( 'NONE', #13700 ) ;
#43666 = ORIENTED_EDGE ( 'NONE', *, *, #29784, .F. ) ;
#43667 = EDGE_CURVE ( 'NONE', #35323, #45277, #42988, .T. ) ;
#43668 = LINE ( 'NONE', #58999, #9418 ) ;
#43669 = CARTESIAN_POINT ( 'NONE',  ( 0.3665391374699472626, 12.13918562134718826, 1.872534962004840597 ) ) ;
#43670 = CARTESIAN_POINT ( 'NONE',  ( -27.35552965826137140, 2.810569013793760007, -1.320216934008374920 ) ) ;
#43671 = CARTESIAN_POINT ( 'NONE',  ( 0.3341166715381246322, -10.49680960898231064, 6.352033667906565206 ) ) ;
#43673 = CIRCLE ( 'NONE', #30948, 6.000000000000000888 ) ;
#43672 = CARTESIAN_POINT ( 'NONE',  ( 5.514970785353741078, 0.0005190732562558549642, 0.004694330894494371832 ) ) ;
#43674 = VECTOR ( 'NONE', #10653, 1000.000000000000000 ) ;
#43675 = CARTESIAN_POINT ( 'NONE',  ( -34.00000000000000000, -15.00000000000000000, 0.000000000000000000 ) ) ;
#43676 = CARTESIAN_POINT ( 'NONE',  ( 0.7400311444011724582, -10.91558650018038001, -5.892391870929129638 ) ) ;
#43677 = CIRCLE ( 'NONE', #1208, 5.000000000000001776 ) ;
#43678 =( BOUNDED_SURFACE ( )  B_SPLINE_SURFACE ( 3, 1, ( 
 ( #8612, #65115 ),
 ( #45170, #44837 ),
 ( #34201, #23928 ),
 ( #60135, #13284 ) ),
 .UNSPECIFIED., .F., .F., .F. ) 
 B_SPLINE_SURFACE_WITH_KNOTS ( ( 4, 4 ),
 ( 2, 2 ),
 ( 0.000000000000000000, 1.000000000000000000 ),
 ( 0.000000000000000000, 1.000000000000000000 ),
 .UNSPECIFIED. ) 
 GEOMETRIC_REPRESENTATION_ITEM ( )  RATIONAL_B_SPLINE_SURFACE ( (
 ( 1.000000000000000000, 1.000000000000000000),
 ( 0.9942764183789327692, 0.8450855930916585379),
 ( 0.9942764183789327692, 0.8450855930916585379),
 ( 1.000000000000000000, 1.000000000000000000) ) ) 
 REPRESENTATION_ITEM ( '' )  SURFACE ( )  );
#43679 = ORIENTED_EDGE ( 'NONE', *, *, #24762, .T. ) ;
#43680 = B_SPLINE_CURVE_WITH_KNOTS ( 'NONE', 3,
 ( #54200, #8972, #53877, #9275, #8315, #3350, #43545, #43890, #63828, #64175, #18309, #38573, #13937, #18647, #59197, #14277, #29558, #8642, #13613, #28927, #39216, #44521 ),
 .UNSPECIFIED., .F., .F.,
 ( 4, 3, 3, 3, 3, 3, 3, 4 ),
 ( 2.501313391450904306E-18, 4.449119708436507478E-05, 6.626296329540233153E-05, 8.803456484962373025E-05, 0.0001098060367612770181, 0.0001315774408628485239, 0.0001760698110411154768, 0.0001829697163287807187 ),
 .UNSPECIFIED. ) ;
#43681 = DIRECTION ( 'NONE',  ( -1.000000000000000000, 0.000000000000000000, 0.000000000000000000 ) ) ;
#43682 = VECTOR ( 'NONE', #36703, 1000.000000000000000 ) ;
#43683 = CARTESIAN_POINT ( 'NONE',  ( 35.00000000000000000, 4.705694406421931860E-17, -3.469127814946512892E-15 ) ) ;
#43684 = LINE ( 'NONE', #34367, #12630 ) ;
#43685 = ADVANCED_FACE ( 'NONE', ( #58297 ), #27361, .T. ) ;
#43686 = ADVANCED_FACE ( 'NONE', ( #65238 ), #29644, .T. ) ;
#43687 = CARTESIAN_POINT ( 'NONE',  ( -17.87894447371652262, -11.34875452035182164, 3.899500356681847801 ) ) ;
#43688 = CARTESIAN_POINT ( 'NONE',  ( -37.00000000000000711, -6.917234959366895808, 9.493370459201672773 ) ) ;
#43689 = AXIS2_PLACEMENT_3D ( 'NONE', #7266, #27552, #12572 ) ;
#43690 =( BOUNDED_SURFACE ( )  B_SPLINE_SURFACE ( 3, 2, ( 
 ( #37771, #51540, #46517 ),
 ( #41514, #7171, #21239 ),
 ( #15592, #30883, #46211 ),
 ( #47751, #53060, #2201 ),
 ( #653, #58064, #41186 ),
 ( #48094, #63036, #12478 ),
 ( #36194, #32753, #56502 ),
 ( #64341, #58387, #24117 ),
 ( #24428, #49085, #38422 ),
 ( #38758, #48423, #39067 ),
 ( #14123, #44071, #33101 ),
 ( #59057, #7854, #49719 ),
 ( #28769, #19123, #53407 ),
 ( #3536, #59363, #13466 ),
 ( #53732, #23810, #18809 ),
 ( #23460, #59698, #33748 ),
 ( #29423, #2875, #54052 ),
 ( #23131, #3193, #8486 ),
 ( #64993, #43737, #4166 ),
 ( #18505, #13785, #34075 ),
 ( #28128, #64018, #34418 ),
 ( #13159, #54393, #43396 ),
 ( #63672, #8826, #29115 ),
 ( #54718, #18149, #8167 ),
 ( #33441, #58737, #44702 ),
 ( #28438, #48742, #49419 ),
 ( #3859, #44375, #39396 ),
 ( #64654, #9140, #38084 ),
 ( #12813, #46367, #51379 ),
 ( #56330, #4836, #10442 ),
 ( #25420, #45055, #29737 ),
 ( #40717, #35042, #50706 ),
 ( #25102, #5830, #36033 ),
 ( #5493, #15441, #45371 ),
 ( #501, #65631, #46049 ),
 ( #55355, #15108, #30409 ),
 ( #61319, #20107, #40369 ),
 ( #41036, #34721, #60673 ),
 ( #35387, #20766, #9792 ),
 ( #45699, #30722, #10779 ),
 ( #4506, #50390, #56006 ),
 ( #25759, #60335, #55020 ),
 ( #19793, #24776, #9453 ),
 ( #14763, #50046, #55694 ),
 ( #26091, #65326, #40048 ),
 ( #10131, #159, #39735 ),
 ( #5152, #20440, #14444 ),
 ( #61007, #31067, #30077 ),
 ( #35709, #51030, #60027 ),
 ( #15753, #19465, #41356 ) ),
 .UNSPECIFIED., .F., .F., .F. ) 
 B_SPLINE_SURFACE_WITH_KNOTS ( ( 4, 2, 2, 2, 2, 2, 2, 2, 2, 2, 2, 2, 2, 2, 2, 2, 2, 2, 2, 2, 2, 2, 2, 2, 4 ),
 ( 3, 3 ),
 ( 0.06047842900482980344, 0.06367705432712369995, 0.06527636698827063433, 0.06687567964941758258, 0.06847499231056453084, 0.07007430497171146522, 0.07327293029400536173, 0.07647155561629924436, 0.07807086827744619262, 0.07967018093859312700, 0.08286880626088702351, 0.08446811892203395788, 0.08606743158318090614, 0.08926605690547478877, 0.09086536956662173703, 0.09246468222776868529, 0.09566330755006256792, 0.09726262021120951617, 0.09886193287235645055, 0.1020605581946503471, 0.1052591835169442297, 0.1068584961780911780, 0.1084578088392381123, 0.1100571215003850606, 0.1116564341615320088 ),
 ( 0.000000000000000000, 1.000000000000000000 ),
 .UNSPECIFIED. ) 
 GEOMETRIC_REPRESENTATION_ITEM ( )  RATIONAL_B_SPLINE_SURFACE ( (
 ( 1.000000000000000000, 0.4999999999999997224, 1.000000000000000000),
 ( 1.000000000000000000, 0.5048840838053595403, 1.000000000000000000),
 ( 1.000000000000000000, 0.5132072642500213888, 1.000000000000000000),
 ( 1.000000000000000000, 0.5290214861663711243, 1.000000000000000000),
 ( 1.000000000000000000, 0.5348648783786191796, 1.000000000000000000),
 ( 1.000000000000000000, 0.5473516051742142174, 1.000000000000000000),
 ( 1.000000000000000000, 0.5539126387906357918, 1.000000000000000000),
 ( 1.000000000000000000, 0.5674101295481593921, 1.000000000000000000),
 ( 1.000000000000000000, 0.5743474342084209372, 1.000000000000000000),
 ( 1.000000000000000000, 0.5883951384281623787, 1.000000000000000000),
 ( 1.000000000000000000, 0.5955302209471763364, 1.000000000000000000),
 ( 1.000000000000000000, 0.6167715304226695228, 1.000000000000000000),
 ( 1.000000000000000000, 0.6305661306848210357, 1.000000000000000000),
 ( 1.000000000000000000, 0.6565125894471607326, 1.000000000000000000),
 ( 1.000000000000000000, 0.6686743926051859077, 1.000000000000000000),
 ( 1.000000000000000000, 0.6851014456086408355, 1.000000000000000000),
 ( 1.000000000000000000, 0.6902475665164403695, 1.000000000000000000),
 ( 1.000000000000000000, 0.6997062435422888305, 1.000000000000000000),
 ( 1.000000000000000000, 0.7040363771866375853, 1.000000000000000000),
 ( 1.000000000000000000, 0.7157418617804421901, 1.000000000000000000),
 ( 1.000000000000000000, 0.7218341033859928535, 1.000000000000000000),
 ( 1.000000000000000000, 0.7280280015705831165, 1.000000000000000000),
 ( 1.000000000000000000, 0.7296036051598838723, 1.000000000000000000),
 ( 1.000000000000000000, 0.7316818214130017539, 1.000000000000000000),
 ( 1.000000000000000000, 0.7321927565546040295, 1.000000000000000000),
 ( 1.000000000000000000, 0.7321641879719948953, 1.000000000000000000),
 ( 1.000000000000000000, 0.7300624469253677029, 1.000000000000000000),
 ( 1.000000000000000000, 0.7238943330023113187, 1.000000000000000000),
 ( 1.000000000000000000, 0.7213359435419863797, 1.000000000000000000),
 ( 1.000000000000000000, 0.7152343487863939142, 1.000000000000000000),
 ( 1.000000000000000000, 0.7117056589944237288, 1.000000000000000000),
 ( 1.000000000000000000, 0.6999072021060018800, 1.000000000000000000),
 ( 1.000000000000000000, 0.6903911339382012846, 1.000000000000000000),
 ( 1.000000000000000000, 0.6741089150890702264, 1.000000000000000000),
 ( 1.000000000000000000, 0.6683461163768288360, 1.000000000000000000),
 ( 1.000000000000000000, 0.6562237482357344831, 1.000000000000000000),
 ( 1.000000000000000000, 0.6498375142660873793, 1.000000000000000000),
 ( 1.000000000000000000, 0.6302143011361827085, 1.000000000000000000),
 ( 1.000000000000000000, 0.6164540672887562911, 1.000000000000000000),
 ( 1.000000000000000000, 0.5885848209491306715, 1.000000000000000000),
 ( 1.000000000000000000, 0.5744580946949985334, 1.000000000000000000),
 ( 1.000000000000000000, 0.5540565490002123950, 1.000000000000000000),
 ( 1.000000000000000000, 0.5474350731751959076, 1.000000000000000000),
 ( 1.000000000000000000, 0.5350293539659718434, 1.000000000000000000),
 ( 1.000000000000000000, 0.5292092555093077522, 1.000000000000000000),
 ( 1.000000000000000000, 0.5186171472262492976, 1.000000000000000000),
 ( 1.000000000000000000, 0.5138445523878416576, 1.000000000000000000),
 ( 1.000000000000000000, 0.5056909436241932010, 1.000000000000000000),
 ( 1.000000000000000000, 0.5023956439952826925, 1.000000000000000000),
 ( 1.000000000000000000, 0.4999999999999995004, 1.000000000000000000) ) ) 
 REPRESENTATION_ITEM ( '' )  SURFACE ( )  );
#43691 = CARTESIAN_POINT ( 'NONE',  ( -11.33725458716604706, -6.569267747456280837, 11.79584098982448914 ) ) ;
#43692 = CARTESIAN_POINT ( 'NONE',  ( -10.65488365322695508, -5.750401750040496474, 12.22026421357526260 ) ) ;
#43693 = CIRCLE ( 'NONE', #32005, 11.99999999999998579 ) ;
#43694 = AXIS2_PLACEMENT_3D ( 'NONE', #57478, #52162, #1299 ) ;
#43695 = EDGE_LOOP ( 'NONE', ( #3868, #16182, #15146, #52822 ) ) ;
#43696 = CARTESIAN_POINT ( 'NONE',  ( 0.2650492594609241137, 2.234872523101338881, -12.04046128294315920 ) ) ;
#43697 = CARTESIAN_POINT ( 'NONE',  ( 2.000000000000001776, 0.000000000000000000, 0.000000000000000000 ) ) ;
#43698 = CARTESIAN_POINT ( 'NONE',  ( -26.74023318801843985, -1.425982498898169082, -3.035730054944089318 ) ) ;
#43699 = EDGE_CURVE ( 'NONE', #13960, #18567, #41039, .T. ) ;
#43700 = ADVANCED_FACE ( 'NONE', ( #65543 ), #30322, .T. ) ;
#43701 = AXIS2_PLACEMENT_3D ( 'NONE', #51825, #26534, #46823 ) ;
#43702 = VECTOR ( 'NONE', #57850, 1000.000000000000000 ) ;
#43703 = AXIS2_PLACEMENT_3D ( 'NONE', #20403, #55973, #25724 ) ;
#43704 = EDGE_CURVE ( 'NONE', #10053, #50233, #9180, .T. ) ;
#43705 = CARTESIAN_POINT ( 'NONE',  ( -27.15511094194038222, 0.1446243978645498918, 2.499833641087588099 ) ) ;
#43706 = LINE ( 'NONE', #59666, #43657 ) ;
#43707 = ORIENTED_EDGE ( 'NONE', *, *, #51994, .F. ) ;
#43708 = CARTESIAN_POINT ( 'NONE',  ( -17.90133771828480391, 4.124690485994089606, 12.85602718881228945 ) ) ;
#43709 = CARTESIAN_POINT ( 'NONE',  ( 0.2869720083484391115, 9.251312689958767876, 8.034871682535136728 ) ) ;
#43710 = DIRECTION ( 'NONE',  ( 1.000000000000000000, 0.000000000000000000, 0.000000000000000000 ) ) ;
#43711 = ORIENTED_EDGE ( 'NONE', *, *, #58082, .F. ) ;
#43712 = EDGE_CURVE ( 'NONE', #26006, #13578, #53779, .T. ) ;
#43713 = CARTESIAN_POINT ( 'NONE',  ( 0.3654063281920730821, 2.391195511198650259, 12.04448018134536369 ) ) ;
#43714 = DIRECTION ( 'NONE',  ( 0.000000000000000000, 0.8835120444460208278, 0.4684084406997939265 ) ) ;
#43715 = EDGE_LOOP ( 'NONE', ( #61818, #48188, #34828, #25040 ) ) ;
#43716 = ORIENTED_EDGE ( 'NONE', *, *, #33340, .T. ) ;
#43717 = CARTESIAN_POINT ( 'NONE',  ( 35.00000000000000000, -3.614449339633571512, -11.17622378668005290 ) ) ;
#43718 = AXIS2_PLACEMENT_3D ( 'NONE', #60936, #16013, #31327 ) ;
#43719 = VECTOR ( 'NONE', #35530, 1000.000000000000000 ) ;
#43720 = ORIENTED_EDGE ( 'NONE', *, *, #64449, .T. ) ;
#43721 = CIRCLE ( 'NONE', #21429, 5.000000000000000888 ) ;
#43722 = CARTESIAN_POINT ( 'NONE',  ( 0.9296196016834358256, -12.19921892949987274, -2.573053270830791384 ) ) ;
#43723 = CARTESIAN_POINT ( 'NONE',  ( -21.17861794710831091, -13.00977982294134883, -3.604945070120774808 ) ) ;
#43724 = CARTESIAN_POINT ( 'NONE',  ( 0.2648978790185619880, -7.972372351882965447, -9.295532325666529871 ) ) ;
#43725 = CARTESIAN_POINT ( 'NONE',  ( 2.251152103363645907, -7.542379262759450143, -1.202724109297157451 ) ) ;
#43726 = VECTOR ( 'NONE', #40287, 1000.000000000000000 ) ;
#43727 = CARTESIAN_POINT ( 'NONE',  ( 0.000000000000000000, -5.396716205731396876, -4.158041573745144603 ) ) ;
#43729 = ORIENTED_EDGE ( 'NONE', *, *, #61088, .F. ) ;
#43728 = LINE ( 'NONE', #27133, #33982 ) ;
#43730 = CARTESIAN_POINT ( 'NONE',  ( 5.515188684475870851, -0.005339000964282158458, 0.0003622115669627282630 ) ) ;
#43731 = ORIENTED_EDGE ( 'NONE', *, *, #21541, .F. ) ;
#43732 = CARTESIAN_POINT ( 'NONE',  ( 35.00000000000000000, 4.237620530777968852, 11.42599468261424178 ) ) ;
#43733 = AXIS2_PLACEMENT_3D ( 'NONE', #2487, #3143, #23402 ) ;
#43734 = VERTEX_POINT ( 'NONE', #5061 ) ;
#43735 = ORIENTED_EDGE ( 'NONE', *, *, #13121, .T. ) ;
#43736 = CARTESIAN_POINT ( 'NONE',  ( -15.21025129788659136, 8.472317264167026352, 10.51053406556264314 ) ) ;
#43737 = CARTESIAN_POINT ( 'NONE',  ( -5.808548865027071351, -28.57390223679936980, 12.95295593664479483 ) ) ;
#43738 = B_SPLINE_CURVE_WITH_KNOTS ( 'NONE', 3,
 ( #17237, #52807, #23202, #16899, #47818, #52503, #43463, #11904, #57479, #12547, #2277, #63743, #17571, #32825, #1941, #58461 ),
 .UNSPECIFIED., .F., .F.,
 ( 4, 3, 3, 3, 3, 4 ),
 ( 1.084202172485504434E-19, 0.0003017745587525269275, 0.0006035491769808807878, 0.0009053241094668276322, 0.001207275924541018237, 0.001510325902535035285 ),
 .UNSPECIFIED. ) ;
#43739 = CYLINDRICAL_SURFACE ( 'NONE', #24773, 12.74999999999999822 ) ;
#43740 = DIRECTION ( 'NONE',  ( 0.000000000000000000, 0.01356324068817998940, -0.9999080150203990547 ) ) ;
#43741 = CYLINDRICAL_SURFACE ( 'NONE', #16534, 12.18649999999999878 ) ;
#43742 = DIRECTION ( 'NONE',  ( 0.000000000000000000, -0.01356324068817999114, 0.9999080150203989437 ) ) ;
#43743 = ORIENTED_EDGE ( 'NONE', *, *, #11104, .T. ) ;
#43744 = AXIS2_PLACEMENT_3D ( 'NONE', #45385, #40387, #9807 ) ;
#43745 = EDGE_CURVE ( 'NONE', #49132, #50940, #55258, .T. ) ;
#43746 = DIRECTION ( 'NONE',  ( 0.000000000000000000, 0.8827602140260332186, -0.4698238015817332580 ) ) ;
#43747 = DIRECTION ( 'NONE',  ( 0.000000000000000000, 0.01356324068817998940, -0.9999080150203990547 ) ) ;
#43748 = CARTESIAN_POINT ( 'NONE',  ( 1.937114397841932290, 1.334979369128424853, 12.76557247858998778 ) ) ;
#43749 = ORIENTED_EDGE ( 'NONE', *, *, #57506, .T. ) ;
#43750 = CARTESIAN_POINT ( 'NONE',  ( -35.00000000000000000, 0.7008968033238767159, 12.16632754454236931 ) ) ;
#43751 = ORIENTED_EDGE ( 'NONE', *, *, #23293, .T. ) ;
#43752 = ADVANCED_FACE ( 'NONE', ( #24680 ), #59602, .T. ) ;
#43754 = AXIS2_PLACEMENT_3D ( 'NONE', #21830, #42077, #62357 ) ;
#43753 = CARTESIAN_POINT ( 'NONE',  ( 2.242418902651939661, -7.500817491983891472, 1.423836467585327448 ) ) ;
#43755 = CARTESIAN_POINT ( 'NONE',  ( -22.76187086591099984, 1.734723475976807094E-15, -8.673617379884035472E-15 ) ) ;
#43756 = CYLINDRICAL_SURFACE ( 'NONE', #31020, 4.999999999999999112 ) ;
#43757 = CARTESIAN_POINT ( 'NONE',  ( -22.28939870658739864, 3.068935452695165544, -2.099199915896291291 ) ) ;
#43758 = CIRCLE ( 'NONE', #23603, 12.75000000000000178 ) ;
#43759 = CIRCLE ( 'NONE', #52278, 12.73084802173761787 ) ;
#43760 = CARTESIAN_POINT ( 'NONE',  ( -35.00000000000000000, 7.561043153947966999, 9.557269938331581116 ) ) ;
#43761 = DIRECTION ( 'NONE',  ( 1.000000000000000000, 0.000000000000000000, 0.000000000000000000 ) ) ;
#43762 = CIRCLE ( 'NONE', #36344, 5.000000000000001776 ) ;
#43763 = DIRECTION ( 'NONE',  ( 0.000000000000000000, -0.9796553971857762111, -0.2006870767258790988 ) ) ;
#43764 = ORIENTED_EDGE ( 'NONE', *, *, #35157, .T. ) ;
#43765 = ORIENTED_EDGE ( 'NONE', *, *, #27584, .F. ) ;
#43766 = ADVANCED_FACE ( 'NONE', ( #45285 ), #39640, .T. ) ;
#43767 = DIRECTION ( 'NONE',  ( -1.000000000000000000, 0.000000000000000000, -0.000000000000000000 ) ) ;
#43768 = EDGE_CURVE ( 'NONE', #61650, #53266, #35293, .T. ) ;
#43769 = PRESENTATION_STYLE_ASSIGNMENT (( #23490 ) ) ;
#43770 = FACE_OUTER_BOUND ( 'NONE', #15733, .T. ) ;
#43771 = VECTOR ( 'NONE', #59629, 1000.000000000000000 ) ;
#43772 = ADVANCED_FACE ( 'NONE', ( #19037 ), #14032, .T. ) ;
#43773 = AXIS2_PLACEMENT_3D ( 'NONE', #5881, #61693, #6191 ) ;
#43774 = ORIENTED_EDGE ( 'NONE', *, *, #13862, .F. ) ;
#43775 = DIRECTION ( 'NONE',  ( 0.000000000000000000, 0.01356324068817998940, -0.9999080150203989437 ) ) ;
#43776 = ORIENTED_EDGE ( 'NONE', *, *, #49517, .T. ) ;
#43777 = CARTESIAN_POINT ( 'NONE',  ( 3.152665057734129306, -7.923639299008720549, -0.4801242025592799556 ) ) ;
#43778 = DIRECTION ( 'NONE',  ( 1.000000000000000000, 0.000000000000000000, 0.000000000000000000 ) ) ;
#43779 = VECTOR ( 'NONE', #48585, 1000.000000000000227 ) ;
#43780 = CARTESIAN_POINT ( 'NONE',  ( 2.241317068080781016, 1.415707718487511757, 7.501982551779186714 ) ) ;
#43781 = DIRECTION ( 'NONE',  ( 1.000000000000000000, 0.000000000000000000, 0.000000000000000000 ) ) ;
#43782 = VERTEX_POINT ( 'NONE', #59941 ) ;
#43783 = CARTESIAN_POINT ( 'NONE',  ( 3.152665057735613008, -6.378477742801520023, -4.725420687649700469 ) ) ;
#43784 = DIRECTION ( 'NONE',  ( 0.000000000000000000, 0.9718671068226466536, -0.2355298848897482422 ) ) ;
#43785 = CARTESIAN_POINT ( 'NONE',  ( 2.000000000000001776, 6.767909380267589370, 0.7805499053121639497 ) ) ;
#43786 = CARTESIAN_POINT ( 'NONE',  ( -37.00000000000000711, -12.14284015767849390, -1.030638227056693834 ) ) ;
#43787 = EDGE_CURVE ( 'NONE', #58300, #57308, #40277, .T. ) ;
#43788 = ADVANCED_FACE ( 'NONE', ( #14668 ), #44604, .T. ) ;
#43789 = LINE ( 'NONE', #34460, #139 ) ;
#43790 = CIRCLE ( 'NONE', #37419, 12.18649999999999700 ) ;
#43791 = CARTESIAN_POINT ( 'NONE',  ( -17.54726996257253191, -12.93490414535027710, 3.865003848717349033 ) ) ;
#43792 = VERTEX_POINT ( 'NONE', #19374 ) ;
#43793 = CARTESIAN_POINT ( 'NONE',  ( 2.241317068080785013, -2.524952427345706241, 7.204761327832128082 ) ) ;
#43794 = CARTESIAN_POINT ( 'NONE',  ( -37.00000000000000711, -12.09831040184925222, 1.463443770872732141 ) ) ;
#43795 = CARTESIAN_POINT ( 'NONE',  ( 2.990024434114437302, -31.21813892570122206, -14.24440799104838717 ) ) ;
#43796 = VERTEX_POINT ( 'NONE', #9359 ) ;
#43797 = CARTESIAN_POINT ( 'NONE',  ( -10.21993208096348660, -3.717392186318608793, -12.98382749989833052 ) ) ;
#43798 = FACE_OUTER_BOUND ( 'NONE', #20553, .T. ) ;
#43799 = DIRECTION ( 'NONE',  ( 0.000000000000000000, -0.01356324068817998940, 0.9999080150203990547 ) ) ;
#43800 = VECTOR ( 'NONE', #6364, 1000.000000000000000 ) ;
#43801 = CARTESIAN_POINT ( 'NONE',  ( 0.4626703367442810966, 12.30872794628565892, 0.2831487465612879117 ) ) ;
#43802 = CARTESIAN_POINT ( 'NONE',  ( -9.658042753202595421, -11.20703797639928112, -7.536491558063052487 ) ) ;
#43803 = AXIS2_PLACEMENT_3D ( 'NONE', #64459, #59177, #59487 ) ;
#43804 = CIRCLE ( 'NONE', #9810, 6.936499999999989008 ) ;
#43805 = CARTESIAN_POINT ( 'NONE',  ( 35.00000000000000000, 4.705694406421931860E-17, -3.469127814946512892E-15 ) ) ;
#43806 = ORIENTED_EDGE ( 'NONE', *, *, #62194, .T. ) ;
#43807 = CARTESIAN_POINT ( 'NONE',  ( -35.00000000000000000, 0.000000000000000000, 0.000000000000000000 ) ) ;
#43808 = CARTESIAN_POINT ( 'NONE',  ( 5.516018279890452902, -0.0002248006052447136570, 0.006771744149385739570 ) ) ;
#43809 = CARTESIAN_POINT ( 'NONE',  ( 0.2958664285830429064, -9.529149585189895078, -7.708042451272270945 ) ) ;
#43810 = CARTESIAN_POINT ( 'NONE',  ( 2.717984159220105500, -4.788867404453539756, 6.148373979319240235 ) ) ;
#43811 = DIRECTION ( 'NONE',  ( 1.000000000000000000, -0.000000000000000000, 0.000000000000000000 ) ) ;
#43812 = CARTESIAN_POINT ( 'NONE',  ( 10.48620311856346454, 8.250315036047107142, 10.68561190601526611 ) ) ;
#43813 = CARTESIAN_POINT ( 'NONE',  ( -35.00000000000000000, -10.84030624090601869, -6.711949091238257559 ) ) ;
#43814 = CARTESIAN_POINT ( 'NONE',  ( -16.98800322446194855, 2.922502605998049674, -13.17987020110343543 ) ) ;
#43815 = ORIENTED_EDGE ( 'NONE', *, *, #54926, .T. ) ;
#43816 = VERTEX_POINT ( 'NONE', #4410 ) ;
#43817 =( NAMED_UNIT ( * ) PLANE_ANGLE_UNIT ( ) SI_UNIT ( $, .RADIAN. ) );
#43818 = ORIENTED_EDGE ( 'NONE', *, *, #48029, .F. ) ;
#43819 = B_SPLINE_CURVE_WITH_KNOTS ( 'NONE', 3,
 ( #29858, #4628, #50168, #13905, #65430, #19894, #60450, #14874, #5608, #25877, #15863, #46799, #40494, #30833, #1265, #611, #6249, #15549, #10235, #51497, #36500, #5943 ),
 .UNSPECIFIED., .F., .F.,
 ( 4, 3, 3, 3, 3, 3, 3, 4 ),
 ( 0.000000000000000000, 4.447697177976374735E-05, 6.624143997791376683E-05, 8.800576886944418142E-05, 0.0001097699864780915817, 0.0001315341395364400380, 0.0001760120188223304890, 0.0001867971373174766379 ),
 .UNSPECIFIED. ) ;
#43820 = PRESENTATION_STYLE_ASSIGNMENT (( #60410 ) ) ;
#43821 = CARTESIAN_POINT ( 'NONE',  ( -22.27710395300133683, 2.620347679538758801, -2.585700543510485616 ) ) ;
#43822 = CARTESIAN_POINT ( 'NONE',  ( 37.00000000000000711, 7.745827850123149005, 10.12742074351888100 ) ) ;
#43823 = CARTESIAN_POINT ( 'NONE',  ( 37.00000000000000711, -12.46157735505187247, 2.696588552979187536 ) ) ;
#43824 = ORIENTED_EDGE ( 'NONE', *, *, #5858, .F. ) ;
#43825 = CARTESIAN_POINT ( 'NONE',  ( 0.3474126878361826209, 5.911350916722190263, -10.75620725594709803 ) ) ;
#43826 = EDGE_CURVE ( 'NONE', #63134, #14001, #34950, .T. ) ;
#43827 = CIRCLE ( 'NONE', #53373, 2.899999999999997247 ) ;
#43828 = DIRECTION ( 'NONE',  ( -1.000000000000000000, 0.000000000000000000, 0.000000000000000000 ) ) ;
#43829 = CARTESIAN_POINT ( 'NONE',  ( 2.899286259009689282, -1.713434346771278038, 7.664525129300153061 ) ) ;
#43830 = ORIENTED_EDGE ( 'NONE', *, *, #20735, .T. ) ;
#43831 = AXIS2_PLACEMENT_3D ( 'NONE', #21920, #61816, #16270 ) ;
#43832 = ORIENTED_EDGE ( 'NONE', *, *, #38334, .T. ) ;
#43833 = DIRECTION ( 'NONE',  ( -1.000000000000000000, 0.000000000000000000, 0.000000000000000000 ) ) ;
#43834 = DIRECTION ( 'NONE',  ( -1.000000000000000000, 0.000000000000000000, 0.000000000000000000 ) ) ;
#43835 = ORIENTED_EDGE ( 'NONE', *, *, #45542, .F. ) ;
#43836 = ORIENTED_EDGE ( 'NONE', *, *, #57622, .F. ) ;
#43837 = CARTESIAN_POINT ( 'NONE',  ( 35.00000000000000000, 1.463443770872944194, 12.09831040184922024 ) ) ;
#43838 = DIRECTION ( 'NONE',  ( 0.000000000000000000, 0.3193015301359743985, 0.9476531711828043436 ) ) ;
#43839 = CARTESIAN_POINT ( 'NONE',  ( -27.08871896697732140, -2.297279805116094753, 0.1856437051692867712 ) ) ;
#43841 = EDGE_CURVE ( 'NONE', #60276, #34377, #15591, .T. ) ;
#43840 = DIRECTION ( 'NONE',  ( -1.000000000000000000, -0.000000000000000000, 0.000000000000000000 ) ) ;
#43842 = CARTESIAN_POINT ( 'NONE',  ( -35.00000000000000000, 0.000000000000000000, 0.000000000000000000 ) ) ;
#43843 = CARTESIAN_POINT ( 'NONE',  ( 3.152665057734104437, -3.546019893116280741, -7.102135024645891193 ) ) ;
#43844 = EDGE_LOOP ( 'NONE', ( #27260, #23741, #23052, #35300 ) ) ;
#43845 = CARTESIAN_POINT ( 'NONE',  ( -19.56743653832047158, -33.00000000000000000, -5.000000000000003553 ) ) ;
#43846 = CARTESIAN_POINT ( 'NONE',  ( 2.000000000000001776, 0.000000000000000000, 0.000000000000000000 ) ) ;
#43847 = CYLINDRICAL_SURFACE ( 'NONE', #280, 12.18649999999999878 ) ;
#43848 = CARTESIAN_POINT ( 'NONE',  ( -37.00000000000000711, -4.986700593229626222, -10.63508530065527147 ) ) ;
#43850 = CARTESIAN_POINT ( 'NONE',  ( 0.3610902822527225497, -8.091349661862569320, -9.234828023175179368 ) ) ;
#43849 = AXIS2_PLACEMENT_3D ( 'NONE', #9274, #34858, #49549 ) ;
#43851 = CARTESIAN_POINT ( 'NONE',  ( 0.5572780756289488213, 0.3055340344622364257, -12.33974848088654319 ) ) ;
#43852 = CARTESIAN_POINT ( 'NONE',  ( -37.00000000000000711, -9.040300684349640292, -7.499679039484155041 ) ) ;
#43853 = LINE ( 'NONE', #23584, #2673 ) ;
#43854 = AXIS2_PLACEMENT_3D ( 'NONE', #26239, #21236, #40881 ) ;
#43855 = DIRECTION ( 'NONE',  ( 0.000000000000000000, -0.01356324068817998940, 0.9999080150203990547 ) ) ;
#43856 = CIRCLE ( 'NONE', #16228, 7.499999999999988454 ) ;
#43857 = CIRCLE ( 'NONE', #45948, 7.499999999999988454 ) ;
#43858 = ORIENTED_EDGE ( 'NONE', *, *, #58339, .T. ) ;
#43859 = LINE ( 'NONE', #64142, #48213 ) ;
#43860 = ORIENTED_EDGE ( 'NONE', *, *, #36409, .T. ) ;
#43861 = CARTESIAN_POINT ( 'NONE',  ( 2.305787727787084407, 7.508843116234155346, 1.493241775258449255 ) ) ;
#43862 = DIRECTION ( 'NONE',  ( 0.000000000000000000, -0.01356324068817992175, 0.9999080150203990547 ) ) ;
#43863 = DIRECTION ( 'NONE',  ( -1.000000000000000000, 0.000000000000000000, 0.000000000000000000 ) ) ;
#43864 = CARTESIAN_POINT ( 'NONE',  ( 0.2651627682582904932, 9.437482589529976096, 7.803986935114045842 ) ) ;
#43865 = CARTESIAN_POINT ( 'NONE',  ( 2.556980015514285220, 5.149458076504937587, 5.777953785406889864 ) ) ;
#43866 = VERTEX_POINT ( 'NONE', #52 ) ;
#43867 = AXIS2_PLACEMENT_3D ( 'NONE', #44102, #59392, #29148 ) ;
#43868 = CARTESIAN_POINT ( 'NONE',  ( -27.31188777422505964, 8.574970748528185638, -8.395320217058440448 ) ) ;
#43869 = CARTESIAN_POINT ( 'NONE',  ( 2.266490820343223689, -3.694838443752345825, 6.690312181904310762 ) ) ;
#43870 = CARTESIAN_POINT ( 'NONE',  ( -35.00000000000000000, -10.42955799785324444, 6.303578524886909840 ) ) ;
#43871 = CARTESIAN_POINT ( 'NONE',  ( -22.29770266787582500, 2.703976473263656199, 2.588315884842612657 ) ) ;
#43872 = CIRCLE ( 'NONE', #6717, 7.938172270156617749 ) ;
#43873 = CARTESIAN_POINT ( 'NONE',  ( -37.00000000000000711, -0.2661492558804205988, 12.18359334611896472 ) ) ;
#43874 = ORIENTED_EDGE ( 'NONE', *, *, #22467, .F. ) ;
#43875 = VECTOR ( 'NONE', #58237, 1000.000000000000000 ) ;
#43876 = DIRECTION ( 'NONE',  ( 0.000000000000000000, -0.9868265225415276953, 0.1617819965527552140 ) ) ;
#43877 = ORIENTED_EDGE ( 'NONE', *, *, #18344, .F. ) ;
#43878 = CARTESIAN_POINT ( 'NONE',  ( 3.092491956585066148, 5.768471164323067946, -5.424230976133981308 ) ) ;
#43879 = CARTESIAN_POINT ( 'NONE',  ( 2.244591118396558116, -3.910457279126670738, -6.558116599718206707 ) ) ;
#43880 = EDGE_CURVE ( 'NONE', #34726, #2019, #61269, .T. ) ;
#43881 = EDGE_CURVE ( 'NONE', #45989, #42736, #28328, .T. ) ;
#43882 = AXIS2_PLACEMENT_3D ( 'NONE', #55923, #6057, #5065 ) ;
#43883 = ORIENTED_EDGE ( 'NONE', *, *, #34760, .F. ) ;
#43884 = ORIENTED_EDGE ( 'NONE', *, *, #60167, .T. ) ;
#43885 = CARTESIAN_POINT ( 'NONE',  ( -27.08429572838383947, 2.217805374070540125, -0.5764601019425888984 ) ) ;
#43886 = CARTESIAN_POINT ( 'NONE',  ( -36.00000000000000711, 7.238157050195776598, -10.49626516989263614 ) ) ;
#43888 = CARTESIAN_POINT ( 'NONE',  ( 2.241536586108913820, -5.852386772940035620, -4.902521014023387913 ) ) ;
#43887 =( BOUNDED_CURVE ( )  B_SPLINE_CURVE ( 3, ( #6319, #36222, #57520, #679 ),
 .UNSPECIFIED., .F., .F. ) 
 B_SPLINE_CURVE_WITH_KNOTS ( ( 4, 4 ),
 ( 4.985513291461030505, 4.993910677237380469 ),
 .UNSPECIFIED. ) 
 CURVE ( )  GEOMETRIC_REPRESENTATION_ITEM ( )  RATIONAL_B_SPLINE_CURVE ( ( 1.000000000000000000, 0.9999941236679763534, 0.9999941236679763534, 1.000000000000000000 ) ) 
 REPRESENTATION_ITEM ( '' )  );
#43889 = CARTESIAN_POINT ( 'NONE',  ( 0.3160775863651093531, 12.26075464248084046, 0.2401734240703286283 ) ) ;
#43890 = CARTESIAN_POINT ( 'NONE',  ( 0.2834382757448009049, 9.254160138069064345, -8.029794915379463660 ) ) ;
#43891 = CARTESIAN_POINT ( 'NONE',  ( -22.30625920655495165, -2.110841417170890466, -3.150098859949351571 ) ) ;
#43892 = ORIENTED_EDGE ( 'NONE', *, *, #57490, .T. ) ;
#43893 = AXIS2_PLACEMENT_3D ( 'NONE', #22775, #38035, #48385 ) ;
#43894 = CIRCLE ( 'NONE', #51376, 5.000000000000000888 ) ;
#43895 = ORIENTED_EDGE ( 'NONE', *, *, #38046, .F. ) ;
#43896 = ORIENTED_EDGE ( 'NONE', *, *, #61940, .F. ) ;
#43897 = CARTESIAN_POINT ( 'NONE',  ( 0.000000000000000000, -3.805198749487460841, 5.799611601383201531 ) ) ;
#43898 = AXIS2_PLACEMENT_3D ( 'NONE', #14090, #34380, #15070 ) ;
#43900 = AXIS2_PLACEMENT_3D ( 'NONE', #38226, #28272, #34231 ) ;
#43899 = CARTESIAN_POINT ( 'NONE',  ( 32.00000000000000000, -14.99999999999997513, 0.000000000000000000 ) ) ;
#43901 = ADVANCED_FACE ( 'NONE', ( #6054 ), #41925, .T. ) ;
#43902 = ORIENTED_EDGE ( 'NONE', *, *, #12422, .F. ) ;
#43903 = DIRECTION ( 'NONE',  ( 0.000000000000000000, 0.6269146997507929475, 0.7790879021242551605 ) ) ;
#43904 = LINE ( 'NONE', #43230, #16201 ) ;
#43905 = ORIENTED_EDGE ( 'NONE', *, *, #22672, .T. ) ;
#43906 = CARTESIAN_POINT ( 'NONE',  ( 2.573738926104374158, 7.194322927777959897, 2.868819712476736949 ) ) ;
#43907 = EDGE_CURVE ( 'NONE', #37124, #13910, #16662, .T. ) ;
#43908 = CARTESIAN_POINT ( 'NONE',  ( 37.00000000000000711, -5.927257550915237871, 10.64792938439761549 ) ) ;
#43909 = CARTESIAN_POINT ( 'NONE',  ( -22.23402523511428086, 1.734723475976807094E-15, -8.673617379884035472E-15 ) ) ;
#43910 = EDGE_LOOP ( 'NONE', ( #27150, #9641, #38014, #37076, #11086, #35957, #28590 ) ) ;
#43911 = CIRCLE ( 'NONE', #15228, 5.000000000000000888 ) ;
#43912 = ORIENTED_EDGE ( 'NONE', *, *, #15732, .T. ) ;
#43913 = CARTESIAN_POINT ( 'NONE',  ( -18.10791796330941494, -9.538085361946240681, 7.283445145555468514 ) ) ;
#43914 = EDGE_CURVE ( 'NONE', #37661, #15944, #17285, .T. ) ;
#43915 = ORIENTED_EDGE ( 'NONE', *, *, #60376, .F. ) ;
#43916 = CARTESIAN_POINT ( 'NONE',  ( 0.000000000000000000, 0.000000000000000000, 0.000000000000000000 ) ) ;
#43917 = VERTEX_POINT ( 'NONE', #36933 ) ;
#43918 = VECTOR ( 'NONE', #39524, 1000.000000000000000 ) ;
#43919 = VERTEX_POINT ( 'NONE', #46592 ) ;
#43920 = CARTESIAN_POINT ( 'NONE',  ( 0.000000000000000000, -6.539067737394485214, -2.314222412769890713 ) ) ;
#43921 = DIRECTION ( 'NONE',  ( 1.000000000000000000, -0.000000000000000000, 0.000000000000000000 ) ) ;
#43922 = CIRCLE ( 'NONE', #23762, 12.75000000000000178 ) ;
#43923 = CARTESIAN_POINT ( 'NONE',  ( -14.82142464308680907, -33.91165328791170452, -8.853132628082329703 ) ) ;
#43924 = CARTESIAN_POINT ( 'NONE',  ( -35.00000000000000000, 3.511814412392118445, 11.66953048682401040 ) ) ;
#43926 = ADVANCED_FACE ( 'NONE', ( #10350 ), #35934, .T. ) ;
#43925 = LINE ( 'NONE', #64511, #45727 ) ;
#43927 = CARTESIAN_POINT ( 'NONE',  ( 1.719304012338517706, -0.7661785589593724799, 12.70777170744426243 ) ) ;
#43928 = ORIENTED_EDGE ( 'NONE', *, *, #15424, .F. ) ;
#43929 = CARTESIAN_POINT ( 'NONE',  ( -47.00000000000000711, 0.000000000000000000, 0.000000000000000000 ) ) ;
#43930 = CIRCLE ( 'NONE', #7805, 12.18649999999999878 ) ;
#43931 = ORIENTED_EDGE ( 'NONE', *, *, #51147, .F. ) ;
#43932 = CARTESIAN_POINT ( 'NONE',  ( 2.000000000000001776, -2.469490258309472441, 6.482025155313308140 ) ) ;
#43933 = ADVANCED_FACE ( 'NONE', ( #51279 ), #45952, .T. ) ;
#43934 = VECTOR ( 'NONE', #22246, 1000.000000000000000 ) ;
#43935 = FACE_OUTER_BOUND ( 'NONE', #33353, .T. ) ;
#43936 = ORIENTED_EDGE ( 'NONE', *, *, #11188, .T. ) ;
#43937 = CARTESIAN_POINT ( 'NONE',  ( 0.3675815128205912052, -10.76447900494944321, 5.910255304480407368 ) ) ;
#43938 = CARTESIAN_POINT ( 'NONE',  ( 0.3278977287071228042, 3.961557589215610520, 11.60975784853193460 ) ) ;
#43939 = CARTESIAN_POINT ( 'NONE',  ( -27.19357181888462094, 25.00000000000000000, 5.138615876886901468 ) ) ;
#43940 = VERTEX_POINT ( 'NONE', #56235 ) ;
#43941 = ORIENTED_EDGE ( 'NONE', *, *, #5961, .F. ) ;
#43942 = CARTESIAN_POINT ( 'NONE',  ( 3.092491956585922797, -7.070043156103695381, -3.565393530441119285 ) ) ;
#43943 = EDGE_CURVE ( 'NONE', #9689, #6901, #50938, .T. ) ;
#43944 = VERTEX_POINT ( 'NONE', #15989 ) ;
#43945 = CARTESIAN_POINT ( 'NONE',  ( 2.000000000000001776, -4.376687952327290354, -5.220963330856675633 ) ) ;
#43946 = FACE_OUTER_BOUND ( 'NONE', #65348, .T. ) ;
#43947 = FACE_OUTER_BOUND ( 'NONE', #28609, .T. ) ;
#43948 = CARTESIAN_POINT ( 'NONE',  ( 0.3160775863651091311, -9.237902461149193556, -8.065044686487407688 ) ) ;
#43949 = CARTESIAN_POINT ( 'NONE',  ( 13.04069548818232249, 11.52624043203086046, -3.362534750561068098 ) ) ;
#43950 = ORIENTED_EDGE ( 'NONE', *, *, #14678, .T. ) ;
#43951 = AXIS2_PLACEMENT_3D ( 'NONE', #49778, #39795, #48809 ) ;
#43952 = VECTOR ( 'NONE', #25222, 999.9999999999998863 ) ;
#43953 = B_SPLINE_CURVE_WITH_KNOTS ( 'NONE', 3,
 ( #5698, #15633, #21637, #61853, #55891, #31585, #25625 ),
 .UNSPECIFIED., .F., .F.,
 ( 4, 3, 4 ),
 ( 7.377595983537455577E-15, 0.002398160485434805075, 0.005002426799384204585 ),
 .UNSPECIFIED. ) ;
#43954 = CARTESIAN_POINT ( 'NONE',  ( 3.152665057736261822, -7.102135024647099115, -3.546019893114602972 ) ) ;
#43955 = AXIS2_PLACEMENT_3D ( 'NONE', #59744, #34464, #54766 ) ;
#43956 = CARTESIAN_POINT ( 'NONE',  ( 16.79789036561810889, -29.41979974037718293, -9.796743230926868051 ) ) ;
#43957 = AXIS2_PLACEMENT_3D ( 'NONE', #23164, #52126, #38791 ) ;
#43958 = DIRECTION ( 'NONE',  ( -1.000000000000000000, 0.000000000000000000, 0.000000000000000000 ) ) ;
#43959 = PRODUCT_DEFINITION_SHAPE ( 'NONE', 'NONE',  #65283 ) ;
#43960 = CARTESIAN_POINT ( 'NONE',  ( 5.520433897694421610, 0.007971295965052600102, 0.01278034823632019125 ) ) ;
#43961 = DIRECTION ( 'NONE',  ( -1.000000000000000000, 0.000000000000000000, 0.000000000000000000 ) ) ;
#43962 = LINE ( 'NONE', #24660, #31125 ) ;
#43963 = AXIS2_PLACEMENT_3D ( 'NONE', #57161, #43151, #8246 ) ;
#43964 = EDGE_CURVE ( 'NONE', #62360, #19513, #44266, .T. ) ;
#43965 = ORIENTED_EDGE ( 'NONE', *, *, #9284, .T. ) ;
#43966 = CARTESIAN_POINT ( 'NONE',  ( -35.00000000000000000, 10.91536515067641844, 4.339012074900148619 ) ) ;
#43967 = ORIENTED_EDGE ( 'NONE', *, *, #25720, .T. ) ;
#43968 = CARTESIAN_POINT ( 'NONE',  ( 0.2872850955227764236, 1.921748909352319012, -12.10187515377841017 ) ) ;
#43969 = FACE_OUTER_BOUND ( 'NONE', #34416, .T. ) ;
#43970 = DIRECTION ( 'NONE',  ( -1.000000000000000000, 0.000000000000000000, -0.000000000000000000 ) ) ;
#43971 = VECTOR ( 'NONE', #265, 1000.000000000000000 ) ;
#43972 = PLANE ( 'NONE',  #39261 ) ;
#43973 = VERTEX_POINT ( 'NONE', #21671 ) ;
#43974 = VERTEX_POINT ( 'NONE', #405 ) ;
#43975 = ORIENTED_EDGE ( 'NONE', *, *, #1681, .T. ) ;
#43976 = CARTESIAN_POINT ( 'NONE',  ( 0.3002738374340846450, -7.705051734330212732, -9.533456882268719568 ) ) ;
#43977 = CARTESIAN_POINT ( 'NONE',  ( 2.244591118396558116, -7.137527852925273031, 2.712243649838676163 ) ) ;
#43978 = AXIS2_PLACEMENT_3D ( 'NONE', #51314, #52619, #16022 ) ;
#43979 = EDGE_CURVE ( 'NONE', #44540, #62927, #1390, .T. ) ;
#43980 = ORIENTED_EDGE ( 'NONE', *, *, #57993, .T. ) ;
#43981 = CARTESIAN_POINT ( 'NONE',  ( -22.27715239060371744, -2.513478159995845562, -2.689999469426704426 ) ) ;
#43982 = DIRECTION ( 'NONE',  ( 0.000000000000000000, 0.000000000000000000, 1.000000000000000000 ) ) ;
#43983 = CARTESIAN_POINT ( 'NONE',  ( 35.00000000000000000, 4.705694406421931860E-17, -3.469127814946512892E-15 ) ) ;
#43984 = CARTESIAN_POINT ( 'NONE',  ( 5.514970785353741078, 0.002796696073589740195, -0.003805873180274790303 ) ) ;
#43985 = VERTEX_POINT ( 'NONE', #42230 ) ;
#43986 = DIRECTION ( 'NONE',  ( 0.000000000000000000, 0.5767582926624912343, 0.8169148498130317515 ) ) ;
#43987 = EDGE_CURVE ( 'NONE', #16407, #34070, #32056, .T. ) ;
#43988 = FACE_OUTER_BOUND ( 'NONE', #891, .T. ) ;
#43989 = CARTESIAN_POINT ( 'NONE',  ( 2.256373768223416842, -1.457292142211169539, -7.499124080223150912 ) ) ;
#43991 = ORIENTED_EDGE ( 'NONE', *, *, #7260, .T. ) ;
#43990 = DIRECTION ( 'NONE',  ( 0.000000000000000000, 0.01356324068817998940, -0.9999080150203990547 ) ) ;
#43992 = CARTESIAN_POINT ( 'NONE',  ( 0.000000000000000000, 0.000000000000000000, 0.000000000000000000 ) ) ;
#43993 = EDGE_CURVE ( 'NONE', #51364, #38363, #39247, .T. ) ;
#43994 = ORIENTED_EDGE ( 'NONE', *, *, #9099, .F. ) ;
#43995 = AXIS2_PLACEMENT_3D ( 'NONE', #11731, #1123, #62279 ) ;
#43996 = DIRECTION ( 'NONE',  ( 0.000000000000000000, -0.7790879021242573810, 0.6269146997507903940 ) ) ;
#43997 = CIRCLE ( 'NONE', #5804, 12.75000000000000178 ) ;
#43998 = VERTEX_POINT ( 'NONE', #6367 ) ;
#43999 = CARTESIAN_POINT ( 'NONE',  ( -35.00000000000000000, 2.216820770815248309, -11.53507381115581332 ) ) ;
#44000 = CYLINDRICAL_SURFACE ( 'NONE', #47869, 12.75000000000000178 ) ;
#44001 = CARTESIAN_POINT ( 'NONE',  ( 1.719304012341317467, -0.7661785589597189805, -12.70777170743969009 ) ) ;
#44002 = CARTESIAN_POINT ( 'NONE',  ( 2.080613030138688480, 0.000000000000000000, 0.000000000000000000 ) ) ;
#44003 = DIRECTION ( 'NONE',  ( 0.8317381556525372810, -0.5551681190699946367, 0.000000000000000000 ) ) ;
#44004 = EDGE_CURVE ( 'NONE', #49616, #17690, #26635, .T. ) ;
#44005 = CARTESIAN_POINT ( 'NONE',  ( -8.724429002833421265, -2.835377106281230297, -13.19961944769576334 ) ) ;
#44006 = DIRECTION ( 'NONE',  ( -1.000000000000000000, 0.000000000000000000, 0.000000000000000000 ) ) ;
#44007 = CLOSED_SHELL ( 'NONE', ( #47697, #42285, #62309, #30725, #64308, #40075, #26296, #58424, #7490, #9019, #14648, #59228, #9561, #22092, #31397, #5441, #63395, #4200, #46036, #20189, #6908, #23113, #37801, #53552, #13557, #44337, #8203, #35335, #58687, #43616, #53620, #32912, #49026, #53778, #22322, #4737, #21298, #42538, #9826, #44408, #7140, #10634, #19009, #24789, #40914, #56130, #15622, #38121, #62446, #31182, #32725, #54590, #12318, #15231, #11830, #63835, #20176, #44818, #12148, #60503, #2943, #33970, #42410, #57756, #53094, #24476, #49433, #3780, #19125, #17078, #36433, #55250, #27790, #25516, #48113, #64310, #20117, #40936, #26290, #6649, #59014, #58917, #37297, #26298, #65071, #948, #15943, #1189, #35669, #6998, #51892, #39736, #57200, #50445, #547, #51908, #25151, #26971, #27028, #16159, #4734, #48900, #37524, #13490, #18131, #34955, #57351, #20241, #4768, #34602, #51831, #30059, #1293, #9582, #60197, #7737, #32569, #49443, #40783, #36732, #44214, #20208, #35768, #8882, #51755, #55568, #53885, #55122, #31231, #5016, #65003, #43324, #65663, #2572, #13720, #52639, #59841, #10206, #59587, #7962, #27517, #46958, #37518, #65509, #65132, #32090, #21868, #10923, #29331, #26120, #18466, #4106, #7724, #49839, #60079, #55451, #49851, #10661, #27335, #14159, #9494, #17221, #55588, #57446, #18961, #25688, #11321, #20016, #21149, #55800, #50327, #28166, #32254, #55014, #39943, #18798, #53692, #1584, #39275, #4353, #20924, #23101, #10969, #41043, #46183, #19841, #5359, #4225, #21008, #29406, #7142, #17666, #6250, #21310, #43160, #12713, #55704, #29809, #51826, #47005, #31132, #21546, #11045, #50790, #1031, #6563, #3829, #3670, #14180, #8366, #35514, #40348, #29354, #50818, #64954, #1908, #18562, #37055, #15060, #35436, #25083, #9891, #27976, #35215, #43752, #10193, #22910, #39338, #12759, #43700, #21395, #39788, #61376, #57822, #18040, #11693, #4566, #61079, #52303, #10024, #1834, #51555, #57925, #22138, #23626, #18711, #61266, #62277, #57457, #40273, #32675, #64474, #38575, #29539, #54613, #2951, #6870, #1765, #12633, #61903, #20876, #6853, #3818, #61010, #29141, #605, #52086, #65217, #3087, #50629, #40671, #47968, #53406, #259, #33463, #51213, #50139, #6818, #43257, #21119, #17024, #24554, #1376, #24313, #44350, #16967, #2291, #2576, #53210, #18605, #64897, #1889, #48880, #55371, #38836, #49374, #45199, #15334, #20364, #24196, #18445, #13131, #11551, #47576, #34381, #33476, #54687, #35272, #26480, #47490, #41056, #4436, #1677, #50482, #19741, #13622, #50805, #8412, #676, #36977, #837, #21575, #23669, #7807, #17214, #15063, #58065, #38887, #49791, #30369, #39041, #35551, #10629, #26669, #43252, #3345, #51531, #34840, #12216, #17183, #51634, #61321, #15900, #15255, #26550, #52694, #35579, #51748, #1660, #24142, #56546, #53019, #43686, #44682, #61479, #11338, #52035, #7810, #45634, #24472, #19680, #34515, #26739, #26621, #7918, #44026, #1321, #50084, #34003, #4996, #32157, #7554, #18631, #636, #5605, #47824, #16815, #517, #37738, #44051, #29122, #5038, #20067, #65754, #59641, #42767, #50401, #31871, #52592, #19952, #44888, #48055, #65562, #17213, #44126, #24658, #40987, #26410, #21987, #27546, #52728, #29139, #28923, #25784, #57547, #32630, #57853, #49124, #42099, #7335, #31889, #8709, #33323, #55062, #43397, #54015, #46107, #30987, #120, #17355, #48163, #44555, #37086, #38659, #62806, #53453, #1344, #36064, #41573, #3950, #11909, #52067, #44730, #24448, #12688, #47255, #13287, #47584, #41737, #39777, #44238, #5985, #34885, #39585, #31104, #45949, #40309, #14380, #36801, #711, #42160, #60187, #19061, #33555, #59180, #31426, #15889, #3704, #19625, #35861, #12847, #18408, #8128, #4488, #12594, #13596, #52401, #27010, #62570, #41321, #51391, #6173, #15472, #42363, #48336, #6352, #30680, #52560, #64785, #33012, #44090, #34922, #22881, #35771, #32841, #41103, #32295, #6410, #12107, #30391, #48081, #2749, #25460, #23902, #37321, #25638, #35845, #18771, #15541, #26141, #12983, #35120, #8846, #31304, #31046, #38185, #60704, #10547, #22460, #10124, #26134, #55091, #51838, #28715, #1693, #73, #32781, #12313, #6369, #18781, #982, #40050, #51911, #34646, #59198, #27245, #63923, #63162, #27046, #40352, #26191, #48310, #58098, #55214, #13295, #56458, #33405, #48644, #65499, #36492, #62361, #46874, #1391, #4862, #55064, #32700, #27752, #25609, #27717, #26650, #30616, #56230, #64489, #3098, #3212, #12229, #38556, #46629, #46219, #18727, #30619, #36425, #12766, #15754, #34376, #60680, #33807, #26677, #56971, #19435, #12921, #40923, #64730, #11941, #4189, #28580, #15409, #25859, #19932, #8207, #16858, #64528, #54348, #8627, #62759, #47767, #64924, #18257, #56729, #19520, #26499, #41088, #39383, #39020, #62347, #37565, #21939, #4966, #40059, #58955, #19963, #8306, #21068, #10287, #2313, #43933, #15953, #15521, #10581, #54599, #46567, #62938, #3008, #643, #23788, #55717, #64003, #56914, #46565, #48432, #44140, #58718, #45278, #63073, #63063, #20188, #24397, #63697, #27938, #29908, #43901, #18350, #49605, #41301, #65125, #9255, #11085, #13956, #65305, #50878, #20064, #32496, #14485, #62723, #40417, #10134, #56627, #14621, #27061, #61306, #22190, #41678, #42020, #43926, #28648, #57141, #55317, #59939, #567, #17836, #62969, #42360, #18860, #2744, #11486, #52323, #37477, #47091, #61459, #17969, #4819, #45793, #31448, #185, #56392, #38789, #38453, #7047, #5794, #50470, #30303, #50518, #30092, #4987, #65256, #16288, #458, #20433, #54940, #13969, #41853, #61038, #10638, #30921, #61115, #3407, #17206, #63972, #32341, #41108, #50592, #27482, #6931, #21697, #54394, #25854, #2971, #45612, #9344, #37724, #17731, #15294, #51319, #6683, #53684, #5719, #41700, #4508, #14309, #46266, #31315, #20724, #55418, #15047, #48591, #59365, #39304, #47073, #20719, #65444, #25739, #61944, #58815, #5134, #56636, #39201, #3172, #29316, #10718, #56835, #49044, #11218, #7710, #47369, #25782, #23009, #40414, #50928, #2107, #43788, #56190, #7428, #8107, #39174, #7914, #43303, #51353, #3380, #60010, #30023, #15858, #24121, #20065, #14665, #7843, #20134, #61862, #48940, #9961, #12396, #9612, #13499, #19033, #48362, #58249, #25541, #18946, #16936, #34703, #50169, #64198, #33117, #38032, #11117, #22370, #54511, #40069, #61387, #50976, #62414, #62071, #65533, #7435, #31521, #19821, #25863, #5333, #48999, #38723, #62497, #58951, #2877, #24243, #22985, #63297, #24123, #47686, #32420, #25918, #19332, #42600, #4531, #27748, #5801, #35797, #30088, #31283, #39228, #36637, #39110, #44585, #12132, #23495, #9337, #14726, #61904, #60797, #15453, #48137, #45404, #3415, #41644, #60830, #7406, #38290, #9419, #6496, #27803, #26843, #10556, #61405, #11836, #38951, #30478, #55903, #21135, #4291, #454, #1009, #63239, #39468, #21157, #33176, #25496, #47174, #53227, #9445, #63892, #54986, #19898, #45340, #21263, #18038, #55810, #24461, #2491, #16826, #42793, #16514, #25813, #9165, #41350, #43766, #59621, #23162, #60020, #57115, #16025, #17800, #8471, #2159, #44267, #21792, #14757, #15135, #60223, #4936, #28912, #55791, #19301, #22304, #19595, #28176, #63869, #10443, #62391, #31064, #60753, #1196, #55482, #30911, #41163, #3682, #42748, #29832, #25427, #22240, #21268, #13263, #37415, #29469, #49201, #13145, #12610, #12664, #22928, #27102, #22276, #47695, #6746, #25362, #6090, #57695, #14886, #27694, #49674, #6104, #52106, #49615, #43373, #63050, #26600, #22935, #14781, #19743, #34146, #20691, #4118, #33591, #40428, #18007, #3177, #14345, #5503, #3102, #56202, #3940, #60884, #38735, #13424, #25705, #63578, #8440, #14978, #40558, #8188, #46048, #23059, #4663, #13940, #38265, #54149, #23177, #11808, #49996, #63229, #34316, #51079, #39028, #8460, #41522, #37382, #11974, #23605, #30791, #21721, #52180, #48234, #43376, #23015, #46679, #42191, #31244, #52205, #54107, #61592, #43772, #32897, #60365, #56191, #9882, #15720, #44012, #26587, #45263, #32098, #41421, #55493, #51900, #24127, #32120, #4584, #19142, #14712, #57544, #45779, #40288, #21644, #23060, #5778, #43685, #843, #11608, #18179, #64320 ) ) ;
#44008 = VERTEX_POINT ( 'NONE', #22291 ) ;
#44009 = CARTESIAN_POINT ( 'NONE',  ( -35.00000000000000000, -11.86701198550358427, 2.772148766916072926 ) ) ;
#44010 = ORIENTED_EDGE ( 'NONE', *, *, #21862, .T. ) ;
#44011 = EDGE_CURVE ( 'NONE', #49256, #9187, #52778, .T. ) ;
#44012 = ADVANCED_FACE ( 'NONE', ( #33600 ), #27960, .T. ) ;
#44013 = ORIENTED_EDGE ( 'NONE', *, *, #4807, .T. ) ;
#44014 = CARTESIAN_POINT ( 'NONE',  ( 0.8320506296491561038, 1.781423711749740235, -12.30686996250299359 ) ) ;
#44015 = CARTESIAN_POINT ( 'NONE',  ( -27.08429572838383947, 0.2296550094123047669, 2.279961732801582208 ) ) ;
#44016 = CYLINDRICAL_SURFACE ( 'NONE', #64157, 5.000000000000000000 ) ;
#44017 = CARTESIAN_POINT ( 'NONE',  ( -22.28776923226071460, 2.100802264239995942, 3.061913732988043702 ) ) ;
#44018 = ADVANCED_FACE ( 'NONE', ( #53573 ), #62862, .T. ) ;
#44019 = CARTESIAN_POINT ( 'NONE',  ( 5.514624014163232779, 0.003278974416024983164, 0.002529391395135016912 ) ) ;
#44020 = AXIS2_PLACEMENT_3D ( 'NONE', #52077, #38073, #11499 ) ;
#44021 = DIRECTION ( 'NONE',  ( -1.000000000000000000, -0.000000000000000000, -0.000000000000000000 ) ) ;
#44022 = DIRECTION ( 'NONE',  ( 0.000000000000000000, 0.01356324068817998940, -0.9999080150203990547 ) ) ;
#44023 = EDGE_CURVE ( 'NONE', #50432, #9279, #33645, .T. ) ;
#44024 = EDGE_LOOP ( 'NONE', ( #55330, #20199, #16313, #13078 ) ) ;
#44025 = DIRECTION ( 'NONE',  ( -0.3939253465568944290, 0.9190910618577644575, -0.009718094113436451242 ) ) ;
#44026 = ADVANCED_FACE ( 'NONE', ( #3028 ), #22648, .T. ) ;
#44027 = CARTESIAN_POINT ( 'NONE',  ( 2.242819959140646358, -5.782321801516506099, -4.985618132689735305 ) ) ;
#44028 = DIRECTION ( 'NONE',  ( 1.000000000000000000, -0.000000000000000000, 0.000000000000000000 ) ) ;
#44029 = CARTESIAN_POINT ( 'NONE',  ( -37.00000000000000711, -5.710938531231627202, -11.39945968423477751 ) ) ;
#44030 = VECTOR ( 'NONE', #56103, 1000.000000000000000 ) ;
#44031 = CARTESIAN_POINT ( 'NONE',  ( 2.241526690369556096, -2.627393882429269301, -7.168108047190864696 ) ) ;
#44032 = DIRECTION ( 'NONE',  ( -1.000000000000000000, 0.000000000000000000, -0.000000000000000000 ) ) ;
#44033 = ORIENTED_EDGE ( 'NONE', *, *, #63593, .F. ) ;
#44034 = DIRECTION ( 'NONE',  ( -1.000000000000000000, 0.000000000000000000, 0.000000000000000000 ) ) ;
#44035 = AXIS2_PLACEMENT_3D ( 'NONE', #36013, #61622, #45037 ) ;
#44036 = FACE_OUTER_BOUND ( 'NONE', #53910, .T. ) ;
#44037 = CARTESIAN_POINT ( 'NONE',  ( 37.00000000000000711, 7.717887834988244045, -8.854740511458876639 ) ) ;
#44038 = EDGE_CURVE ( 'NONE', #40020, #35019, #50655, .T. ) ;
#44039 = CARTESIAN_POINT ( 'NONE',  ( -25.16431053358520131, 6.644570256749198656, 9.998964924726404746 ) ) ;
#44040 = DIRECTION ( 'NONE',  ( 0.000000000000000000, -0.01356324068817998940, 0.9999080150203990547 ) ) ;
#44041 = AXIS2_PLACEMENT_3D ( 'NONE', #34445, #54748, #44738 ) ;
#44042 = VERTEX_POINT ( 'NONE', #17978 ) ;
#44043 = CARTESIAN_POINT ( 'NONE',  ( 0.3665391374699467075, -1.872534962004718473, -12.13918562134720602 ) ) ;
#44044 = FACE_OUTER_BOUND ( 'NONE', #8703, .T. ) ;
#44045 = CARTESIAN_POINT ( 'NONE',  ( -2.532614230583026593, 25.00000000000000000, 10.89930238848911337 ) ) ;
#44046 = ORIENTED_EDGE ( 'NONE', *, *, #23404, .T. ) ;
#44047 = CARTESIAN_POINT ( 'NONE',  ( 22.58560133430949080, 11.74609238061706940, -6.663691428441929077 ) ) ;
#44048 = FACE_OUTER_BOUND ( 'NONE', #9285, .T. ) ;
#44049 = ORIENTED_EDGE ( 'NONE', *, *, #24910, .F. ) ;
#44050 = AXIS2_PLACEMENT_3D ( 'NONE', #62540, #7033, #21996 ) ;
#44051 = ADVANCED_FACE ( 'NONE', ( #37605 ), #7016, .T. ) ;
#44052 = VERTEX_POINT ( 'NONE', #27287 ) ;
#44053 = CARTESIAN_POINT ( 'NONE',  ( -35.05175862995318425, 0.01030783735684465130, -0.007207337213517919783 ) ) ;
#44054 = AXIS2_PLACEMENT_3D ( 'NONE', #20986, #55263, #41267 ) ;
#44055 = EDGE_CURVE ( 'NONE', #31243, #50772, #16646, .T. ) ;
#44056 = ORIENTED_EDGE ( 'NONE', *, *, #2506, .F. ) ;
#44057 = DIRECTION ( 'NONE',  ( -1.000000000000000000, 0.000000000000000000, 0.000000000000000000 ) ) ;
#44058 = CARTESIAN_POINT ( 'NONE',  ( 35.00000000000000000, 1.903127969211351189, 11.59095880812005497 ) ) ;
#44059 = CARTESIAN_POINT ( 'NONE',  ( 0.3278977287071176416, -6.347150352417378905, 10.49733767381180449 ) ) ;
#44060 = LINE ( 'NONE', #64328, #28745 ) ;
#44061 = FACE_OUTER_BOUND ( 'NONE', #61753, .T. ) ;
#44063 = ORIENTED_EDGE ( 'NONE', *, *, #884, .F. ) ;
#44062 = DIRECTION ( 'NONE',  ( 1.000000000000000000, -0.000000000000000000, 0.000000000000000000 ) ) ;
#44064 = CARTESIAN_POINT ( 'NONE',  ( -22.27721038036499834, 2.320305412324252803, 2.858424446490910320 ) ) ;
#44065 = EDGE_CURVE ( 'NONE', #41945, #5651, #37260, .T. ) ;
#44066 = ORIENTED_EDGE ( 'NONE', *, *, #56223, .T. ) ;
#44067 = DIRECTION ( 'NONE',  ( 0.000000000000000000, -0.8989688749565202253, -0.4380125133593881226 ) ) ;
#44068 = VERTEX_POINT ( 'NONE', #2027 ) ;
#44069 = ORIENTED_EDGE ( 'NONE', *, *, #26283, .T. ) ;
#44070 = DIRECTION ( 'NONE',  ( -1.000000000000000000, 0.000000000000000000, 0.000000000000000000 ) ) ;
#44071 = CARTESIAN_POINT ( 'NONE',  ( -12.11665614333141505, -29.85821820039599928, 8.776459307919161290 ) ) ;
#44072 = CARTESIAN_POINT ( 'NONE',  ( 36.00000000000000711, -11.10408318471055011, 6.265926637539606325 ) ) ;
#44073 = VECTOR ( 'NONE', #34675, 1000.000000000000000 ) ;
#44074 = LINE ( 'NONE', #13790, #9470 ) ;
#44075 = DIRECTION ( 'NONE',  ( 0.000000000000000000, -0.01356324068817998940, 0.9999080150203990547 ) ) ;
#44076 = DIRECTION ( 'NONE',  ( -1.000000000000000000, 0.000000000000000000, 0.000000000000000000 ) ) ;
#44077 = VERTEX_POINT ( 'NONE', #23629 ) ;
#44078 =( BOUNDED_SURFACE ( )  B_SPLINE_SURFACE ( 3, 1, ( 
 ( #59287, #53657 ),
 ( #23380, #8410 ),
 ( #23058, #28686 ),
 ( #49000, #3785 ) ),
 .UNSPECIFIED., .F., .F., .F. ) 
 B_SPLINE_SURFACE_WITH_KNOTS ( ( 4, 4 ),
 ( 2, 2 ),
 ( 0.000000000000000000, 1.000000000000000000 ),
 ( 0.000000000000000000, 1.000000000000000000 ),
 .UNSPECIFIED. ) 
 GEOMETRIC_REPRESENTATION_ITEM ( )  RATIONAL_B_SPLINE_SURFACE ( (
 ( 1.000000000000000000, 1.000000000000000000),
 ( 0.9942764183789327692, 0.8450855930916580938),
 ( 0.9942764183789327692, 0.8450855930916580938),
 ( 1.000000000000000000, 1.000000000000000000) ) ) 
 REPRESENTATION_ITEM ( '' )  SURFACE ( )  );
#44079 = CARTESIAN_POINT ( 'NONE',  ( -22.27722019110237284, 0.6492757894141428787, 3.623957119342502864 ) ) ;
#44080 = ORIENTED_EDGE ( 'NONE', *, *, #12436, .F. ) ;
#44081 = CARTESIAN_POINT ( 'NONE',  ( 0.9232058338315048962, 1.793035206307345808, 12.34162163148534219 ) ) ;
#44082 = FACE_OUTER_BOUND ( 'NONE', #15208, .T. ) ;
#44083 = ORIENTED_EDGE ( 'NONE', *, *, #25836, .F. ) ;
#44084 = CARTESIAN_POINT ( 'NONE',  ( 2.260457164927188511, -7.499412009325147288, 1.462935478981580051 ) ) ;
#44085 = LINE ( 'NONE', #33115, #39384 ) ;
#44086 = CARTESIAN_POINT ( 'NONE',  ( 2.000000000000001776, 6.643843315911821534, -1.507714007300717585 ) ) ;
#44087 = EDGE_CURVE ( 'NONE', #49125, #17671, #42117, .T. ) ;
#44088 = CARTESIAN_POINT ( 'NONE',  ( -22.28236030719477867, 3.035028179399219983, -2.111163412226028768 ) ) ;
#44089 = CARTESIAN_POINT ( 'NONE',  ( 3.152665057733881504, -7.719888720907738922, -1.848755561851823881 ) ) ;
#44090 = ADVANCED_FACE ( 'NONE', ( #57572 ), #42559, .T. ) ;
#44091 = CARTESIAN_POINT ( 'NONE',  ( 0.000000000000000000, -6.643843315911820646, 1.507714007300648307 ) ) ;
#44092 = EDGE_LOOP ( 'NONE', ( #62244, #19609, #18943, #21404 ) ) ;
#44093 = AXIS2_PLACEMENT_3D ( 'NONE', #49037, #39932, #60215 ) ;
#44094 =( BOUNDED_CURVE ( )  B_SPLINE_CURVE ( 3, ( #4495, #40703, #15429, #489 ),
 .UNSPECIFIED., .F., .F. ) 
 B_SPLINE_CURVE_WITH_KNOTS ( ( 4, 4 ),
 ( 1.199391138076630670, 1.218670143242656545 ),
 .UNSPECIFIED. ) 
 CURVE ( )  GEOMETRIC_REPRESENTATION_ITEM ( )  RATIONAL_B_SPLINE_CURVE ( ( 1.000000000000000000, 0.9999690269031535905, 0.9999690269031535905, 1.000000000000000000 ) ) 
 REPRESENTATION_ITEM ( '' )  );
#44095 = ORIENTED_EDGE ( 'NONE', *, *, #55509, .F. ) ;
#44096 = EDGE_CURVE ( 'NONE', #5306, #42222, #41074, .T. ) ;
#44097 = DIRECTION ( 'NONE',  ( -1.000000000000000000, 0.000000000000000000, 0.000000000000000000 ) ) ;
#44098 = CARTESIAN_POINT ( 'NONE',  ( 2.368238019615359402, 4.795442552788066415, -5.994627685103000481 ) ) ;
#44099 = CARTESIAN_POINT ( 'NONE',  ( -10.79971841461721382, -9.842872838453383011, 6.865048668419092337 ) ) ;
#44100 = AXIS2_PLACEMENT_3D ( 'NONE', #39740, #53737, #44075 ) ;
#44101 = CARTESIAN_POINT ( 'NONE',  ( 2.000000000000001776, 0.000000000000000000, 0.000000000000000000 ) ) ;
#44102 = CARTESIAN_POINT ( 'NONE',  ( 2.000000000000001776, 0.000000000000000000, 0.000000000000000000 ) ) ;
#44103 = CARTESIAN_POINT ( 'NONE',  ( -8.117819346152851168, -2.374925147350410715, -11.76537966265405188 ) ) ;
#44104 = CARTESIAN_POINT ( 'NONE',  ( 2.241451721903215955, 5.887257931662910337, -4.860585618235909955 ) ) ;
#44105 = CARTESIAN_POINT ( 'NONE',  ( 2.297017764050092836, 1.490897313050684847, 7.506328781223009727 ) ) ;
#44106 = CARTESIAN_POINT ( 'NONE',  ( -37.00000000000000711, 3.827046518385245122, -11.56998259273173701 ) ) ;
#44107 = ORIENTED_EDGE ( 'NONE', *, *, #29039, .F. ) ;
#44108 = DIRECTION ( 'NONE',  ( -0.9746931518056332067, -0.2235469969004301727, 0.000000000000000000 ) ) ;
#44109 = CARTESIAN_POINT ( 'NONE',  ( -26.43258404273188233, -0.2934201954354099806, 3.465947334857387041 ) ) ;
#44110 = CARTESIAN_POINT ( 'NONE',  ( 2.665405856346782620, 6.944580094494342326, 6.580881457836746939 ) ) ;
#44111 = B_SPLINE_CURVE_WITH_KNOTS ( 'NONE', 3,
 ( #37483, #21550, #31822, #933, #11237, #21199, #26855 ),
 .UNSPECIFIED., .F., .F.,
 ( 4, 3, 4 ),
 ( 9.486769009248163798E-19, 6.607638129004467199E-05, 8.338150981373126328E-05 ),
 .UNSPECIFIED. ) ;
#44112 = CIRCLE ( 'NONE', #15443, 3.999999999999999556 ) ;
#44113 = EDGE_CURVE ( 'NONE', #2142, #61832, #47912, .T. ) ;
#44114 = CARTESIAN_POINT ( 'NONE',  ( 2.305787727787083519, -6.545285700970500109, -3.971363876084033961 ) ) ;
#44115 = EDGE_CURVE ( 'NONE', #18081, #16086, #3944, .T. ) ;
#44116 = CARTESIAN_POINT ( 'NONE',  ( 1.719304012340749033, -5.066286238787660601, -11.67935079956571087 ) ) ;
#44117 = EDGE_LOOP ( 'NONE', ( #50553, #53535, #65308, #57836 ) ) ;
#44118 = CARTESIAN_POINT ( 'NONE',  ( -35.04709527796842394, -0.007030359780627049027, 0.01016988845956717791 ) ) ;
#44119 = CARTESIAN_POINT ( 'NONE',  ( 29.14248432514131437, 11.83124089669624901, 6.514580338249294833 ) ) ;
#44120 = CARTESIAN_POINT ( 'NONE',  ( 0.8665813290829081916, -31.03691730605172694, -14.44326482629603881 ) ) ;
#44121 = ORIENTED_EDGE ( 'NONE', *, *, #31510, .T. ) ;
#44122 = DIRECTION ( 'NONE',  ( -1.000000000000000000, 0.000000000000000000, 0.000000000000000000 ) ) ;
#44123 = CARTESIAN_POINT ( 'NONE',  ( -22.46225619532220819, 4.233934615764574083, -0.1595555201818063817 ) ) ;
#44124 = DIRECTION ( 'NONE',  ( 1.000000000000000000, 0.000000000000000000, 0.000000000000000000 ) ) ;
#44125 = PRODUCT_DEFINITION_FORMATION_WITH_SPECIFIED_SOURCE ( 'ANY', '', #54043, .NOT_KNOWN. ) ;
#44126 = ADVANCED_FACE ( 'NONE', ( #28281 ), #48577, .T. ) ;
#44127 = CARTESIAN_POINT ( 'NONE',  ( 0.2911222467163514516, -8.040284153519429822, 9.248441845564659758 ) ) ;
#44128 = CARTESIAN_POINT ( 'NONE',  ( -37.00000000000000711, -11.73808581813438323, 0.4353888892047964587 ) ) ;
#44129 = ORIENTED_EDGE ( 'NONE', *, *, #41064, .F. ) ;
#44130 = CARTESIAN_POINT ( 'NONE',  ( 2.261269890822072082, -7.226741992146805238, 2.481875047312914528 ) ) ;
#44131 = CARTESIAN_POINT ( 'NONE',  ( 35.00000000000000000, 4.545979934229410269, -11.30684963584391234 ) ) ;
#44133 = CIRCLE ( 'NONE', #61131, 5.000000000000000888 ) ;
#44132 = CARTESIAN_POINT ( 'NONE',  ( -37.00000000000000711, -11.07407352312210058, -3.916263239775468197 ) ) ;
#44134 = CARTESIAN_POINT ( 'NONE',  ( 2.430348790457645070, -4.796903114819432545, 6.019963855523926988 ) ) ;
#44135 = CARTESIAN_POINT ( 'NONE',  ( 2.262775599886258426, 7.548684916004849477, -1.187656132455193081 ) ) ;
#44136 = CYLINDRICAL_SURFACE ( 'NONE', #37544, 12.74999999999999822 ) ;
#44137 = CARTESIAN_POINT ( 'NONE',  ( -35.00000000000000000, 0.000000000000000000, 0.000000000000000000 ) ) ;
#44138 = CARTESIAN_POINT ( 'NONE',  ( -35.00000000000000000, 0.000000000000000000, 0.000000000000000000 ) ) ;
#44139 = ORIENTED_EDGE ( 'NONE', *, *, #55631, .T. ) ;
#44140 = ADVANCED_FACE ( 'NONE', ( #58903 ), #28936, .T. ) ;
#44141 = ORIENTED_EDGE ( 'NONE', *, *, #6757, .T. ) ;
#44142 = FILL_AREA_STYLE ('',( #7935 ) ) ;
#44143 = ORIENTED_EDGE ( 'NONE', *, *, #28591, .T. ) ;
#44144 = B_SPLINE_CURVE_WITH_KNOTS ( 'NONE', 3,
 ( #49525, #45825, #29228, #55138, #19584, #14248, #3963, #34831, #24226, #9247 ),
 .UNSPECIFIED., .F., .F.,
 ( 4, 3, 3, 4 ),
 ( 0.000000000000000000, 6.607638129004591882E-05, 9.911389841680699796E-05, 0.0001667630577588627449 ),
 .UNSPECIFIED. ) ;
#44145 = FILL_AREA_STYLE_COLOUR ( '', #62171 ) ;
#44146 = EDGE_CURVE ( 'NONE', #56061, #63467, #34241, .T. ) ;
#44148 = CARTESIAN_POINT ( 'NONE',  ( -22.28856623400852399, 2.585606290939623797, -2.668530796663830973 ) ) ;
#44147 = CIRCLE ( 'NONE', #54791, 12.75000000000000178 ) ;
#44149 = DIRECTION ( 'NONE',  ( 1.000000000000000000, 0.000000000000000000, 0.000000000000000000 ) ) ;
#44150 = CARTESIAN_POINT ( 'NONE',  ( -22.30986928587821794, -1.665628047792428568, 3.392803916780406492 ) ) ;
#44151 = ORIENTED_EDGE ( 'NONE', *, *, #12603, .T. ) ;
#44152 = CARTESIAN_POINT ( 'NONE',  ( 0.2767916011545374366, 5.959903879715737318, -10.70244578860289053 ) ) ;
#44153 = CARTESIAN_POINT ( 'NONE',  ( 37.00000000000000711, 4.705694406421931860E-17, -3.469127814946512892E-15 ) ) ;
#44154 = CARTESIAN_POINT ( 'NONE',  ( 24.89615308551568162, -1.134373919475322623, 13.45815213920829656 ) ) ;
#44155 = ORIENTED_EDGE ( 'NONE', *, *, #4876, .F. ) ;
#44156 = VERTEX_POINT ( 'NONE', #51112 ) ;
#44157 = CARTESIAN_POINT ( 'NONE',  ( 0.000000000000000000, -45.00000000000000000, 0.000000000000000000 ) ) ;
#44158 = CARTESIAN_POINT ( 'NONE',  ( 0.000000000000000000, 6.253963800348318003, -4.139799123620975685 ) ) ;
#44159 = ORIENTED_EDGE ( 'NONE', *, *, #14573, .T. ) ;
#44160 = EDGE_LOOP ( 'NONE', ( #37252, #37364, #13191, #985 ) ) ;
#44161 = CARTESIAN_POINT ( 'NONE',  ( 2.000000000000001776, 0.000000000000000000, 0.000000000000000000 ) ) ;
#44162 = ADVANCED_FACE ( 'NONE', ( #39226 ), #59207, .T. ) ;
#44163 = FACE_OUTER_BOUND ( 'NONE', #1217, .T. ) ;
#44164 = CARTESIAN_POINT ( 'NONE',  ( 0.2767916011545381028, 10.51265105824871426, -6.288637995698005412 ) ) ;
#44165 = CYLINDRICAL_SURFACE ( 'NONE', #6534, 4.945031439545089391 ) ;
#44166 = CARTESIAN_POINT ( 'NONE',  ( -35.00000000000000000, -9.512294188640947112, 6.891188680298791169 ) ) ;
#44167 = EDGE_CURVE ( 'NONE', #32142, #27444, #19828, .T. ) ;
#44168 = CARTESIAN_POINT ( 'NONE',  ( 36.00000000000000711, 5.556331110570566167, 11.47561260193570654 ) ) ;
#44169 = ORIENTED_EDGE ( 'NONE', *, *, #236, .T. ) ;
#44170 = CARTESIAN_POINT ( 'NONE',  ( -14.47334165536100059, 0.000000000000000000, 0.000000000000000000 ) ) ;
#44171 = CARTESIAN_POINT ( 'NONE',  ( -17.58491860973004961, 6.768086267375776899, 9.911307288218484501 ) ) ;
#44172 = CARTESIAN_POINT ( 'NONE',  ( -21.17861794710831091, -13.00977982294134883, -3.604945070120774808 ) ) ;
#44173 = CARTESIAN_POINT ( 'NONE',  ( 0.000000000000000000, -5.097042323172487954, 5.501832381651415638 ) ) ;
#44174 = FACE_OUTER_BOUND ( 'NONE', #54754, .T. ) ;
#44175 = CARTESIAN_POINT ( 'NONE',  ( -35.00000000000000000, -10.12742074351902133, 7.745827850122974034 ) ) ;
#44176 = DIRECTION ( 'NONE',  ( -1.000000000000000000, 0.000000000000000000, 0.000000000000000000 ) ) ;
#44177 = DIRECTION ( 'NONE',  ( 0.000000000000000000, -0.01356324068817991828, 0.9999080150203990547 ) ) ;
#44178 = CARTESIAN_POINT ( 'NONE',  ( 1.020182472821187014, 5.858468047366232057, 11.03967505355296552 ) ) ;
#44179 = ORIENTED_EDGE ( 'NONE', *, *, #45424, .F. ) ;
#44180 = CARTESIAN_POINT ( 'NONE',  ( -17.99470809830023654, 7.056672321075245335, -9.708842496525370791 ) ) ;
#44181 = CIRCLE ( 'NONE', #65376, 3.000000000000001332 ) ;
#44182 = AXIS2_PLACEMENT_3D ( 'NONE', #64617, #49681, #4126 ) ;
#44183 = ORIENTED_EDGE ( 'NONE', *, *, #43619, .T. ) ;
#44184 = DIRECTION ( 'NONE',  ( 1.000000000000000000, 0.000000000000000000, -0.000000000000000000 ) ) ;
#44185 = FACE_OUTER_BOUND ( 'NONE', #52463, .T. ) ;
#44186 = CARTESIAN_POINT ( 'NONE',  ( 1.719304012338517706, -0.7661785589593724799, 12.70777170744426243 ) ) ;
#44187 = DIRECTION ( 'NONE',  ( 1.000000000000000000, 0.000000000000000000, 0.000000000000000000 ) ) ;
#44188 = DIRECTION ( 'NONE',  ( 0.000000000000000000, -0.9937233664769772323, 0.1118654143051511785 ) ) ;
#44189 = B_SPLINE_CURVE_WITH_KNOTS ( 'NONE', 3,
 ( #38258, #34583, #54234, #24287, #8676, #39248, #28960, #49267 ),
 .UNSPECIFIED., .F., .F.,
 ( 4, 2, 2, 4 ),
 ( 0.000000000000000000, 0.0003639104015150029445, 0.0007278208030300058889, 0.001455641606060012428 ),
 .UNSPECIFIED. ) ;
#44190 = ORIENTED_EDGE ( 'NONE', *, *, #20257, .T. ) ;
#44191 = CARTESIAN_POINT ( 'NONE',  ( 0.000000000000000000, 0.000000000000000000, 0.000000000000000000 ) ) ;
#44192 = FACE_OUTER_BOUND ( 'NONE', #46476, .T. ) ;
#44193 = LINE ( 'NONE', #44499, #65117 ) ;
#44194 = CYLINDRICAL_SURFACE ( 'NONE', #52940, 12.74999999999999822 ) ;
#44195 = EDGE_CURVE ( 'NONE', #3384, #45709, #59861, .T. ) ;
#44196 = DIRECTION ( 'NONE',  ( -1.000000000000000000, 0.000000000000000000, 0.000000000000000000 ) ) ;
#44197 = EDGE_LOOP ( 'NONE', ( #7963, #63101, #25291, #54143 ) ) ;
#44198 = CARTESIAN_POINT ( 'NONE',  ( 5.514624014163232779, 0.001255375129357668438, -0.003946330869975257262 ) ) ;
#44199 = ORIENTED_EDGE ( 'NONE', *, *, #27405, .T. ) ;
#44200 = CARTESIAN_POINT ( 'NONE',  ( -37.00000000000000711, 7.561043153947966999, 9.557269938331581116 ) ) ;
#44201 = CARTESIAN_POINT ( 'NONE',  ( 2.276905613633650738, -3.955794200962162943, -6.543460433228690754 ) ) ;
#44202 = DIRECTION ( 'NONE',  ( -0.3939253465568944290, -0.9034404741085565460, 0.1691689424289735677 ) ) ;
#44203 = CYLINDRICAL_SURFACE ( 'NONE', #6558, 12.74999999999999822 ) ;
#44204 = EDGE_CURVE ( 'NONE', #10092, #11911, #27318, .T. ) ;
#44205 = VERTEX_POINT ( 'NONE', #8983 ) ;
#44206 = ORIENTED_EDGE ( 'NONE', *, *, #47537, .T. ) ;
#44207 = CARTESIAN_POINT ( 'NONE',  ( -27.19357181888462094, 10.84410562793473431, 5.138615876886901468 ) ) ;
#44208 = CARTESIAN_POINT ( 'NONE',  ( 37.00000000000000711, 4.705694406421931860E-17, -3.469127814946512892E-15 ) ) ;
#44209 = CARTESIAN_POINT ( 'NONE',  ( 2.835339799623981527, -3.628068688271626208, -6.941489812670562642 ) ) ;
#44210 = CARTESIAN_POINT ( 'NONE',  ( 0.2869720083484362805, 12.25163264065381696, 0.2084396331387086132 ) ) ;
#44211 = CARTESIAN_POINT ( 'NONE',  ( 3.031336079629822322, 6.621879275826772826, -4.304138522350520191 ) ) ;
#44212 = CARTESIAN_POINT ( 'NONE',  ( 1.549075743845217179, -12.65619669351034915, -0.6747257554048951000 ) ) ;
#44213 = ORIENTED_EDGE ( 'NONE', *, *, #35412, .F. ) ;
#44214 = ADVANCED_FACE ( 'NONE', ( #44533 ), #56411, .T. ) ;
#44215 = EDGE_LOOP ( 'NONE', ( #54501, #44423, #25078, #61997 ) ) ;
#44216 = VERTEX_POINT ( 'NONE', #3700 ) ;
#44217 = CARTESIAN_POINT ( 'NONE',  ( 2.259830038564998755, 7.225713255971581539, -2.483392345594692685 ) ) ;
#44218 = EDGE_CURVE ( 'NONE', #26747, #64221, #23098, .T. ) ;
#44219 = DIRECTION ( 'NONE',  ( 1.000000000000000000, -0.000000000000000000, -0.000000000000000000 ) ) ;
#44220 = VERTEX_POINT ( 'NONE', #13949 ) ;
#44221 = CIRCLE ( 'NONE', #11329, 12.18649999999999878 ) ;
#44222 = FACE_OUTER_BOUND ( 'NONE', #55162, .T. ) ;
#44223 = FACE_BOUND ( 'NONE', #57245, .T. ) ;
#44224 = EDGE_LOOP ( 'NONE', ( #26779, #43550, #62518, #39158 ) ) ;
#44225 = AXIS2_PLACEMENT_3D ( 'NONE', #39282, #59578, #60226 ) ;
#44226 = DIRECTION ( 'NONE',  ( -1.000000000000000000, 0.000000000000000000, -0.000000000000000000 ) ) ;
#44227 = CARTESIAN_POINT ( 'NONE',  ( 5.514624014163232779, -0.001574979445068916189, 0.003830004412313241843 ) ) ;
#44228 = DIRECTION ( 'NONE',  ( 0.000000000000000000, 0.8276889981568879007, 0.5611870653623863836 ) ) ;
#44229 = ORIENTED_EDGE ( 'NONE', *, *, #24056, .T. ) ;
#44230 = EDGE_LOOP ( 'NONE', ( #49015, #35855, #59219, #28349 ) ) ;
#44231 = CARTESIAN_POINT ( 'NONE',  ( 0.000000000000000000, -6.883677378339447372, -0.8544109087186817497 ) ) ;
#44232 = ORIENTED_EDGE ( 'NONE', *, *, #50566, .F. ) ;
#44233 = CARTESIAN_POINT ( 'NONE',  ( -36.00000000000000711, -2.696588552978969044, -12.46157735505192399 ) ) ;
#44234 = VERTEX_POINT ( 'NONE', #10197 ) ;
#44235 = EDGE_LOOP ( 'NONE', ( #24331, #22398, #61995, #17793 ) ) ;
#44236 = ORIENTED_EDGE ( 'NONE', *, *, #25086, .F. ) ;
#44237 = DIRECTION ( 'NONE',  ( 1.000000000000000000, 0.000000000000000000, 0.000000000000000000 ) ) ;
#44238 = ADVANCED_FACE ( 'NONE', ( #23962 ), #61385, .T. ) ;
#44239 = CARTESIAN_POINT ( 'NONE',  ( -7.187257474343136998, -31.45475789300778047, -14.12255545930396394 ) ) ;
#44240 = CARTESIAN_POINT ( 'NONE',  ( -47.00000000000000711, 0.000000000000000000, 0.000000000000000000 ) ) ;
#44241 = CARTESIAN_POINT ( 'NONE',  ( 1.014383007554946037, 11.58298623339620548, -4.688516792764495733 ) ) ;
#44242 = CARTESIAN_POINT ( 'NONE',  ( 0.3675815128205894289, -0.2638082659429279997, 12.27743992903066150 ) ) ;
#44243 = ORIENTED_EDGE ( 'NONE', *, *, #485, .T. ) ;
#44244 = CARTESIAN_POINT ( 'NONE',  ( 2.290907136833251201, -7.132394668149370176, -2.768669624188762945 ) ) ;
#44245 = ORIENTED_EDGE ( 'NONE', *, *, #7115, .F. ) ;
#44246 = DIRECTION ( 'NONE',  ( 0.000000000000000000, -0.8835120444460271560, 0.4684084406997820471 ) ) ;
#44247 = CARTESIAN_POINT ( 'NONE',  ( -17.77206147034625516, -6.466924801175856885, -11.85381836396156885 ) ) ;
#44248 = VERTEX_POINT ( 'NONE', #18962 ) ;
#44249 = CARTESIAN_POINT ( 'NONE',  ( -16.73444177318988579, 8.125847110238725080, 8.830413162243864633 ) ) ;
#44250 = DIRECTION ( 'NONE',  ( -1.000000000000000000, 0.000000000000000000, -0.000000000000000000 ) ) ;
#44251 = LINE ( 'NONE', #9314, #29134 ) ;
#44253 = EDGE_CURVE ( 'NONE', #32250, #61252, #6122, .T. ) ;
#44252 = ORIENTED_EDGE ( 'NONE', *, *, #60552, .F. ) ;
#44254 = ORIENTED_EDGE ( 'NONE', *, *, #59747, .T. ) ;
#44255 = CARTESIAN_POINT ( 'NONE',  ( 1.283627346226426713, 6.763590725840804119, 10.61381050043330632 ) ) ;
#44256 = VERTEX_POINT ( 'NONE', #15825 ) ;
#44257 = CARTESIAN_POINT ( 'NONE',  ( 2.350038591457883630, 4.227970903881152154, -9.744161863087125397 ) ) ;
#44258 = DIRECTION ( 'NONE',  ( 0.000000000000000000, -0.8369827122275287357, -0.5472293298355359603 ) ) ;
#44259 = CARTESIAN_POINT ( 'NONE',  ( -28.85619398320021745, 3.750539801530000439, 12.96855624952675612 ) ) ;
#44260 = CARTESIAN_POINT ( 'NONE',  ( 0.3675815128205912052, -9.235491948679950269, -8.093875121226169256 ) ) ;
#44261 = DIRECTION ( 'NONE',  ( -1.000000000000000000, 0.000000000000000000, 0.000000000000000000 ) ) ;
#44262 = VERTEX_POINT ( 'NONE', #54553 ) ;
#44263 = CARTESIAN_POINT ( 'NONE',  ( -35.04709527796842394, -0.001082316405377065083, 0.01231589140597219578 ) ) ;
#44264 = AXIS2_PLACEMENT_3D ( 'NONE', #37277, #27299, #27626 ) ;
#44265 = CARTESIAN_POINT ( 'NONE',  ( 1.719304012340734378, -11.38834240361519612, -5.690355757825884986 ) ) ;
#44266 = CIRCLE ( 'NONE', #11377, 6.936499999999987232 ) ;
#44267 = ADVANCED_FACE ( 'NONE', ( #44222 ), #64492, .T. ) ;
#44268 = CARTESIAN_POINT ( 'NONE',  ( -17.77323790556440386, -29.67638950762373540, -8.606028548248501053 ) ) ;
#44269 =( BOUNDED_CURVE ( )  B_SPLINE_CURVE ( 3, ( #6626, #51844, #47196, #1950 ),
 .UNSPECIFIED., .F., .F. ) 
 B_SPLINE_CURVE_WITH_KNOTS ( ( 4, 4 ),
 ( 4.384824308196885845, 4.401948620082515973 ),
 .UNSPECIFIED. ) 
 CURVE ( )  GEOMETRIC_REPRESENTATION_ITEM ( )  RATIONAL_B_SPLINE_CURVE ( ( 1.000000000000000000, 0.9999755633111596653, 0.9999755633111596653, 1.000000000000000000 ) ) 
 REPRESENTATION_ITEM ( '' )  );
#44270 = CARTESIAN_POINT ( 'NONE',  ( -19.47984447937493613, -3.750539801530005768, 11.39883551934753925 ) ) ;
#44271 = CARTESIAN_POINT ( 'NONE',  ( -35.00000000000000000, -2.527899948230555083, -12.49688848680886899 ) ) ;
#44272 = EDGE_CURVE ( 'NONE', #39026, #53160, #61077, .T. ) ;
#44273 = CARTESIAN_POINT ( 'NONE',  ( 2.000000000000001776, 0.000000000000000000, 0.000000000000000000 ) ) ;
#44274 = DIRECTION ( 'NONE',  ( -1.000000000000000000, 0.000000000000000000, 0.000000000000000000 ) ) ;
#44275 = CARTESIAN_POINT ( 'NONE',  ( 0.000000000000000000, -5.396716205731451943, 4.158041573745051345 ) ) ;
#44276 = ADVANCED_FACE ( 'NONE', ( #25837 ), #56076, .T. ) ;
#44277 = ORIENTED_EDGE ( 'NONE', *, *, #50298, .F. ) ;
#44278 = DIRECTION ( 'NONE',  ( 0.000000000000000000, 0.6269146997507930585, 0.7790879021242551605 ) ) ;
#44279 = VERTEX_POINT ( 'NONE', #5566 ) ;
#44280 = DIRECTION ( 'NONE',  ( 0.000000000000000000, -0.3193015301359669600, -0.9476531711828067861 ) ) ;
#44281 = DIRECTION ( 'NONE',  ( 1.000000000000000000, 0.000000000000000000, 0.000000000000000000 ) ) ;
#44282 = DIRECTION ( 'NONE',  ( 0.3865475372811021382, 0.1791957239473723762, -0.9046932595863041993 ) ) ;
#44283 = CARTESIAN_POINT ( 'NONE',  ( 0.000000000000000000, 6.586971819220387658, -3.586335490831350725 ) ) ;
#44284 = ORIENTED_EDGE ( 'NONE', *, *, #51535, .T. ) ;
#44285 = EDGE_CURVE ( 'NONE', #43866, #26911, #53870, .T. ) ;
#44286 = VERTEX_POINT ( 'NONE', #64186 ) ;
#44287 = ORIENTED_EDGE ( 'NONE', *, *, #32616, .T. ) ;
#44288 = CARTESIAN_POINT ( 'NONE',  ( 0.3401186441510243852, -7.690203051555953628, -9.562489599411604146 ) ) ;
#44289 = VERTEX_POINT ( 'NONE', #18658 ) ;
#44290 = EDGE_CURVE ( 'NONE', #13265, #56863, #44311, .T. ) ;
#44291 = CARTESIAN_POINT ( 'NONE',  ( -22.27709082389155171, -2.563977319272125133, -2.641652894015116715 ) ) ;
#44292 = DIRECTION ( 'NONE',  ( 1.000000000000000000, 0.000000000000000000, 0.000000000000000000 ) ) ;
#44293 = CARTESIAN_POINT ( 'NONE',  ( 0.2911222467163550043, 10.50411792397758326, 6.312159098066215890 ) ) ;
#44294 = DIRECTION ( 'NONE',  ( -1.000000000000000000, 0.000000000000000000, 0.000000000000000000 ) ) ;
#44295 = ORIENTED_EDGE ( 'NONE', *, *, #35824, .F. ) ;
#44296 = DIRECTION ( 'NONE',  ( 0.000000000000000000, -0.9289767198167949713, 0.3701381553399054614 ) ) ;
#44297 = VECTOR ( 'NONE', #27720, 1000.000000000000000 ) ;
#44298 = DIRECTION ( 'NONE',  ( 0.000000000000000000, 0.000000000000000000, 1.000000000000000000 ) ) ;
#44299 = CARTESIAN_POINT ( 'NONE',  ( -35.00000000000000000, -1.591260454995328866, 12.08216339958900321 ) ) ;
#44301 = ORIENTED_EDGE ( 'NONE', *, *, #56603, .F. ) ;
#44300 = CARTESIAN_POINT ( 'NONE',  ( -37.00000000000000711, 8.954052073409602741, 9.076753354954030684 ) ) ;
#44302 = FACE_OUTER_BOUND ( 'NONE', #32883, .T. ) ;
#44303 = EDGE_LOOP ( 'NONE', ( #36454, #48180, #40925, #61638 ) ) ;
#44304 = LINE ( 'NONE', #38005, #22029 ) ;
#44305 = VERTEX_POINT ( 'NONE', #58063 ) ;
#44306 = AXIS2_PLACEMENT_3D ( 'NONE', #52908, #46944, #58230 ) ;
#44307 = CARTESIAN_POINT ( 'NONE',  ( 2.241449424704145876, 7.152834201978796713, -2.668712484599891077 ) ) ;
#44308 = CYLINDRICAL_SURFACE ( 'NONE', #50015, 12.74999999999999822 ) ;
#44309 = DIRECTION ( 'NONE',  ( 0.000000000000000000, 0.4380125133593913422, -0.8989688749565187820 ) ) ;
#44310 = CARTESIAN_POINT ( 'NONE',  ( 0.2652384529303142280, -11.48485968917276168, 4.250461213012500572 ) ) ;
#44311 = CIRCLE ( 'NONE', #30496, 5.000000000000000000 ) ;
#44312 = CYLINDRICAL_SURFACE ( 'NONE', #36600, 5.000000000000000888 ) ;
#44313 = CARTESIAN_POINT ( 'NONE',  ( 0.2648321136542690080, -4.054947570138820900, -11.55519783395232203 ) ) ;
#44315 = ORIENTED_EDGE ( 'NONE', *, *, #7362, .T. ) ;
#44314 = CARTESIAN_POINT ( 'NONE',  ( 0.000000000000000000, -3.155844197800055539, -6.177028383390492650 ) ) ;
#44316 = ORIENTED_EDGE ( 'NONE', *, *, #48608, .F. ) ;
#44317 = DIRECTION ( 'NONE',  ( -1.000000000000000000, 0.000000000000000000, 0.000000000000000000 ) ) ;
#44318 = VERTEX_POINT ( 'NONE', #61718 ) ;
#44319 = ORIENTED_EDGE ( 'NONE', *, *, #39999, .T. ) ;
#44320 = CARTESIAN_POINT ( 'NONE',  ( 1.459561108994131606, 1.570807238540870232, -12.54631635028895786 ) ) ;
#44321 = DIRECTION ( 'NONE',  ( 0.000000000000000000, 0.000000000000000000, 1.000000000000000000 ) ) ;
#44322 = CARTESIAN_POINT ( 'NONE',  ( 1.937114397841935398, -3.111612666689993922, -12.45230409340484634 ) ) ;
#44323 = CARTESIAN_POINT ( 'NONE',  ( 0.2872850955227719827, -10.50585060073184884, 6.306790329742891110 ) ) ;
#44324 = LINE ( 'NONE', #27724, #62426 ) ;
#44325 = EDGE_CURVE ( 'NONE', #4816, #22798, #50689, .T. ) ;
#44326 = CARTESIAN_POINT ( 'NONE',  ( 0.2648321136542690080, 10.67551415837658801, -5.999882851577366338 ) ) ;
#44327 = CARTESIAN_POINT ( 'NONE',  ( 35.00000000000000000, -11.99999999999997335, 0.000000000000000000 ) ) ;
#44328 = ORIENTED_EDGE ( 'NONE', *, *, #48042, .T. ) ;
#44329 = CARTESIAN_POINT ( 'NONE',  ( 2.000000000000001776, -5.997115278587647147, 3.485633455389469226 ) ) ;
#44330 = CARTESIAN_POINT ( 'NONE',  ( 2.251139882113958990, -5.770207524085861905, -5.003859976903250129 ) ) ;
#44331 = CARTESIAN_POINT ( 'NONE',  ( -17.28242249393871077, -6.356211991155408469, 11.91462509628643396 ) ) ;
#44332 = VERTEX_POINT ( 'NONE', #42738 ) ;
#44333 = AXIS2_PLACEMENT_3D ( 'NONE', #7415, #2802, #53972 ) ;
#44334 = EDGE_CURVE ( 'NONE', #40228, #50945, #14575, .T. ) ;
#44335 = AXIS2_PLACEMENT_3D ( 'NONE', #12582, #2663, #43179 ) ;
#44336 = CARTESIAN_POINT ( 'NONE',  ( 2.241449424704146320, -2.668712484599915058, -7.152834201978786943 ) ) ;
#44337 = ADVANCED_FACE ( 'NONE', ( #57399 ), #41425, .T. ) ;
#44338 = CARTESIAN_POINT ( 'NONE',  ( -7.720452942165356269, -2.151506517681229802, 13.32786889207912573 ) ) ;
#44339 = EDGE_CURVE ( 'NONE', #20076, #153, #52084, .T. ) ;
#44340 = ORIENTED_EDGE ( 'NONE', *, *, #21431, .F. ) ;
#44341 = DIRECTION ( 'NONE',  ( 0.000000000000000000, -0.01356324068817992175, 0.9999080150203990547 ) ) ;
#44342 = LINE ( 'NONE', #19090, #45270 ) ;
#44343 = DIRECTION ( 'NONE',  ( 0.000000000000000000, 0.01356324068817998073, -0.9999080150203990547 ) ) ;
#44344 = AXIS2_PLACEMENT_3D ( 'NONE', #46383, #57027, #47693 ) ;
#44345 = EDGE_CURVE ( 'NONE', #16346, #55528, #65564, .T. ) ;
#44346 = CARTESIAN_POINT ( 'NONE',  ( 3.152665057735657861, -7.609997527621795932, -2.258875078500884204 ) ) ;
#44347 = FACE_OUTER_BOUND ( 'NONE', #16894, .T. ) ;
#44348 = ORIENTED_EDGE ( 'NONE', *, *, #8180, .F. ) ;
#44349 = CARTESIAN_POINT ( 'NONE',  ( 2.251152103363646795, 0.1252683866805144597, 7.636644423939547011 ) ) ;
#44350 = ADVANCED_FACE ( 'NONE', ( #52747 ), #22143, .T. ) ;
#44351 = CARTESIAN_POINT ( 'NONE',  ( 0.2833330754217391889, -12.09951353627562298, 1.928200609300433355 ) ) ;
#44352 = DIRECTION ( 'NONE',  ( 0.000000000000000000, 0.8009703041134189627, 0.5987040770935648792 ) ) ;
#44353 = ORIENTED_EDGE ( 'NONE', *, *, #4180, .T. ) ;
#44354 = FACE_OUTER_BOUND ( 'NONE', #64973, .T. ) ;
#44355 = CARTESIAN_POINT ( 'NONE',  ( 2.241506898688419458, 6.631235260227164474, 3.783130304541451050 ) ) ;
#44356 = VERTEX_POINT ( 'NONE', #37435 ) ;
#44357 = ORIENTED_EDGE ( 'NONE', *, *, #1936, .F. ) ;
#44358 = DIRECTION ( 'NONE',  ( 0.000000000000000000, 0.01356324068818000848, -0.9999080150203990547 ) ) ;
#44359 = EDGE_LOOP ( 'NONE', ( #8384, #59166, #48702, #19580 ) ) ;
#44360 = EDGE_CURVE ( 'NONE', #15355, #22226, #42161, .T. ) ;
#44361 = DIRECTION ( 'NONE',  ( 0.000000000000000000, 0.01356324068817992175, -0.9999080150203990547 ) ) ;
#44362 = CARTESIAN_POINT ( 'NONE',  ( -37.00000000000000711, -9.493370459201647904, -6.917234959366931335 ) ) ;
#44363 = CARTESIAN_POINT ( 'NONE',  ( 0.2648321136542702847, -6.245325033825803729, 10.53380804838496232 ) ) ;
#44364 = CARTESIAN_POINT ( 'NONE',  ( -35.00000000000000000, 10.99909370905157324, 5.246972444134057056 ) ) ;
#44365 = ADVANCED_FACE ( 'NONE', ( #7170 ), #21502, .T. ) ;
#44366 = DIRECTION ( 'NONE',  ( -0.000000000000000000, -1.000000000000000000, -0.000000000000000000 ) ) ;
#44368 = ORIENTED_EDGE ( 'NONE', *, *, #52732, .T. ) ;
#44367 = CARTESIAN_POINT ( 'NONE',  ( -37.00000000000000711, 0.7008968033238769380, 12.16632754454237286 ) ) ;
#44369 = CARTESIAN_POINT ( 'NONE',  ( -22.27720387087365239, 2.302200479844943359, 2.873095842208868156 ) ) ;
#44370 = VERTEX_POINT ( 'NONE', #11508 ) ;
#44371 = CARTESIAN_POINT ( 'NONE',  ( -35.00000000000000000, 11.99999999999999289, 1.469576158976823158E-15 ) ) ;
#44372 = ORIENTED_EDGE ( 'NONE', *, *, #65136, .F. ) ;
#44373 = ORIENTED_EDGE ( 'NONE', *, *, #17032, .T. ) ;
#44374 = CARTESIAN_POINT ( 'NONE',  ( -25.79691289529483456, 11.91773619621119984, 6.342745573918120883 ) ) ;
#44375 = CARTESIAN_POINT ( 'NONE',  ( 1.845799476744150569, -28.15607794640468597, 13.84328548073729870 ) ) ;
#44376 = AXIS2_PLACEMENT_3D ( 'NONE', #31245, #41865, #51550 ) ;
#44377 = CARTESIAN_POINT ( 'NONE',  ( 1.719304012338199517, 0.000000000000000000, 0.000000000000000000 ) ) ;
#44378 = DIRECTION ( 'NONE',  ( 0.000000000000000000, 0.000000000000000000, -1.000000000000000000 ) ) ;
#44379 = CARTESIAN_POINT ( 'NONE',  ( -35.00000000000000000, 9.060822531526156354, -7.474872387600913548 ) ) ;
#44380 = CARTESIAN_POINT ( 'NONE',  ( 1.000000000000000888, -3.937687286050851831, 6.383151168292441113 ) ) ;
#44381 = ORIENTED_EDGE ( 'NONE', *, *, #25654, .F. ) ;
#44382 = VECTOR ( 'NONE', #2227, 1000.000000000000000 ) ;
#44383 = ORIENTED_EDGE ( 'NONE', *, *, #37377, .T. ) ;
#44384 = FACE_OUTER_BOUND ( 'NONE', #45472, .T. ) ;
#44385 = CIRCLE ( 'NONE', #51877, 2.899999999999995026 ) ;
#44386 = ORIENTED_EDGE ( 'NONE', *, *, #64284, .F. ) ;
#44387 = DIRECTION ( 'NONE',  ( 1.000000000000000000, 0.000000000000000000, -0.000000000000000000 ) ) ;
#44388 = AXIS2_PLACEMENT_3D ( 'NONE', #62008, #31087, #32383 ) ;
#44389 = DIRECTION ( 'NONE',  ( 0.000000000000000000, 0.5472293298355273006, -0.8369827122275343978 ) ) ;
#44390 = FACE_OUTER_BOUND ( 'NONE', #44891, .T. ) ;
#44391 = DIRECTION ( 'NONE',  ( 1.000000000000000000, 0.000000000000000000, 0.000000000000000000 ) ) ;
#44392 = ADVANCED_FACE ( 'NONE', ( #42397 ), #6869, .T. ) ;
#44393 = CARTESIAN_POINT ( 'NONE',  ( 25.00000000000000355, -30.00000000000000000, -5.000000000000000888 ) ) ;
#44394 = CARTESIAN_POINT ( 'NONE',  ( -35.00000000000000000, 11.54110654723652196, -2.185196060783755279 ) ) ;
#44395 = ORIENTED_EDGE ( 'NONE', *, *, #54726, .F. ) ;
#44396 = ORIENTED_EDGE ( 'NONE', *, *, #25027, .T. ) ;
#44397 = CARTESIAN_POINT ( 'NONE',  ( -35.00000000000000000, 10.07641281632186114, -6.036400161834460043 ) ) ;
#44398 = CYLINDRICAL_SURFACE ( 'NONE', #3239, 12.18649999999999878 ) ;
#44399 = EDGE_CURVE ( 'NONE', #51119, #54308, #6759, .T. ) ;
#44400 = LINE ( 'NONE', #20467, #47868 ) ;
#44401 = CARTESIAN_POINT ( 'NONE',  ( 35.00000000000000000, -11.86701198550353986, 2.772148766916240348 ) ) ;
#44402 = EDGE_CURVE ( 'NONE', #8191, #2866, #58458, .T. ) ;
#44403 = DIRECTION ( 'NONE',  ( 0.000000000000000000, -0.3218879778916040602, 0.9467777615094549182 ) ) ;
#44404 = DIRECTION ( 'NONE',  ( 0.000000000000000000, -0.01356324068817998940, 0.9999080150203990547 ) ) ;
#44405 = CARTESIAN_POINT ( 'NONE',  ( 35.00000000000000000, -7.717887834988180984, 8.854740511458926377 ) ) ;
#44406 = CARTESIAN_POINT ( 'NONE',  ( 1.937114397841935398, -12.76557247858997890, -1.334979369128554305 ) ) ;
#44407 = CARTESIAN_POINT ( 'NONE',  ( 0.000000000000000000, -2.315790869867006219, -7.133520354428148025 ) ) ;
#44408 = ADVANCED_FACE ( 'NONE', ( #53059 ), #12811, .T. ) ;
#44409 = ORIENTED_EDGE ( 'NONE', *, *, #28208, .T. ) ;
#44410 = CARTESIAN_POINT ( 'NONE',  ( -20.92008205012190558, 11.37744109147144478, -3.816568647652260893 ) ) ;
#44411 = CARTESIAN_POINT ( 'NONE',  ( 22.88594695219327235, -4.822122601967141264, -10.98850006195556261 ) ) ;
#44412 = CARTESIAN_POINT ( 'NONE',  ( 5.516018279890452902, -0.003580555109620837603, -0.005752102158673828673 ) ) ;
#44413 = VECTOR ( 'NONE', #52537, 1000.000000000000114 ) ;
#44414 = CARTESIAN_POINT ( 'NONE',  ( 0.000000000000000000, 0.000000000000000000, 0.000000000000000000 ) ) ;
#44415 = CARTESIAN_POINT ( 'NONE',  ( 2.276198483117258142, -5.955030244776311044, 4.795748742147491583 ) ) ;
#44416 = AXIS2_PLACEMENT_3D ( 'NONE', #38211, #63170, #42532 ) ;
#44417 = CIRCLE ( 'NONE', #32738, 4.999999999999999112 ) ;
#44418 = ORIENTED_EDGE ( 'NONE', *, *, #21371, .F. ) ;
#44419 = CARTESIAN_POINT ( 'NONE',  ( -35.05175862995318425, 0.007207337213500572548, 0.01030783735683771241 ) ) ;
#44420 = DIRECTION ( 'NONE',  ( 0.000000000000000000, 0.000000000000000000, -1.000000000000000000 ) ) ;
#44421 = EDGE_CURVE ( 'NONE', #49715, #6120, #44768, .T. ) ;
#44422 = CARTESIAN_POINT ( 'NONE',  ( 5.911253750797971662, -28.27393032148221863, -11.47047724608643371 ) ) ;
#44423 = ORIENTED_EDGE ( 'NONE', *, *, #62003, .T. ) ;
#44424 = VECTOR ( 'NONE', #34588, 1000.000000000000000 ) ;
#44425 = DIRECTION ( 'NONE',  ( 1.000000000000000000, 0.000000000000000000, 0.000000000000000000 ) ) ;
#44426 = FACE_OUTER_BOUND ( 'NONE', #30698, .T. ) ;
#44427 = DIRECTION ( 'NONE',  ( -1.000000000000000000, -0.000000000000000000, -0.000000000000000000 ) ) ;
#44428 = EDGE_CURVE ( 'NONE', #57229, #17445, #38424, .T. ) ;
#44429 = AXIS2_PLACEMENT_3D ( 'NONE', #9235, #29517, #34517 ) ;
#44430 = CARTESIAN_POINT ( 'NONE',  ( 0.8375941296786580947, 12.43103843093986427, 0.3844307390181883610 ) ) ;
#44431 = DIRECTION ( 'NONE',  ( 1.000000000000000000, 0.000000000000000000, 0.000000000000000000 ) ) ;
#44432 = EDGE_CURVE ( 'NONE', #4911, #17999, #3858, .T. ) ;
#44433 = CARTESIAN_POINT ( 'NONE',  ( 0.9232167919969100911, 12.19756235544082834, -2.570564963838022354 ) ) ;
#44434 = EDGE_CURVE ( 'NONE', #9194, #33841, #22011, .T. ) ;
#44435 = VERTEX_POINT ( 'NONE', #18808 ) ;
#44436 = CARTESIAN_POINT ( 'NONE',  ( -35.00000000000000000, 10.91536515067641844, 4.339012074900148619 ) ) ;
#44437 = CARTESIAN_POINT ( 'NONE',  ( -7.636175482883169607, 8.975028534027133631, -10.10016484640243206 ) ) ;
#44439 = CARTESIAN_POINT ( 'NONE',  ( -16.32507661864641690, 8.302421046862596299, -10.64603329338183535 ) ) ;
#44438 =( BOUNDED_SURFACE ( )  B_SPLINE_SURFACE ( 3, 1, ( 
 ( #61921, #6086 ),
 ( #25697, #26033 ),
 ( #21017, #46631 ),
 ( #10714, #40317 ) ),
 .UNSPECIFIED., .F., .F., .F. ) 
 B_SPLINE_SURFACE_WITH_KNOTS ( ( 4, 4 ),
 ( 2, 2 ),
 ( 0.000000000000000000, 1.000000000000000000 ),
 ( 0.000000000000000000, 1.000000000000000000 ),
 .UNSPECIFIED. ) 
 GEOMETRIC_REPRESENTATION_ITEM ( )  RATIONAL_B_SPLINE_SURFACE ( (
 ( 1.000000000000000000, 1.000000000000000000),
 ( 0.9856612449720755231, 0.9999558406602322425),
 ( 0.9856612449720755231, 0.9999558406602322425),
 ( 1.000000000000000000, 1.000000000000000000) ) ) 
 REPRESENTATION_ITEM ( '' )  SURFACE ( )  );
#44440 = DIRECTION ( 'NONE',  ( 0.000000000000000000, -0.01356324068817992175, 0.9999080150203990547 ) ) ;
#44441 = CARTESIAN_POINT ( 'NONE',  ( 2.261269890822073414, 7.547924622047993637, -1.189259211195865529 ) ) ;
#44442 = CARTESIAN_POINT ( 'NONE',  ( 2.941278708680199916, -6.021511413163954884, -1.198640839021370974 ) ) ;
#44443 = EDGE_CURVE ( 'NONE', #7895, #8559, #39066, .T. ) ;
#44444 = FACE_OUTER_BOUND ( 'NONE', #16680, .T. ) ;
#44445 = FACE_OUTER_BOUND ( 'NONE', #61790, .T. ) ;
#44446 = ORIENTED_EDGE ( 'NONE', *, *, #37572, .T. ) ;
#44447 = ORIENTED_EDGE ( 'NONE', *, *, #29721, .F. ) ;
#44448 = CARTESIAN_POINT ( 'NONE',  ( -19.16592786555497696, -4.507658645640362671, -11.12154949745637822 ) ) ;
#44449 = ORIENTED_EDGE ( 'NONE', *, *, #44767, .F. ) ;
#44450 =( LENGTH_UNIT ( ) NAMED_UNIT ( * ) SI_UNIT ( .MILLI., .METRE. ) );
#44451 = CARTESIAN_POINT ( 'NONE',  ( -27.35552965826137140, 0.2619431035392177365, -3.094132632038957276 ) ) ;
#44452 = AXIS2_PLACEMENT_3D ( 'NONE', #40918, #24641, #40582 ) ;
#44453 = CARTESIAN_POINT ( 'NONE',  ( 0.9232058338315048962, 3.908895078357520703, 11.84276737136202051 ) ) ;
#44454 = ORIENTED_EDGE ( 'NONE', *, *, #20799, .F. ) ;
#44455 = CARTESIAN_POINT ( 'NONE',  ( 0.3654063281920715833, 5.910280591919207183, -10.76363796011279206 ) ) ;
#44456 = CARTESIAN_POINT ( 'NONE',  ( 2.259025283528082184, 6.547290863799087646, -3.937899517809406280 ) ) ;
#44457 = AXIS2_PLACEMENT_3D ( 'NONE', #35324, #25691, #24713 ) ;
#44458 = CARTESIAN_POINT ( 'NONE',  ( 23.47278007031500735, -4.309240334934965055, 12.79762753354781424 ) ) ;
#44459 = VERTEX_POINT ( 'NONE', #64653 ) ;
#44460 = ORIENTED_EDGE ( 'NONE', *, *, #42171, .F. ) ;
#44461 = DIRECTION ( 'NONE',  ( -1.000000000000000000, 0.000000000000000000, 0.000000000000000000 ) ) ;
#44462 = DIRECTION ( 'NONE',  ( -1.000000000000000000, -0.000000000000000000, 0.000000000000000000 ) ) ;
#44463 = VERTEX_POINT ( 'NONE', #45698 ) ;
#44464 = CARTESIAN_POINT ( 'NONE',  ( 6.145364549962366141, -8.619588047944827025, -8.357433972611021389 ) ) ;
#44465 = ORIENTED_EDGE ( 'NONE', *, *, #45552, .T. ) ;
#44466 = DIRECTION ( 'NONE',  ( 0.000000000000000000, 0.000000000000000000, 1.000000000000000000 ) ) ;
#44468 = CIRCLE ( 'NONE', #23230, 12.18649999999999878 ) ;
#44467 = CARTESIAN_POINT ( 'NONE',  ( -27.08429572838383947, -1.632445743623433421, 1.608131779585712406 ) ) ;
#44469 = EDGE_CURVE ( 'NONE', #43191, #40046, #47163, .T. ) ;
#44470 = DIRECTION ( 'NONE',  ( 0.000000000000000000, 0.01356324068817998940, -0.9999080150203990547 ) ) ;
#44471 = CARTESIAN_POINT ( 'NONE',  ( 0.3665391374699465965, -5.911453292029679396, 10.76665847464310843 ) ) ;
#44472 = DIRECTION ( 'NONE',  ( -1.000000000000000000, -0.000000000000000000, -0.000000000000000000 ) ) ;
#44473 = AXIS2_PLACEMENT_3D ( 'NONE', #29619, #39613, #60224 ) ;
#44474 = VERTEX_POINT ( 'NONE', #30076 ) ;
#44475 = DIRECTION ( 'NONE',  ( 0.000000000000000000, 0.000000000000000000, -1.000000000000000000 ) ) ;
#44476 = CARTESIAN_POINT ( 'NONE',  ( -15.23330792070994022, 7.971159899242214131, 8.970046877445025046 ) ) ;
#44477 = CIRCLE ( 'NONE', #15802, 6.936499999999987232 ) ;
#44478 = CARTESIAN_POINT ( 'NONE',  ( 0.2648978790185584908, -9.465406350830660287, 7.769924372105172949 ) ) ;
#44479 = CARTESIAN_POINT ( 'NONE',  ( -22.30625920655495165, -3.150098859949341357, 2.110841417170906009 ) ) ;
#44480 = CARTESIAN_POINT ( 'NONE',  ( -19.63490967323701142, 13.44825352614632052, -1.323441864413900770 ) ) ;
#44481 = CARTESIAN_POINT ( 'NONE',  ( -27.10512513516317412, 1.618446180706347048, -1.709353012333662880 ) ) ;
#44482 = DIRECTION ( 'NONE',  ( 0.000000000000000000, 0.000000000000000000, 1.000000000000000000 ) ) ;
#44483 = DIRECTION ( 'NONE',  ( -1.000000000000000000, 0.000000000000000000, 0.000000000000000000 ) ) ;
#44484 = EDGE_CURVE ( 'NONE', #5002, #6117, #32618, .T. ) ;
#44485 = AXIS2_PLACEMENT_3D ( 'NONE', #38031, #48696, #54345 ) ;
#44486 = DIRECTION ( 'NONE',  ( -1.000000000000000000, 0.000000000000000000, 0.000000000000000000 ) ) ;
#44487 = VERTEX_POINT ( 'NONE', #61006 ) ;
#44488 = CARTESIAN_POINT ( 'NONE',  ( 5.536195898058073439, 0.001224473329857592423, 0.008411485181668789182 ) ) ;
#44489 = ORIENTED_EDGE ( 'NONE', *, *, #62906, .T. ) ;
#44490 = CARTESIAN_POINT ( 'NONE',  ( 1.719304012338210619, 10.62216384465585328, 7.017415949611872428 ) ) ;
#44491 = CARTESIAN_POINT ( 'NONE',  ( 0.2648321136542718390, -0.1417061099915604971, 12.24520788540325178 ) ) ;
#44492 = CARTESIAN_POINT ( 'NONE',  ( -35.00000000000000000, 6.307491713049167004, -9.908974237959577991 ) ) ;
#44493 = CARTESIAN_POINT ( 'NONE',  ( 2.000000000000001776, 0.000000000000000000, 0.000000000000000000 ) ) ;
#44494 = CARTESIAN_POINT ( 'NONE',  ( 37.00000000000000711, -11.73808581813437613, 0.4353888892049613824 ) ) ;
#44495 = EDGE_CURVE ( 'NONE', #26603, #18880, #57101, .T. ) ;
#44496 = ORIENTED_EDGE ( 'NONE', *, *, #11953, .F. ) ;
#44497 = CARTESIAN_POINT ( 'NONE',  ( 0.000000000000000000, -33.00000000000000000, 0.000000000000000000 ) ) ;
#44498 = CARTESIAN_POINT ( 'NONE',  ( -35.00000000000000000, 12.38385022362081855, 3.033604067594621867 ) ) ;
#44499 = CARTESIAN_POINT ( 'NONE',  ( -25.00000000000000355, -28.99999999999999645, -5.000000000000000888 ) ) ;
#44500 = CYLINDRICAL_SURFACE ( 'NONE', #5160, 5.000000000000000888 ) ;
#44501 = EDGE_CURVE ( 'NONE', #2269, #8147, #50044, .T. ) ;
#44502 = CIRCLE ( 'NONE', #8397, 12.75000000000000178 ) ;
#44503 = CARTESIAN_POINT ( 'NONE',  ( 35.00000000000000000, 4.705694406421931860E-17, -3.469127814946512892E-15 ) ) ;
#44504 = ORIENTED_EDGE ( 'NONE', *, *, #8547, .T. ) ;
#44505 = DIRECTION ( 'NONE',  ( 1.000000000000000000, -0.000000000000000000, -0.000000000000000000 ) ) ;
#44506 = ORIENTED_EDGE ( 'NONE', *, *, #59472, .T. ) ;
#44507 = CARTESIAN_POINT ( 'NONE',  ( 2.305787727787083519, 6.545285700970583598, -3.971363876083895850 ) ) ;
#44508 = CARTESIAN_POINT ( 'NONE',  ( -24.42101984568203221, -3.884389025764515058, 1.824625598916869595 ) ) ;
#44509 = DIRECTION ( 'NONE',  ( 1.000000000000000000, 0.000000000000000000, 0.000000000000000000 ) ) ;
#44510 = CYLINDRICAL_SURFACE ( 'NONE', #57488, 2.899999999999994582 ) ;
#44511 = EDGE_CURVE ( 'NONE', #12277, #42103, #9795, .T. ) ;
#44512 = AXIS2_PLACEMENT_3D ( 'NONE', #4219, #24488, #44765 ) ;
#44513 = VERTEX_POINT ( 'NONE', #65630 ) ;
#44514 = VERTEX_POINT ( 'NONE', #55353 ) ;
#44515 = CARTESIAN_POINT ( 'NONE',  ( -27.09030469827880339, 2.221523195520540117, -0.6314616953885209272 ) ) ;
#44516 = EDGE_CURVE ( 'NONE', #33199, #64603, #41122, .T. ) ;
#44517 = AXIS2_PLACEMENT_3D ( 'NONE', #5705, #36254, #25977 ) ;
#44518 = CARTESIAN_POINT ( 'NONE',  ( 2.260457164926971796, 5.016645293557960628, 5.763213574030991992 ) ) ;
#44519 = CARTESIAN_POINT ( 'NONE',  ( 5.514970785353741078, -0.002619824551223247366, 0.003929719953530060386 ) ) ;
#44520 = DIRECTION ( 'NONE',  ( 0.000000000000000000, 0.9937233664769756780, -0.1118654143051654171 ) ) ;
#44521 = CARTESIAN_POINT ( 'NONE',  ( 0.3675815128205894289, 9.235491948680119023, -8.093875121225982738 ) ) ;
#44522 = EDGE_CURVE ( 'NONE', #7430, #15987, #12445, .T. ) ;
#44523 = CARTESIAN_POINT ( 'NONE',  ( 2.000000000000001776, -4.570217215903314312, -5.218059682435693958 ) ) ;
#44524 = CARTESIAN_POINT ( 'NONE',  ( -18.89934820819560102, -11.99999999999998934, 0.3178145231930626369 ) ) ;
#44525 = ORIENTED_EDGE ( 'NONE', *, *, #17917, .F. ) ;
#44526 = ORIENTED_EDGE ( 'NONE', *, *, #52931, .F. ) ;
#44527 = AXIS2_PLACEMENT_3D ( 'NONE', #36197, #25582, #55184 ) ;
#44528 = VERTEX_POINT ( 'NONE', #40368 ) ;
#44529 = DIRECTION ( 'NONE',  ( -1.000000000000000000, 0.000000000000000000, 0.000000000000000000 ) ) ;
#44530 = CARTESIAN_POINT ( 'NONE',  ( -25.00000000000000355, -28.99999999999999645, 1.530808498934191521E-15 ) ) ;
#44532 = EDGE_CURVE ( 'NONE', #19799, #47363, #1918, .T. ) ;
#44531 = EDGE_LOOP ( 'NONE', ( #9688, #47847, #29263, #64209 ) ) ;
#44533 = FACE_OUTER_BOUND ( 'NONE', #32048, .T. ) ;
#44534 = FACE_BOUND ( 'NONE', #31820, .T. ) ;
#44535 = ORIENTED_EDGE ( 'NONE', *, *, #24082, .F. ) ;
#44536 = CARTESIAN_POINT ( 'NONE',  ( 2.899286259009687061, 7.250549018622942654, 3.018334250363109206 ) ) ;
#44537 = DIRECTION ( 'NONE',  ( 1.000000000000000000, 0.000000000000000000, -0.000000000000000000 ) ) ;
#44538 = CARTESIAN_POINT ( 'NONE',  ( -27.08639648637141661, -2.223359598374791801, -0.5801562253478093067 ) ) ;
#44539 = EDGE_LOOP ( 'NONE', ( #77, #25006, #56652, #52683 ) ) ;
#44540 = VERTEX_POINT ( 'NONE', #21419 ) ;
#44541 = CARTESIAN_POINT ( 'NONE',  ( 2.253265082352432724, 2.491579069691589154, 7.220580418434027870 ) ) ;
#44542 = ORIENTED_EDGE ( 'NONE', *, *, #43964, .F. ) ;
#44543 = CARTESIAN_POINT ( 'NONE',  ( 0.000000000000000000, 0.000000000000000000, 0.000000000000000000 ) ) ;
#44544 = ORIENTED_EDGE ( 'NONE', *, *, #50647, .T. ) ;
#44545 = ORIENTED_EDGE ( 'NONE', *, *, #41245, .F. ) ;
#44546 = ORIENTED_EDGE ( 'NONE', *, *, #52565, .T. ) ;
#44547 = CARTESIAN_POINT ( 'NONE',  ( 2.000000000000001776, 0.000000000000000000, 0.000000000000000000 ) ) ;
#44548 = CARTESIAN_POINT ( 'NONE',  ( -35.04709527796842394, 0.007095259204987700019, -0.01012471662515009030 ) ) ;
#44549 = CIRCLE ( 'NONE', #6327, 4.999999999999999112 ) ;
#44550 = AXIS2_PLACEMENT_3D ( 'NONE', #63959, #59637, #13098 ) ;
#44551 = FACE_OUTER_BOUND ( 'NONE', #13104, .T. ) ;
#44552 = DIRECTION ( 'NONE',  ( -1.000000000000000000, 0.000000000000000000, 0.000000000000000000 ) ) ;
#44553 = ORIENTED_EDGE ( 'NONE', *, *, #51882, .T. ) ;
#44554 = CARTESIAN_POINT ( 'NONE',  ( 37.00000000000000711, -3.340853584269612764, -11.26103545359855040 ) ) ;
#44555 = ADVANCED_FACE ( 'NONE', ( #31066 ), #31700, .T. ) ;
#44556 = ORIENTED_EDGE ( 'NONE', *, *, #43787, .T. ) ;
#44557 = CARTESIAN_POINT ( 'NONE',  ( 35.00000000000000000, -6.657191900728386180, -9.677500615117878624 ) ) ;
#44558 = CARTESIAN_POINT ( 'NONE',  ( -35.00000000000000000, 10.43555801961483098, -5.391785509270847321 ) ) ;
#44559 = VERTEX_POINT ( 'NONE', #36708 ) ;
#44560 = DIRECTION ( 'NONE',  ( 0.000000000000000000, 0.01356324068817998940, -0.9999080150203990547 ) ) ;
#44561 = CARTESIAN_POINT ( 'NONE',  ( 0.2706063244538043921, 4.023948952279264191, 11.56807224179754279 ) ) ;
#44562 = DIRECTION ( 'NONE',  ( -1.000000000000000000, 0.000000000000000000, -0.000000000000000000 ) ) ;
#44563 = VECTOR ( 'NONE', #42549, 1000.000000000000000 ) ;
#44564 = VERTEX_POINT ( 'NONE', #5828 ) ;
#44565 = VERTEX_POINT ( 'NONE', #61986 ) ;
#44566 = CARTESIAN_POINT ( 'NONE',  ( -35.04643116707788408, 0.001845126042312322800, 0.01204777744935429939 ) ) ;
#44567 = VECTOR ( 'NONE', #13127, 1000.000000000000000 ) ;
#44568 = ORIENTED_EDGE ( 'NONE', *, *, #46386, .F. ) ;
#44569 = CARTESIAN_POINT ( 'NONE',  ( 2.034671305879535819, 4.647127512369766400, -10.71175679137433612 ) ) ;
#44570 = CARTESIAN_POINT ( 'NONE',  ( 0.000000000000000000, 2.315790869867158985, -7.133520354428100951 ) ) ;
#44571 = CARTESIAN_POINT ( 'NONE',  ( -19.27703245284564915, -30.00000000000000711, 5.988254523999585466 ) ) ;
#44572 = CARTESIAN_POINT ( 'NONE',  ( -3.318310207868118589, 7.727984809976963909, 9.215577152005407058 ) ) ;
#44573 = CARTESIAN_POINT ( 'NONE',  ( 13.39520346909927184, 10.59327504029797851, -5.642169197513929646 ) ) ;
#44574 = EDGE_CURVE ( 'NONE', #52575, #1524, #17785, .T. ) ;
#44575 = EDGE_LOOP ( 'NONE', ( #65642, #6809, #38396, #22908 ) ) ;
#44576 = CIRCLE ( 'NONE', #21233, 2.899999999999994582 ) ;
#44577 = CARTESIAN_POINT ( 'NONE',  ( 2.241536586108914264, 3.811784405792441710, -6.614789707676422381 ) ) ;
#44578 = LINE ( 'NONE', #3410, #1976 ) ;
#44579 = EDGE_CURVE ( 'NONE', #46339, #5624, #791, .T. ) ;
#44580 = CARTESIAN_POINT ( 'NONE',  ( 0.2717059086739048723, -12.09156413799788510, -1.953280559502818647 ) ) ;
#44581 = CARTESIAN_POINT ( 'NONE',  ( 2.835339799623985080, -5.281994181469023886, 5.783398714696532217 ) ) ;
#44582 = CARTESIAN_POINT ( 'NONE',  ( 2.241352910868908310, -5.901537464758421336, -4.843133558968188979 ) ) ;
#44583 = FACE_OUTER_BOUND ( 'NONE', #17843, .T. ) ;
#44584 = LINE ( 'NONE', #64235, #30127 ) ;
#44585 = ADVANCED_FACE ( 'NONE', ( #36382 ), #46685, .T. ) ;
#44586 = CIRCLE ( 'NONE', #65806, 12.74999999999999822 ) ;
#44587 = AXIS2_PLACEMENT_3D ( 'NONE', #18533, #18831, #28799 ) ;
#44588 = ORIENTED_EDGE ( 'NONE', *, *, #65673, .F. ) ;
#44589 = CARTESIAN_POINT ( 'NONE',  ( 9.976349855587246296, -11.94372303670957081, -1.164441368110342490 ) ) ;
#44590 = ORIENTED_EDGE ( 'NONE', *, *, #25301, .F. ) ;
#44591 = CARTESIAN_POINT ( 'NONE',  ( 2.000000000000001776, -5.888698556700776798, 3.665823448873372747 ) ) ;
#44592 = DIRECTION ( 'NONE',  ( 0.000000000000000000, -0.9635499925192254622, 0.2675283385292119842 ) ) ;
#44593 = CARTESIAN_POINT ( 'NONE',  ( 2.931247277082682068, -7.508560300462421289, 2.338794445044965808 ) ) ;
#44594 = CARTESIAN_POINT ( 'NONE',  ( 2.241528039335006994, 3.803597072146535751, 6.619488482362950954 ) ) ;
#44595 = VERTEX_POINT ( 'NONE', #47671 ) ;
#44596 = ORIENTED_EDGE ( 'NONE', *, *, #20034, .T. ) ;
#44597 = VERTEX_POINT ( 'NONE', #47359 ) ;
#44598 = CARTESIAN_POINT ( 'NONE',  ( 2.770579946183335807, 2.954332771348919362, -7.230573341413116140 ) ) ;
#44599 = AXIS2_PLACEMENT_3D ( 'NONE', #63423, #45124, #3919 ) ;
#44600 = EDGE_CURVE ( 'NONE', #48767, #23964, #6456, .T. ) ;
#44601 = LINE ( 'NONE', #39637, #44841 ) ;
#44602 = VERTEX_POINT ( 'NONE', #51378 ) ;
#44603 = CARTESIAN_POINT ( 'NONE',  ( 3.100650473569742438, 5.767490999797108664, 5.429218121582397139 ) ) ;
#44604 = CYLINDRICAL_SURFACE ( 'NONE', #49606, 4.999999999999999112 ) ;
#44605 = AXIS2_PLACEMENT_3D ( 'NONE', #42069, #48072, #32091 ) ;
#44606 = CARTESIAN_POINT ( 'NONE',  ( 0.2759803524722215795, 10.51260004517012270, 6.288205958087823788 ) ) ;
#44607 = CARTESIAN_POINT ( 'NONE',  ( 3.152665057734108878, -7.886634106564198277, 0.9030954876737806725 ) ) ;
#44608 = VERTEX_POINT ( 'NONE', #37021 ) ;
#44609 = DIRECTION ( 'NONE',  ( -1.000000000000000000, 0.000000000000000000, 0.000000000000000000 ) ) ;
#44610 = CARTESIAN_POINT ( 'NONE',  ( -0.9057367950582522198, -28.12814853318315400, -13.89764383195144326 ) ) ;
#44611 = CARTESIAN_POINT ( 'NONE',  ( 2.242418902651940993, -1.423836467585299914, -7.500817491983890584 ) ) ;
#44613 = ORIENTED_EDGE ( 'NONE', *, *, #58670, .F. ) ;
#44612 = CARTESIAN_POINT ( 'NONE',  ( -14.47334165536100059, 0.000000000000000000, -6.000000000000000888 ) ) ;
#44614 = CARTESIAN_POINT ( 'NONE',  ( -35.00000000000000000, 0.000000000000000000, 0.000000000000000000 ) ) ;
#44615 = ORIENTED_EDGE ( 'NONE', *, *, #20257, .F. ) ;
#44616 = CARTESIAN_POINT ( 'NONE',  ( 0.3223008802179271326, -6.343104382804245489, -10.49760329338526432 ) ) ;
#44617 = AXIS2_PLACEMENT_3D ( 'NONE', #10698, #25678, #23470 ) ;
#44618 = EDGE_LOOP ( 'NONE', ( #58573, #12526, #16798, #11165 ) ) ;
#44619 = DIRECTION ( 'NONE',  ( 0.000000000000000000, 0.000000000000000000, 1.000000000000000000 ) ) ;
#44620 = CARTESIAN_POINT ( 'NONE',  ( 0.000000000000000000, 0.000000000000000000, 0.000000000000000000 ) ) ;
#44621 = CARTESIAN_POINT ( 'NONE',  ( 0.000000000000000000, -5.662015959325215952, 4.918493191653933394 ) ) ;
#44622 = DIRECTION ( 'NONE',  ( 1.000000000000000000, -0.000000000000000000, 0.000000000000000000 ) ) ;
#44623 = DIRECTION ( 'NONE',  ( 0.000000000000000000, -0.01356324068817998940, 0.9999080150203990547 ) ) ;
#44624 = CARTESIAN_POINT ( 'NONE',  ( -9.574630011864375234, -3.691104384415131001, -12.98917911986310081 ) ) ;
#44625 = CARTESIAN_POINT ( 'NONE',  ( 0.3537226245948357217, -3.952322262392311103, -11.62199823003437871 ) ) ;
#44627 = ORIENTED_EDGE ( 'NONE', *, *, #9899, .T. ) ;
#44626 = CARTESIAN_POINT ( 'NONE',  ( 10.12151447205148536, 13.48202713789778429, -0.7009852765882638170 ) ) ;
#44628 = AXIS2_PLACEMENT_3D ( 'NONE', #60756, #30481, #40456 ) ;
#44629 = ADVANCED_FACE ( 'NONE', ( #17420 ), #41695, .T. ) ;
#44630 = ORIENTED_EDGE ( 'NONE', *, *, #62567, .T. ) ;
#44631 = LINE ( 'NONE', #59633, #45437 ) ;
#44632 = ORIENTED_EDGE ( 'NONE', *, *, #6773, .T. ) ;
#44633 = EDGE_CURVE ( 'NONE', #40874, #51496, #808, .T. ) ;
#44634 = ORIENTED_EDGE ( 'NONE', *, *, #37619, .F. ) ;
#44635 = CARTESIAN_POINT ( 'NONE',  ( -37.00000000000000711, -1.908798535168293897, -12.60630747491665282 ) ) ;
#44636 = CARTESIAN_POINT ( 'NONE',  ( -22.31328051695926007, -2.608921479762108753, 2.748895659348124187 ) ) ;
#44637 = CARTESIAN_POINT ( 'NONE',  ( -47.00000000000000711, 0.000000000000000000, 0.000000000000000000 ) ) ;
#44638 = CARTESIAN_POINT ( 'NONE',  ( 0.000000000000000000, 1.530946385938383614, 7.342084388195340594 ) ) ;
#44639 = CARTESIAN_POINT ( 'NONE',  ( 37.00000000000000711, 2.905556151562782574, 11.38112321385047210 ) ) ;
#44640 = CARTESIAN_POINT ( 'NONE',  ( 2.305787727787084407, 7.249469779319909435, 2.461236246751095536 ) ) ;
#44641 = VECTOR ( 'NONE', #65365, 1000.000000000000000 ) ;
#44642 = VECTOR ( 'NONE', #11778, 1000.000000000000000 ) ;
#44643 = ADVANCED_FACE ( 'NONE', ( #26736 ), #29368, .T. ) ;
#44644 = AXIS2_PLACEMENT_3D ( 'NONE', #2849, #7152, #2169 ) ;
#44645 = DIRECTION ( 'NONE',  ( -1.000000000000000000, 0.000000000000000000, 0.000000000000000000 ) ) ;
#44646 =( BOUNDED_SURFACE ( )  B_SPLINE_SURFACE ( 3, 1, ( 
 ( #1939, #42468 ),
 ( #32176, #22206 ),
 ( #46194, #51523 ),
 ( #11262, #52501 ) ),
 .UNSPECIFIED., .F., .F., .F. ) 
 B_SPLINE_SURFACE_WITH_KNOTS ( ( 4, 4 ),
 ( 2, 2 ),
 ( 0.000000000000000000, 1.000000000000000000 ),
 ( 0.000000000000000000, 1.000000000000000000 ),
 .UNSPECIFIED. ) 
 GEOMETRIC_REPRESENTATION_ITEM ( )  RATIONAL_B_SPLINE_SURFACE ( (
 ( 1.000000000000000000, 1.000000000000000000),
 ( 0.9257577194822556033, 0.9980522942447415113),
 ( 0.9257577194822556033, 0.9980522942447415113),
 ( 1.000000000000000000, 1.000000000000000000) ) ) 
 REPRESENTATION_ITEM ( '' )  SURFACE ( )  );
#44647 = EDGE_LOOP ( 'NONE', ( #31112, #4264, #52350, #50679 ) ) ;
#44648 = DIRECTION ( 'NONE',  ( 0.000000000000000000, 0.01356324068817998940, -0.9999080150203990547 ) ) ;
#44649 = DIRECTION ( 'NONE',  ( -0.3939253465568944290, 0.8669868725995557579, 0.3052156353794350796 ) ) ;
#44650 = CARTESIAN_POINT ( 'NONE',  ( 1.020182472821379527, 12.22263240120502026, 2.608319446514492324 ) ) ;
#44651 = EDGE_CURVE ( 'NONE', #13952, #49136, #10368, .T. ) ;
#44652 = EDGE_CURVE ( 'NONE', #32109, #8260, #39944, .T. ) ;
#44653 = ORIENTED_EDGE ( 'NONE', *, *, #8556, .T. ) ;
#44654 = VECTOR ( 'NONE', #37761, 1000.000000000000114 ) ;
#44655 = AXIS2_PLACEMENT_3D ( 'NONE', #61573, #36309, #56616 ) ;
#44656 = VECTOR ( 'NONE', #55725, 1000.000000000000000 ) ;
#44657 = AXIS2_PLACEMENT_3D ( 'NONE', #1287, #47173, #62423 ) ;
#44658 = CARTESIAN_POINT ( 'NONE',  ( 30.66651853351974211, -3.164325622109354086, -24.36290982288815243 ) ) ;
#44659 = CIRCLE ( 'NONE', #27838, 12.18649999999999878 ) ;
#44660 = CARTESIAN_POINT ( 'NONE',  ( -10.90165637463000259, -7.712772661594503809, -11.08256590525389385 ) ) ;
#44661 = ORIENTED_EDGE ( 'NONE', *, *, #39239, .T. ) ;
#44662 = DIRECTION ( 'NONE',  ( -1.000000000000000000, 0.000000000000000000, 0.000000000000000000 ) ) ;
#44663 = DIRECTION ( 'NONE',  ( -1.000000000000000000, 0.000000000000000000, 0.000000000000000000 ) ) ;
#44664 = DIRECTION ( 'NONE',  ( 1.000000000000000000, -0.000000000000000000, 0.000000000000000000 ) ) ;
#44665 = AXIS2_PLACEMENT_3D ( 'NONE', #39246, #32936, #28301 ) ;
#44666 = LINE ( 'NONE', #10410, #47992 ) ;
#44667 = DIRECTION ( 'NONE',  ( 0.000000000000000000, 0.01356324068817991828, -0.9999080150203990547 ) ) ;
#44668 = AXIS2_PLACEMENT_3D ( 'NONE', #33926, #39902, #28953 ) ;
#44669 = ORIENTED_EDGE ( 'NONE', *, *, #64731, .F. ) ;
#44670 = CARTESIAN_POINT ( 'NONE',  ( 35.00000000000000000, 4.705694406421931860E-17, -3.469127814946512892E-15 ) ) ;
#44671 = CARTESIAN_POINT ( 'NONE',  ( -37.00000000000000711, 9.512294188641000403, -6.891188680298720115 ) ) ;
#44672 = CARTESIAN_POINT ( 'NONE',  ( 22.88594695219327235, -4.822122601967141264, 25.00000000000000000 ) ) ;
#44673 = VERTEX_POINT ( 'NONE', #49005 ) ;
#44674 = CARTESIAN_POINT ( 'NONE',  ( 8.555237949900300620, 3.417757171820648310, 13.06309840801727162 ) ) ;
#44675 = VECTOR ( 'NONE', #30387, 1000.000000000000000 ) ;
#44676 = DIRECTION ( 'NONE',  ( 1.000000000000000000, 0.000000000000000000, 0.000000000000000000 ) ) ;
#44677 = VERTEX_POINT ( 'NONE', #58987 ) ;
#44678 = EDGE_CURVE ( 'NONE', #21209, #5898, #36912, .T. ) ;
#44679 = VERTEX_POINT ( 'NONE', #33016 ) ;
#44680 = VERTEX_POINT ( 'NONE', #23065 ) ;
#44681 = CARTESIAN_POINT ( 'NONE',  ( -36.00000000000000711, 6.415447294506706477, 11.01837265713075631 ) ) ;
#44682 = ADVANCED_FACE ( 'NONE', ( #57991 ), #52983, .T. ) ;
#44683 = CIRCLE ( 'NONE', #35140, 5.000000000000001776 ) ;
#44684 = AXIS2_PLACEMENT_3D ( 'NONE', #17940, #16952, #7290 ) ;
#44685 = VERTEX_POINT ( 'NONE', #12732 ) ;
#44686 = CARTESIAN_POINT ( 'NONE',  ( 1.634816307076185193, -12.36483956257026939, -2.910502128620845674 ) ) ;
#44687 = CARTESIAN_POINT ( 'NONE',  ( -35.04834644901396956, 0.01211993185717642925, 0.006670072992069154237 ) ) ;
#44688 = CARTESIAN_POINT ( 'NONE',  ( -37.25000000000000711, -27.21021009056489603, 4.499999999999997335 ) ) ;
#44689 = LINE ( 'NONE', #39722, #30105 ) ;
#44690 = CIRCLE ( 'NONE', #21360, 5.000000000000000888 ) ;
#44691 = CARTESIAN_POINT ( 'NONE',  ( 0.3474126878361846749, -10.75620725594711580, -5.911350916722150295 ) ) ;
#44692 = CARTESIAN_POINT ( 'NONE',  ( 2.241526690369556096, 0.01730530154276703134, 7.634439869182785721 ) ) ;
#44694 = ORIENTED_EDGE ( 'NONE', *, *, #2841, .T. ) ;
#44693 = LINE ( 'NONE', #54040, #28721 ) ;
#44695 = CARTESIAN_POINT ( 'NONE',  ( 5.514970785353741078, -0.004694330894494715307, -0.0005190732562554894796 ) ) ;
#44696 = VERTEX_POINT ( 'NONE', #37697 ) ;
#44697 = CARTESIAN_POINT ( 'NONE',  ( -35.00000000000000000, 12.18632975068353019, 0.06441628369840693424 ) ) ;
#44698 = ORIENTED_EDGE ( 'NONE', *, *, #8039, .T. ) ;
#44699 = ORIENTED_EDGE ( 'NONE', *, *, #5818, .F. ) ;
#44700 = CARTESIAN_POINT ( 'NONE',  ( -22.28694879868232803, -0.9088670759107992936, 3.597828382597537011 ) ) ;
#44701 = VECTOR ( 'NONE', #885, 1000.000000000000000 ) ;
#44702 = CARTESIAN_POINT ( 'NONE',  ( -0.4406170177989196524, -30.53628804997674706, 15.30998899416534975 ) ) ;
#44703 = CARTESIAN_POINT ( 'NONE',  ( -35.04683013664716640, 0.009445816769477739447, 0.007968230201761825754 ) ) ;
#44704 = CIRCLE ( 'NONE', #12815, 12.74999999999999822 ) ;
#44705 = EDGE_CURVE ( 'NONE', #12978, #8671, #17749, .T. ) ;
#44706 = CARTESIAN_POINT ( 'NONE',  ( 24.07863249974178999, 1.047192704403120844, 11.95862630624809420 ) ) ;
#44707 = CARTESIAN_POINT ( 'NONE',  ( 5.536195898058073439, -0.001726268814999567603, -0.008323005098841091201 ) ) ;
#44708 = CARTESIAN_POINT ( 'NONE',  ( 2.000000000000001776, 6.643843315911800218, 1.507714007300793968 ) ) ;
#44710 = EDGE_LOOP ( 'NONE', ( #64324, #46212, #8048, #64822 ) ) ;
#44709 = VECTOR ( 'NONE', #28983, 1000.000000000000000 ) ;
#44711 = CIRCLE ( 'NONE', #29855, 5.000000000000000000 ) ;
#44712 = EDGE_CURVE ( 'NONE', #43321, #44959, #64576, .T. ) ;
#44713 = ORIENTED_EDGE ( 'NONE', *, *, #64861, .T. ) ;
#44714 = EDGE_CURVE ( 'NONE', #27543, #3865, #64545, .T. ) ;
#44715 = DIRECTION ( 'NONE',  ( 0.000000000000000000, 0.000000000000000000, 1.000000000000000000 ) ) ;
#44716 = VERTEX_POINT ( 'NONE', #2804 ) ;
#44717 = AXIS2_PLACEMENT_3D ( 'NONE', #34069, #29731, #64333 ) ;
#44718 = ADVANCED_FACE ( 'NONE', ( #33365 ), #63598, .T. ) ;
#44719 = EDGE_LOOP ( 'NONE', ( #20327, #25085, #30626, #62936 ) ) ;
#44720 = CIRCLE ( 'NONE', #56408, 6.936499999999990784 ) ;
#44721 = CARTESIAN_POINT ( 'NONE',  ( 2.251152103363646351, -7.498874008626767562, 1.449454666117707236 ) ) ;
#44722 = LINE ( 'NONE', #32381, #57440 ) ;
#44723 = CARTESIAN_POINT ( 'NONE',  ( -4.806344283790351390, -7.508992741355383416, 25.00000000000000000 ) ) ;
#44724 = CARTESIAN_POINT ( 'NONE',  ( 2.255723233588951882, 7.638048593862505342, 0.1321982600347512971 ) ) ;
#44725 = DIRECTION ( 'NONE',  ( 1.000000000000000000, -0.000000000000000000, 0.000000000000000000 ) ) ;
#44726 = EDGE_CURVE ( 'NONE', #43974, #49728, #18886, .T. ) ;
#44727 = CARTESIAN_POINT ( 'NONE',  ( 2.406456491625821759, 1.188938370543313860, -10.36527681096184672 ) ) ;
#44728 = AXIS2_PLACEMENT_3D ( 'NONE', #40557, #35873, #45227 ) ;
#44729 = VERTEX_POINT ( 'NONE', #8753 ) ;
#44730 = ADVANCED_FACE ( 'NONE', ( #12402 ), #3461, .T. ) ;
#44731 = ORIENTED_EDGE ( 'NONE', *, *, #59298, .F. ) ;
#44732 = CONICAL_SURFACE ( 'NONE', #16064, 7.580821595991582562, 0.3217505529694035249 ) ;
#44733 = CARTESIAN_POINT ( 'NONE',  ( -22.31328051695926007, -3.148362328073157190, 2.109671368890621679 ) ) ;
#44734 = FACE_OUTER_BOUND ( 'NONE', #12918, .T. ) ;
#44735 = CARTESIAN_POINT ( 'NONE',  ( 2.000000000000001776, 0.000000000000000000, 0.000000000000000000 ) ) ;
#44736 = AXIS2_PLACEMENT_3D ( 'NONE', #65450, #40178, #33892 ) ;
#44737 = AXIS2_PLACEMENT_3D ( 'NONE', #16781, #22425, #42047 ) ;
#44738 = DIRECTION ( 'NONE',  ( 0.000000000000000000, -0.01356324068817991828, 0.9999080150203990547 ) ) ;
#44739 = CIRCLE ( 'NONE', #6502, 12.75000000000000178 ) ;
#44740 = DIRECTION ( 'NONE',  ( 0.000000000000000000, -0.6943713148249690548, 0.7196168960969742123 ) ) ;
#44741 = EDGE_CURVE ( 'NONE', #2944, #57171, #13547, .T. ) ;
#44742 = CARTESIAN_POINT ( 'NONE',  ( 6.406045832739715173, -9.118602296057780165, -9.956832946668152218 ) ) ;
#44743 = DIRECTION ( 'NONE',  ( -1.000000000000000000, 0.000000000000000000, -0.000000000000000000 ) ) ;
#44744 = B_SPLINE_CURVE_WITH_KNOTS ( 'NONE', 3,
 ( #41151, #25543, #45491, #51505, #64231, #15875, #5953, #19905, #60802, #15239, #51165, #65441 ),
 .UNSPECIFIED., .F., .F.,
 ( 4, 2, 2, 2, 2, 4 ),
 ( 0.005924275648040054458, 0.006464403524968336673, 0.007004531401896618888, 0.008084787155753182450, 0.009165042909609746880, 0.01024529866346631131 ),
 .UNSPECIFIED. ) ;
#44745 = DIRECTION ( 'NONE',  ( 0.000000000000000000, 0.7617968321374901652, 0.6478160128811921714 ) ) ;
#44746 = CARTESIAN_POINT ( 'NONE',  ( -37.00000000000000711, 11.81949347079751256, -2.968224442958276921 ) ) ;
#44747 = ORIENTED_EDGE ( 'NONE', *, *, #43239, .F. ) ;
#44748 = CARTESIAN_POINT ( 'NONE',  ( 0.2650492433740059273, 12.07870441534856631, 2.017984765249114076 ) ) ;
#44749 = DIRECTION ( 'NONE',  ( 0.000000000000000000, -0.01356324068817998593, 0.9999080150203990547 ) ) ;
#44750 = DIRECTION ( 'NONE',  ( 1.000000000000000000, 0.000000000000000000, 0.000000000000000000 ) ) ;
#44751 = VECTOR ( 'NONE', #8172, 1000.000000000000000 ) ;
#44752 = AXIS2_PLACEMENT_3D ( 'NONE', #21035, #41314, #27338 ) ;
#44753 = CIRCLE ( 'NONE', #46914, 12.18650000000000055 ) ;
#44754 = LINE ( 'NONE', #30761, #17126 ) ;
#44755 = CARTESIAN_POINT ( 'NONE',  ( 2.284126774967659923, -5.959830409747688407, 4.793997684221343647 ) ) ;
#44756 = ORIENTED_EDGE ( 'NONE', *, *, #53382, .F. ) ;
#44757 = CARTESIAN_POINT ( 'NONE',  ( 0.2646305136544072623, -7.770320294339239098, 9.465888453932937097 ) ) ;
#44758 = CARTESIAN_POINT ( 'NONE',  ( -35.00000000000000000, -12.08216339958899788, -1.591260454995368390 ) ) ;
#44759 = AXIS2_PLACEMENT_3D ( 'NONE', #52007, #26731, #57663 ) ;
#44760 = CARTESIAN_POINT ( 'NONE',  ( 5.268658153349320195, -26.03085267760928545, -15.19911252589913886 ) ) ;
#44761 = EDGE_LOOP ( 'NONE', ( #35193, #29420, #24640, #26299 ) ) ;
#44762 = DIRECTION ( 'NONE',  ( -1.000000000000000000, 0.000000000000000000, 0.000000000000000000 ) ) ;
#44763 = CARTESIAN_POINT ( 'NONE',  ( -28.14392221313259057, -12.90664841586573530, -3.969767364051066227 ) ) ;
#44764 = CARTESIAN_POINT ( 'NONE',  ( -22.28415773361649954, -0.9981933716384904232, -3.565377603762390546 ) ) ;
#44765 = DIRECTION ( 'NONE',  ( 0.000000000000000000, 0.01356324068817992175, -0.9999080150203990547 ) ) ;
#44766 = CARTESIAN_POINT ( 'NONE',  ( 2.080613030138688480, 4.898587196589412829E-16, -4.000000000000000000 ) ) ;
#44767 = EDGE_CURVE ( 'NONE', #46970, #9266, #19353, .T. ) ;
#44768 = B_SPLINE_CURVE_WITH_KNOTS ( 'NONE', 3,
 ( #33440, #13784, #58736, #28127, #28768, #2874, #8166, #49418, #14122, #53405, #18147, #7853, #48741, #33100, #48422, #34417, #27789, #23458, #49084, #38421, #44374, #39394, #38083, #43074, #28437, #19122, #8485, #22818 ),
 .UNSPECIFIED., .F., .F.,
 ( 4, 2, 2, 2, 2, 2, 2, 2, 2, 2, 2, 2, 2, 4 ),
 ( 0.000000000000000000, 0.001016716753235190340, 0.002033433506470380681, 0.003050150259705570587, 0.003558508636323166625, 0.004066867012940762229, 0.004575225389558358266, 0.005083583766175953436, 0.005591942142793548606, 0.006100300519411143776, 0.006608658896028738947, 0.007117017272646334117, 0.007625375649263929287, 0.008133734025881524457 ),
 .UNSPECIFIED. ) ;
#44769 = CARTESIAN_POINT ( 'NONE',  ( -37.00000000000000711, -11.59095880812009582, 1.903127969211145132 ) ) ;
#44770 = ORIENTED_EDGE ( 'NONE', *, *, #33030, .F. ) ;
#44771 = CARTESIAN_POINT ( 'NONE',  ( 2.251139882113957658, -7.218573619021352528, 2.495216312514858981 ) ) ;
#44772 = CARTESIAN_POINT ( 'NONE',  ( -8.901467632063809532, 10.71271741810010170, -8.221947568083972868 ) ) ;
#44773 = CARTESIAN_POINT ( 'NONE',  ( -35.00000000000000000, 0.000000000000000000, 0.000000000000000000 ) ) ;
#44774 = DIRECTION ( 'NONE',  ( -1.000000000000000000, -0.000000000000000000, 0.000000000000000000 ) ) ;
#44775 = EDGE_CURVE ( 'NONE', #59375, #63362, #45400, .T. ) ;
#44776 = DIRECTION ( 'NONE',  ( -1.000000000000000000, 0.000000000000000000, 0.000000000000000000 ) ) ;
#44777 = CARTESIAN_POINT ( 'NONE',  ( -22.66110217412718342, 4.900671186447937089, 0.6585288088159688691 ) ) ;
#44778 = CARTESIAN_POINT ( 'NONE',  ( 0.3675815128205894289, 5.910255304480445560, 10.76447900494942367 ) ) ;
#44779 = CARTESIAN_POINT ( 'NONE',  ( 2.260457164925433027, 1.190240296004817511, -7.547495527592634090 ) ) ;
#44780 = VERTEX_POINT ( 'NONE', #29034 ) ;
#44781 = AXIS2_PLACEMENT_3D ( 'NONE', #12236, #27520, #47817 ) ;
#44782 = ORIENTED_EDGE ( 'NONE', *, *, #50598, .T. ) ;
#44783 = CARTESIAN_POINT ( 'NONE',  ( -17.97425243782675253, -5.939124358307740437, -10.42822101977554361 ) ) ;
#44784 = VERTEX_POINT ( 'NONE', #9069 ) ;
#44786 = CARTESIAN_POINT ( 'NONE',  ( 37.00000000000000711, 9.063649021438955344, -8.146229107149434157 ) ) ;
#44785 = CIRCLE ( 'NONE', #60749, 12.74999999999999822 ) ;
#44787 = VECTOR ( 'NONE', #50561, 1000.000000000000000 ) ;
#44788 = VECTOR ( 'NONE', #13367, 1000.000000000000000 ) ;
#44789 = EDGE_CURVE ( 'NONE', #20190, #61052, #19721, .T. ) ;
#44790 = CARTESIAN_POINT ( 'NONE',  ( -21.24030193723618609, 25.00000000000000000, -5.230344621181295395 ) ) ;
#44791 = ORIENTED_EDGE ( 'NONE', *, *, #47699, .T. ) ;
#44792 = DIRECTION ( 'NONE',  ( 0.000000000000000000, -0.01356324068817992175, 0.9999080150203990547 ) ) ;
#44793 = CARTESIAN_POINT ( 'NONE',  ( 12.90485164427657239, 10.90052374342006303, -5.021923595418537722 ) ) ;
#44794 = ADVANCED_FACE ( 'NONE', ( #24353 ), #39975, .T. ) ;
#44795 = CARTESIAN_POINT ( 'NONE',  ( 22.88594695219327235, -4.822122601967141264, 12.60940655271284427 ) ) ;
#44796 = ORIENTED_EDGE ( 'NONE', *, *, #6531, .T. ) ;
#44797 = ORIENTED_EDGE ( 'NONE', *, *, #37438, .F. ) ;
#44798 = DIRECTION ( 'NONE',  ( -0.000000000000000000, -1.000000000000000000, -0.000000000000000000 ) ) ;
#44799 = EDGE_CURVE ( 'NONE', #30305, #53784, #12982, .T. ) ;
#44800 = DIRECTION ( 'NONE',  ( 1.000000000000000000, -0.000000000000000000, -0.000000000000000000 ) ) ;
#44801 = EDGE_LOOP ( 'NONE', ( #37873, #43994, #41689, #12395 ) ) ;
#44802 = CARTESIAN_POINT ( 'NONE',  ( 0.3675815128205894289, 2.391755495700603973, 12.04510820461660003 ) ) ;
#44803 = ORIENTED_EDGE ( 'NONE', *, *, #22438, .T. ) ;
#44804 = AXIS2_PLACEMENT_3D ( 'NONE', #44854, #49225, #50190 ) ;
#44805 = CARTESIAN_POINT ( 'NONE',  ( 0.000000000000000000, 6.160607635185464837, -4.277489166005534749 ) ) ;
#44806 = FACE_OUTER_BOUND ( 'NONE', #57501, .T. ) ;
#44807 = VECTOR ( 'NONE', #60147, 1000.000000000000000 ) ;
#44808 = DIRECTION ( 'NONE',  ( 1.000000000000000000, -0.000000000000000000, -0.000000000000000000 ) ) ;
#44809 = DIRECTION ( 'NONE',  ( 1.000000000000000000, 0.000000000000000000, 0.000000000000000000 ) ) ;
#44810 = VECTOR ( 'NONE', #56644, 1000.000000000000000 ) ;
#44811 = CARTESIAN_POINT ( 'NONE',  ( -35.00000000000000000, 5.636262487437317503, 10.80478261802183937 ) ) ;
#44812 = ORIENTED_EDGE ( 'NONE', *, *, #36296, .T. ) ;
#44813 = CARTESIAN_POINT ( 'NONE',  ( 2.257661810676419467, 7.638648121130928281, -0.1348365785571233599 ) ) ;
#44814 = ADVANCED_FACE ( 'NONE', ( #39654 ), #9373, .F. ) ;
#44815 = DIRECTION ( 'NONE',  ( 0.000000000000000000, 0.9551603052523468529, -0.2960891610144544828 ) ) ;
#44816 = VECTOR ( 'NONE', #45294, 1000.000000000000000 ) ;
#44817 = DIRECTION ( 'NONE',  ( 0.000000000000000000, -0.9999080150203990547, -0.01356324068816951688 ) ) ;
#44818 = ADVANCED_FACE ( 'NONE', ( #60260 ), #4085, .T. ) ;
#44819 = CARTESIAN_POINT ( 'NONE',  ( 35.00000000000000000, 4.705694406421931860E-17, -3.469127814946512892E-15 ) ) ;
#44820 = CARTESIAN_POINT ( 'NONE',  ( 11.74548640120467979, 10.73597826697114677, -8.184666801472349817 ) ) ;
#44821 = CARTESIAN_POINT ( 'NONE',  ( 24.35372750138188991, -1.446416020193747931, 13.42696394628527479 ) ) ;
#44822 = DIRECTION ( 'NONE',  ( -1.000000000000000000, -0.000000000000000000, 0.000000000000000000 ) ) ;
#44823 = DIRECTION ( 'NONE',  ( 0.000000000000000000, 0.000000000000000000, -1.000000000000000000 ) ) ;
#44824 = B_SPLINE_CURVE_WITH_KNOTS ( 'NONE', 3,
 ( #49508, #39169, #50485, #55120, #59461, #54490, #19880 ),
 .UNSPECIFIED., .F., .F.,
 ( 4, 3, 4 ),
 ( 0.000000000000000000, 0.001700533616330542541, 0.005002426799371243599 ),
 .UNSPECIFIED. ) ;
#44825 = CARTESIAN_POINT ( 'NONE',  ( 0.3278977287071236923, 9.235688435081733871, 8.073566434006613335 ) ) ;
#44826 = EDGE_CURVE ( 'NONE', #1597, #62432, #22049, .T. ) ;
#44827 = VERTEX_POINT ( 'NONE', #25025 ) ;
#44828 = CARTESIAN_POINT ( 'NONE',  ( 0.3223008802179229693, 0.2444878876723223515, 12.26274332232494224 ) ) ;
#44829 = EDGE_CURVE ( 'NONE', #61242, #11917, #12498, .T. ) ;
#44830 = AXIS2_PLACEMENT_3D ( 'NONE', #1588, #31803, #7528 ) ;
#44831 = ORIENTED_EDGE ( 'NONE', *, *, #40900, .F. ) ;
#44832 = CARTESIAN_POINT ( 'NONE',  ( -3.433867940172757649, -8.302961779614593141, 8.673267303339269318 ) ) ;
#44833 = CARTESIAN_POINT ( 'NONE',  ( 2.298277635560282750, -7.506689984432316720, -1.491234112749268759 ) ) ;
#44834 = DIRECTION ( 'NONE',  ( 0.000000000000000000, 0.01356324068817998940, -0.9999080150203989437 ) ) ;
#44835 = EDGE_CURVE ( 'NONE', #63621, #13407, #64526, .T. ) ;
#44836 = DIRECTION ( 'NONE',  ( -1.000000000000000000, 0.000000000000000000, 0.000000000000000000 ) ) ;
#44837 = CARTESIAN_POINT ( 'NONE',  ( 0.3040950598368152291, -4.428852722102656791, -11.43390362554257322 ) ) ;
#44838 = VERTEX_POINT ( 'NONE', #55270 ) ;
#44839 = CARTESIAN_POINT ( 'NONE',  ( 35.00000000000000000, 4.705694406421931860E-17, -3.469127814946512892E-15 ) ) ;
#44840 = DIRECTION ( 'NONE',  ( -1.000000000000000000, 0.000000000000000000, 0.000000000000000000 ) ) ;
#44841 = VECTOR ( 'NONE', #14358, 1000.000000000000000 ) ;
#44842 = DIRECTION ( 'NONE',  ( 0.000000000000000000, 0.01356324068818000848, -0.9999080150203990547 ) ) ;
#44843 = CARTESIAN_POINT ( 'NONE',  ( 15.82795513634483875, -34.24358411257726686, -7.361295665690556156 ) ) ;
#44844 = VECTOR ( 'NONE', #44840, 1000.000000000000000 ) ;
#44845 = AXIS2_PLACEMENT_3D ( 'NONE', #25522, #10546, #50803 ) ;
#44846 = CARTESIAN_POINT ( 'NONE',  ( -35.00000000000000000, 0.4353888892048373149, 11.73808581813438323 ) ) ;
#44847 =( BOUNDED_CURVE ( )  B_SPLINE_CURVE ( 3, ( #8781, #8127, #28395, #43350 ),
 .UNSPECIFIED., .F., .F. ) 
 B_SPLINE_CURVE_WITH_KNOTS ( ( 4, 4 ),
 ( 5.064515163936929909, 5.083794169102955784 ),
 .UNSPECIFIED. ) 
 CURVE ( )  GEOMETRIC_REPRESENTATION_ITEM ( )  RATIONAL_B_SPLINE_CURVE ( ( 1.000000000000000000, 0.9999690269031535905, 0.9999690269031535905, 1.000000000000000000 ) ) 
 REPRESENTATION_ITEM ( '' )  );
#44848 = VERTEX_POINT ( 'NONE', #45298 ) ;
#44849 = CARTESIAN_POINT ( 'NONE',  ( 2.000000000000001776, 2.473437528934141483, 7.080403010454977775 ) ) ;
#44850 = B_SPLINE_CURVE_WITH_KNOTS ( 'NONE', 3,
 ( #59115, #59416, #49469, #24166, #34772, #30144, #28834, #19179, #50109, #55413, #43802, #3601, #29471, #39452, #59754, #13839 ),
 .UNSPECIFIED., .F., .F.,
 ( 4, 2, 2, 2, 2, 2, 2, 4 ),
 ( 0.000000000000000000, 0.001179563962946403180, 0.001769345944419603144, 0.002359127925892802891, 0.003538691888839202819, 0.004718255851785603180, 0.007077383777678405638, 0.009436511703571208096 ),
 .UNSPECIFIED. ) ;
#44851 = ORIENTED_EDGE ( 'NONE', *, *, #20493, .F. ) ;
#44852 = CARTESIAN_POINT ( 'NONE',  ( 0.2648978790185602672, 12.24533305150758089, -0.1321385342562831633 ) ) ;
#44853 = CARTESIAN_POINT ( 'NONE',  ( 35.00000000000000000, -1.113475361586580226, -12.70128625845192438 ) ) ;
#44854 = CARTESIAN_POINT ( 'NONE',  ( 0.000000000000000000, -5.450255447309714896, -4.087611905901492371 ) ) ;
#44855 = AXIS2_PLACEMENT_3D ( 'NONE', #31142, #24850, #56407 ) ;
#44856 = DIRECTION ( 'NONE',  ( 0.000000000000000000, 0.000000000000000000, -1.000000000000000000 ) ) ;
#44857 = ADVANCED_FACE ( 'NONE', ( #5075 ), #19049, .T. ) ;
#44858 = ORIENTED_EDGE ( 'NONE', *, *, #43095, .T. ) ;
#44859 = ORIENTED_EDGE ( 'NONE', *, *, #54760, .F. ) ;
#44860 = DIRECTION ( 'NONE',  ( 1.000000000000000000, -0.000000000000000000, 0.000000000000000000 ) ) ;
#44861 = VERTEX_POINT ( 'NONE', #40292 ) ;
#44862 = CARTESIAN_POINT ( 'NONE',  ( 12.47628546223243617, 0.000000000000000000, -13.50000000000000178 ) ) ;
#44863 = CARTESIAN_POINT ( 'NONE',  ( 35.00000000000000000, -11.13736569743270621, 4.946702696913284569 ) ) ;
#44864 = CARTESIAN_POINT ( 'NONE',  ( 2.276198483118645921, 6.543270001966289939, 3.955655305431081015 ) ) ;
#44865 = CARTESIAN_POINT ( 'NONE',  ( -37.00000000000000711, 0.000000000000000000, 0.000000000000000000 ) ) ;
#44866 = CARTESIAN_POINT ( 'NONE',  ( 2.556980015514263460, 6.584367695372324469, -4.067895092073666952 ) ) ;
#44867 = CARTESIAN_POINT ( 'NONE',  ( 36.00000000000000711, 12.38385022362086119, 3.033604067594442899 ) ) ;
#44868 = FACE_OUTER_BOUND ( 'NONE', #29730, .T. ) ;
#44869 = VERTEX_POINT ( 'NONE', #10054 ) ;
#44870 = EDGE_CURVE ( 'NONE', #57900, #6726, #30336, .T. ) ;
#44871 = ORIENTED_EDGE ( 'NONE', *, *, #17547, .T. ) ;
#44872 = VERTEX_POINT ( 'NONE', #45614 ) ;
#44873 = CARTESIAN_POINT ( 'NONE',  ( 0.09505445835107226293, -0.1369421331495649097, 13.50000000000000355 ) ) ;
#44874 = DIRECTION ( 'NONE',  ( 0.000000000000000000, 0.7381862504171974315, -0.6745969609292639113 ) ) ;
#44875 = EDGE_CURVE ( 'NONE', #5276, #63698, #36767, .T. ) ;
#44876 = ORIENTED_EDGE ( 'NONE', *, *, #50067, .T. ) ;
#44877 = B_SPLINE_CURVE_WITH_KNOTS ( 'NONE', 3,
 ( #12186, #27473, #11215, #1583, #7192, #36480, #1246, #904, #41791, #5926, #51479, #52765, #47773, #62085, #42102, #56793, #57102, #20856, #41124 ),
 .UNSPECIFIED., .F., .F.,
 ( 4, 3, 3, 3, 3, 3, 4 ),
 ( 0.000000000000000000, 2.831840207499747818E-05, 4.217266859840622183E-05, 5.602024318396007954E-05, 6.290810167969113043E-05, 9.120440630945109367E-05, 0.0001153103026479756967 ),
 .UNSPECIFIED. ) ;
#44878 = CIRCLE ( 'NONE', #16214, 4.999999999999999112 ) ;
#44879 = FACE_BOUND ( 'NONE', #49171, .T. ) ;
#44880 = ORIENTED_EDGE ( 'NONE', *, *, #43009, .T. ) ;
#44881 = LINE ( 'NONE', #49880, #44978 ) ;
#44882 = CARTESIAN_POINT ( 'NONE',  ( 0.3665391374699465965, 10.50279796150445755, -6.368473106897019065 ) ) ;
#44883 = CARTESIAN_POINT ( 'NONE',  ( 0.000000000000000000, -33.00000000000000000, 0.000000000000000000 ) ) ;
#44884 = CARTESIAN_POINT ( 'NONE',  ( 3.092491956585503132, 7.275786042219460015, -3.124176487320081019 ) ) ;
#44885 = ORIENTED_EDGE ( 'NONE', *, *, #60542, .F. ) ;
#44886 = ORIENTED_EDGE ( 'NONE', *, *, #9458, .F. ) ;
#44887 = CARTESIAN_POINT ( 'NONE',  ( 3.100650473569750876, -7.074394303868237976, 3.562766772868519727 ) ) ;
#44888 = ADVANCED_FACE ( 'NONE', ( #3006 ), #49539, .T. ) ;
#44889 = ORIENTED_EDGE ( 'NONE', *, *, #49272, .T. ) ;
#44890 = CARTESIAN_POINT ( 'NONE',  ( -36.00000000000000711, -11.90598845858530730, -4.561791185930541559 ) ) ;
#44891 = EDGE_LOOP ( 'NONE', ( #2814, #1432, #24111, #18096 ) ) ;
#44892 = AXIS2_PLACEMENT_3D ( 'NONE', #6429, #36993, #57299 ) ;
#44893 = CIRCLE ( 'NONE', #12998, 7.938172270156617749 ) ;
#44894 = VERTEX_POINT ( 'NONE', #28263 ) ;
#44895 = ORIENTED_EDGE ( 'NONE', *, *, #19514, .F. ) ;
#44896 = CYLINDRICAL_SURFACE ( 'NONE', #56364, 5.000000000000000000 ) ;
#44897 = CARTESIAN_POINT ( 'NONE',  ( 2.000000000000001776, 5.769711778877324448, 4.791703871138532023 ) ) ;
#44898 = AXIS2_PLACEMENT_3D ( 'NONE', #49939, #43970, #19361 ) ;
#44899 = CARTESIAN_POINT ( 'NONE',  ( -35.00000000000000000, 7.718225330433806874, 9.430788938294076829 ) ) ;
#44900 = DIRECTION ( 'NONE',  ( 0.000000000000000000, -0.01356324068817991828, 0.9999080150203990547 ) ) ;
#44901 = VERTEX_POINT ( 'NONE', #44200 ) ;
#44902 = DIRECTION ( 'NONE',  ( -1.000000000000000000, -0.000000000000000000, 0.000000000000000000 ) ) ;
#44903 = ORIENTED_EDGE ( 'NONE', *, *, #40785, .F. ) ;
#44904 = DIRECTION ( 'NONE',  ( 0.000000000000000000, 0.6943713148249639477, -0.7196168960969794304 ) ) ;
#44905 = CARTESIAN_POINT ( 'NONE',  ( -37.00000000000000711, -8.295159312811792418, -8.927548052240984688 ) ) ;
#44906 = ORIENTED_EDGE ( 'NONE', *, *, #63377, .T. ) ;
#44907 = CARTESIAN_POINT ( 'NONE',  ( 0.8375941296816566961, 9.769835228044911446, -7.696026447556128858 ) ) ;
#44908 = FACE_OUTER_BOUND ( 'NONE', #49624, .T. ) ;
#44909 = DIRECTION ( 'NONE',  ( -0.7648446667472313942, 0.000000000000000000, 0.6442147435043042991 ) ) ;
#44910 = EDGE_CURVE ( 'NONE', #53880, #42172, #49685, .T. ) ;
#44911 = EDGE_LOOP ( 'NONE', ( #15646, #32680, #31525, #7453 ) ) ;
#44912 = CIRCLE ( 'NONE', #42760, 12.18649999999999878 ) ;
#44913 = ORIENTED_EDGE ( 'NONE', *, *, #22422, .T. ) ;
#44914 = CARTESIAN_POINT ( 'NONE',  ( 1.719304012338439325, 7.017415949612858306, 10.62216384465677521 ) ) ;
#44915 = EDGE_CURVE ( 'NONE', #59, #3146, #30536, .T. ) ;
#44916 = ORIENTED_EDGE ( 'NONE', *, *, #64686, .T. ) ;
#44917 = CARTESIAN_POINT ( 'NONE',  ( 0.2648978790185593790, 10.67083876753491900, 6.008231198269021078 ) ) ;
#44918 = CARTESIAN_POINT ( 'NONE',  ( 37.00000000000000711, 4.705694406421931860E-17, -3.469127814946512892E-15 ) ) ;
#44919 = CIRCLE ( 'NONE', #40649, 6.936499999999989008 ) ;
#44920 = CARTESIAN_POINT ( 'NONE',  ( 3.527934398658590709, -26.69696348912970763, 16.00979375678724281 ) ) ;
#44921 = EDGE_CURVE ( 'NONE', #13767, #28521, #22957, .T. ) ;
#44922 = LINE ( 'NONE', #61201, #11772 ) ;
#44923 = CARTESIAN_POINT ( 'NONE',  ( 13.40637569210417368, 10.89743038486300719, -5.029693541956189229 ) ) ;
#44924 = ORIENTED_EDGE ( 'NONE', *, *, #8539, .T. ) ;
#44925 = CARTESIAN_POINT ( 'NONE',  ( -37.00000000000000711, 0.000000000000000000, 0.000000000000000000 ) ) ;
#44926 = CARTESIAN_POINT ( 'NONE',  ( 1.719304012341537957, 12.20344780066137602, -3.626341562669237906 ) ) ;
#44927 = DIRECTION ( 'NONE',  ( -1.000000000000000000, 0.000000000000000000, 0.000000000000000000 ) ) ;
#44928 = AXIS2_PLACEMENT_3D ( 'NONE', #60057, #20139, #50421 ) ;
#44929 = CARTESIAN_POINT ( 'NONE',  ( -0.5028117989624658613, -26.55343892596427224, -16.22424428316958611 ) ) ;
#44930 = CARTESIAN_POINT ( 'NONE',  ( 37.00000000000000711, 4.705694406421931860E-17, -3.469127814946512892E-15 ) ) ;
#44931 = CARTESIAN_POINT ( 'NONE',  ( 2.251152103363643242, -5.930529991878042750, -4.812779263775083471 ) ) ;
#44932 = CARTESIAN_POINT ( 'NONE',  ( 3.152665057736256493, -0.9030954876717440793, 7.886634106564762270 ) ) ;
#44933 = LINE ( 'NONE', #19351, #29000 ) ;
#44934 = CIRCLE ( 'NONE', #43849, 2.899999999999994582 ) ;
#44935 = AXIS2_PLACEMENT_3D ( 'NONE', #30477, #20836, #61386 ) ;
#44936 = CIRCLE ( 'NONE', #16280, 5.000000000000001776 ) ;
#44937 = AXIS2_PLACEMENT_3D ( 'NONE', #27207, #47500, #57817 ) ;
#44938 = EDGE_CURVE ( 'NONE', #61338, #95, #33720, .T. ) ;
#44939 = ORIENTED_EDGE ( 'NONE', *, *, #24942, .F. ) ;
#44940 = DIRECTION ( 'NONE',  ( -1.000000000000000000, 0.000000000000000000, 0.000000000000000000 ) ) ;
#44941 = ADVANCED_FACE ( 'NONE', ( #7997 ), #65604, .F. ) ;
#44942 = VERTEX_POINT ( 'NONE', #38562 ) ;
#44943 = CARTESIAN_POINT ( 'NONE',  ( 35.00000000000000000, 11.72195762423409704, 0.7536123767498881243 ) ) ;
#44944 = CARTESIAN_POINT ( 'NONE',  ( -22.27711653538342773, -3.657713416444755783, 0.4190680140413455823 ) ) ;
#44945 = CARTESIAN_POINT ( 'NONE',  ( 0.2648978790185584908, 6.008231198268983775, 10.67083876753494032 ) ) ;
#44946 = VECTOR ( 'NONE', #13994, 1000.000000000000000 ) ;
#44947 = CARTESIAN_POINT ( 'NONE',  ( -37.00000000000000711, 0.000000000000000000, 0.000000000000000000 ) ) ;
#44948 = ORIENTED_EDGE ( 'NONE', *, *, #36006, .T. ) ;
#44949 = AXIS2_PLACEMENT_3D ( 'NONE', #5271, #10908, #60799 ) ;
#44950 = EDGE_CURVE ( 'NONE', #7261, #11247, #1042, .T. ) ;
#44951 = EDGE_LOOP ( 'NONE', ( #13460, #3844, #8071, #18230 ) ) ;
#44952 = ORIENTED_EDGE ( 'NONE', *, *, #61557, .F. ) ;
#44953 = CARTESIAN_POINT ( 'NONE',  ( 29.39893672795668778, -9.588109978674381750, 7.219804916327976052 ) ) ;
#44954 = DIRECTION ( 'NONE',  ( -1.000000000000000000, 0.000000000000000000, 0.000000000000000000 ) ) ;
#44955 = EDGE_LOOP ( 'NONE', ( #26314, #28515, #20496, #29708 ) ) ;
#44956 = CARTESIAN_POINT ( 'NONE',  ( 35.00000000000000000, -3.916263239775270577, 11.07407352312216453 ) ) ;
#44957 = DIRECTION ( 'NONE',  ( 0.000000000000000000, -0.01356324068818000328, 0.9999080150203990547 ) ) ;
#44958 = LINE ( 'NONE', #24341, #46073 ) ;
#44959 = VERTEX_POINT ( 'NONE', #13923 ) ;
#44960 = AXIS2_PLACEMENT_3D ( 'NONE', #26078, #62945, #36367 ) ;
#44961 = DIRECTION ( 'NONE',  ( 1.000000000000000000, -0.000000000000000000, 0.000000000000000000 ) ) ;
#44962 = VECTOR ( 'NONE', #13884, 1000.000000000000114 ) ;
#44963 = CARTESIAN_POINT ( 'NONE',  ( -2.287538219536363382, -28.18941229671508708, -13.77533426008797335 ) ) ;
#44964 = DIRECTION ( 'NONE',  ( 0.000000000000000000, 0.1118654143051546757, 0.9937233664769770103 ) ) ;
#44966 = ORIENTED_EDGE ( 'NONE', *, *, #6269, .T. ) ;
#44965 = CARTESIAN_POINT ( 'NONE',  ( 0.000000000000000000, -7.414200355365233364, -1.131208685655244350 ) ) ;
#44967 = FACE_OUTER_BOUND ( 'NONE', #47905, .T. ) ;
#44968 = EDGE_CURVE ( 'NONE', #48281, #22893, #32688, .T. ) ;
#44969 = EDGE_CURVE ( 'NONE', #32172, #20267, #223, .T. ) ;
#44970 = ORIENTED_EDGE ( 'NONE', *, *, #36785, .F. ) ;
#44971 = CARTESIAN_POINT ( 'NONE',  ( 0.5572780756284869685, -9.649189244958623846, 7.697784780878684785 ) ) ;
#44972 = ORIENTED_EDGE ( 'NONE', *, *, #7345, .T. ) ;
#44973 = DIRECTION ( 'NONE',  ( -0.6845106172691086677, 0.000000000000000000, -0.7290028908350527637 ) ) ;
#44974 = DIRECTION ( 'NONE',  ( -1.000000000000000000, 0.000000000000000000, -0.000000000000000000 ) ) ;
#44975 = EDGE_CURVE ( 'NONE', #58033, #49868, #2955, .T. ) ;
#44976 = DIRECTION ( 'NONE',  ( 1.000000000000000000, 0.000000000000000000, 0.000000000000000000 ) ) ;
#44977 = DIRECTION ( 'NONE',  ( 1.000000000000000000, 0.000000000000000000, 0.000000000000000000 ) ) ;
#44978 = VECTOR ( 'NONE', #3365, 1000.000000000000000 ) ;
#44979 = CYLINDRICAL_SURFACE ( 'NONE', #43118, 4.999999999999999112 ) ;
#44980 = CARTESIAN_POINT ( 'NONE',  ( 2.259025283528087513, 5.764013728792251712, -5.014999102875807857 ) ) ;
#44981 = CARTESIAN_POINT ( 'NONE',  ( -27.08704841010922593, -0.1930432016059823730, -2.291653842312389333 ) ) ;
#44982 = CARTESIAN_POINT ( 'NONE',  ( 35.00000000000000000, -4.545979934229326780, 11.30684963584393543 ) ) ;
#44984 = VERTEX_POINT ( 'NONE', #54473 ) ;
#44983 = CARTESIAN_POINT ( 'NONE',  ( 35.00000000000000000, 3.916263239775349625, -11.07407352312214144 ) ) ;
#44985 = ORIENTED_EDGE ( 'NONE', *, *, #20088, .T. ) ;
#44986 = CARTESIAN_POINT ( 'NONE',  ( 13.41004496935349799, -12.48441396568899187, -5.141889352316721506 ) ) ;
#44987 = VERTEX_POINT ( 'NONE', #2644 ) ;
#44988 = B_SPLINE_CURVE_WITH_KNOTS ( 'NONE', 3,
 ( #6275, #946, #61139, #42140, #6603, #26219, #21214, #5629, #41834, #62122, #41162, #41488, #35833, #11567, #20583, #11254, #16240, #31841, #1621, #61783, #56134, #56475, #630, #56830 ),
 .UNSPECIFIED., .F., .F.,
 ( 4, 2, 2, 2, 2, 2, 2, 2, 2, 2, 2, 4 ),
 ( 2.637977740025101358E-18, 0.001239215294917696492, 0.001858822942376543328, 0.002478430589835390382, 0.003717645884753084055, 0.004337253532211930891, 0.004956861179670778161, 0.005576468827129624564, 0.006196076474588470100, 0.007435291769506157701, 0.008674507064423846170, 0.009913722359341532037 ),
 .UNSPECIFIED. ) ;
#44989 = AXIS2_PLACEMENT_3D ( 'NONE', #39800, #59426, #49477 ) ;
#44990 = ORIENTED_EDGE ( 'NONE', *, *, #25008, .F. ) ;
#44992 = AXIS2_PLACEMENT_3D ( 'NONE', #35640, #44977, #19725 ) ;
#44991 = CARTESIAN_POINT ( 'NONE',  ( 0.3223008802179207488, 8.069628056118119730, 9.236652594547164696 ) ) ;
#44993 = FACE_OUTER_BOUND ( 'NONE', #60419, .T. ) ;
#44994 = DIRECTION ( 'NONE',  ( 0.000000000000000000, 0.6745969609292609137, 0.7381862504172000961 ) ) ;
#44995 = CARTESIAN_POINT ( 'NONE',  ( 35.00000000000000000, -8.573591947375261313, 8.029056188533775895 ) ) ;
#44996 = DIRECTION ( 'NONE',  ( -0.9582930651793755139, 0.06744057189511765138, -0.2777159889015695104 ) ) ;
#44997 = EDGE_CURVE ( 'NONE', #7860, #16892, #50735, .T. ) ;
#44998 = CIRCLE ( 'NONE', #59858, 5.000000000000001776 ) ;
#44999 = CARTESIAN_POINT ( 'NONE',  ( 36.00000000000000711, 0.9416912585476251429, 12.71517666308946382 ) ) ;
#45000 = LINE ( 'NONE', #24067, #50386 ) ;
#45001 = EDGE_CURVE ( 'NONE', #45854, #18262, #29194, .T. ) ;
#45002 = AXIS2_PLACEMENT_3D ( 'NONE', #53461, #1367, #51906 ) ;
#45003 = VERTEX_POINT ( 'NONE', #23218 ) ;
#45004 = CARTESIAN_POINT ( 'NONE',  ( 2.034671305879419467, -8.476347594674740193, -8.030508024280845092 ) ) ;
#45005 = AXIS2_PLACEMENT_3D ( 'NONE', #41137, #20213, #40489 ) ;
#45006 = FACE_OUTER_BOUND ( 'NONE', #14306, .T. ) ;
#45007 = CARTESIAN_POINT ( 'NONE',  ( -18.51542011345573613, -4.386464785673767075, 12.76797095508238300 ) ) ;
#45008 = EDGE_LOOP ( 'NONE', ( #53039, #62152, #52071, #35835 ) ) ;
#45009 = AXIS2_PLACEMENT_3D ( 'NONE', #45633, #40650, #15381 ) ;
#45010 = AXIS2_PLACEMENT_3D ( 'NONE', #50033, #60322, #24760 ) ;
#45011 = CARTESIAN_POINT ( 'NONE',  ( 49.78928762170308886, -0.04292493490551599344, 3.265281182697543638 ) ) ;
#45012 = VECTOR ( 'NONE', #39497, 1000.000000000000000 ) ;
#45013 = CARTESIAN_POINT ( 'NONE',  ( -35.05175862995318425, -0.005323180402361238350, 0.01139565579894724623 ) ) ;
#45014 = FACE_OUTER_BOUND ( 'NONE', #32762, .T. ) ;
#45015 = ORIENTED_EDGE ( 'NONE', *, *, #10142, .T. ) ;
#45016 = LINE ( 'NONE', #60971, #36260 ) ;
#45017 = CARTESIAN_POINT ( 'NONE',  ( 6.333770985428929912, -31.24637718316046531, 14.41548832156072102 ) ) ;
#45018 = CARTESIAN_POINT ( 'NONE',  ( 37.00000000000000711, 4.705694406421931860E-17, -3.469127814946512892E-15 ) ) ;
#45019 = AXIS2_PLACEMENT_3D ( 'NONE', #20295, #40572, #55878 ) ;
#45020 = CARTESIAN_POINT ( 'NONE',  ( 2.941278708680199916, 1.198640839021308357, 6.021511413163964654 ) ) ;
#45021 = CARTESIAN_POINT ( 'NONE',  ( 2.000000000000001776, -7.387287142779360494, 1.295372019972132804 ) ) ;
#45022 = EDGE_CURVE ( 'NONE', #13885, #3120, #26327, .T. ) ;
#45023 = ORIENTED_EDGE ( 'NONE', *, *, #21816, .T. ) ;
#45024 = DIRECTION ( 'NONE',  ( 1.000000000000000000, -0.000000000000000000, 0.000000000000000000 ) ) ;
#45025 = CARTESIAN_POINT ( 'NONE',  ( 0.2648321136542700072, -12.08378267055566013, 1.986804758684075578 ) ) ;
#45026 = DIRECTION ( 'NONE',  ( 0.000000000000000000, -0.01356324068817998940, 0.9999080150203990547 ) ) ;
#45027 = ORIENTED_EDGE ( 'NONE', *, *, #62909, .F. ) ;
#45028 = CARTESIAN_POINT ( 'NONE',  ( 0.000000000000000000, -5.217815162096798076, -5.387430271863655307 ) ) ;
#45029 = CARTESIAN_POINT ( 'NONE',  ( -37.00000000000000711, 0.000000000000000000, 0.000000000000000000 ) ) ;
#45030 = ORIENTED_EDGE ( 'NONE', *, *, #5870, .T. ) ;
#45031 = CIRCLE ( 'NONE', #43951, 2.899999999999994582 ) ;
#45032 = CIRCLE ( 'NONE', #14215, 12.74999999999999822 ) ;
#45033 = ORIENTED_EDGE ( 'NONE', *, *, #9137, .T. ) ;
#45034 = ORIENTED_EDGE ( 'NONE', *, *, #31825, .F. ) ;
#45035 = EDGE_CURVE ( 'NONE', #47412, #20061, #35836, .T. ) ;
#45036 = ORIENTED_EDGE ( 'NONE', *, *, #36412, .F. ) ;
#45037 = DIRECTION ( 'NONE',  ( 0.000000000000000000, 0.000000000000000000, 1.000000000000000000 ) ) ;
#45038 = CARTESIAN_POINT ( 'NONE',  ( -22.30625920655495165, -2.610366806364689651, 2.750410778797883982 ) ) ;
#45040 = DIRECTION ( 'NONE',  ( -1.000000000000000000, 0.000000000000000000, -0.000000000000000000 ) ) ;
#45039 = SHAPE_REPRESENTATION ( 'tweezer drum assembly', ( #24966 ), #7986 ) ;
#45041 = DIRECTION ( 'NONE',  ( -1.000000000000000000, 0.000000000000000000, 0.000000000000000000 ) ) ;
#45042 = AXIS2_PLACEMENT_3D ( 'NONE', #33475, #29147, #64369 ) ;
#45043 = CARTESIAN_POINT ( 'NONE',  ( -13.20530710592869283, -34.09051099065911217, 9.405657446765959051 ) ) ;
#45044 = CARTESIAN_POINT ( 'NONE',  ( -27.05874794189610455, 2.503708927703406609E-30, 1.499999999999991562 ) ) ;
#45046 = ORIENTED_EDGE ( 'NONE', *, *, #6986, .F. ) ;
#45045 = CARTESIAN_POINT ( 'NONE',  ( -17.05023968204110929, -34.50000000000000000, -4.356789313881321846 ) ) ;
#45047 = DIRECTION ( 'NONE',  ( 1.000000000000000000, -0.000000000000000000, 0.000000000000000000 ) ) ;
#45048 = ADVANCED_FACE ( 'NONE', ( #48191 ), #49148, .F. ) ;
#45049 = ORIENTED_EDGE ( 'NONE', *, *, #50357, .F. ) ;
#45050 = CARTESIAN_POINT ( 'NONE',  ( 37.00000000000000711, 11.47758908105697806, 2.497432891016712286 ) ) ;
#45051 = AXIS2_PLACEMENT_3D ( 'NONE', #65094, #54491, #23574 ) ;
#45052 = ORIENTED_EDGE ( 'NONE', *, *, #13889, .T. ) ;
#45053 = ORIENTED_EDGE ( 'NONE', *, *, #47728, .T. ) ;
#45054 = CARTESIAN_POINT ( 'NONE',  ( -27.32337605527169089, 2.404211887218409949, 1.812546145273324028 ) ) ;
#45055 = CARTESIAN_POINT ( 'NONE',  ( 4.972137933590733638, -28.45452681573965137, 13.21946257705964811 ) ) ;
#45056 = EDGE_CURVE ( 'NONE', #58885, #16670, #20998, .T. ) ;
#45057 = AXIS2_PLACEMENT_3D ( 'NONE', #47710, #46721, #2154 ) ;
#45058 = CARTESIAN_POINT ( 'NONE',  ( -22.28506771379528573, -0.2569416992704395830, -3.718191140878645218 ) ) ;
#45059 = LINE ( 'NONE', #19795, #33387 ) ;
#45060 = DIRECTION ( 'NONE',  ( 0.000000000000000000, -0.9467777615094538080, -0.3218879778916074463 ) ) ;
#45061 = DIRECTION ( 'NONE',  ( 1.000000000000000000, 0.000000000000000000, 0.000000000000000000 ) ) ;
#45062 = ORIENTED_EDGE ( 'NONE', *, *, #61498, .T. ) ;
#45063 =( BOUNDED_SURFACE ( )  B_SPLINE_SURFACE ( 3, 1, ( 
 ( #53101, #58429 ),
 ( #38459, #23167 ),
 ( #63710, #33480 ),
 ( #53769, #22179 ) ),
 .UNSPECIFIED., .F., .F., .F. ) 
 B_SPLINE_SURFACE_WITH_KNOTS ( ( 4, 4 ),
 ( 2, 2 ),
 ( 0.000000000000000000, 1.000000000000000000 ),
 ( 0.000000000000000000, 1.000000000000000000 ),
 .UNSPECIFIED. ) 
 GEOMETRIC_REPRESENTATION_ITEM ( )  RATIONAL_B_SPLINE_SURFACE ( (
 ( 1.000000000000000000, 1.000000000000000000),
 ( 0.9942764183789327692, 0.8450855930916580938),
 ( 0.9942764183789327692, 0.8450855930916580938),
 ( 1.000000000000000000, 1.000000000000000000) ) ) 
 REPRESENTATION_ITEM ( '' )  SURFACE ( )  );
#45064 = ORIENTED_EDGE ( 'NONE', *, *, #21202, .F. ) ;
#45065 = LINE ( 'NONE', #35054, #65590 ) ;
#45066 = ORIENTED_EDGE ( 'NONE', *, *, #37842, .T. ) ;
#45067 = ORIENTED_EDGE ( 'NONE', *, *, #63208, .T. ) ;
#45068 = B_SPLINE_CURVE_WITH_KNOTS ( 'NONE', 3,
 ( #47896, #38221, #17644, #33249, #21389, #46657, #56979, #16061, #48252, #63489 ),
 .UNSPECIFIED., .F., .F.,
 ( 4, 2, 2, 2, 4 ),
 ( 0.000000000000000000, 0.001114213790187107336, 0.002228427580374214671, 0.003342641370561322007, 0.004456855160748429343 ),
 .UNSPECIFIED. ) ;
#45069 = AXIS2_PLACEMENT_3D ( 'NONE', #58101, #48460, #42782 ) ;
#45070 = CARTESIAN_POINT ( 'NONE',  ( 2.273267844204866162, -7.501135923490791946, 1.476347988307447734 ) ) ;
#45071 = CARTESIAN_POINT ( 'NONE',  ( -22.29770266787582500, 0.8895590726607195409, -3.635870259503093838 ) ) ;
#45072 = B_SPLINE_CURVE_WITH_KNOTS ( 'NONE', 3,
 ( #49153, #3918, #39136, #23878, #59429, #8894, #40110, #59766 ),
 .UNSPECIFIED., .F., .F.,
 ( 4, 2, 2, 4 ),
 ( 0.000000000000000000, 0.002717879308656051540, 0.004076818962984075576, 0.005435758617312099611 ),
 .UNSPECIFIED. ) ;
#45073 = CARTESIAN_POINT ( 'NONE',  ( 0.3675815128205894289, -12.04510820461660892, 2.391755495700564449 ) ) ;
#45074 = DIRECTION ( 'NONE',  ( 0.000000000000000000, 0.8369827122275362852, 0.5472293298355244140 ) ) ;
#45075 = ADVANCED_FACE ( 'NONE', ( #27884 ), #5573, .T. ) ;
#45076 = CARTESIAN_POINT ( 'NONE',  ( -11.37391343693395562, -6.796058610810909784, -9.899934513732258523 ) ) ;
#45077 = AXIS2_PLACEMENT_3D ( 'NONE', #59470, #54820, #9553 ) ;
#45078 = CARTESIAN_POINT ( 'NONE',  ( -37.00000000000000711, -9.217970097227665249, -7.971186206369574201 ) ) ;
#45079 = ORIENTED_EDGE ( 'NONE', *, *, #53569, .F. ) ;
#45080 = VERTEX_POINT ( 'NONE', #30482 ) ;
#45081 = FACE_OUTER_BOUND ( 'NONE', #48334, .T. ) ;
#45082 = AXIS2_PLACEMENT_3D ( 'NONE', #22804, #43058, #3179 ) ;
#45083 = DIRECTION ( 'NONE',  ( 1.000000000000000000, 0.000000000000000000, 0.000000000000000000 ) ) ;
#45084 = CIRCLE ( 'NONE', #14266, 5.000000000000000888 ) ;
#45085 = CYLINDRICAL_SURFACE ( 'NONE', #43618, 12.75000000000000178 ) ;
#45086 = EDGE_CURVE ( 'NONE', #41139, #27477, #32655, .T. ) ;
#45087 = CARTESIAN_POINT ( 'NONE',  ( 6.800436580320503133, -6.134824022537911148, 10.31531696979683410 ) ) ;
#45088 = CARTESIAN_POINT ( 'NONE',  ( 2.305787727787084407, -5.970480882365253983, 4.792270232040873879 ) ) ;
#45089 = CIRCLE ( 'NONE', #61039, 2.899999999999994582 ) ;
#45090 = CARTESIAN_POINT ( 'NONE',  ( -10.60692174091447981, -5.627218222672255798, -10.60063337488197632 ) ) ;
#45091 = B_SPLINE_CURVE_WITH_KNOTS ( 'NONE', 3,
 ( #50392, #40049, #55022, #24778, #45700, #60337, #15756 ),
 .UNSPECIFIED., .F., .F.,
 ( 4, 3, 4 ),
 ( 3.893818994016422208E-15, 0.002398160485434589102, 0.005002426799381067338 ),
 .UNSPECIFIED. ) ;
#45092 = CYLINDRICAL_SURFACE ( 'NONE', #32192, 5.000000000000000888 ) ;
#45093 = DIRECTION ( 'NONE',  ( -1.000000000000000000, 0.000000000000000000, 0.000000000000000000 ) ) ;
#45094 = ORIENTED_EDGE ( 'NONE', *, *, #7883, .F. ) ;
#45095 = AXIS2_PLACEMENT_3D ( 'NONE', #45623, #55626, #74 ) ;
#45096 = CARTESIAN_POINT ( 'NONE',  ( 0.2653141334712571520, 12.06772877558523227, 2.083134085643086220 ) ) ;
#45097 = CYLINDRICAL_SURFACE ( 'NONE', #1385, 2.899999999999994582 ) ;
#45098 = CYLINDRICAL_SURFACE ( 'NONE', #57789, 2.899999999999994582 ) ;
#45099 = AXIS2_PLACEMENT_3D ( 'NONE', #24419, #33431, #28428 ) ;
#45100 = CARTESIAN_POINT ( 'NONE',  ( -14.83484859610164364, -34.67578963454042196, -7.338086519100818883 ) ) ;
#45101 = CYLINDRICAL_SURFACE ( 'NONE', #41458, 12.18649999999999878 ) ;
#45102 = EDGE_CURVE ( 'NONE', #44008, #33918, #19812, .T. ) ;
#45103 = EDGE_LOOP ( 'NONE', ( #54240, #37720, #63595, #63889 ) ) ;
#45104 = EDGE_CURVE ( 'NONE', #17490, #6738, #40124, .T. ) ;
#45105 = CARTESIAN_POINT ( 'NONE',  ( -8.891032880924177206, 12.93614229090409395, -3.860857758255646921 ) ) ;
#45106 = CARTESIAN_POINT ( 'NONE',  ( 2.899286259009568045, 6.616268644969683699, 4.231523595108440894 ) ) ;
#45107 = CARTESIAN_POINT ( 'NONE',  ( 9.079541994506246994, -32.62122108031978485, -12.39463523794014321 ) ) ;
#45108 = ORIENTED_EDGE ( 'NONE', *, *, #35028, .T. ) ;
#45109 = EDGE_CURVE ( 'NONE', #64126, #54960, #842, .T. ) ;
#45110 = FACE_OUTER_BOUND ( 'NONE', #3590, .T. ) ;
#45111 = CARTESIAN_POINT ( 'NONE',  ( 35.00000000000000000, -3.805206332242389244, 12.16893194857553340 ) ) ;
#45112 = CARTESIAN_POINT ( 'NONE',  ( -35.00000000000000000, -4.545979934229492869, 11.30684963584387681 ) ) ;
#45113 = CARTESIAN_POINT ( 'NONE',  ( 1.287602823384977446, 12.57487505104494119, 0.5522659225141822725 ) ) ;
#45114 = DIRECTION ( 'NONE',  ( -1.000000000000000000, 0.000000000000000000, 0.000000000000000000 ) ) ;
#45115 = ADVANCED_FACE ( 'NONE', ( #19861 ), #35475, .T. ) ;
#45116 = LINE ( 'NONE', #9510, #4293 ) ;
#45117 = ORIENTED_EDGE ( 'NONE', *, *, #48130, .T. ) ;
#45118 = CARTESIAN_POINT ( 'NONE',  ( 2.305787727787083519, -7.654065630109506913, -0.1666591538753489643 ) ) ;
#45119 = CARTESIAN_POINT ( 'NONE',  ( -27.08429572838383947, -1.338867938658200307, -1.859677275556420151 ) ) ;
#45120 = CARTESIAN_POINT ( 'NONE',  ( -32.00000000000000000, 5.510910596163098430E-16, 0.000000000000000000 ) ) ;
#45121 = CYLINDRICAL_SURFACE ( 'NONE', #36127, 12.75000000000000178 ) ;
#45122 = CARTESIAN_POINT ( 'NONE',  ( 0.3537226245948363323, -11.44347094181049229, -4.442821955543915458 ) ) ;
#45123 = CARTESIAN_POINT ( 'NONE',  ( -27.35552965826137140, 2.548625910254547655, 1.773915698030531951 ) ) ;
#45124 = DIRECTION ( 'NONE',  ( -1.000000000000000000, -1.836970198721029688E-16, -0.000000000000000000 ) ) ;
#45125 = ORIENTED_EDGE ( 'NONE', *, *, #236, .F. ) ;
#45126 = CIRCLE ( 'NONE', #47282, 5.000000000000000000 ) ;
#45127 = ORIENTED_EDGE ( 'NONE', *, *, #13774, .T. ) ;
#45128 = CARTESIAN_POINT ( 'NONE',  ( 2.251139882113958102, -5.003859976903235030, 5.770207524085884110 ) ) ;
#45129 = ORIENTED_EDGE ( 'NONE', *, *, #17329, .T. ) ;
#45130 = FILL_AREA_STYLE_COLOUR ( '', #42980 ) ;
#45131 = LINE ( 'NONE', #65391, #65103 ) ;
#45132 = EDGE_CURVE ( 'NONE', #40821, #35283, #17654, .T. ) ;
#45133 = FACE_OUTER_BOUND ( 'NONE', #11278, .T. ) ;
#45134 = EDGE_LOOP ( 'NONE', ( #13052, #43883, #37666, #55349 ) ) ;
#45135 = FACE_OUTER_BOUND ( 'NONE', #23429, .T. ) ;
#45136 = VECTOR ( 'NONE', #18928, 1000.000000000000000 ) ;
#45137 = CYLINDRICAL_SURFACE ( 'NONE', #63331, 7.499999999999988454 ) ;
#45138 = FACE_OUTER_BOUND ( 'NONE', #48276, .T. ) ;
#45139 = ORIENTED_EDGE ( 'NONE', *, *, #34090, .T. ) ;
#45140 = VERTEX_POINT ( 'NONE', #30797 ) ;
#45141 = CARTESIAN_POINT ( 'NONE',  ( 37.00000000000000711, 1.456211999474505969, 11.65554240571055011 ) ) ;
#45142 = ORIENTED_EDGE ( 'NONE', *, *, #61916, .T. ) ;
#45143 = CARTESIAN_POINT ( 'NONE',  ( 37.00000000000000711, -8.699265615723044576, -8.534258022646067587 ) ) ;
#45144 = ORIENTED_EDGE ( 'NONE', *, *, #58702, .F. ) ;
#45145 = CARTESIAN_POINT ( 'NONE',  ( -27.08954555554413446, 2.300063521504144948, -0.1819824474943290971 ) ) ;
#45146 = AXIS2_PLACEMENT_3D ( 'NONE', #61237, #49957, #44964 ) ;
#45147 = CARTESIAN_POINT ( 'NONE',  ( 2.297017764050092836, 7.133399178907352756, -2.771707546665520994 ) ) ;
#45148 = CARTESIAN_POINT ( 'NONE',  ( -7.287102677926679206, 8.374986170366049976, -10.59034548381062102 ) ) ;
#45149 = CARTESIAN_POINT ( 'NONE',  ( 25.00000000000000355, -9.999999999999998224, 1.530808498934191521E-15 ) ) ;
#45150 = CARTESIAN_POINT ( 'NONE',  ( -35.00000000000000000, 11.67026961469348123, 4.564151185897115326 ) ) ;
#45151 = ORIENTED_EDGE ( 'NONE', *, *, #40451, .F. ) ;
#45152 = CARTESIAN_POINT ( 'NONE',  ( -37.00000000000000711, 0.000000000000000000, 0.000000000000000000 ) ) ;
#45153 = CARTESIAN_POINT ( 'NONE',  ( 0.2648978790185602672, 7.769924372105329269, -9.465406350830530613 ) ) ;
#45154 = CARTESIAN_POINT ( 'NONE',  ( 0.2650492433740071485, -9.309907554970028087, 7.955688793816054982 ) ) ;
#45155 = CARTESIAN_POINT ( 'NONE',  ( 1.452237505248552996, -10.65201107290462623, -6.833827325205429126 ) ) ;
#45156 = CARTESIAN_POINT ( 'NONE',  ( -20.34436657951988181, 13.27874470876743729, -2.506383895450033261 ) ) ;
#45157 = DIRECTION ( 'NONE',  ( -1.000000000000000000, 0.000000000000000000, 0.000000000000000000 ) ) ;
#45158 = DIRECTION ( 'NONE',  ( 1.000000000000000000, 0.000000000000000000, 0.000000000000000000 ) ) ;
#45159 = DIRECTION ( 'NONE',  ( -1.000000000000000000, 0.000000000000000000, 0.000000000000000000 ) ) ;
#45160 = DIRECTION ( 'NONE',  ( 0.000000000000000000, 0.8009703041134145218, 0.5987040770935704304 ) ) ;
#45161 = EDGE_CURVE ( 'NONE', #22647, #11898, #24859, .T. ) ;
#45162 = AXIS2_PLACEMENT_3D ( 'NONE', #23678, #3405, #7718 ) ;
#45163 = VERTEX_POINT ( 'NONE', #15515 ) ;
#45164 = CARTESIAN_POINT ( 'NONE',  ( 0.3109076770649027432, 0.2359198520041151936, 12.25911371383827309 ) ) ;
#45165 = ORIENTED_EDGE ( 'NONE', *, *, #13311, .T. ) ;
#45166 = CARTESIAN_POINT ( 'NONE',  ( 2.000000000000001776, -1.754183803416586196, 6.711026108862235162 ) ) ;
#45167 = CARTESIAN_POINT ( 'NONE',  ( 2.259830038564996091, -7.499347412930715606, -1.462175769136920156 ) ) ;
#45168 = DIRECTION ( 'NONE',  ( -1.000000000000000000, -0.000000000000000000, 0.000000000000000000 ) ) ;
#45169 = DIRECTION ( 'NONE',  ( -1.000000000000000000, -0.000000000000000000, -0.000000000000000000 ) ) ;
#45170 = CARTESIAN_POINT ( 'NONE',  ( 5.515539859299206427, -0.003193223631738841602, 0.005142293699651627470 ) ) ;
#45171 = ORIENTED_EDGE ( 'NONE', *, *, #52998, .T. ) ;
#45172 = CARTESIAN_POINT ( 'NONE',  ( 2.241352910868909643, -2.532612177304395029, -7.202080440908765979 ) ) ;
#45173 = CARTESIAN_POINT ( 'NONE',  ( 2.717984159219170692, 2.397195612260841102, -7.415470774236799123 ) ) ;
#45174 = CARTESIAN_POINT ( 'NONE',  ( -27.08456565417846917, 2.084650034356375858, 0.9533904527919445648 ) ) ;
#45175 = CYLINDRICAL_SURFACE ( 'NONE', #16810, 12.74999999999999822 ) ;
#45176 = ADVANCED_FACE ( 'NONE', ( #35782 ), #45137, .T. ) ;
#45177 = FACE_OUTER_BOUND ( 'NONE', #17523, .T. ) ;
#45178 = AXIS2_PLACEMENT_3D ( 'NONE', #40845, #35816, #26519 ) ;
#45179 = ORIENTED_EDGE ( 'NONE', *, *, #26941, .F. ) ;
#45180 = EDGE_CURVE ( 'NONE', #33526, #23975, #37903, .T. ) ;
#45181 = DIRECTION ( 'NONE',  ( 0.000000000000000000, -0.2355298848897586228, -0.9718671068226442111 ) ) ;
#45182 = VERTEX_POINT ( 'NONE', #34797 ) ;
#45183 = ADVANCED_FACE ( 'NONE', ( #65712 ), #31636, .F. ) ;
#45184 = CARTESIAN_POINT ( 'NONE',  ( 0.3341166715381287955, -0.2526177176099212440, -12.26652061402056404 ) ) ;
#45185 = CARTESIAN_POINT ( 'NONE',  ( -14.24371601685106548, -33.70914924250434552, 9.547107017906496296 ) ) ;
#45186 = CARTESIAN_POINT ( 'NONE',  ( -7.181456785175555524, -5.890186129966251904, -10.45493698471458188 ) ) ;
#45187 = DIRECTION ( 'NONE',  ( 0.000000000000000000, -0.01356324068817991307, 0.9999080150203990547 ) ) ;
#45188 = CIRCLE ( 'NONE', #44100, 12.75000000000000178 ) ;
#45189 = EDGE_LOOP ( 'NONE', ( #62482, #44386, #19330, #482 ) ) ;
#45191 = VERTEX_POINT ( 'NONE', #47117 ) ;
#45190 = EDGE_CURVE ( 'NONE', #19934, #45235, #22148, .T. ) ;
#45192 = DIRECTION ( 'NONE',  ( 0.000000000000000000, 0.000000000000000000, 1.000000000000000000 ) ) ;
#45193 = ORIENTED_EDGE ( 'NONE', *, *, #10570, .F. ) ;
#45194 = CARTESIAN_POINT ( 'NONE',  ( -37.00000000000000711, -8.766823244862047559, 7.817610399097479679 ) ) ;
#45195 = CARTESIAN_POINT ( 'NONE',  ( 36.00000000000000711, 7.094637218249506994, 10.59380114696461916 ) ) ;
#45196 = CARTESIAN_POINT ( 'NONE',  ( -22.27713295444592845, -3.528329525272665634, -1.050517974989019221 ) ) ;
#45197 = DIRECTION ( 'NONE',  ( -1.000000000000000000, 0.000000000000000000, 0.000000000000000000 ) ) ;
#45198 = DIRECTION ( 'NONE',  ( 0.000000000000000000, 0.01356324068817998940, -0.9999080150203989437 ) ) ;
#45199 = ADVANCED_FACE ( 'NONE', ( #52437 ), #51774, .T. ) ;
#45200 = LINE ( 'NONE', #23041, #22172 ) ;
#45201 = FACE_OUTER_BOUND ( 'NONE', #17292, .T. ) ;
#45202 = ORIENTED_EDGE ( 'NONE', *, *, #21248, .T. ) ;
#45204 = VERTEX_POINT ( 'NONE', #1229 ) ;
#45203 = CARTESIAN_POINT ( 'NONE',  ( -8.841892098821560353, -8.618917129353741657, -8.357420571532406584 ) ) ;
#45205 = ORIENTED_EDGE ( 'NONE', *, *, #46205, .F. ) ;
#45206 = CARTESIAN_POINT ( 'NONE',  ( 2.406456491626046912, -8.382123850278466293, -6.212289237905048722 ) ) ;
#45207 = EDGE_CURVE ( 'NONE', #47458, #23272, #61264, .T. ) ;
#45208 = AXIS2_PLACEMENT_3D ( 'NONE', #23333, #47954, #48617 ) ;
#45209 = CARTESIAN_POINT ( 'NONE',  ( -27.09602251845159415, 1.927725285105659880, -1.302811993375590172 ) ) ;
#45210 = ORIENTED_EDGE ( 'NONE', *, *, #26458, .T. ) ;
#45211 = ADVANCED_FACE ( 'NONE', ( #56418 ), #17685, .F. ) ;
#45212 = CARTESIAN_POINT ( 'NONE',  ( -35.05012975565874456, -0.01363945138522591922, 0.002839961651350852816 ) ) ;
#45213 = ORIENTED_EDGE ( 'NONE', *, *, #33284, .F. ) ;
#45214 = DIRECTION ( 'NONE',  ( -1.000000000000000000, 0.000000000000000000, 0.000000000000000000 ) ) ;
#45215 = DIRECTION ( 'NONE',  ( -1.000000000000000000, 0.000000000000000000, 0.000000000000000000 ) ) ;
#45216 = CARTESIAN_POINT ( 'NONE',  ( 17.11285760380292231, 10.50878607827772804, 5.793619504978376078 ) ) ;
#45217 = CARTESIAN_POINT ( 'NONE',  ( -27.08430792439081003, -2.211452765398044473, -0.6005833784282822441 ) ) ;
#45218 = ORIENTED_EDGE ( 'NONE', *, *, #9075, .F. ) ;
#45220 = EDGE_CURVE ( 'NONE', #57171, #29799, #6544, .T. ) ;
#45219 = VERTEX_POINT ( 'NONE', #62371 ) ;
#45221 = CARTESIAN_POINT ( 'NONE',  ( 2.655192694323576852, 2.733486750964913892, -9.204230091443479367 ) ) ;
#45222 = EDGE_LOOP ( 'NONE', ( #41879, #52156, #19264, #3856 ) ) ;
#45223 = CARTESIAN_POINT ( 'NONE',  ( 0.3278977287071236923, 11.60975784853197545, -3.961557589215493280 ) ) ;
#45224 = ORIENTED_EDGE ( 'NONE', *, *, #23195, .F. ) ;
#45225 = ORIENTED_EDGE ( 'NONE', *, *, #34213, .T. ) ;
#45226 = VERTEX_POINT ( 'NONE', #6876 ) ;
#45227 = DIRECTION ( 'NONE',  ( 0.000000000000000000, -0.01356324068817998940, 0.9999080150203990547 ) ) ;
#45228 = CARTESIAN_POINT ( 'NONE',  ( 17.99690872998901980, -28.74566129397116754, 8.126501682513223912 ) ) ;
#45229 = DIRECTION ( 'NONE',  ( 1.000000000000000000, 0.000000000000000000, 0.000000000000000000 ) ) ;
#45230 = CARTESIAN_POINT ( 'NONE',  ( -35.04709527796842394, -0.005292201869334239861, -0.01117341439756461274 ) ) ;
#45231 = ORIENTED_EDGE ( 'NONE', *, *, #38814, .F. ) ;
#45232 = AXIS2_PLACEMENT_3D ( 'NONE', #16753, #62616, #12406 ) ;
#45233 = DIRECTION ( 'NONE',  ( -1.000000000000000000, 0.000000000000000000, -0.000000000000000000 ) ) ;
#45234 = CIRCLE ( 'NONE', #16521, 4.999999999999999112 ) ;
#45235 = VERTEX_POINT ( 'NONE', #888 ) ;
#45236 = CARTESIAN_POINT ( 'NONE',  ( 37.00000000000000711, -12.18359334611896472, -0.2661492558802951991 ) ) ;
#45237 = DIRECTION ( 'NONE',  ( 0.000000000000000000, 0.7621620551276332423, 0.6473862847818313560 ) ) ;
#45238 = ORIENTED_EDGE ( 'NONE', *, *, #9691, .T. ) ;
#45239 = CARTESIAN_POINT ( 'NONE',  ( 0.2657645697724667633, -10.68050050043095567, 5.991637049003212034 ) ) ;
#45240 = CARTESIAN_POINT ( 'NONE',  ( 0.3053067050349170808, 3.975408458060513794, 11.59706307017084193 ) ) ;
#45241 = CARTESIAN_POINT ( 'NONE',  ( 2.266490820343221468, -6.690312181904289446, -3.694838443752371582 ) ) ;
#45242 = VECTOR ( 'NONE', #5406, 1000.000000000000000 ) ;
#45243 = EDGE_CURVE ( 'NONE', #21897, #54995, #10272, .T. ) ;
#45244 = ADVANCED_FACE ( 'NONE', ( #36792 ), #11513, .T. ) ;
#45245 = EDGE_LOOP ( 'NONE', ( #24423, #38589, #36736, #15393 ) ) ;
#45246 = CARTESIAN_POINT ( 'NONE',  ( 2.889800649504073782, -3.002151847318954125, 5.334644486274186193 ) ) ;
#45247 =( BOUNDED_CURVE ( )  B_SPLINE_CURVE ( 3, ( #56662, #21392, #48255, #27595 ),
 .UNSPECIFIED., .F., .F. ) 
 B_SPLINE_CURVE_WITH_KNOTS ( ( 4, 4 ),
 ( 1.289813438233471610, 1.322487409060285168 ),
 .UNSPECIFIED. ) 
 CURVE ( )  GEOMETRIC_REPRESENTATION_ITEM ( )  RATIONAL_B_SPLINE_CURVE ( ( 1.000000000000000000, 0.9999110362812402286, 0.9999110362812402286, 1.000000000000000000 ) ) 
 REPRESENTATION_ITEM ( '' )  );
#45248 = ORIENTED_EDGE ( 'NONE', *, *, #26032, .T. ) ;
#45249 = CARTESIAN_POINT ( 'NONE',  ( -24.35967074841363456, -9.892812110492778643, 9.188125470810931006 ) ) ;
#45250 = FILL_AREA_STYLE ('',( #24977 ) ) ;
#45251 = CARTESIAN_POINT ( 'NONE',  ( 2.835339799623982859, 6.941489812670579518, -3.628068688271603559 ) ) ;
#45252 = CARTESIAN_POINT ( 'NONE',  ( 2.258463476536300973, -3.701774005561162095, -6.683417898966597548 ) ) ;
#45253 = DIRECTION ( 'NONE',  ( 0.000000000000000000, 0.01356324068817999114, -0.9999080150203989437 ) ) ;
#45254 = ORIENTED_EDGE ( 'NONE', *, *, #38899, .T. ) ;
#45255 = EDGE_CURVE ( 'NONE', #30228, #57752, #47463, .T. ) ;
#45256 = CARTESIAN_POINT ( 'NONE',  ( -17.54726996257253191, -11.36053454945672136, 3.865003848717349033 ) ) ;
#45257 = CARTESIAN_POINT ( 'NONE',  ( 2.000000000000001776, 0.000000000000000000, 0.000000000000000000 ) ) ;
#45258 = DIRECTION ( 'NONE',  ( -1.000000000000000000, 0.000000000000000000, 0.000000000000000000 ) ) ;
#45259 = DIRECTION ( 'NONE',  ( -0.000000000000000000, -0.000000000000000000, -1.000000000000000000 ) ) ;
#45260 = EDGE_CURVE ( 'NONE', #41945, #24950, #45420, .T. ) ;
#45261 = CARTESIAN_POINT ( 'NONE',  ( 0.3223008802179238019, -12.11889957318022937, -1.888629463821808852 ) ) ;
#45262 = CARTESIAN_POINT ( 'NONE',  ( -27.35552965826137140, -0.2619431035391951434, 3.094132632038943065 ) ) ;
#45263 = ADVANCED_FACE ( 'NONE', ( #53417 ), #64025, .T. ) ;
#45264 = DIRECTION ( 'NONE',  ( -1.000000000000000000, 0.000000000000000000, 0.000000000000000000 ) ) ;
#45265 = DIRECTION ( 'NONE',  ( 0.000000000000000000, -0.01356324068817991828, 0.9999080150203990547 ) ) ;
#45266 = CARTESIAN_POINT ( 'NONE',  ( -35.00000000000000000, -11.42599468261432527, 4.237620530777758354 ) ) ;
#45267 = AXIS2_PLACEMENT_3D ( 'NONE', #39962, #44292, #49631 ) ;
#45268 = ORIENTED_EDGE ( 'NONE', *, *, #8860, .T. ) ;
#45269 = CARTESIAN_POINT ( 'NONE',  ( -27.09729107899852352, -1.302895495071029419, -1.932259710108178430 ) ) ;
#45270 = VECTOR ( 'NONE', #39697, 1000.000000000000000 ) ;
#45271 = EDGE_LOOP ( 'NONE', ( #52251, #41155, #22272, #25937 ) ) ;
#45272 = CARTESIAN_POINT ( 'NONE',  ( 1.000000000000000888, -6.936109781200648250, -2.853135311045116307 ) ) ;
#45273 = CARTESIAN_POINT ( 'NONE',  ( 5.515539859299206427, -0.0001942659352248233629, 0.006049968793488396702 ) ) ;
#45274 = DIRECTION ( 'NONE',  ( 0.000000000000000000, 0.000000000000000000, 1.000000000000000000 ) ) ;
#45275 = EDGE_CURVE ( 'NONE', #666, #21047, #7380, .T. ) ;
#45276 = CARTESIAN_POINT ( 'NONE',  ( 5.515539859299206427, -0.004759416711442203581, -0.003740028639278331068 ) ) ;
#45277 = VERTEX_POINT ( 'NONE', #2882 ) ;
#45278 = ADVANCED_FACE ( 'NONE', ( #7505 ), #38767, .T. ) ;
#45279 = ORIENTED_EDGE ( 'NONE', *, *, #4589, .T. ) ;
#45280 = VERTEX_POINT ( 'NONE', #2556 ) ;
#45281 = EDGE_CURVE ( 'NONE', #39745, #9785, #37560, .T. ) ;
#45282 = CARTESIAN_POINT ( 'NONE',  ( 2.781367136452478572, 3.637318098960558022, -6.916275212954685614 ) ) ;
#45283 = ORIENTED_EDGE ( 'NONE', *, *, #28993, .T. ) ;
#45284 = EDGE_CURVE ( 'NONE', #25983, #31872, #29402, .T. ) ;
#45285 = FACE_OUTER_BOUND ( 'NONE', #56766, .T. ) ;
#45286 = CARTESIAN_POINT ( 'NONE',  ( 3.031336079629378677, -2.306006909710469621, 7.553623348802286586 ) ) ;
#45287 = ORIENTED_EDGE ( 'NONE', *, *, #38418, .F. ) ;
#45288 = LINE ( 'NONE', #409, #6735 ) ;
#45289 = CARTESIAN_POINT ( 'NONE',  ( 0.9185403246812442468, -30.53691730605505228, -15.30924831176142042 ) ) ;
#45290 = FACE_OUTER_BOUND ( 'NONE', #7395, .T. ) ;
#45292 = ORIENTED_EDGE ( 'NONE', *, *, #61867, .F. ) ;
#45291 = CARTESIAN_POINT ( 'NONE',  ( -27.05874794189610455, -0.3907329275428090276, -2.180117559290211116 ) ) ;
#45293 = EDGE_CURVE ( 'NONE', #54568, #1623, #3936, .T. ) ;
#45294 = DIRECTION ( 'NONE',  ( 1.000000000000000000, -0.000000000000000000, -0.000000000000000000 ) ) ;
#45295 = ORIENTED_EDGE ( 'NONE', *, *, #8860, .F. ) ;
#45296 = CARTESIAN_POINT ( 'NONE',  ( 35.00000000000000000, -2.627174906296994905, -11.44858830469739530 ) ) ;
#45297 = VERTEX_POINT ( 'NONE', #33755 ) ;
#45298 = CARTESIAN_POINT ( 'NONE',  ( 35.00000000000000000, 12.71517666308947803, -0.9416912585474880304 ) ) ;
#45299 = FACE_OUTER_BOUND ( 'NONE', #28932, .T. ) ;
#45300 = DIRECTION ( 'NONE',  ( -1.000000000000000000, 0.000000000000000000, -0.000000000000000000 ) ) ;
#45301 = CARTESIAN_POINT ( 'NONE',  ( 1.283627346226769328, -6.763590725840913365, -10.61381050043338448 ) ) ;
#45302 = CYLINDRICAL_SURFACE ( 'NONE', #14482, 2.899999999999994582 ) ;
#45303 = CARTESIAN_POINT ( 'NONE',  ( 0.2958664285830425733, -12.25438626999990355, 0.2205161970873960042 ) ) ;
#45304 = DIRECTION ( 'NONE',  ( 0.000000000000000000, 1.000000000000000000, 0.000000000000000000 ) ) ;
#45305 = CARTESIAN_POINT ( 'NONE',  ( 35.00000000000000000, 8.052525312709883920, -8.551552972817113130 ) ) ;
#45306 = DIRECTION ( 'NONE',  ( -0.000000000000000000, -0.000000000000000000, -1.000000000000000000 ) ) ;
#45308 = ORIENTED_EDGE ( 'NONE', *, *, #62250, .F. ) ;
#45307 = CARTESIAN_POINT ( 'NONE',  ( 12.32157157451222496, 13.32610988528976570, -2.183319616765905025 ) ) ;
#45309 = FACE_OUTER_BOUND ( 'NONE', #17896, .T. ) ;
#45310 = ORIENTED_EDGE ( 'NONE', *, *, #56243, .T. ) ;
#45311 = CARTESIAN_POINT ( 'NONE',  ( 37.00000000000000711, 4.705694406421931860E-17, -3.469127814946512892E-15 ) ) ;
#45312 = EDGE_LOOP ( 'NONE', ( #13149, #23360, #36001, #51534 ) ) ;
#45313 = VERTEX_POINT ( 'NONE', #13473 ) ;
#45314 = CARTESIAN_POINT ( 'NONE',  ( 24.90014556888634800, 8.538933172091805801, -8.433831666448901032 ) ) ;
#45315 = CARTESIAN_POINT ( 'NONE',  ( -27.08416974970326763, 0.4041872645907068629, 2.255186831366090772 ) ) ;
#45316 = CARTESIAN_POINT ( 'NONE',  ( 0.000000000000000000, 2.562706407243739992, -6.312399813420325856 ) ) ;
#45317 = AXIS2_PLACEMENT_3D ( 'NONE', #46768, #16184, #16831 ) ;
#45318 = CARTESIAN_POINT ( 'NONE',  ( -37.00000000000000711, 0.4353888892048373149, 11.73808581813438323 ) ) ;
#45319 = CARTESIAN_POINT ( 'NONE',  ( 2.241352910868908310, 7.202080440908741998, 2.532612177304466972 ) ) ;
#45320 = EDGE_CURVE ( 'NONE', #3030, #54788, #8492, .T. ) ;
#45321 = AXIS2_PLACEMENT_3D ( 'NONE', #31613, #40951, #25657 ) ;
#45322 = CARTESIAN_POINT ( 'NONE',  ( 3.152665057734040488, 0.000000000000000000, 0.000000000000000000 ) ) ;
#45323 = EDGE_CURVE ( 'NONE', #48416, #42832, #3545, .T. ) ;
#45324 = ORIENTED_EDGE ( 'NONE', *, *, #29442, .T. ) ;
#45325 = CARTESIAN_POINT ( 'NONE',  ( 2.770579946183323372, -6.173813901927566405, 4.784693811915867734 ) ) ;
#45326 = DIRECTION ( 'NONE',  ( 1.000000000000000000, -0.000000000000000000, 0.000000000000000000 ) ) ;
#45327 = CARTESIAN_POINT ( 'NONE',  ( 0.2653519789438750220, -7.888580323518811888, -9.366970421692856874 ) ) ;
#45328 = EDGE_LOOP ( 'NONE', ( #47474, #40990, #24229, #54221 ) ) ;
#45329 = EDGE_CURVE ( 'NONE', #3120, #22798, #64350, .T. ) ;
#45330 = B_SPLINE_CURVE_WITH_KNOTS ( 'NONE', 3,
 ( #22396, #37705, #18426, #37362, #27383, #47678, #42660, #32678, #52991, #2473, #43012, #17756, #58318, #38013, #4776, #65568, #45307, #54659, #64278, #29666, #28698, #54323, #64584, #44626, #30008, #3470 ),
 .UNSPECIFIED., .F., .F.,
 ( 4, 2, 2, 2, 2, 2, 2, 2, 2, 2, 2, 2, 4 ),
 ( 0.000000000000000000, 0.001323017225618347038, 0.001984525838427520558, 0.002646034451236694077, 0.003969051676855037646, 0.005292068902473381214, 0.005953577515282554300, 0.006615086128091725651, 0.007938103353710070087, 0.008599611966519243172, 0.009261120579328416258, 0.009922629192137589343, 0.01058413780494676243 ),
 .UNSPECIFIED. ) ;
#45331 = CARTESIAN_POINT ( 'NONE',  ( 37.50900221036943805, -2.222235401316472903, 21.66089349574500744 ) ) ;
#45332 = CARTESIAN_POINT ( 'NONE',  ( 22.57855258442565116, 3.026812727784649493, 25.00000000000000000 ) ) ;
#45333 = CARTESIAN_POINT ( 'NONE',  ( -28.29050403390679591, -3.446535021889315598, -24.79622249374515519 ) ) ;
#45334 = B_SPLINE_CURVE_WITH_KNOTS ( 'NONE', 3,
 ( #45073, #35726, #50721, #177, #65008, #20458, #30737, #40734, #65340, #51050, #34735, #5509, #25776, #15771, #31086, #19481 ),
 .UNSPECIFIED., .F., .F.,
 ( 4, 3, 3, 3, 3, 4 ),
 ( 4.336808689942017736E-19, 0.0003017745587525235665, 0.0006035491769808712468, 0.0009053241094668126702, 0.001207275924540017736, 0.001510325902533037534 ),
 .UNSPECIFIED. ) ;
#45336 = ORIENTED_EDGE ( 'NONE', *, *, #55928, .F. ) ;
#45335 = EDGE_CURVE ( 'NONE', #3708, #6580, #4218, .T. ) ;
#45337 = CARTESIAN_POINT ( 'NONE',  ( 2.268878695253353950, 6.692359410363658334, -3.692782103667214155 ) ) ;
#45338 = DIRECTION ( 'NONE',  ( -1.000000000000000000, 0.000000000000000000, 0.000000000000000000 ) ) ;
#45339 = CARTESIAN_POINT ( 'NONE',  ( 3.057491736622230061, 2.783847009521732030, 11.67432880372605020 ) ) ;
#45340 = ADVANCED_FACE ( 'NONE', ( #16360 ), #21334, .T. ) ;
#45341 = CARTESIAN_POINT ( 'NONE',  ( -35.00000000000000000, 0.000000000000000000, 0.000000000000000000 ) ) ;
#45342 = VERTEX_POINT ( 'NONE', #35949 ) ;
#45343 = CARTESIAN_POINT ( 'NONE',  ( -35.04683013664716640, -0.006266879427269670538, -0.01065093278706642776 ) ) ;
#45344 = CARTESIAN_POINT ( 'NONE',  ( -22.27716857039623477, 3.514919882996461187, 1.095155339732065913 ) ) ;
#45345 = DIRECTION ( 'NONE',  ( -1.000000000000000000, -0.000000000000000000, -0.000000000000000000 ) ) ;
#45346 = ORIENTED_EDGE ( 'NONE', *, *, #17308, .T. ) ;
#45347 = DIRECTION ( 'NONE',  ( -1.000000000000000000, 0.000000000000000000, 0.000000000000000000 ) ) ;
#45348 = CARTESIAN_POINT ( 'NONE',  ( 35.00000000000000000, 4.705694406421931860E-17, -3.469127814946512892E-15 ) ) ;
#45349 = VERTEX_POINT ( 'NONE', #56601 ) ;
#45350 = VERTEX_POINT ( 'NONE', #11042 ) ;
#45351 = ORIENTED_EDGE ( 'NONE', *, *, #31405, .F. ) ;
#45352 = EDGE_CURVE ( 'NONE', #45530, #38028, #20354, .T. ) ;
#45353 = VECTOR ( 'NONE', #8655, 1000.000000000000000 ) ;
#45354 = ORIENTED_EDGE ( 'NONE', *, *, #14834, .T. ) ;
#45355 = EDGE_CURVE ( 'NONE', #23572, #29673, #9221, .T. ) ;
#45356 = CARTESIAN_POINT ( 'NONE',  ( -8.891032880924177206, -11.36194426013948444, -3.860857758255646921 ) ) ;
#45357 = CARTESIAN_POINT ( 'NONE',  ( -35.04709527796842394, 0.01231589140598780829, 0.001082316405371860912 ) ) ;
#45358 = CYLINDRICAL_SURFACE ( 'NONE', #64083, 4.999999999999999112 ) ;
#45359 = CARTESIAN_POINT ( 'NONE',  ( -22.49803948133827447, -2.269619744675244188, -3.704553751086701485 ) ) ;
#45360 = CARTESIAN_POINT ( 'NONE',  ( 0.3610902822527242151, -10.76187877352508870, -5.910495176556292307 ) ) ;
#45361 = CARTESIAN_POINT ( 'NONE',  ( 23.97866493766117557, 2.287510638894525883, -13.30844455837636886 ) ) ;
#45363 = ORIENTED_EDGE ( 'NONE', *, *, #57427, .T. ) ;
#45362 = CARTESIAN_POINT ( 'NONE',  ( 2.305787727787084407, -1.493241775258372872, -7.508843116234172221 ) ) ;
#45364 = ADVANCED_FACE ( 'NONE', ( #50634 ), #45302, .T. ) ;
#45365 = DIRECTION ( 'NONE',  ( -0.7886918350401329603, -0.6147887355352468219, 0.000000000000000000 ) ) ;
#45366 = ORIENTED_EDGE ( 'NONE', *, *, #44325, .T. ) ;
#45367 = DIRECTION ( 'NONE',  ( 0.000000000000000000, -0.01356324068817992175, 0.9999080150203990547 ) ) ;
#45368 = VERTEX_POINT ( 'NONE', #60589 ) ;
#45369 = ORIENTED_EDGE ( 'NONE', *, *, #63398, .F. ) ;
#45370 = CARTESIAN_POINT ( 'NONE',  ( 0.3106921474978561748, 9.542334142800575236, -7.699584408545789849 ) ) ;
#45371 = CARTESIAN_POINT ( 'NONE',  ( 8.372133460183182052, -31.76502814486162407, 13.66429824708607477 ) ) ;
#45372 = FACE_OUTER_BOUND ( 'NONE', #17789, .T. ) ;
#45373 = DIRECTION ( 'NONE',  ( -0.9688695217174486674, 0.000000000000000000, -0.2475719085175094036 ) ) ;
#45374 = EDGE_CURVE ( 'NONE', #46293, #25983, #12401, .T. ) ;
#45375 = CARTESIAN_POINT ( 'NONE',  ( -19.80028988669405976, 11.89697986174693511, -1.598264803601076478 ) ) ;
#45376 = CARTESIAN_POINT ( 'NONE',  ( 36.00000000000000711, 1.113475361586665491, 12.70128625845191195 ) ) ;
#45377 = ORIENTED_EDGE ( 'NONE', *, *, #39564, .F. ) ;
#45378 = ORIENTED_EDGE ( 'NONE', *, *, #39999, .F. ) ;
#45379 = CARTESIAN_POINT ( 'NONE',  ( 47.00000000000000711, 4.705694406421931860E-17, -3.469127814946512892E-15 ) ) ;
#45380 = ORIENTED_EDGE ( 'NONE', *, *, #21921, .F. ) ;
#45381 = EDGE_LOOP ( 'NONE', ( #34081, #14963, #40492, #43402 ) ) ;
#45382 = CYLINDRICAL_SURFACE ( 'NONE', #8362, 13.50000000000000178 ) ;
#45383 = CARTESIAN_POINT ( 'NONE',  ( 0.3632410797595246321, 10.49990774419911155, -6.365652464380801234 ) ) ;
#45384 = CARTESIAN_POINT ( 'NONE',  ( -22.30398854582848145, 0.8844201765542331062, -3.656532484463044241 ) ) ;
#45385 = CARTESIAN_POINT ( 'NONE',  ( 2.000000000000001776, 5.860254403322073813, -3.474373880649762381 ) ) ;
#45386 = CARTESIAN_POINT ( 'NONE',  ( 1.719304012338199517, 12.20344780065974888, 3.626341562670754914 ) ) ;
#45387 = AXIS2_PLACEMENT_3D ( 'NONE', #27702, #48352, #3459 ) ;
#45388 = DIRECTION ( 'NONE',  ( 0.000000000000000000, -0.01356324068817998940, 0.9999080150203990547 ) ) ;
#45389 = CARTESIAN_POINT ( 'NONE',  ( 35.00000000000000000, 11.29812557209481483, 3.213188559034117819 ) ) ;
#45390 = EDGE_CURVE ( 'NONE', #39365, #24342, #57340, .T. ) ;
#45391 = ORIENTED_EDGE ( 'NONE', *, *, #14672, .F. ) ;
#45392 = ORIENTED_EDGE ( 'NONE', *, *, #34213, .F. ) ;
#45393 = CARTESIAN_POINT ( 'NONE',  ( 2.000000000000001776, -5.860254403322033845, 3.474373880649773039 ) ) ;
#45394 = DIRECTION ( 'NONE',  ( -1.000000000000000000, -0.000000000000000000, 0.000000000000000000 ) ) ;
#45395 = AXIS2_PLACEMENT_3D ( 'NONE', #47452, #62710, #7517 ) ;
#45396 = CARTESIAN_POINT ( 'NONE',  ( -37.00000000000000711, -9.506317355798310942, -8.496612874013262484 ) ) ;
#45397 = B_SPLINE_CURVE_WITH_KNOTS ( 'NONE', 3,
 ( #12588, #13893, #8931, #23241, #23580, #38190, #18270, #34186, #54494, #63149, #63784, #43184, #64133, #47862, #43502, #17615, #2321, #53177 ),
 .UNSPECIFIED., .F., .F.,
 ( 4, 2, 2, 2, 2, 2, 2, 2, 4 ),
 ( 0.000000000000000000, 0.001482986184832410168, 0.002965972369664820335, 0.004448958554497230503, 0.005931944739329640670, 0.007414930924162050838, 0.008897917108994461005, 0.01038090329382687117, 0.01186388947865928134 ),
 .UNSPECIFIED. ) ;
#45398 = CARTESIAN_POINT ( 'NONE',  ( 35.00000000000000000, 6.711949091238142984, -10.84030624090608974 ) ) ;
#45399 = CARTESIAN_POINT ( 'NONE',  ( 3.459614771489464946, -11.09853614738469396, 4.563167253695070258 ) ) ;
#45400 = CIRCLE ( 'NONE', #16730, 2.899999999999994582 ) ;
#45401 = CARTESIAN_POINT ( 'NONE',  ( 37.00000000000000711, 11.91791701451269958, 2.544412758415708353 ) ) ;
#45402 = DIRECTION ( 'NONE',  ( 0.000000000000000000, -0.4134677391718577510, -0.9105187689795923855 ) ) ;
#45403 = CARTESIAN_POINT ( 'NONE',  ( -27.08419797710328680, -2.125717714519619328, -0.8552720754637029854 ) ) ;
#45404 = ADVANCED_FACE ( 'NONE', ( #36634 ), #65561, .T. ) ;
#45405 = ORIENTED_EDGE ( 'NONE', *, *, #36524, .F. ) ;
#45406 = CARTESIAN_POINT ( 'NONE',  ( 2.639814597422739162, -0.2564041122425642083, 7.763021810282391577 ) ) ;
#45407 = CARTESIAN_POINT ( 'NONE',  ( 0.3665391374699472626, 10.50279796150445577, -6.368473106897019953 ) ) ;
#45408 = CYLINDRICAL_SURFACE ( 'NONE', #4689, 14.99999999999998757 ) ;
#45409 = EDGE_CURVE ( 'NONE', #31390, #57924, #33642, .T. ) ;
#45410 = DIRECTION ( 'NONE',  ( 0.000000000000000000, -0.01356324068818000328, 0.9999080150203990547 ) ) ;
#45411 = CARTESIAN_POINT ( 'NONE',  ( 5.516018279890452902, -0.004525000489649900863, 0.005042957932159117078 ) ) ;
#45412 = VERTEX_POINT ( 'NONE', #55622 ) ;
#45413 = CARTESIAN_POINT ( 'NONE',  ( 2.241509619876138171, -3.784042210004660678, -6.630717740088888590 ) ) ;
#45414 = LINE ( 'NONE', #46100, #39678 ) ;
#45415 = CARTESIAN_POINT ( 'NONE',  ( 8.088853370213684002, -28.65367229866794219, -10.33367282332731385 ) ) ;
#45416 = ORIENTED_EDGE ( 'NONE', *, *, #54054, .T. ) ;
#45417 = DIRECTION ( 'NONE',  ( 1.000000000000000000, 0.000000000000000000, 0.000000000000000000 ) ) ;
#45418 = CARTESIAN_POINT ( 'NONE',  ( -22.31328051695926007, 3.781397440874590732, -0.2528478350593763024 ) ) ;
#45419 = CARTESIAN_POINT ( 'NONE',  ( 35.00000000000000000, 11.17622378668006355, -3.614449339633533764 ) ) ;
#45420 = B_SPLINE_CURVE_WITH_KNOTS ( 'NONE', 3,
 ( #42089, #47442, #42405, #17166, #52753, #21161, #7178, #31154, #27458, #47757, #15831, #36110, #5912, #26169, #41433, #36467, #38089, #55274, #58395, #17824, #7861, #12821, #18158, #9715, #4771, #33107 ),
 .UNSPECIFIED., .F., .F.,
 ( 4, 2, 2, 2, 2, 2, 2, 2, 2, 2, 2, 2, 4 ),
 ( 0.000000000000000000, 0.002656797653146665897, 0.003320997066433334973, 0.003985196479720003182, 0.005313595306293336130, 0.005977794719579998702, 0.006641994132866661273, 0.007306193546153324711, 0.007970392959439987282, 0.008634592372726649853, 0.009298791786013312424, 0.009962991199299976730, 0.01062719061258663930 ),
 .UNSPECIFIED. ) ;
#45422 = ORIENTED_EDGE ( 'NONE', *, *, #11622, .T. ) ;
#45421 = DIRECTION ( 'NONE',  ( 1.000000000000000000, 0.000000000000000000, 0.000000000000000000 ) ) ;
#45423 = CARTESIAN_POINT ( 'NONE',  ( -27.10307689719060420, 2.283215755731188068, 0.5470785519252191476 ) ) ;
#45424 = EDGE_CURVE ( 'NONE', #54776, #55347, #38960, .T. ) ;
#45425 = AXIS2_PLACEMENT_3D ( 'NONE', #24438, #38431, #44715 ) ;
#45426 = CARTESIAN_POINT ( 'NONE',  ( 2.907497136250727365, -7.497839665536855769, -2.346692756478276021 ) ) ;
#45427 = ORIENTED_EDGE ( 'NONE', *, *, #832, .F. ) ;
#45428 = CARTESIAN_POINT ( 'NONE',  ( 0.2648978790185584908, 7.769924372105204036, 9.465406350830633642 ) ) ;
#45429 = FACE_OUTER_BOUND ( 'NONE', #31341, .T. ) ;
#45430 = AXIS2_PLACEMENT_3D ( 'NONE', #22047, #17056, #6121 ) ;
#45431 = CARTESIAN_POINT ( 'NONE',  ( -22.00000000000000711, -20.00000000000000000, 2.449293598294706907E-15 ) ) ;
#45432 = DIRECTION ( 'NONE',  ( 1.000000000000000000, 0.000000000000000000, 0.000000000000000000 ) ) ;
#45433 =( BOUNDED_SURFACE ( )  B_SPLINE_SURFACE ( 3, 1, ( 
 ( #39517, #35511 ),
 ( #50815, #34199 ),
 ( #19249, #45480 ),
 ( #4282, #59481 ) ),
 .UNSPECIFIED., .F., .F., .F. ) 
 B_SPLINE_SURFACE_WITH_KNOTS ( ( 4, 4 ),
 ( 2, 2 ),
 ( 0.000000000000000000, 1.000000000000000000 ),
 ( 0.000000000000000000, 1.000000000000000000 ),
 .UNSPECIFIED. ) 
 GEOMETRIC_REPRESENTATION_ITEM ( )  RATIONAL_B_SPLINE_SURFACE ( (
 ( 1.000000000000000000, 1.000000000000000000),
 ( 0.9942764183789327692, 0.8450855930916580938),
 ( 0.9942764183789327692, 0.8450855930916580938),
 ( 1.000000000000000000, 1.000000000000000000) ) ) 
 REPRESENTATION_ITEM ( '' )  SURFACE ( )  );
#45434 = CARTESIAN_POINT ( 'NONE',  ( 0.3218525148189834151, -11.43947393562873849, -4.423735011438943765 ) ) ;
#45435 = CARTESIAN_POINT ( 'NONE',  ( -11.40165637462999904, -7.508992741355383416, 11.21895841913464409 ) ) ;
#45436 = CARTESIAN_POINT ( 'NONE',  ( 2.266490820341529044, 1.183790889243382383, -7.550546162186090982 ) ) ;
#45437 = VECTOR ( 'NONE', #33027, 1000.000000000000000 ) ;
#45438 = ORIENTED_EDGE ( 'NONE', *, *, #5390, .T. ) ;
#45439 = CARTESIAN_POINT ( 'NONE',  ( -35.00000000000000000, 0.000000000000000000, 0.000000000000000000 ) ) ;
#45440 = ORIENTED_EDGE ( 'NONE', *, *, #5069, .T. ) ;
#45441 = CIRCLE ( 'NONE', #57142, 12.74999999999999822 ) ;
#45442 = EDGE_CURVE ( 'NONE', #11288, #60004, #45967, .T. ) ;
#45443 = LINE ( 'NONE', #55096, #8823 ) ;
#45444 = CYLINDRICAL_SURFACE ( 'NONE', #51094, 12.74999999999999822 ) ;
#45445 = VERTEX_POINT ( 'NONE', #61902 ) ;
#45446 = CARTESIAN_POINT ( 'NONE',  ( -35.00000000000000000, 8.052525312710004712, -8.551552972816995890 ) ) ;
#45447 = CARTESIAN_POINT ( 'NONE',  ( 9.975240977089113059, 11.94374578141113119, -1.164188000379794419 ) ) ;
#45448 = CARTESIAN_POINT ( 'NONE',  ( 36.00000000000000711, 1.908798535168558352, 12.60630747491660486 ) ) ;
#45449 = EDGE_LOOP ( 'NONE', ( #166, #63193, #39742, #9533 ) ) ;
#45450 = ORIENTED_EDGE ( 'NONE', *, *, #13034, .F. ) ;
#45451 = DIRECTION ( 'NONE',  ( 0.000000000000000000, 0.7790879021242486102, -0.6269146997508011632 ) ) ;
#45452 = ORIENTED_EDGE ( 'NONE', *, *, #23280, .T. ) ;
#45453 = CARTESIAN_POINT ( 'NONE',  ( 22.12621674078617318, -11.11704163603532081, -4.533068918720905671 ) ) ;
#45454 = DIRECTION ( 'NONE',  ( -1.000000000000000000, 0.000000000000000000, 0.000000000000000000 ) ) ;
#45455 = B_SPLINE_CURVE_WITH_KNOTS ( 'NONE', 3,
 ( #31272, #57203, #40919, #30927, #36902, #21949, #36585, #51574, #50899, #26936, #47236, #46556, #62180, #5349, #1350, #1013, #56888, #21279, #11313, #25963, #41555, #11629, #20947, #1683, #31899, #31580, #16632, #51888, #690, #15315, #52221, #41225, #35591, #6332, #46248, #26598, #46890, #10316, #38545, #42872, #63160, #63797, #17626, #27921, #53188, #48229 ),
 .UNSPECIFIED., .F., .F.,
 ( 4, 2, 2, 2, 2, 2, 2, 2, 2, 2, 2, 2, 2, 2, 2, 2, 2, 2, 2, 2, 2, 2, 4 ),
 ( 0.000000000000000000, 0.001519118309396224427, 0.003038236618792448853, 0.004557354928188673063, 0.006076473237584897706, 0.009114709856377337452, 0.01215294647516977807, 0.01519118309396221868, 0.01822941971275466103, 0.01974853802215088133, 0.02126765633154709817, 0.02430589295033953531, 0.02582501125973575562, 0.02734412956913197593, 0.03038236618792440960, 0.03342060280671684674, 0.03645883942550928736, 0.03949707604430172797, 0.04101619435369794481, 0.04253531266309416164, 0.04405443097249037848, 0.04557354928188660226, 0.04861178590067902899 ),
 .UNSPECIFIED. ) ;
#45456 = CARTESIAN_POINT ( 'NONE',  ( -27.08456565417852246, 2.282055114149009967, -0.2166646653333907935 ) ) ;
#45457 = DIRECTION ( 'NONE',  ( 0.000000000000000000, 0.8515178078024887576, -0.5243256840888532722 ) ) ;
#45458 = DIRECTION ( 'NONE',  ( 1.000000000000000000, 0.000000000000000000, -0.000000000000000000 ) ) ;
#45459 = CARTESIAN_POINT ( 'NONE',  ( 0.2653519991613820794, -10.61652626436032953, 6.104031847944984435 ) ) ;
#45460 = CARTESIAN_POINT ( 'NONE',  ( -27.08429572838383947, -0.9410937941433956677, 2.089332284968712816 ) ) ;
#45461 = EDGE_CURVE ( 'NONE', #58933, #58366, #35743, .T. ) ;
#45462 = EDGE_LOOP ( 'NONE', ( #47614, #47919, #27152, #42824 ) ) ;
#45463 = CARTESIAN_POINT ( 'NONE',  ( 0.9296196016834894493, -11.85136013469028704, 3.871279966919827675 ) ) ;
#45464 = EDGE_CURVE ( 'NONE', #47167, #57461, #61246, .T. ) ;
#45465 = DIRECTION ( 'NONE',  ( -1.000000000000000000, -0.000000000000000000, 0.000000000000000000 ) ) ;
#45466 = CARTESIAN_POINT ( 'NONE',  ( 11.35368172282957033, 13.35992779450903711, -1.943390003085933015 ) ) ;
#45467 = CARTESIAN_POINT ( 'NONE',  ( -35.00000000000000000, -3.093009498344009955, 11.78745411414838884 ) ) ;
#45468 = CARTESIAN_POINT ( 'NONE',  ( 8.437200413559441614, 4.476360154859203355, 25.00000000000000000 ) ) ;
#45469 = FACE_OUTER_BOUND ( 'NONE', #6639, .T. ) ;
#45470 = CARTESIAN_POINT ( 'NONE',  ( -28.67667724226168602, -1.840944188131431236, -0.4371157725390102389 ) ) ;
#45471 = CIRCLE ( 'NONE', #10444, 5.000000000000000000 ) ;
#45472 = EDGE_LOOP ( 'NONE', ( #39900, #46925, #58415, #7167 ) ) ;
#45473 = EDGE_CURVE ( 'NONE', #50294, #3168, #15674, .T. ) ;
#45474 = DIRECTION ( 'NONE',  ( 0.000000000000000000, 0.7621620551276333533, 0.6473862847818311339 ) ) ;
#45475 = AXIS2_PLACEMENT_3D ( 'NONE', #58873, #19259, #33572 ) ;
#45476 = CIRCLE ( 'NONE', #923, 7.499999999999988454 ) ;
#45477 = EDGE_LOOP ( 'NONE', ( #56322, #49158, #60274, #15748 ) ) ;
#45478 = DIRECTION ( 'NONE',  ( -1.000000000000000000, -0.000000000000000000, 0.000000000000000000 ) ) ;
#45479 = CARTESIAN_POINT ( 'NONE',  ( 35.00000000000000000, 7.882940143791773657, -10.02106554660711524 ) ) ;
#45480 = CARTESIAN_POINT ( 'NONE',  ( 0.3040950598368144520, 11.43390362554253237, 4.428852722102769590 ) ) ;
#45481 = AXIS2_PLACEMENT_3D ( 'NONE', #35885, #56184, #4355 ) ;
#45482 = CARTESIAN_POINT ( 'NONE',  ( 2.969415267404351244, -7.815364626283974658, -0.9841783286031883238 ) ) ;
#45483 = LINE ( 'NONE', #286, #36052 ) ;
#45484 = EDGE_CURVE ( 'NONE', #18262, #30237, #48512, .T. ) ;
#45485 = ORIENTED_EDGE ( 'NONE', *, *, #30998, .T. ) ;
#45486 = CARTESIAN_POINT ( 'NONE',  ( 37.00000000000000711, 11.65150730582934635, 1.488153103997001514 ) ) ;
#45487 = CARTESIAN_POINT ( 'NONE',  ( 2.247112776671466694, -3.716786765232484857, 6.670755883245758966 ) ) ;
#45488 = DIRECTION ( 'NONE',  ( 0.000000000000000000, 0.6269146997507929475, 0.7790879021242551605 ) ) ;
#45489 = CIRCLE ( 'NONE', #44429, 12.18650000000000055 ) ;
#45490 = CARTESIAN_POINT ( 'NONE',  ( 2.241449424704146320, -6.642105568284079276, -3.763973574060608840 ) ) ;
#45491 = CARTESIAN_POINT ( 'NONE',  ( 8.948006322247541888, 4.815211251969169659, -12.61333397820095570 ) ) ;
#45492 = DIRECTION ( 'NONE',  ( -0.9606638835031803270, -0.07465901992591204850, 0.2674900627617601279 ) ) ;
#45493 = VERTEX_POINT ( 'NONE', #26652 ) ;
#45494 = CARTESIAN_POINT ( 'NONE',  ( -27.10113028276155944, -0.5479825692848022678, 2.276991616290404696 ) ) ;
#45495 = EDGE_LOOP ( 'NONE', ( #9372, #61316, #7336, #49697 ) ) ;
#45496 = DIRECTION ( 'NONE',  ( 0.000000000000000000, 0.3807014730195220631, -0.9246979985058721985 ) ) ;
#45497 = DIRECTION ( 'NONE',  ( 0.000000000000000000, 0.3807014730195152907, -0.9246979985058750851 ) ) ;
#45498 = B_SPLINE_CURVE_WITH_KNOTS ( 'NONE', 3,
 ( #43356, #2836, #63631, #3156, #18106, #23418, #43692, #3495, #13748, #63980, #18461, #38716, #59018, #23768, #13431, #54010, #59988, #44338, #60297, #20393, #65592, #64946, #64614, #60968 ),
 .UNSPECIFIED., .F., .F.,
 ( 4, 2, 2, 2, 2, 2, 2, 2, 2, 2, 2, 4 ),
 ( 0.002913801881037346962, 0.003520887530297034471, 0.004127973179556721980, 0.005342144478076094397, 0.006556315776595466813, 0.007163401425855153888, 0.007770487075114840096, 0.008984658373634213380, 0.009591744022893901322, 0.01019882967215358580, 0.01141300097067296168, 0.01262717226919233410 ),
 .UNSPECIFIED. ) ;
#45499 = CARTESIAN_POINT ( 'NONE',  ( 47.00000000000000711, 4.705694406421931860E-17, -3.469127814946512892E-15 ) ) ;
#45500 = DIRECTION ( 'NONE',  ( 0.000000000000000000, 0.000000000000000000, -1.000000000000000000 ) ) ;
#45501 = CIRCLE ( 'NONE', #60363, 19.99999999999999645 ) ;
#45502 = VERTEX_POINT ( 'NONE', #7692 ) ;
#45503 = EDGE_LOOP ( 'NONE', ( #47760, #1093, #9161, #63764 ) ) ;
#45504 = CARTESIAN_POINT ( 'NONE',  ( 0.2646305136544072623, 7.770320294339302158, -9.465888453932885582 ) ) ;
#45505 = ORIENTED_EDGE ( 'NONE', *, *, #29588, .T. ) ;
#45506 = CARTESIAN_POINT ( 'NONE',  ( -35.00000000000000000, 0.000000000000000000, 0.000000000000000000 ) ) ;
#45507 = DIRECTION ( 'NONE',  ( 1.000000000000000000, 0.000000000000000000, -0.000000000000000000 ) ) ;
#45508 = CARTESIAN_POINT ( 'NONE',  ( -22.27722019094931127, -3.463038365117174333, -1.249795790945215312 ) ) ;
#45509 = CARTESIAN_POINT ( 'NONE',  ( 0.7446945582506564465, 9.270687147117307347, 8.243982823408627425 ) ) ;
#45511 = DIRECTION ( 'NONE',  ( 1.000000000000000000, 0.000000000000000000, -0.000000000000000000 ) ) ;
#45510 = CIRCLE ( 'NONE', #16848, 12.75000000000000178 ) ;
#45512 = CARTESIAN_POINT ( 'NONE',  ( -27.78468958554971380, 25.00000000000000000, 8.565911087387465983 ) ) ;
#45513 = DIRECTION ( 'NONE',  ( -1.000000000000000000, 0.000000000000000000, 0.000000000000000000 ) ) ;
#45514 = ORIENTED_EDGE ( 'NONE', *, *, #48710, .T. ) ;
#45515 = CARTESIAN_POINT ( 'NONE',  ( -8.957233933390911673, -8.874460928901493517, -8.086001677246498431 ) ) ;
#45516 = ORIENTED_EDGE ( 'NONE', *, *, #45086, .T. ) ;
#45517 = CARTESIAN_POINT ( 'NONE',  ( -35.05175862995318425, 0.003178856583447783879, -0.01216930940959627672 ) ) ;
#45518 = CIRCLE ( 'NONE', #64634, 5.000000000000000888 ) ;
#45519 = EDGE_CURVE ( 'NONE', #36643, #52670, #43167, .T. ) ;
#45520 = CARTESIAN_POINT ( 'NONE',  ( -27.10128162969832388, 1.945744751330104272, -1.304299867634916010 ) ) ;
#45521 = ORIENTED_EDGE ( 'NONE', *, *, #775, .T. ) ;
#45522 = PLANE ( 'NONE',  #11919 ) ;
#45524 = EDGE_LOOP ( 'NONE', ( #64194, #6953, #18401, #25354 ) ) ;
#45523 = VECTOR ( 'NONE', #48788, 1000.000000000000000 ) ;
#45525 = VECTOR ( 'NONE', #23641, 1000.000000000000000 ) ;
#45526 = CARTESIAN_POINT ( 'NONE',  ( 35.00000000000000000, -5.865551165830998670, 11.32068061209301035 ) ) ;
#45527 = DIRECTION ( 'NONE',  ( 1.000000000000000000, 0.000000000000000000, -0.000000000000000000 ) ) ;
#45528 = CARTESIAN_POINT ( 'NONE',  ( 16.94760237393649405, 10.49682181221983157, 5.815268149447246238 ) ) ;
#45529 = CARTESIAN_POINT ( 'NONE',  ( 2.524535260912363466, 7.184101064217870203, -2.850096701925667109 ) ) ;
#45530 = VERTEX_POINT ( 'NONE', #2040 ) ;
#45531 = VERTEX_POINT ( 'NONE', #32934 ) ;
#45532 = AXIS2_PLACEMENT_3D ( 'NONE', #43845, #54152, #63144 ) ;
#45533 = DIRECTION ( 'NONE',  ( -1.000000000000000000, 0.000000000000000000, 0.000000000000000000 ) ) ;
#45534 = ORIENTED_EDGE ( 'NONE', *, *, #23413, .T. ) ;
#45535 = FACE_OUTER_BOUND ( 'NONE', #59966, .T. ) ;
#45536 = ORIENTED_EDGE ( 'NONE', *, *, #35759, .F. ) ;
#45537 = ORIENTED_EDGE ( 'NONE', *, *, #1259, .T. ) ;
#45538 = VECTOR ( 'NONE', #40742, 1000.000000000000000 ) ;
#45539 = ORIENTED_EDGE ( 'NONE', *, *, #11173, .F. ) ;
#45540 = CARTESIAN_POINT ( 'NONE',  ( 2.305787727787084407, -5.756228004061490822, 5.047606869483037606 ) ) ;
#45541 = CARTESIAN_POINT ( 'NONE',  ( 1.375507693217066008, 11.64019206974653642, 4.865932489130583072 ) ) ;
#45542 = EDGE_CURVE ( 'NONE', #52056, #64815, #20906, .T. ) ;
#45543 = CARTESIAN_POINT ( 'NONE',  ( 3.047904605210430162, -0.9519317672906252303, -7.845751380824991017 ) ) ;
#45544 = DIRECTION ( 'NONE',  ( 0.000000000000000000, -0.1387779952735677669, 0.9903235168508569553 ) ) ;
#45545 = CARTESIAN_POINT ( 'NONE',  ( -35.00000000000000000, 0.2661492558805056974, -12.18359334611896116 ) ) ;
#45546 = EDGE_LOOP ( 'NONE', ( #6734, #6928, #43915, #57119 ) ) ;
#45547 = CARTESIAN_POINT ( 'NONE',  ( 2.276198483116796289, -2.469789406312446811, -7.236140649716140238 ) ) ;
#45548 = ORIENTED_EDGE ( 'NONE', *, *, #54696, .T. ) ;
#45549 = DIRECTION ( 'NONE',  ( -0.000000000000000000, -0.000000000000000000, -1.000000000000000000 ) ) ;
#45550 = EDGE_CURVE ( 'NONE', #31183, #21600, #7100, .T. ) ;
#45551 = DIRECTION ( 'NONE',  ( -1.000000000000000000, 0.000000000000000000, 0.000000000000000000 ) ) ;
#45552 = EDGE_CURVE ( 'NONE', #16066, #16210, #23019, .T. ) ;
#45553 = ORIENTED_EDGE ( 'NONE', *, *, #48710, .F. ) ;
#45554 = CARTESIAN_POINT ( 'NONE',  ( 0.3218525148189824159, -10.74192973049792066, 5.919623386703301904 ) ) ;
#45555 = CARTESIAN_POINT ( 'NONE',  ( 0.3675815128205894289, 7.689697408877401941, -9.574637318041888889 ) ) ;
#45556 = CARTESIAN_POINT ( 'NONE',  ( -25.54417658651491863, 25.00000000000000000, 11.22596262356930197 ) ) ;
#45557 = AXIS2_PLACEMENT_3D ( 'NONE', #18507, #28772, #33444 ) ;
#45558 = ORIENTED_EDGE ( 'NONE', *, *, #34472, .F. ) ;
#45559 = EDGE_CURVE ( 'NONE', #8013, #40304, #42576, .T. ) ;
#45560 = CARTESIAN_POINT ( 'NONE',  ( 2.260457164927186291, -7.639515169785726201, 0.1384509728648797844 ) ) ;
#45561 = CIRCLE ( 'NONE', #32826, 12.75000000000000178 ) ;
#45562 = VERTEX_POINT ( 'NONE', #63525 ) ;
#45563 = EDGE_CURVE ( 'NONE', #33980, #5232, #50652, .T. ) ;
#45564 = DIRECTION ( 'NONE',  ( 0.000000000000000000, -1.000000000000000000, 0.000000000000000000 ) ) ;
#45565 = CARTESIAN_POINT ( 'NONE',  ( 0.5547464869798253151, 9.648168635481845001, 7.697709668896102642 ) ) ;
#45566 = CARTESIAN_POINT ( 'NONE',  ( 2.373367633546870525, 6.738274194514266568, -3.681545031436583848 ) ) ;
#45567 = CARTESIAN_POINT ( 'NONE',  ( -35.00000000000000000, 0.000000000000000000, 0.000000000000000000 ) ) ;
#45568 = CARTESIAN_POINT ( 'NONE',  ( 2.241449424704146320, 7.528892370271791812, 1.265244293929113972 ) ) ;
#45569 = ORIENTED_EDGE ( 'NONE', *, *, #22499, .F. ) ;
#45570 = LINE ( 'NONE', #8130, #42993 ) ;
#45571 = CARTESIAN_POINT ( 'NONE',  ( 1.194176325881334710, 5.827386336993033211, -11.12159247766666326 ) ) ;
#45572 = LINE ( 'NONE', #29613, #24741 ) ;
#45573 = CARTESIAN_POINT ( 'NONE',  ( 2.305787727787083519, 3.682701754025512919, 6.711944854845837583 ) ) ;
#45574 = VECTOR ( 'NONE', #28830, 1000.000000000000227 ) ;
#45575 = AXIS2_PLACEMENT_3D ( 'NONE', #41501, #35846, #644 ) ;
#45576 = B_SPLINE_CURVE_WITH_KNOTS ( 'NONE', 3,
 ( #58292, #53305, #48335, #43302, #18052, #58636, #33344, #50291 ),
 .UNSPECIFIED., .F., .F.,
 ( 4, 2, 2, 4 ),
 ( 0.000000000000000000, 0.001617793918133567837, 0.002426690877200354032, 0.003235587836267140010 ),
 .UNSPECIFIED. ) ;
#45577 = EDGE_CURVE ( 'NONE', #54027, #27642, #62226, .T. ) ;
#45578 = AXIS2_PLACEMENT_3D ( 'NONE', #49846, #59183, #55152 ) ;
#45579 = CARTESIAN_POINT ( 'NONE',  ( 0.3057689695767519256, -12.11137787899270002, -1.901059295891038836 ) ) ;
#45580 = EDGE_CURVE ( 'NONE', #50423, #33155, #42246, .T. ) ;
#45581 = CARTESIAN_POINT ( 'NONE',  ( -35.00000000000000000, -10.99909370905153594, -5.246972444134134328 ) ) ;
#45582 = CARTESIAN_POINT ( 'NONE',  ( 2.244591118396555451, -5.917635828475942716, -4.825158615932966910 ) ) ;
#45583 = DIRECTION ( 'NONE',  ( 0.000000000000000000, -0.01356324068817999114, 0.9999080150203989437 ) ) ;
#45584 = CARTESIAN_POINT ( 'NONE',  ( 2.941278708680199916, 0.1348063076487806822, -6.138172921908579660 ) ) ;
#45585 = VECTOR ( 'NONE', #45992, 1000.000000000000000 ) ;
#45586 = EDGE_LOOP ( 'NONE', ( #32038, #4066, #54552, #46164 ) ) ;
#45587 = EDGE_LOOP ( 'NONE', ( #9299, #16721, #44095, #54632, #5575, #52193, #55360 ) ) ;
#45588 = DIRECTION ( 'NONE',  ( 1.000000000000000000, -0.000000000000000000, -0.000000000000000000 ) ) ;
#45589 = FACE_OUTER_BOUND ( 'NONE', #5073, .T. ) ;
#45590 = DIRECTION ( 'NONE',  ( -0.000000000000000000, -0.000000000000000000, -1.000000000000000000 ) ) ;
#45591 = CARTESIAN_POINT ( 'NONE',  ( 35.00000000000000000, -5.130401251914806338, -11.05394794832827898 ) ) ;
#45592 = ORIENTED_EDGE ( 'NONE', *, *, #57172, .F. ) ;
#45593 = VERTEX_POINT ( 'NONE', #57588 ) ;
#45594 = EDGE_LOOP ( 'NONE', ( #64948, #15652, #51846, #2325 ) ) ;
#45595 = CARTESIAN_POINT ( 'NONE',  ( -27.10719052120871098, 2.355164825213508450, -0.1538293304135275597 ) ) ;
#45596 = EDGE_CURVE ( 'NONE', #33067, #26019, #1801, .T. ) ;
#45597 = CARTESIAN_POINT ( 'NONE',  ( -22.27716857039623477, 0.8090275962000628152, 3.591587580807983127 ) ) ;
#45598 = B_SPLINE_CURVE_WITH_KNOTS ( 'NONE', 3,
 ( #18403, #12716, #28040, #53647, #7757, #8087, #48652 ),
 .UNSPECIFIED., .F., .F.,
 ( 4, 3, 4 ),
 ( 0.000000000000000000, 0.001700533616330600437, 0.005002426799370906195 ),
 .UNSPECIFIED. ) ;
#45599 = ORIENTED_EDGE ( 'NONE', *, *, #30332, .F. ) ;
#45600 = CARTESIAN_POINT ( 'NONE',  ( 2.305787727787085295, -7.249469779319927198, 2.461236246751046242 ) ) ;
#45601 = DIRECTION ( 'NONE',  ( 0.000000000000000000, -1.000000000000000000, 0.000000000000000000 ) ) ;
#45602 = DIRECTION ( 'NONE',  ( 0.000000000000000000, 0.01356324068817998940, -0.9999080150203989437 ) ) ;
#45603 = ORIENTED_EDGE ( 'NONE', *, *, #40930, .T. ) ;
#45604 = DIRECTION ( 'NONE',  ( 0.000000000000000000, -0.3554799084908832896, -0.9346839223284592046 ) ) ;
#45605 = CIRCLE ( 'NONE', #12700, 7.499999999999988454 ) ;
#45606 = CARTESIAN_POINT ( 'NONE',  ( -6.246056400524260255, -31.23659747722423319, -14.42616998329098799 ) ) ;
#45607 = CARTESIAN_POINT ( 'NONE',  ( 37.00000000000000711, -10.25474254703957477, -6.584150480049516752 ) ) ;
#45608 = ORIENTED_EDGE ( 'NONE', *, *, #62381, .T. ) ;
#45609 = CYLINDRICAL_SURFACE ( 'NONE', #35269, 5.000000000000000888 ) ;
#45610 = EDGE_LOOP ( 'NONE', ( #53465, #62266, #53713, #39600 ) ) ;
#45611 = CARTESIAN_POINT ( 'NONE',  ( 0.3164563675027652345, -6.338687639235967453, -10.49799587805937229 ) ) ;
#45612 = ADVANCED_FACE ( 'NONE', ( #7029 ), #52276, .T. ) ;
#45613 = EDGE_LOOP ( 'NONE', ( #34728, #24670, #12944, #18642 ) ) ;
#45614 = CARTESIAN_POINT ( 'NONE',  ( 2.080613030138688480, 3.872983346207417021, 1.000000000000000000 ) ) ;
#45615 = LINE ( 'NONE', #55619, #25544 ) ;
#45616 = CIRCLE ( 'NONE', #10577, 2.899999999999994582 ) ;
#45617 = CARTESIAN_POINT ( 'NONE',  ( -0.8753493882091067935, -31.04850208196501526, 14.43082775300658938 ) ) ;
#45618 = DIRECTION ( 'NONE',  ( -1.000000000000000000, 0.000000000000000000, 0.000000000000000000 ) ) ;
#45619 = DIRECTION ( 'NONE',  ( 0.000000000000000000, 0.01356324068817298112, -0.9999080150203990547 ) ) ;
#45620 = DIRECTION ( 'NONE',  ( -1.000000000000000000, 0.000000000000000000, 0.000000000000000000 ) ) ;
#45621 = EDGE_CURVE ( 'NONE', #95, #6107, #17343, .T. ) ;
#45622 = CARTESIAN_POINT ( 'NONE',  ( 1.719304012341582588, 5.690355757825640737, -11.38834240361563488 ) ) ;
#45623 = CARTESIAN_POINT ( 'NONE',  ( 0.000000000000000000, 0.000000000000000000, 0.000000000000000000 ) ) ;
#45624 = DIRECTION ( 'NONE',  ( 0.000000000000000000, -0.01356324068817998073, 0.9999080150203990547 ) ) ;
#45626 = VERTEX_POINT ( 'NONE', #12010 ) ;
#45625 = CARTESIAN_POINT ( 'NONE',  ( 7.278150647452634736, -5.674969998030102047, 12.25652322899233937 ) ) ;
#45627 = VECTOR ( 'NONE', #43368, 1000.000000000000000 ) ;
#45628 = LINE ( 'NONE', #60599, #17305 ) ;
#45629 =( BOUNDED_CURVE ( )  B_SPLINE_CURVE ( 3, ( #35290, #48, #61229, #40949 ),
 .UNSPECIFIED., .F., .F. ) 
 B_SPLINE_CURVE_WITH_KNOTS ( ( 4, 4 ),
 ( 4.379469035996294224, 4.407264310173042432 ),
 .UNSPECIFIED. ) 
 CURVE ( )  GEOMETRIC_REPRESENTATION_ITEM ( )  RATIONAL_B_SPLINE_CURVE ( ( 1.000000000000000000, 0.9999356195973556627, 0.9999356195973556627, 1.000000000000000000 ) ) 
 REPRESENTATION_ITEM ( '' )  );
#45630 = ORIENTED_EDGE ( 'NONE', *, *, #42941, .T. ) ;
#45631 = CARTESIAN_POINT ( 'NONE',  ( -37.00000000000000711, 0.000000000000000000, 0.000000000000000000 ) ) ;
#45632 = ORIENTED_EDGE ( 'NONE', *, *, #59756, .T. ) ;
#45633 = CARTESIAN_POINT ( 'NONE',  ( -37.00000000000000711, 7.817610399097512541, 8.766823244862019138 ) ) ;
#45634 = ADVANCED_FACE ( 'NONE', ( #47929 ), #12335, .T. ) ;
#45635 = ORIENTED_EDGE ( 'NONE', *, *, #64808, .F. ) ;
#45636 = CARTESIAN_POINT ( 'NONE',  ( -36.00000000000000711, 10.49626516989271252, 7.238157050195668241 ) ) ;
#45637 = DIRECTION ( 'NONE',  ( -1.000000000000000000, -0.000000000000000000, -0.000000000000000000 ) ) ;
#45638 = AXIS2_PLACEMENT_3D ( 'NONE', #49492, #3930, #8906 ) ;
#45639 = CARTESIAN_POINT ( 'NONE',  ( -27.08588607604433207, -2.215240480751993868, 0.6046196991082962713 ) ) ;
#45640 = CYLINDRICAL_SURFACE ( 'NONE', #50773, 6.000000000000000888 ) ;
#45641 = CARTESIAN_POINT ( 'NONE',  ( 11.86932257037118177, 8.667155996924391204, -8.300945040779886597 ) ) ;
#45642 = VERTEX_POINT ( 'NONE', #42930 ) ;
#45643 = DIRECTION ( 'NONE',  ( 1.000000000000000000, 0.000000000000000000, 0.000000000000000000 ) ) ;
#45644 = ORIENTED_EDGE ( 'NONE', *, *, #16344, .T. ) ;
#45645 = EDGE_CURVE ( 'NONE', #54601, #31785, #25180, .T. ) ;
#45646 = CARTESIAN_POINT ( 'NONE',  ( -22.28506771379528573, 0.8783543640077344783, -3.622079238249916067 ) ) ;
#45647 = CARTESIAN_POINT ( 'NONE',  ( -36.00000000000000711, 5.300372733891805410, -11.59605747147781152 ) ) ;
#45648 = CARTESIAN_POINT ( 'NONE',  ( -2.532614230583026593, 5.020478806276888584, 10.89930238848911337 ) ) ;
#45649 = ADVANCED_FACE ( 'NONE', ( #22665 ), #63210, .T. ) ;
#45650 = ORIENTED_EDGE ( 'NONE', *, *, #42275, .F. ) ;
#45651 = FACE_OUTER_BOUND ( 'NONE', #16792, .T. ) ;
#45652 = ADVANCED_FACE ( 'NONE', ( #48284 ), #24452, .F. ) ;
#45653 = AXIS2_PLACEMENT_3D ( 'NONE', #17951, #28573, #38214 ) ;
#45654 = VECTOR ( 'NONE', #56800, 1000.000000000000000 ) ;
#45655 = EDGE_CURVE ( 'NONE', #21860, #42381, #3979, .T. ) ;
#45656 = EDGE_CURVE ( 'NONE', #28963, #27631, #39903, .T. ) ;
#45657 = CARTESIAN_POINT ( 'NONE',  ( 47.41971561978370886, -0.5128904950765936777, 11.09198065024578916 ) ) ;
#45658 = EDGE_CURVE ( 'NONE', #33142, #55082, #59881, .T. ) ;
#45659 = DIRECTION ( 'NONE',  ( -1.000000000000000000, 0.000000000000000000, 0.000000000000000000 ) ) ;
#45660 = CARTESIAN_POINT ( 'NONE',  ( -25.82596324657533415, -3.714872568654937091, -25.00000000000000355 ) ) ;
#45661 = VERTEX_POINT ( 'NONE', #3379 ) ;
#45662 = CARTESIAN_POINT ( 'NONE',  ( 0.2653141334712560417, 2.083134085643206568, -12.06772877558521806 ) ) ;
#45663 = DIRECTION ( 'NONE',  ( -1.000000000000000000, 0.000000000000000000, 0.000000000000000000 ) ) ;
#45664 = CARTESIAN_POINT ( 'NONE',  ( 3.968427614672949577, 6.597710521095812020, 10.03374174353559845 ) ) ;
#45665 = AXIS2_PLACEMENT_3D ( 'NONE', #6863, #53394, #2541 ) ;
#45666 = CARTESIAN_POINT ( 'NONE',  ( -35.00000000000000000, -10.68873102412847587, 6.950793414699756312 ) ) ;
#45667 = CARTESIAN_POINT ( 'NONE',  ( 37.00000000000000711, 10.91072401419418192, 5.428340790341586342 ) ) ;
#45668 = AXIS2_PLACEMENT_3D ( 'NONE', #13527, #33808, #39793 ) ;
#45669 = ORIENTED_EDGE ( 'NONE', *, *, #64177, .T. ) ;
#45670 = CARTESIAN_POINT ( 'NONE',  ( 2.257661810676420355, 0.1348365785570998787, 7.638648121130935387 ) ) ;
#45671 = CARTESIAN_POINT ( 'NONE',  ( 3.291290029914074378, 8.250315036047103590, -8.713914264323182834 ) ) ;
#45672 = CARTESIAN_POINT ( 'NONE',  ( 5.520433897694421610, -0.01397038704729854953, -0.005630909886753013814 ) ) ;
#45673 = ORIENTED_EDGE ( 'NONE', *, *, #27086, .T. ) ;
#45674 = CARTESIAN_POINT ( 'NONE',  ( 37.00000000000000711, -8.624332853795991127, 9.390600770288079602 ) ) ;
#45675 = LINE ( 'NONE', #9119, #49001 ) ;
#45676 = ORIENTED_EDGE ( 'NONE', *, *, #52372, .F. ) ;
#45677 = CIRCLE ( 'NONE', #42477, 5.000000000000000000 ) ;
#45678 = ORIENTED_EDGE ( 'NONE', *, *, #53503, .F. ) ;
#45679 = ORIENTED_EDGE ( 'NONE', *, *, #53469, .F. ) ;
#45680 = EDGE_CURVE ( 'NONE', #19321, #31870, #52815, .T. ) ;
#45681 = ORIENTED_EDGE ( 'NONE', *, *, #36263, .F. ) ;
#45682 = DIRECTION ( 'NONE',  ( 0.000000000000000000, 0.01356324068817998940, -0.9999080150203990547 ) ) ;
#45683 = LINE ( 'NONE', #65313, #31501 ) ;
#45684 = CARTESIAN_POINT ( 'NONE',  ( 3.152665057736204535, -4.377619405894248139, -6.622010822085805160 ) ) ;
#45685 = CIRCLE ( 'NONE', #45051, 12.18650000000000411 ) ;
#45686 = CARTESIAN_POINT ( 'NONE',  ( 35.00000000000000000, 2.627174906297071733, 11.44858830469737221 ) ) ;
#45687 = CARTESIAN_POINT ( 'NONE',  ( 2.000000000000001776, 0.4129979343797385294, 6.800241778083691457 ) ) ;
#45688 = CARTESIAN_POINT ( 'NONE',  ( -12.89187373143239945, -27.44222185127960145, 12.55025375818352629 ) ) ;
#45689 = CARTESIAN_POINT ( 'NONE',  ( 24.88574069546950085, -1.123412547988487775, -13.45466109831467705 ) ) ;
#45691 = ORIENTED_EDGE ( 'NONE', *, *, #59765, .F. ) ;
#45690 = LINE ( 'NONE', #20430, #32974 ) ;
#45692 = CARTESIAN_POINT ( 'NONE',  ( 3.780834652287974773, 8.352030633203074927, 8.616471685210687070 ) ) ;
#45693 = VERTEX_POINT ( 'NONE', #58918 ) ;
#45694 = DIRECTION ( 'NONE',  ( 0.000000000000000000, 0.7790879021242486102, -0.6269146997508011632 ) ) ;
#45695 = ORIENTED_EDGE ( 'NONE', *, *, #20641, .F. ) ;
#45696 = EDGE_CURVE ( 'NONE', #60506, #1959, #19869, .T. ) ;
#45697 = VERTEX_POINT ( 'NONE', #64204 ) ;
#45698 = CARTESIAN_POINT ( 'NONE',  ( 35.00000000000000000, 4.018060380616396365, -11.50504120060944757 ) ) ;
#45699 = CARTESIAN_POINT ( 'NONE',  ( 15.30590914263659386, -29.00884126188377365, 11.24874127360776654 ) ) ;
#45700 = CARTESIAN_POINT ( 'NONE',  ( 2.655192694324109759, 7.714239566599824016, 5.716669423974572339 ) ) ;
#45701 = VECTOR ( 'NONE', #938, 1000.000000000000000 ) ;
#45702 = PRESENTATION_LAYER_ASSIGNMENT (  '', '', ( #17031 ) ) ;
#45703 = CIRCLE ( 'NONE', #62673, 12.75000000000000178 ) ;
#45705 = CIRCLE ( 'NONE', #5367, 5.000000000000001776 ) ;
#45704 = CARTESIAN_POINT ( 'NONE',  ( 47.00000000000000711, 4.705694406421931860E-17, -3.469127814946512892E-15 ) ) ;
#45706 = CARTESIAN_POINT ( 'NONE',  ( -35.00000000000000000, -5.246972444134095248, 10.99909370905155370 ) ) ;
#45707 = CARTESIAN_POINT ( 'NONE',  ( 0.3223008802179264110, -12.03398982086835112, 2.370176598416293245 ) ) ;
#45708 = ORIENTED_EDGE ( 'NONE', *, *, #23529, .F. ) ;
#45709 = VERTEX_POINT ( 'NONE', #44897 ) ;
#45710 = DIRECTION ( 'NONE',  ( 0.000000000000000000, 0.01356324068817999808, -0.9999080150203990547 ) ) ;
#45711 = ORIENTED_EDGE ( 'NONE', *, *, #39361, .F. ) ;
#45712 = EDGE_CURVE ( 'NONE', #11505, #48583, #23647, .T. ) ;
#45713 = VERTEX_POINT ( 'NONE', #19310 ) ;
#45714 = DIRECTION ( 'NONE',  ( 0.000000000000000000, 0.000000000000000000, 1.000000000000000000 ) ) ;
#45715 = CARTESIAN_POINT ( 'NONE',  ( 0.2872850955227737590, 10.50585060073189680, -6.306790329742824497 ) ) ;
#45716 = CARTESIAN_POINT ( 'NONE',  ( -37.00000000000000711, -11.74226168163341022, -0.3025107581132430723 ) ) ;
#45717 = CARTESIAN_POINT ( 'NONE',  ( 37.00000000000000711, -4.983891302653661093, -11.73555825188274682 ) ) ;
#45719 = CIRCLE ( 'NONE', #26632, 7.499999999999988454 ) ;
#45718 = LINE ( 'NONE', #24794, #8245 ) ;
#45720 = CARTESIAN_POINT ( 'NONE',  ( 2.000000000000001776, 0.3246585432986198727, 6.805031400696091914 ) ) ;
#45721 = CIRCLE ( 'NONE', #59545, 12.18650000000000055 ) ;
#45722 = VERTEX_POINT ( 'NONE', #54879 ) ;
#45723 = ORIENTED_EDGE ( 'NONE', *, *, #775, .F. ) ;
#45724 = AXIS2_PLACEMENT_3D ( 'NONE', #49666, #4107, #24375 ) ;
#45725 = CARTESIAN_POINT ( 'NONE',  ( 37.00000000000000711, 4.705694406421931860E-17, -3.469127814946512892E-15 ) ) ;
#45726 = DIRECTION ( 'NONE',  ( 0.8386510381079236298, 0.5446691071471760903, -0.000000000000000000 ) ) ;
#45727 = VECTOR ( 'NONE', #64207, 1000.000000000000000 ) ;
#45728 = FACE_OUTER_BOUND ( 'NONE', #26745, .T. ) ;
#45729 = EDGE_CURVE ( 'NONE', #26969, #45854, #24715, .T. ) ;
#45730 = EDGE_CURVE ( 'NONE', #38995, #10202, #19646, .T. ) ;
#45731 = DIRECTION ( 'NONE',  ( -1.000000000000000000, 0.000000000000000000, 0.000000000000000000 ) ) ;
#45732 = EDGE_CURVE ( 'NONE', #659, #26603, #4934, .T. ) ;
#45733 = CIRCLE ( 'NONE', #49975, 12.18650000000000055 ) ;
#45734 = CARTESIAN_POINT ( 'NONE',  ( 22.57855258442565116, 3.026812727784649493, -13.15630665159948975 ) ) ;
#45735 = CARTESIAN_POINT ( 'NONE',  ( -37.00000000000000711, -10.07641281632181673, 6.036400161834530209 ) ) ;
#45736 = EDGE_CURVE ( 'NONE', #12199, #20112, #51221, .T. ) ;
#45737 = CARTESIAN_POINT ( 'NONE',  ( 2.844750968615535669, 6.210802026112107299, 4.777247819183539690 ) ) ;
#45738 = VECTOR ( 'NONE', #64718, 1000.000000000000114 ) ;
#45739 = VERTEX_POINT ( 'NONE', #65486 ) ;
#45740 = CARTESIAN_POINT ( 'NONE',  ( 2.931247277082685176, -0.3703309885897361209, 7.855653518374115407 ) ) ;
#45741 = FACE_OUTER_BOUND ( 'NONE', #49045, .T. ) ;
#45742 = CYLINDRICAL_SURFACE ( 'NONE', #14181, 12.74999999999999822 ) ;
#45743 = AXIS2_PLACEMENT_3D ( 'NONE', #31439, #14805, #35090 ) ;
#45744 = CIRCLE ( 'NONE', #20256, 12.18650000000000233 ) ;
#45745 = CIRCLE ( 'NONE', #41510, 12.18649999999999878 ) ;
#45746 = CARTESIAN_POINT ( 'NONE',  ( 2.994568964204213479, -6.620406464816364966, -4.283796412555548550 ) ) ;
#45747 = DIRECTION ( 'NONE',  ( 0.000000000000000000, 0.01356324068817992175, -0.9999080150203990547 ) ) ;
#45748 = ORIENTED_EDGE ( 'NONE', *, *, #48878, .F. ) ;
#45749 = CARTESIAN_POINT ( 'NONE',  ( 2.241526690369556096, -3.832206765347542010, -6.602966219605680642 ) ) ;
#45750 = CARTESIAN_POINT ( 'NONE',  ( -36.00000000000000711, -4.983891302653499444, -11.73555825188281787 ) ) ;
#45751 = CARTESIAN_POINT ( 'NONE',  ( 18.18435566811206527, -28.78814669831782780, -7.856426167042674713 ) ) ;
#45752 = ORIENTED_EDGE ( 'NONE', *, *, #46751, .F. ) ;
#45753 = DIRECTION ( 'NONE',  ( 0.000000000000000000, -0.01356324068817999114, 0.9999080150203989437 ) ) ;
#45754 = CARTESIAN_POINT ( 'NONE',  ( 0.000000000000000000, 0.000000000000000000, 0.000000000000000000 ) ) ;
#45755 = CARTESIAN_POINT ( 'NONE',  ( -22.27719381268171261, -0.9326100520993095833, -3.561499689648256251 ) ) ;
#45757 = VERTEX_POINT ( 'NONE', #344 ) ;
#45756 = LINE ( 'NONE', #26142, #48773 ) ;
#45758 = DIRECTION ( 'NONE',  ( 0.000000000000000000, -0.01356324068817999114, 0.9999080150203989437 ) ) ;
#45759 = CIRCLE ( 'NONE', #13898, 5.000000000000000888 ) ;
#45760 = AXIS2_PLACEMENT_3D ( 'NONE', #63866, #22677, #58240 ) ;
#45761 = PRODUCT_RELATED_PRODUCT_CATEGORY ( 'part', '', ( #33322 ) ) ;
#45762 = EDGE_CURVE ( 'NONE', #26019, #36323, #53868, .T. ) ;
#45763 = CARTESIAN_POINT ( 'NONE',  ( 3.031336079629428859, -7.553623348802302573, -2.306006909710477171 ) ) ;
#45764 = ORIENTED_EDGE ( 'NONE', *, *, #36157, .T. ) ;
#45765 = VECTOR ( 'NONE', #28004, 1000.000000000000000 ) ;
#45766 = CARTESIAN_POINT ( 'NONE',  ( 0.3160775863651080764, 7.697077652699450212, 9.546663463486071421 ) ) ;
#45767 = EDGE_CURVE ( 'NONE', #43301, #64826, #46977, .T. ) ;
#45768 = CARTESIAN_POINT ( 'NONE',  ( -9.181000754636428951, 11.30974670563849571, -7.379660233987727302 ) ) ;
#45769 = DIRECTION ( 'NONE',  ( -1.000000000000000000, -0.000000000000000000, -0.000000000000000000 ) ) ;
#45770 = CARTESIAN_POINT ( 'NONE',  ( 37.00000000000000711, 4.705694406421931860E-17, -3.469127814946512892E-15 ) ) ;
#45771 = CARTESIAN_POINT ( 'NONE',  ( -37.00000000000000711, 0.000000000000000000, 0.000000000000000000 ) ) ;
#45772 = AXIS2_PLACEMENT_3D ( 'NONE', #9605, #29903, #25244 ) ;
#45773 = CYLINDRICAL_SURFACE ( 'NONE', #5831, 4.999999999999999112 ) ;
#45774 = CARTESIAN_POINT ( 'NONE',  ( 35.00000000000000000, 2.346765782874432382, -11.95840593935202278 ) ) ;
#45775 = ORIENTED_EDGE ( 'NONE', *, *, #23960, .F. ) ;
#45776 = CARTESIAN_POINT ( 'NONE',  ( 2.276198483117261251, -5.031786924855515153, 5.756970692722257255 ) ) ;
#45777 = AXIS2_PLACEMENT_3D ( 'NONE', #53830, #63773, #8265 ) ;
#45778 = ORIENTED_EDGE ( 'NONE', *, *, #12295, .F. ) ;
#45779 = ADVANCED_FACE ( 'NONE', ( #11607 ), #52196, .T. ) ;
#45780 = SURFACE_STYLE_USAGE ( .BOTH. , #51768 ) ;
#45781 = DIRECTION ( 'NONE',  ( 0.000000000000000000, -0.1081190184239489566, 0.9941379571543588201 ) ) ;
#45782 = CARTESIAN_POINT ( 'NONE',  ( 3.031336079629727731, 1.779751109289623434, 7.694633165537369202 ) ) ;
#45783 = CARTESIAN_POINT ( 'NONE',  ( -17.97077823246242190, -9.629623312810583258, 9.462431742398617729 ) ) ;
#45784 = EDGE_LOOP ( 'NONE', ( #43590, #21653, #1468, #18305 ) ) ;
#45786 = DIRECTION ( 'NONE',  ( 0.000000000000000000, -0.01356324068817999114, 0.9999080150203989437 ) ) ;
#45785 = AXIS2_PLACEMENT_3D ( 'NONE', #24284, #48924, #29587 ) ;
#45787 = CARTESIAN_POINT ( 'NONE',  ( 12.28749691143031697, 11.61437747111016172, -3.022945891257621032 ) ) ;
#45788 = FACE_BOUND ( 'NONE', #6949, .T. ) ;
#45789 = ORIENTED_EDGE ( 'NONE', *, *, #31745, .F. ) ;
#45790 = VERTEX_POINT ( 'NONE', #31876 ) ;
#45791 = CARTESIAN_POINT ( 'NONE',  ( 2.000000000000001776, -7.203928197742088813, -2.086484728383233289 ) ) ;
#45792 = CIRCLE ( 'NONE', #50022, 12.75000000000000178 ) ;
#45793 = ADVANCED_FACE ( 'NONE', ( #16930 ), #6644, .T. ) ;
#45794 = ADVANCED_FACE ( 'NONE', ( #57849 ), #56868, .T. ) ;
#45795 = ORIENTED_EDGE ( 'NONE', *, *, #13158, .F. ) ;
#45796 = DIRECTION ( 'NONE',  ( 0.000000000000000000, 0.01356324068817998940, -0.9999080150203989437 ) ) ;
#45797 = DIRECTION ( 'NONE',  ( 0.000000000000000000, 0.000000000000000000, 1.000000000000000000 ) ) ;
#45798 = LINE ( 'NONE', #41442, #62819 ) ;
#45799 = EDGE_CURVE ( 'NONE', #42911, #2803, #54904, .T. ) ;
#45800 = CARTESIAN_POINT ( 'NONE',  ( 2.889800649504073782, -3.118861721612602889, 5.267262008933660589 ) ) ;
#45801 = AXIS2_PLACEMENT_3D ( 'NONE', #31362, #123, #55662 ) ;
#45802 = VECTOR ( 'NONE', #58694, 1000.000000000000000 ) ;
#45803 = CARTESIAN_POINT ( 'NONE',  ( 25.05309951391468459, -8.823569016628452388, -8.132934882857099979 ) ) ;
#45804 = DIRECTION ( 'NONE',  ( -1.000000000000000000, 0.000000000000000000, 0.000000000000000000 ) ) ;
#45805 = AXIS2_PLACEMENT_3D ( 'NONE', #32968, #53937, #22343 ) ;
#45806 = ORIENTED_EDGE ( 'NONE', *, *, #38913, .F. ) ;
#45807 = CARTESIAN_POINT ( 'NONE',  ( 2.263328370261529887, 7.640407877530305925, -0.1420109704216046820 ) ) ;
#45808 = DIRECTION ( 'NONE',  ( 0.000000000000000000, 0.2355298848897447450, 0.9718671068226475418 ) ) ;
#45809 = DIRECTION ( 'NONE',  ( -1.000000000000000000, 0.000000000000000000, 0.000000000000000000 ) ) ;
#45810 = CARTESIAN_POINT ( 'NONE',  ( 12.44012537477689229, 11.41883593682970321, -7.203604244167406634 ) ) ;
#45811 = CARTESIAN_POINT ( 'NONE',  ( -19.47984447937493613, -3.750539801530005768, 12.96855624952674724 ) ) ;
#45812 = CARTESIAN_POINT ( 'NONE',  ( 10.48620311856346454, 8.250315036047107142, 25.00000000000000000 ) ) ;
#45813 = DIRECTION ( 'NONE',  ( 1.000000000000000000, 0.000000000000000000, 0.000000000000000000 ) ) ;
#45814 = CARTESIAN_POINT ( 'NONE',  ( -35.00000000000000000, -2.497432891016921008, 11.47758908105693720 ) ) ;
#45815 = CIRCLE ( 'NONE', #39436, 5.000000000000000000 ) ;
#45816 = ADVANCED_FACE ( 'NONE', ( #27232 ), #12263, .T. ) ;
#45817 = AXIS2_PLACEMENT_3D ( 'NONE', #12691, #43281, #32970 ) ;
#45818 = ORIENTED_EDGE ( 'NONE', *, *, #37377, .F. ) ;
#45819 = DIRECTION ( 'NONE',  ( 1.000000000000000000, 0.000000000000000000, -0.000000000000000000 ) ) ;
#45820 = AXIS2_PLACEMENT_3D ( 'NONE', #25206, #4632, #14876 ) ;
#45821 = EDGE_CURVE ( 'NONE', #35612, #8110, #914, .T. ) ;
#45822 = VERTEX_POINT ( 'NONE', #7267 ) ;
#45823 = LINE ( 'NONE', #35163, #65707 ) ;
#45824 = DIRECTION ( 'NONE',  ( 0.000000000000000000, -0.01356324068817991828, 0.9999080150203990547 ) ) ;
#45825 = CARTESIAN_POINT ( 'NONE',  ( 2.241449424704146320, -4.860179885671838562, 5.887589908049627674 ) ) ;
#45826 = CIRCLE ( 'NONE', #51155, 12.74999999999999822 ) ;
#45827 = CARTESIAN_POINT ( 'NONE',  ( 0.000000000000000000, 0.000000000000000000, 0.000000000000000000 ) ) ;
#45828 = DIRECTION ( 'NONE',  ( 0.000000000000000000, -0.8827602140260366603, 0.4698238015817268187 ) ) ;
#45829 = ORIENTED_EDGE ( 'NONE', *, *, #58482, .T. ) ;
#45830 = CARTESIAN_POINT ( 'NONE',  ( 2.000000000000001776, -1.530946385938423582, 7.342084388195347699 ) ) ;
#45832 = AXIS2_PLACEMENT_3D ( 'NONE', #39753, #49435, #23828 ) ;
#45831 = CARTESIAN_POINT ( 'NONE',  ( 0.000000000000000000, 0.000000000000000000, 0.000000000000000000 ) ) ;
#45833 = CARTESIAN_POINT ( 'NONE',  ( -37.00000000000000711, 0.000000000000000000, 0.000000000000000000 ) ) ;
#45834 = CARTESIAN_POINT ( 'NONE',  ( 2.350038591457883186, 5.855794476068868271, -8.861946706686296693 ) ) ;
#45835 = CARTESIAN_POINT ( 'NONE',  ( -18.35038919876964059, -4.541481526684528092, 11.10824452668961193 ) ) ;
#45836 = AXIS2_PLACEMENT_3D ( 'NONE', #62380, #37786, #51783 ) ;
#45837 = CYLINDRICAL_SURFACE ( 'NONE', #31877, 12.18649999999999878 ) ;
#45838 =( BOUNDED_SURFACE ( )  B_SPLINE_SURFACE ( 3, 1, ( 
 ( #64577, #43654 ),
 ( #59620, #8101 ),
 ( #63944, #18420 ),
 ( #38686, #13400 ) ),
 .UNSPECIFIED., .F., .F., .F. ) 
 B_SPLINE_SURFACE_WITH_KNOTS ( ( 4, 4 ),
 ( 2, 2 ),
 ( 0.000000000000000000, 1.000000000000000000 ),
 ( 0.000000000000000000, 1.000000000000000000 ),
 .UNSPECIFIED. ) 
 GEOMETRIC_REPRESENTATION_ITEM ( )  RATIONAL_B_SPLINE_SURFACE ( (
 ( 1.000000000000000000, 1.000000000000000000),
 ( 0.8716676215708681896, 0.8964445200148167814),
 ( 0.8716676215708681896, 0.8964445200148167814),
 ( 1.000000000000000000, 1.000000000000000000) ) ) 
 REPRESENTATION_ITEM ( '' )  SURFACE ( )  );
#45839 = ORIENTED_EDGE ( 'NONE', *, *, #12428, .F. ) ;
#45840 = DIRECTION ( 'NONE',  ( 1.000000000000000000, 0.000000000000000000, 0.000000000000000000 ) ) ;
#45841 = AXIS2_PLACEMENT_3D ( 'NONE', #42642, #27056, #62947 ) ;
#45842 = ORIENTED_EDGE ( 'NONE', *, *, #2328, .T. ) ;
#45843 = AXIS2_PLACEMENT_3D ( 'NONE', #12546, #62768, #11263 ) ;
#45844 = CARTESIAN_POINT ( 'NONE',  ( 0.3632410797595224117, -0.2628628737172604701, -12.27601307605977965 ) ) ;
#45845 = LINE ( 'NONE', #14264, #43719 ) ;
#45846 = CARTESIAN_POINT ( 'NONE',  ( -22.30625920655495165, -1.076742202099146839, -3.635849356906419416 ) ) ;
#45847 = CARTESIAN_POINT ( 'NONE',  ( 35.00000000000000000, -12.54989509947652415, -2.250029553613715372 ) ) ;
#45848 = AXIS2_PLACEMENT_3D ( 'NONE', #39128, #45114, #65375 ) ;
#45849 = CIRCLE ( 'NONE', #46903, 5.000000000000000000 ) ;
#45850 = AXIS2_PLACEMENT_3D ( 'NONE', #42287, #36347, #36674 ) ;
#45851 = ORIENTED_EDGE ( 'NONE', *, *, #3123, .T. ) ;
#45852 = ORIENTED_EDGE ( 'NONE', *, *, #17584, .F. ) ;
#45853 = CARTESIAN_POINT ( 'NONE',  ( -28.85619398320021745, 3.750539801530000439, 11.39883551934754280 ) ) ;
#45854 = VERTEX_POINT ( 'NONE', #42499 ) ;
#45855 = EDGE_CURVE ( 'NONE', #30464, #29745, #59187, .T. ) ;
#45856 = CARTESIAN_POINT ( 'NONE',  ( 2.903928887688506322, 4.835706109686078058, 7.316175791235219883 ) ) ;
#45857 = CARTESIAN_POINT ( 'NONE',  ( -37.00000000000000711, 11.07407352312212723, 3.916263239775389149 ) ) ;
#45858 = DIRECTION ( 'NONE',  ( 1.000000000000000000, -0.000000000000000000, 0.000000000000000000 ) ) ;
#45859 = CARTESIAN_POINT ( 'NONE',  ( 0.6511581176954504002, 9.263557799002967386, 8.205008037406312127 ) ) ;
#45860 = CARTESIAN_POINT ( 'NONE',  ( 2.990245332647883281, -4.676740826320302524, 7.075286609974379637 ) ) ;
#45861 = CARTESIAN_POINT ( 'NONE',  ( 0.3675815128205894289, 10.76447900494948584, -5.910255304480332761 ) ) ;
#45862 = CARTESIAN_POINT ( 'NONE',  ( -9.994394625950207001, -3.431105229675856627, 11.50047856588473216 ) ) ;
#45863 = ORIENTED_EDGE ( 'NONE', *, *, #62654, .F. ) ;
#45864 = CARTESIAN_POINT ( 'NONE',  ( 0.9296196016833910836, -10.99907063288863540, 5.870433615766981639 ) ) ;
#45865 = ORIENTED_EDGE ( 'NONE', *, *, #9151, .T. ) ;
#45866 = DIRECTION ( 'NONE',  ( 0.000000000000000000, 0.01356324068817998940, -0.9999080150203990547 ) ) ;
#45867 = AXIS2_PLACEMENT_3D ( 'NONE', #31226, #65780, #61153 ) ;
#45868 = AXIS2_PLACEMENT_3D ( 'NONE', #31519, #26216, #15884 ) ;
#45869 = CARTESIAN_POINT ( 'NONE',  ( -27.10422407540546885, 1.954655484500564588, -1.306850885988315003 ) ) ;
#45870 = EDGE_CURVE ( 'NONE', #35715, #8602, #57046, .T. ) ;
#45871 = ORIENTED_EDGE ( 'NONE', *, *, #40748, .F. ) ;
#45872 = AXIS2_PLACEMENT_3D ( 'NONE', #1442, #31353, #21722 ) ;
#45873 = CARTESIAN_POINT ( 'NONE',  ( 1.719304012340734378, -7.581471372739226666, -10.22720798541506682 ) ) ;
#45874 = ORIENTED_EDGE ( 'NONE', *, *, #42434, .T. ) ;
#45875 = DIRECTION ( 'NONE',  ( -1.000000000000000000, 0.000000000000000000, 0.000000000000000000 ) ) ;
#45876 = LINE ( 'NONE', #39892, #27550 ) ;
#45877 = CARTESIAN_POINT ( 'NONE',  ( 2.000000000000001776, -7.493043167941613625, 0.3229614270519164942 ) ) ;
#45878 = CARTESIAN_POINT ( 'NONE',  ( 2.305787727787083519, 7.135468203930020792, -2.774453000917077805 ) ) ;
#45879 = ORIENTED_EDGE ( 'NONE', *, *, #16648, .T. ) ;
#45880 = AXIS2_PLACEMENT_3D ( 'NONE', #30973, #40959, #34960 ) ;
#45881 = ORIENTED_EDGE ( 'NONE', *, *, #56435, .T. ) ;
#45882 = CARTESIAN_POINT ( 'NONE',  ( 3.047904605210427942, -7.047014837597081360, 3.577928268982043747 ) ) ;
#45883 = VERTEX_POINT ( 'NONE', #17601 ) ;
#45884 = EDGE_CURVE ( 'NONE', #33198, #36759, #10324, .T. ) ;
#45885 = CARTESIAN_POINT ( 'NONE',  ( 0.4613984246114875010, -11.66278164635732217, -3.943860067443764716 ) ) ;
#45886 = ORIENTED_EDGE ( 'NONE', *, *, #59555, .T. ) ;
#45887 = CIRCLE ( 'NONE', #22474, 3.999999999999999112 ) ;
#45888 = ORIENTED_EDGE ( 'NONE', *, *, #47128, .F. ) ;
#45889 = ORIENTED_EDGE ( 'NONE', *, *, #60975, .T. ) ;
#45890 = CARTESIAN_POINT ( 'NONE',  ( 2.969415267404014624, -5.777543886622418690, 5.354299007565158419 ) ) ;
#45891 = CARTESIAN_POINT ( 'NONE',  ( 18.54281746013980126, -28.86505449477128593, 7.298814700743933237 ) ) ;
#45892 = LINE ( 'NONE', #21258, #44787 ) ;
#45893 = CARTESIAN_POINT ( 'NONE',  ( -22.94572469358971034, 4.424217216616520787, -2.078200699019419062 ) ) ;
#45894 = CARTESIAN_POINT ( 'NONE',  ( -22.27384469013076185, -1.508555848190757276, 3.358914544760229326 ) ) ;
#45895 = ORIENTED_EDGE ( 'NONE', *, *, #64825, .F. ) ;
#45896 = CARTESIAN_POINT ( 'NONE',  ( 2.259830038564644816, -2.483392345595102579, -7.225713255971310645 ) ) ;
#45897 = VECTOR ( 'NONE', #19138, 1000.000000000000000 ) ;
#45898 = EDGE_LOOP ( 'NONE', ( #65749, #53869, #5041, #23127 ) ) ;
#45899 = CARTESIAN_POINT ( 'NONE',  ( 37.25000000000000711, -20.00000000000000000, 2.449293598294706907E-15 ) ) ;
#45900 = CARTESIAN_POINT ( 'NONE',  ( -27.10719052120871098, 0.6736837626858914740, 2.261993590776020469 ) ) ;
#45901 = CARTESIAN_POINT ( 'NONE',  ( 0.2833330754217375791, -10.71034013638382021, 5.950193237802373858 ) ) ;
#45902 = CARTESIAN_POINT ( 'NONE',  ( 5.536195898058073439, 0.002666509901870070445, -0.008071068258923577710 ) ) ;
#45903 = CARTESIAN_POINT ( 'NONE',  ( 1.549075743847115660, -10.62322497417014411, -6.912427991524592308 ) ) ;
#45904 = AXIS2_PLACEMENT_3D ( 'NONE', #57391, #32099, #27131 ) ;
#45905 = B_SPLINE_CURVE_WITH_KNOTS ( 'NONE', 3,
 ( #54709, #9130, #4156, #44692, #64982, #19455, #39725 ),
 .UNSPECIFIED., .F., .F.,
 ( 4, 3, 4 ),
 ( 9.486769009248163798E-19, 6.607638129004464488E-05, 8.338150981378363025E-05 ),
 .UNSPECIFIED. ) ;
#45906 = EDGE_CURVE ( 'NONE', #29286, #11102, #37952, .T. ) ;
#45907 = CIRCLE ( 'NONE', #11893, 6.936499999999989008 ) ;
#45908 = VECTOR ( 'NONE', #65104, 1000.000000000000000 ) ;
#45909 = ORIENTED_EDGE ( 'NONE', *, *, #41490, .T. ) ;
#45910 = DIRECTION ( 'NONE',  ( 0.000000000000000000, 0.9903235168508555120, 0.1387779952735781197 ) ) ;
#45911 = ORIENTED_EDGE ( 'NONE', *, *, #18326, .F. ) ;
#45912 = CARTESIAN_POINT ( 'NONE',  ( -24.51086266037313521, -9.341341120805065401, 9.748122042855369429 ) ) ;
#45913 = CARTESIAN_POINT ( 'NONE',  ( 2.639814597422738718, 6.851176153958525639, -3.659458430304273868 ) ) ;
#45914 = DIRECTION ( 'NONE',  ( -1.000000000000000000, 0.000000000000000000, 0.000000000000000000 ) ) ;
#45915 = DIRECTION ( 'NONE',  ( -1.000000000000000000, 0.000000000000000000, 0.000000000000000000 ) ) ;
#45916 = VERTEX_POINT ( 'NONE', #62798 ) ;
#45917 = CYLINDRICAL_SURFACE ( 'NONE', #39859, 5.000000000000000888 ) ;
#45918 = LINE ( 'NONE', #372, #37536 ) ;
#45919 = DIRECTION ( 'NONE',  ( 0.000000000000000000, 0.01356324068817991828, -0.9999080150203990547 ) ) ;
#45920 = CARTESIAN_POINT ( 'NONE',  ( 22.98496193214445782, -11.91169011612080197, -6.361484732325027203 ) ) ;
#45921 = VECTOR ( 'NONE', #26161, 1000.000000000000000 ) ;
#45922 = EDGE_CURVE ( 'NONE', #24889, #42846, #62335, .T. ) ;
#45923 = CARTESIAN_POINT ( 'NONE',  ( 0.2958664285830414076, 12.25438626999990710, -0.2205161970874815469 ) ) ;
#45924 = CIRCLE ( 'NONE', #9824, 4.999999999999999112 ) ;
#45925 = AXIS2_PLACEMENT_3D ( 'NONE', #23559, #43833, #18593 ) ;
#45926 = CARTESIAN_POINT ( 'NONE',  ( 35.00000000000000000, 0.2661492558803343345, -12.18359334611896649 ) ) ;
#45927 = CARTESIAN_POINT ( 'NONE',  ( -35.04582288351658548, -0.006225574250549492823, 0.01107592729723125800 ) ) ;
#45928 = CYLINDRICAL_SURFACE ( 'NONE', #10232, 5.000000000000000888 ) ;
#45929 = DIRECTION ( 'NONE',  ( -1.000000000000000000, -0.000000000000000000, 0.000000000000000000 ) ) ;
#45930 = EDGE_CURVE ( 'NONE', #52466, #49767, #33682, .T. ) ;
#45931 = ORIENTED_EDGE ( 'NONE', *, *, #5994, .T. ) ;
#45932 = AXIS2_PLACEMENT_3D ( 'NONE', #41128, #56098, #25864 ) ;
#45934 = ORIENTED_EDGE ( 'NONE', *, *, #31100, .F. ) ;
#45933 = EDGE_CURVE ( 'NONE', #53268, #38732, #18899, .T. ) ;
#45935 = PLANE ( 'NONE',  #9775 ) ;
#45936 = CARTESIAN_POINT ( 'NONE',  ( 5.514970785353741078, 0.001326349372336578557, 0.004532877335078321253 ) ) ;
#45937 = CYLINDRICAL_SURFACE ( 'NONE', #9855, 12.18650000000000055 ) ;
#45938 = CARTESIAN_POINT ( 'NONE',  ( 2.247206125383336417, -1.211896144125592878, -7.539576157880987672 ) ) ;
#45939 = EDGE_CURVE ( 'NONE', #5675, #27379, #51736, .T. ) ;
#45940 = EDGE_LOOP ( 'NONE', ( #31813, #1346, #35369, #58641 ) ) ;
#45941 = CIRCLE ( 'NONE', #48139, 6.936499999999989896 ) ;
#45942 = AXIS2_PLACEMENT_3D ( 'NONE', #28934, #49243, #39223 ) ;
#45943 = ORIENTED_EDGE ( 'NONE', *, *, #53913, .T. ) ;
#45944 = ORIENTED_EDGE ( 'NONE', *, *, #31470, .T. ) ;
#45945 = CARTESIAN_POINT ( 'NONE',  ( 2.373367633546871414, 2.795365972209170824, -7.151506276328599476 ) ) ;
#45946 = AXIS2_PLACEMENT_3D ( 'NONE', #36422, #31434, #51734 ) ;
#45948 = AXIS2_PLACEMENT_3D ( 'NONE', #30383, #65607, #35683 ) ;
#45947 = CARTESIAN_POINT ( 'NONE',  ( -22.65999102136914445, 1.886119913916099122, 4.450325798697146062 ) ) ;
#45949 = ADVANCED_FACE ( 'NONE', ( #44806 ), #24203, .T. ) ;
#45950 = ORIENTED_EDGE ( 'NONE', *, *, #26557, .T. ) ;
#45951 = CARTESIAN_POINT ( 'NONE',  ( -35.00000000000000000, 5.428340790341860789, -10.91072401419405402 ) ) ;
#45952 = CYLINDRICAL_SURFACE ( 'NONE', #25140, 12.74999999999999822 ) ;
#45953 = DIRECTION ( 'NONE',  ( 0.000000000000000000, 0.9847383929261610547, -0.1740410799127650732 ) ) ;
#45954 = ORIENTED_EDGE ( 'NONE', *, *, #21145, .T. ) ;
#45955 = CARTESIAN_POINT ( 'NONE',  ( -22.28121537037576871, 0.3168735205819809830, 3.680034389105500292 ) ) ;
#45956 = EDGE_CURVE ( 'NONE', #55487, #30787, #1757, .T. ) ;
#45957 = CARTESIAN_POINT ( 'NONE',  ( -8.789023433376842220, -31.87591480792562137, -13.49878314047872507 ) ) ;
#45958 = CARTESIAN_POINT ( 'NONE',  ( 0.3665391374699472626, -10.50279796150441136, 6.368473106897092784 ) ) ;
#45959 = VERTEX_POINT ( 'NONE', #23565 ) ;
#45960 = LINE ( 'NONE', #50306, #44816 ) ;
#45961 = ORIENTED_EDGE ( 'NONE', *, *, #894, .T. ) ;
#45962 = DIRECTION ( 'NONE',  ( -1.000000000000000000, 0.000000000000000000, 0.000000000000000000 ) ) ;
#45963 = CIRCLE ( 'NONE', #58751, 4.999999999999999112 ) ;
#45964 = ORIENTED_EDGE ( 'NONE', *, *, #694, .F. ) ;
#45965 = CARTESIAN_POINT ( 'NONE',  ( 0.2655924914740778742, -11.52280271232868003, -4.147079829127369166 ) ) ;
#45966 = DIRECTION ( 'NONE',  ( 0.000000000000000000, 0.01356324068817998940, -0.9999080150203989437 ) ) ;
#45967 = LINE ( 'NONE', #422, #2853 ) ;
#45968 = CARTESIAN_POINT ( 'NONE',  ( 0.2834382757448027368, -12.25055062943084394, 0.2027202995056558987 ) ) ;
#45969 = CARTESIAN_POINT ( 'NONE',  ( 2.256373768223416842, 5.765785888499285861, -5.011614056001876705 ) ) ;
#45970 = DIRECTION ( 'NONE',  ( 1.000000000000000000, 0.000000000000000000, 0.000000000000000000 ) ) ;
#45971 = CARTESIAN_POINT ( 'NONE',  ( 0.2638984909335716500, 1.930290337334056749, 12.09426044257624788 ) ) ;
#45973 = ORIENTED_EDGE ( 'NONE', *, *, #11757, .T. ) ;
#45972 = CARTESIAN_POINT ( 'NONE',  ( 4.724233633166516455, -10.62268705308553329, 8.332287045309458406 ) ) ;
#45974 = EDGE_CURVE ( 'NONE', #10832, #13628, #2901, .T. ) ;
#45975 = B_SPLINE_CURVE_WITH_KNOTS ( 'NONE', 3,
 ( #20907, #6865, #37427, #52742, #2868, #2543, #62687, #58056, #51194, #22812 ),
 .UNSPECIFIED., .F., .F.,
 ( 4, 2, 2, 2, 4 ),
 ( 0.000000000000000000, 0.001081654908065314818, 0.002163309816130629636, 0.003244964724195944453, 0.004326619632261259271 ),
 .UNSPECIFIED. ) ;
#45976 = FACE_OUTER_BOUND ( 'NONE', #60347, .T. ) ;
#45977 = ORIENTED_EDGE ( 'NONE', *, *, #3584, .T. ) ;
#45978 = CARTESIAN_POINT ( 'NONE',  ( 10.53916981844864509, -13.47532649378942260, -0.8438262861795845504 ) ) ;
#45979 = ORIENTED_EDGE ( 'NONE', *, *, #45161, .F. ) ;
#45980 = DIRECTION ( 'NONE',  ( 0.000000000000000000, 0.8696919319575201479, 0.4935949184179230786 ) ) ;
#45981 = ORIENTED_EDGE ( 'NONE', *, *, #26062, .F. ) ;
#45982 = CARTESIAN_POINT ( 'NONE',  ( 0.2648978790185602672, 7.972372351883029395, 9.295532325666474804 ) ) ;
#45983 = LINE ( 'NONE', #26029, #36138 ) ;
#45984 = CARTESIAN_POINT ( 'NONE',  ( 2.000000000000001776, 0.000000000000000000, 0.000000000000000000 ) ) ;
#45985 = DIRECTION ( 'NONE',  ( 1.000000000000000000, 0.000000000000000000, -0.000000000000000000 ) ) ;
#45986 = CARTESIAN_POINT ( 'NONE',  ( 2.000000000000001776, -6.164400007374799095, 2.900694413976478536 ) ) ;
#45987 = ORIENTED_EDGE ( 'NONE', *, *, #58535, .T. ) ;
#45988 = CYLINDRICAL_SURFACE ( 'NONE', #38594, 4.999999999999998224 ) ;
#45989 = VERTEX_POINT ( 'NONE', #28536 ) ;
#45990 = CARTESIAN_POINT ( 'NONE',  ( 35.00000000000000000, 4.705694406421931860E-17, -3.469127814946512892E-15 ) ) ;
#45991 = CYLINDRICAL_SURFACE ( 'NONE', #7974, 5.000000000000000000 ) ;
#45992 = DIRECTION ( 'NONE',  ( 1.000000000000000000, -0.000000000000000000, -0.000000000000000000 ) ) ;
#45993 = EDGE_LOOP ( 'NONE', ( #51518, #48563, #14601, #16820 ) ) ;
#45994 = VECTOR ( 'NONE', #21968, 1000.000000000000000 ) ;
#45995 = VECTOR ( 'NONE', #65706, 1000.000000000000000 ) ;
#45996 = DIRECTION ( 'NONE',  ( 0.000000000000000000, -0.01356324068817998940, 0.9999080150203990547 ) ) ;
#45997 = CIRCLE ( 'NONE', #47092, 6.936499999999988120 ) ;
#45998 = EDGE_CURVE ( 'NONE', #64338, #33727, #11372, .T. ) ;
#45999 = CARTESIAN_POINT ( 'NONE',  ( -35.05012975565874456, -0.009279204628466307739, -0.01039213056760250956 ) ) ;
#46000 = B_SPLINE_CURVE_WITH_KNOTS ( 'NONE', 3,
 ( #58681, #38026, #8122, #59312, #43676, #13738, #58334, #23407, #13103, #63963, #18444, #39681, #14397, #15392, #14072, #55957 ),
 .UNSPECIFIED., .F., .F.,
 ( 4, 3, 3, 3, 3, 4 ),
 ( 5.421010862427522170E-20, 0.0003017745587525248675, 0.0006035491769808740657, 0.0009053241094668204765, 0.001207275924540515818, 0.001510325902534030229 ),
 .UNSPECIFIED. ) ;
#46001 = CARTESIAN_POINT ( 'NONE',  ( 35.00000000000000000, 1.171570255487609291, 11.68758509253246380 ) ) ;
#46002 = CIRCLE ( 'NONE', #17335, 2.899999999999994582 ) ;
#46003 = CARTESIAN_POINT ( 'NONE',  ( 2.241352910868908310, 0.08337961031714861970, -7.633946224498473043 ) ) ;
#46004 = DIRECTION ( 'NONE',  ( 0.000000000000000000, 0.6269146997507987207, 0.7790879021242507196 ) ) ;
#46005 = EDGE_LOOP ( 'NONE', ( #27400, #3995, #61254, #27712 ) ) ;
#46006 = CARTESIAN_POINT ( 'NONE',  ( -37.00000000000000711, 11.37311665002359540, 2.936739658820077370 ) ) ;
#46007 = CARTESIAN_POINT ( 'NONE',  ( -35.00000000000000000, 0.000000000000000000, 0.000000000000000000 ) ) ;
#46008 = CARTESIAN_POINT ( 'NONE',  ( 1.020182472823635500, -3.852445298735368784, -11.88926988382057282 ) ) ;
#46009 = VECTOR ( 'NONE', #49531, 1000.000000000000000 ) ;
#46010 = AXIS2_PLACEMENT_3D ( 'NONE', #45120, #39798, #9198 ) ;
#46011 = EDGE_CURVE ( 'NONE', #40836, #7740, #38996, .T. ) ;
#46012 = FACE_OUTER_BOUND ( 'NONE', #38237, .T. ) ;
#46013 = CARTESIAN_POINT ( 'NONE',  ( 0.2646305136544065406, -10.67138229758225343, -6.008537389229527292 ) ) ;
#46014 = AXIS2_PLACEMENT_3D ( 'NONE', #58299, #63585, #47998 ) ;
#46015 = ORIENTED_EDGE ( 'NONE', *, *, #19786, .T. ) ;
#46016 = EDGE_CURVE ( 'NONE', #8079, #11936, #27315, .T. ) ;
#46017 = CARTESIAN_POINT ( 'NONE',  ( 37.00000000000000711, -10.70999494708488520, 5.814360711498399503 ) ) ;
#46018 = CARTESIAN_POINT ( 'NONE',  ( -37.00000000000000711, 11.32068061209295529, 5.865551165831118574 ) ) ;
#46019 = VECTOR ( 'NONE', #675, 1000.000000000000000 ) ;
#46020 = DIRECTION ( 'NONE',  ( 0.000000000000000000, 0.000000000000000000, -1.000000000000000000 ) ) ;
#46021 = ORIENTED_EDGE ( 'NONE', *, *, #30308, .T. ) ;
#46022 = CARTESIAN_POINT ( 'NONE',  ( 2.305787727787084407, -6.545285700970554288, 3.971363876083942035 ) ) ;
#46023 = CARTESIAN_POINT ( 'NONE',  ( 37.00000000000000711, 7.718225330433935660, 9.430788938293964918 ) ) ;
#46024 = EDGE_CURVE ( 'NONE', #59239, #21159, #64472, .T. ) ;
#46025 = ORIENTED_EDGE ( 'NONE', *, *, #24222, .T. ) ;
#46026 = ORIENTED_EDGE ( 'NONE', *, *, #53397, .F. ) ;
#46027 = ORIENTED_EDGE ( 'NONE', *, *, #61526, .T. ) ;
#46028 = EDGE_CURVE ( 'NONE', #57486, #58933, #32614, .T. ) ;
#46029 = ORIENTED_EDGE ( 'NONE', *, *, #63412, .T. ) ;
#46030 = DIRECTION ( 'NONE',  ( 0.000000000000000000, 0.01356324068817998940, -0.9999080150203989437 ) ) ;
#46031 = DIRECTION ( 'NONE',  ( 0.000000000000000000, 0.000000000000000000, 1.000000000000000000 ) ) ;
#46032 = CYLINDRICAL_SURFACE ( 'NONE', #14184, 12.75000000000000178 ) ;
#46033 = DIRECTION ( 'NONE',  ( -0.000000000000000000, -1.000000000000000000, -0.000000000000000000 ) ) ;
#46034 =( BOUNDED_SURFACE ( )  B_SPLINE_SURFACE ( 3, 1, ( 
 ( #27100, #61675 ),
 ( #16134, #41729 ),
 ( #21458, #62023 ),
 ( #25795, #11463 ) ),
 .UNSPECIFIED., .F., .F., .F. ) 
 B_SPLINE_SURFACE_WITH_KNOTS ( ( 4, 4 ),
 ( 2, 2 ),
 ( 0.000000000000000000, 1.000000000000000000 ),
 ( 0.000000000000000000, 1.000000000000000000 ),
 .UNSPECIFIED. ) 
 GEOMETRIC_REPRESENTATION_ITEM ( )  RATIONAL_B_SPLINE_SURFACE ( (
 ( 1.000000000000000000, 1.000000000000000000),
 ( 0.9257577194822556033, 0.9980522942447415113),
 ( 0.9257577194822556033, 0.9980522942447415113),
 ( 1.000000000000000000, 1.000000000000000000) ) ) 
 REPRESENTATION_ITEM ( '' )  SURFACE ( )  );
#46035 = CARTESIAN_POINT ( 'NONE',  ( 2.889800649504073782, -2.156828754871506604, 5.728825117897699215 ) ) ;
#46036 = ADVANCED_FACE ( 'NONE', ( #44163 ), #13877, .T. ) ;
#46037 = CARTESIAN_POINT ( 'NONE',  ( 0.3341166715381324592, -10.74942732659227751, -5.914486946114021926 ) ) ;
#46039 = ORIENTED_EDGE ( 'NONE', *, *, #61841, .T. ) ;
#46038 = DIRECTION ( 'NONE',  ( 0.000000000000000000, 0.000000000000000000, -1.000000000000000000 ) ) ;
#46040 = PLANE ( 'NONE',  #16109 ) ;
#46041 = VERTEX_POINT ( 'NONE', #3941 ) ;
#46042 = VECTOR ( 'NONE', #39933, 1000.000000000000000 ) ;
#46043 = CYLINDRICAL_SURFACE ( 'NONE', #43383, 12.75000000000000178 ) ;
#46044 = VERTEX_POINT ( 'NONE', #19218 ) ;
#46045 = AXIS2_PLACEMENT_3D ( 'NONE', #9073, #34651, #34968 ) ;
#46046 = ORIENTED_EDGE ( 'NONE', *, *, #2463, .F. ) ;
#46047 = CARTESIAN_POINT ( 'NONE',  ( 0.3160775863651184570, 9.546663463486153134, -7.697077652699344519 ) ) ;
#46048 = ADVANCED_FACE ( 'NONE', ( #39492 ), #59789, .F. ) ;
#46049 = CARTESIAN_POINT ( 'NONE',  ( 8.782331025771487276, -31.88110954670732866, 13.48440172003490289 ) ) ;
#46051 = CARTESIAN_POINT ( 'NONE',  ( -10.48620311856347875, -9.720786832536937538, -7.036071585506805448 ) ) ;
#46050 = AXIS2_PLACEMENT_3D ( 'NONE', #52058, #15799, #36077 ) ;
#46052 = AXIS2_PLACEMENT_3D ( 'NONE', #233, #14506, #29807 ) ;
#46053 = DIRECTION ( 'NONE',  ( 1.000000000000000000, 0.000000000000000000, -0.000000000000000000 ) ) ;
#46054 = CARTESIAN_POINT ( 'NONE',  ( -35.00000000000000000, 2.497432891017006718, -11.47758908105691766 ) ) ;
#46055 = CARTESIAN_POINT ( 'NONE',  ( 0.2915757698887282423, -12.02962099476165392, 2.339174865979246398 ) ) ;
#46057 = EDGE_LOOP ( 'NONE', ( #46530, #2607, #64214, #29552 ) ) ;
#46056 = EDGE_CURVE ( 'NONE', #60869, #57837, #19912, .T. ) ;
#46058 = EDGE_LOOP ( 'NONE', ( #28645, #5824, #65403, #65014 ) ) ;
#46059 = CARTESIAN_POINT ( 'NONE',  ( 1.000000000000000888, -7.493043167941613625, 0.3229614270519164942 ) ) ;
#46060 = ORIENTED_EDGE ( 'NONE', *, *, #61208, .T. ) ;
#46061 = AXIS2_PLACEMENT_3D ( 'NONE', #22256, #37885, #12942 ) ;
#46062 = EDGE_CURVE ( 'NONE', #15837, #46970, #4102, .T. ) ;
#46063 = B_SPLINE_CURVE_WITH_KNOTS ( 'NONE', 3,
 ( #49022, #3480, #39336, #33379, #63616, #54669, #27723, #23748, #23080, #43339, #44017, #64290, #58677, #48027, #59308, #13734, #18089, #34017, #54334, #38356, #22762, #19071 ),
 .UNSPECIFIED., .F., .F.,
 ( 4, 3, 3, 3, 3, 3, 3, 4 ),
 ( 0.000000000000000000, 4.447697177976273769E-05, 6.624143997791219474E-05, 8.800576886944384261E-05, 0.0001097699864780899689, 0.0001315341395364383575, 0.0001760120188223303806, 0.0001867971373174759061 ),
 .UNSPECIFIED. ) ;
#46064 = VERTEX_POINT ( 'NONE', #56428 ) ;
#46065 = CIRCLE ( 'NONE', #25883, 12.74999999999999822 ) ;
#46066 = DIRECTION ( 'NONE',  ( 1.000000000000000000, 0.000000000000000000, 0.000000000000000000 ) ) ;
#46067 = CARTESIAN_POINT ( 'NONE',  ( 1.372161826076370383, -10.61825687422744124, 6.811451307636625430 ) ) ;
#46068 = CARTESIAN_POINT ( 'NONE',  ( 0.2657645697724685951, 0.1513403555227276764, -12.24540328300721725 ) ) ;
#46069 = CARTESIAN_POINT ( 'NONE',  ( 17.20489889795780769, -8.941181588450204387, 8.020780947141853190 ) ) ;
#46070 = CARTESIAN_POINT ( 'NONE',  ( 2.245754705088395031, 7.635057163463317309, 0.1113317465207070839 ) ) ;
#46071 = VECTOR ( 'NONE', #795, 1000.000000000000000 ) ;
#46072 = DIRECTION ( 'NONE',  ( 1.000000000000000000, 0.000000000000000000, 0.000000000000000000 ) ) ;
#46073 = VECTOR ( 'NONE', #10042, 1000.000000000000000 ) ;
#46074 = ORIENTED_EDGE ( 'NONE', *, *, #58476, .F. ) ;
#46075 = VECTOR ( 'NONE', #16198, 1000.000000000000000 ) ;
#46076 = CYLINDRICAL_SURFACE ( 'NONE', #11556, 5.000000000000000888 ) ;
#46077 = CARTESIAN_POINT ( 'NONE',  ( 2.241317068080785901, 7.501982551779192043, -1.415707718487429823 ) ) ;
#46078 = CARTESIAN_POINT ( 'NONE',  ( 1.719304012343089161, 12.64775761152706401, -1.452142814147889816 ) ) ;
#46079 = EDGE_CURVE ( 'NONE', #49417, #16846, #34809, .T. ) ;
#46080 = CARTESIAN_POINT ( 'NONE',  ( 6.769303024027612636, -6.819793210492989033, 9.875810308326745002 ) ) ;
#46081 = CIRCLE ( 'NONE', #27996, 12.74999999999999822 ) ;
#46082 = CARTESIAN_POINT ( 'NONE',  ( -17.83419946441818027, -9.720786832536937538, 25.00000000000000000 ) ) ;
#46083 = CARTESIAN_POINT ( 'NONE',  ( 0.3665391374699464300, -9.237363111276710725, -8.095513416941326312 ) ) ;
#46084 = CARTESIAN_POINT ( 'NONE',  ( 0.7446945582529461705, 2.504154979876664910, -12.15064199164638126 ) ) ;
#46085 = FACE_OUTER_BOUND ( 'NONE', #25084, .T. ) ;
#46086 = ORIENTED_EDGE ( 'NONE', *, *, #13218, .T. ) ;
#46087 = CIRCLE ( 'NONE', #5759, 12.73084802173761787 ) ;
#46088 = CARTESIAN_POINT ( 'NONE',  ( 0.2653519991613820239, 10.59450977800982230, 6.142165520908205778 ) ) ;
#46089 = CARTESIAN_POINT ( 'NONE',  ( 2.556980015514295435, 1.116161541731621520, -7.658710847181731118 ) ) ;
#46090 = EDGE_CURVE ( 'NONE', #14897, #52497, #60768, .T. ) ;
#46091 = AXIS2_PLACEMENT_3D ( 'NONE', #39486, #13556, #54802 ) ;
#46092 = CARTESIAN_POINT ( 'NONE',  ( 14.33157020396088832, -34.50275931095601578, 8.076358832431466794 ) ) ;
#46093 = VECTOR ( 'NONE', #17047, 1000.000000000000000 ) ;
#46094 = EDGE_CURVE ( 'NONE', #7532, #53819, #12787, .T. ) ;
#46095 = CARTESIAN_POINT ( 'NONE',  ( -6.824045466202398380, -31.96248520358999201, -13.34027024243112791 ) ) ;
#46096 = FACE_OUTER_BOUND ( 'NONE', #19241, .T. ) ;
#46097 = CIRCLE ( 'NONE', #63074, 12.18649999999999878 ) ;
#46098 = ORIENTED_EDGE ( 'NONE', *, *, #3843, .T. ) ;
#46099 = CARTESIAN_POINT ( 'NONE',  ( -27.32343372485684796, -2.534722478175144289, -1.625341394141124773 ) ) ;
#46100 = CARTESIAN_POINT ( 'NONE',  ( -27.01437459610461644, 25.00000000000000000, -8.240233560378637634 ) ) ;
#46101 = CIRCLE ( 'NONE', #35442, 2.899999999999994582 ) ;
#46102 = CARTESIAN_POINT ( 'NONE',  ( 11.58535936493820273, -27.13779202276463920, -13.20710129366601926 ) ) ;
#46103 = VERTEX_POINT ( 'NONE', #55449 ) ;
#46104 = CARTESIAN_POINT ( 'NONE',  ( 1.719304012339833099, -9.242227816401946683, 8.755325027794301107 ) ) ;
#46105 = CARTESIAN_POINT ( 'NONE',  ( -14.74450257587757029, 7.920733541773330444, -9.014605533771735679 ) ) ;
#46106 = CARTESIAN_POINT ( 'NONE',  ( 37.00000000000000711, 4.705694406421931860E-17, -3.469127814946512892E-15 ) ) ;
#46107 = ADVANCED_FACE ( 'NONE', ( #30493 ), #36120, .T. ) ;
#46108 = VECTOR ( 'NONE', #56352, 1000.000000000000000 ) ;
#46110 = EDGE_LOOP ( 'NONE', ( #64197, #53894, #20642, #6956 ) ) ;
#46109 = CARTESIAN_POINT ( 'NONE',  ( 2.705197763288543555, 1.076142490489871317, 7.714317563576063463 ) ) ;
#46111 = DIRECTION ( 'NONE',  ( 0.000000000000000000, 0.01356324068817992001, -0.9999080150203990547 ) ) ;
#46112 = AXIS2_PLACEMENT_3D ( 'NONE', #31432, #6832, #62997 ) ;
#46113 = CARTESIAN_POINT ( 'NONE',  ( 35.00000000000000000, -5.143145423404194894, 11.66664283989685025 ) ) ;
#46114 = ORIENTED_EDGE ( 'NONE', *, *, #62170, .F. ) ;
#46115 = CARTESIAN_POINT ( 'NONE',  ( 0.3053067050349148603, 7.702091166066015404, 9.538004819224376263 ) ) ;
#46116 = CARTESIAN_POINT ( 'NONE',  ( -27.09150307427401216, 1.305148381378462563, 1.909742362149637440 ) ) ;
#46117 = CARTESIAN_POINT ( 'NONE',  ( 0.2653141617321028156, -7.905395731875554333, 9.352766656400028467 ) ) ;
#46118 = CARTESIAN_POINT ( 'NONE',  ( -37.00000000000000711, 0.000000000000000000, -1.750000000000000000 ) ) ;
#46119 = VECTOR ( 'NONE', #400, 1000.000000000000000 ) ;
#46120 = CARTESIAN_POINT ( 'NONE',  ( 35.00000000000000000, -2.185196060783960892, -11.54110654723648466 ) ) ;
#46121 = CARTESIAN_POINT ( 'NONE',  ( 0.3675815128205912052, 11.44679196252415210, -4.447030445008065769 ) ) ;
#46122 = VERTEX_POINT ( 'NONE', #61094 ) ;
#46123 = DIRECTION ( 'NONE',  ( -1.000000000000000000, -0.000000000000000000, 0.000000000000000000 ) ) ;
#46124 = ORIENTED_EDGE ( 'NONE', *, *, #38002, .T. ) ;
#46125 = CARTESIAN_POINT ( 'NONE',  ( 35.00000000000000000, -1.488153103996881610, 11.65150730582935701 ) ) ;
#46126 = EDGE_CURVE ( 'NONE', #57990, #57528, #15526, .T. ) ;
#46127 = CARTESIAN_POINT ( 'NONE',  ( 0.3278977287071177527, 11.44003061923231535, 4.427879319182928874 ) ) ;
#46128 = CONICAL_SURFACE ( 'NONE', #12118, 7.938172270156617749, 1.280189991382167047 ) ;
#46129 = EDGE_CURVE ( 'NONE', #51211, #24505, #4030, .T. ) ;
#46130 = DIRECTION ( 'NONE',  ( 0.000000000000000000, 0.000000000000000000, 1.000000000000000000 ) ) ;
#46131 = ORIENTED_EDGE ( 'NONE', *, *, #63153, .T. ) ;
#46132 = CARTESIAN_POINT ( 'NONE',  ( 0.2638984909335716500, -10.50550771760515545, -6.295352574289097447 ) ) ;
#46133 = DIRECTION ( 'NONE',  ( -1.000000000000000000, 0.000000000000000000, 0.000000000000000000 ) ) ;
#46134 = CARTESIAN_POINT ( 'NONE',  ( -22.27722022243423794, -1.227876413014574952, 3.470949075637804970 ) ) ;
#46135 = ORIENTED_EDGE ( 'NONE', *, *, #48168, .F. ) ;
#46136 = ORIENTED_EDGE ( 'NONE', *, *, #23419, .F. ) ;
#46137 = EDGE_CURVE ( 'NONE', #22708, #34425, #31873, .T. ) ;
#46138 = CARTESIAN_POINT ( 'NONE',  ( 29.21347414222148942, -9.161122334729320471, 9.924607052662393514 ) ) ;
#46139 = CIRCLE ( 'NONE', #17458, 12.75000000000000178 ) ;
#46140 = AXIS2_PLACEMENT_3D ( 'NONE', #21563, #36838, #6599 ) ;
#46141 = ORIENTED_EDGE ( 'NONE', *, *, #26334, .T. ) ;
#46142 = CARTESIAN_POINT ( 'NONE',  ( 22.11355691832442005, -11.89259483616537594, -1.644240265049296879 ) ) ;
#46143 = CARTESIAN_POINT ( 'NONE',  ( 5.530133899448235191, 0.01536822665454895542, -0.004396748047611278437 ) ) ;
#46144 = CARTESIAN_POINT ( 'NONE',  ( -27.09048036756592026, 2.303144499688039470, -0.1785511875142904714 ) ) ;
#46145 = CARTESIAN_POINT ( 'NONE',  ( -28.62125010117446777, 3.140874940710094876, 11.58806648538879358 ) ) ;
#46146 = CARTESIAN_POINT ( 'NONE',  ( -35.00000000000000000, 3.340853584269533716, 11.26103545359857350 ) ) ;
#46147 = CARTESIAN_POINT ( 'NONE',  ( 0.000000000000000000, 0.000000000000000000, 0.000000000000000000 ) ) ;
#46148 = CARTESIAN_POINT ( 'NONE',  ( -37.00000000000000711, 11.13736569743281457, -4.946702696913053643 ) ) ;
#46149 = ORIENTED_EDGE ( 'NONE', *, *, #63940, .T. ) ;
#46150 = CARTESIAN_POINT ( 'NONE',  ( 36.00000000000000711, 10.49626516989280844, 7.238157050195514586 ) ) ;
#46151 = PRODUCT_DEFINITION_SHAPE ( 'NONE', 'NONE',  #65808 ) ;
#46152 = CARTESIAN_POINT ( 'NONE',  ( 21.97631981833123049, 11.77024062219680012, -2.366125064793188848 ) ) ;
#46153 = DIRECTION ( 'NONE',  ( 0.000000000000000000, 0.01356324068818000328, -0.9999080150203990547 ) ) ;
#46154 = DIRECTION ( 'NONE',  ( 0.000000000000000000, 0.000000000000000000, 1.000000000000000000 ) ) ;
#46155 = DIRECTION ( 'NONE',  ( 0.000000000000000000, -0.04924826701373154203, -0.9987865678893285137 ) ) ;
#46156 = CARTESIAN_POINT ( 'NONE',  ( 0.3057689695767532578, -10.73077184758787617, -5.928746590069690292 ) ) ;
#46157 = CARTESIAN_POINT ( 'NONE',  ( 2.034671305880252135, 10.71175679137217784, 4.647127512368699698 ) ) ;
#46158 = DIRECTION ( 'NONE',  ( -1.000000000000000000, 0.000000000000000000, 0.000000000000000000 ) ) ;
#46159 = AXIS2_PLACEMENT_3D ( 'NONE', #29482, #49784, #4235 ) ;
#46160 = EDGE_CURVE ( 'NONE', #60006, #42211, #62724, .T. ) ;
#46161 = ORIENTED_EDGE ( 'NONE', *, *, #42492, .T. ) ;
#46162 = DIRECTION ( 'NONE',  ( 0.000000000000000000, 0.000000000000000000, 1.000000000000000000 ) ) ;
#46163 = EDGE_CURVE ( 'NONE', #22582, #47105, #839, .T. ) ;
#46164 = ORIENTED_EDGE ( 'NONE', *, *, #23972, .T. ) ;
#46165 = CARTESIAN_POINT ( 'NONE',  ( 35.00000000000000000, 3.033604067594578790, -12.38385022362083276 ) ) ;
#46166 = LINE ( 'NONE', #36824, #19740 ) ;
#46167 = DIRECTION ( 'NONE',  ( -1.000000000000000000, -0.000000000000000000, -0.000000000000000000 ) ) ;
#46168 = DIRECTION ( 'NONE',  ( -1.000000000000000000, 0.000000000000000000, 0.000000000000000000 ) ) ;
#46169 = VERTEX_POINT ( 'NONE', #2221 ) ;
#46170 = DIRECTION ( 'NONE',  ( 1.000000000000000000, -0.000000000000000000, 0.000000000000000000 ) ) ;
#46171 = CARTESIAN_POINT ( 'NONE',  ( 0.000000000000000000, 0.000000000000000000, 0.000000000000000000 ) ) ;
#46172 = EDGE_CURVE ( 'NONE', #48483, #35632, #34791, .T. ) ;
#46173 = CARTESIAN_POINT ( 'NONE',  ( 3.031336079629786795, -0.9593005538805217114, 7.839300734793265057 ) ) ;
#46174 = CARTESIAN_POINT ( 'NONE',  ( -22.59983133926799326, 3.996991822164152719, 2.378226455340815448 ) ) ;
#46175 = AXIS2_PLACEMENT_3D ( 'NONE', #20547, #10544, #30822 ) ;
#46176 = DIRECTION ( 'NONE',  ( 0.000000000000000000, -0.01356324068817992175, 0.9999080150203990547 ) ) ;
#46177 = DIRECTION ( 'NONE',  ( 0.9606638835031803270, -0.02862840969242716124, -0.2762341707520462042 ) ) ;
#46178 = ORIENTED_EDGE ( 'NONE', *, *, #44799, .T. ) ;
#46179 = CARTESIAN_POINT ( 'NONE',  ( 0.000000000000000000, -6.164400007374764456, -2.900694413976575792 ) ) ;
#46180 = ORIENTED_EDGE ( 'NONE', *, *, #40149, .F. ) ;
#46181 = FACE_OUTER_BOUND ( 'NONE', #30181, .T. ) ;
#46182 = DIRECTION ( 'NONE',  ( -1.000000000000000000, 0.000000000000000000, 0.000000000000000000 ) ) ;
#46183 = ADVANCED_FACE ( 'NONE', ( #42415 ), #22495, .T. ) ;
#46184 = STYLED_ITEM ( 'NONE', ( #47508 ), #37239 ) ;
#46185 = CARTESIAN_POINT ( 'NONE',  ( -30.15636683828732245, -0.5078987883301536721, -13.49786359043454986 ) ) ;
#46186 = B_SPLINE_CURVE_WITH_KNOTS ( 'NONE', 3,
 ( #49380, #54349, #18768, #63630, #43691, #49676, #19425, #9102, #33396, #64303, #8132, #23765, #28728, #18459, #33713, #64612, #59016, #59323, #3494, #59654, #63978, #9406, #50003, #24076, #18105, #4120, #48700, #4462 ),
 .UNSPECIFIED., .F., .F.,
 ( 4, 2, 2, 2, 2, 2, 2, 2, 2, 2, 2, 2, 2, 4 ),
 ( 0.003178514824100456618, 0.003833261448045587744, 0.004488008071990718870, 0.005142754695935849996, 0.005797501319880981122, 0.007106994567771237302, 0.007761741191716364958, 0.008416487815661493482, 0.009725981063551748795, 0.01038072768749687645, 0.01103547431144200411, 0.01169022093538713003, 0.01234496755933225769, 0.01365446080722251126 ),
 .UNSPECIFIED. ) ;
#46187 = EDGE_CURVE ( 'NONE', #11911, #61252, #41787, .T. ) ;
#46188 = CARTESIAN_POINT ( 'NONE',  ( 0.3053067050349194678, -11.59706307017085791, 3.975408458060472938 ) ) ;
#46189 = VERTEX_POINT ( 'NONE', #11847 ) ;
#46190 = ORIENTED_EDGE ( 'NONE', *, *, #14415, .T. ) ;
#46191 = DIRECTION ( 'NONE',  ( -1.000000000000000000, -0.000000000000000000, 0.000000000000000000 ) ) ;
#46192 = ORIENTED_EDGE ( 'NONE', *, *, #17607, .F. ) ;
#46193 = CARTESIAN_POINT ( 'NONE',  ( 2.241311220309555541, -6.564680916077770156, -3.897297589552050301 ) ) ;
#46195 = VECTOR ( 'NONE', #65352, 1000.000000000000000 ) ;
#46194 = CARTESIAN_POINT ( 'NONE',  ( -35.04582288351658548, -0.01107592729725561699, -0.006225574250545745821 ) ) ;
#46196 = CARTESIAN_POINT ( 'NONE',  ( -22.27719443589224113, -3.500848524682613760, -1.139586749255983911 ) ) ;
#46197 = CARTESIAN_POINT ( 'NONE',  ( -35.00000000000000000, 0.000000000000000000, 0.000000000000000000 ) ) ;
#46198 = DIRECTION ( 'NONE',  ( 1.000000000000000000, 0.000000000000000000, 0.000000000000000000 ) ) ;
#46199 = CARTESIAN_POINT ( 'NONE',  ( 0.6511581176972721652, 10.87850887236121977, -5.898618881004612291 ) ) ;
#46200 = CARTESIAN_POINT ( 'NONE',  ( 1.287602823390032958, 12.47973441446294807, -1.639728374784856113 ) ) ;
#46201 = EDGE_LOOP ( 'NONE', ( #60860, #9259, #5320, #15103 ) ) ;
#46202 = CARTESIAN_POINT ( 'NONE',  ( -8.434691090653316792, -7.831301396948528115, -9.099002668205912414 ) ) ;
#46203 = ORIENTED_EDGE ( 'NONE', *, *, #9759, .T. ) ;
#46204 = CARTESIAN_POINT ( 'NONE',  ( -22.27720412283625961, 2.444672752438211916, 2.752887114864203788 ) ) ;
#46205 = EDGE_CURVE ( 'NONE', #36007, #52324, #25224, .T. ) ;
#46207 = CARTESIAN_POINT ( 'NONE',  ( 0.2958664285830445717, -9.245659426743934262, 8.045892866065326388 ) ) ;
#46206 = AXIS2_PLACEMENT_3D ( 'NONE', #21412, #41687, #61977 ) ;
#46208 = CARTESIAN_POINT ( 'NONE',  ( 18.84867683979355846, 5.944105725974518251, 12.12095735156415088 ) ) ;
#46209 = ORIENTED_EDGE ( 'NONE', *, *, #30224, .T. ) ;
#46210 = EDGE_CURVE ( 'NONE', #31440, #30237, #63055, .T. ) ;
#46211 = CARTESIAN_POINT ( 'NONE',  ( -16.47895549814540672, -34.42947327577542893, 6.127516784536641836 ) ) ;
#46212 = ORIENTED_EDGE ( 'NONE', *, *, #45762, .T. ) ;
#46213 = CARTESIAN_POINT ( 'NONE',  ( 1.948354844648340745, 11.88693049003635238, 1.364409644998757276 ) ) ;
#46214 = CYLINDRICAL_SURFACE ( 'NONE', #56216, 12.18650000000000055 ) ;
#46215 = CARTESIAN_POINT ( 'NONE',  ( 2.781367136452389310, 2.960151187465042355, 7.232043329634182172 ) ) ;
#46216 = CARTESIAN_POINT ( 'NONE',  ( -40.83349710434619340, -1.696348104764183962, -18.10529304745324097 ) ) ;
#46217 = VERTEX_POINT ( 'NONE', #32769 ) ;
#46218 = ORIENTED_EDGE ( 'NONE', *, *, #36465, .T. ) ;
#46219 = ADVANCED_FACE ( 'NONE', ( #46779 ), #46450, .T. ) ;
#46220 = CARTESIAN_POINT ( 'NONE',  ( 1.275613388608518362, 1.084079264376230256, 13.45952210748621170 ) ) ;
#46221 = ORIENTED_EDGE ( 'NONE', *, *, #5650, .F. ) ;
#46222 = CARTESIAN_POINT ( 'NONE',  ( 0.2676618633000479863, 11.56235835488945973, -4.037335446657117188 ) ) ;
#46223 = ORIENTED_EDGE ( 'NONE', *, *, #62442, .F. ) ;
#46224 = EDGE_LOOP ( 'NONE', ( #26568, #32201, #32594, #55017 ) ) ;
#46225 = ORIENTED_EDGE ( 'NONE', *, *, #23729, .T. ) ;
#46226 = DIRECTION ( 'NONE',  ( 1.000000000000000000, 0.000000000000000000, 0.000000000000000000 ) ) ;
#46227 = CARTESIAN_POINT ( 'NONE',  ( 1.198791140417288847, 11.61358959650646483, 4.776130053251955943 ) ) ;
#46228 = AXIS2_PLACEMENT_3D ( 'NONE', #62903, #6093, #12355 ) ;
#46229 = FACE_OUTER_BOUND ( 'NONE', #51149, .T. ) ;
#46230 = CARTESIAN_POINT ( 'NONE',  ( -7.181456785175555524, 8.540743096806467705, -10.45493698471458188 ) ) ;
#46231 = EDGE_LOOP ( 'NONE', ( #35690, #5261, #43776, #6634 ) ) ;
#46232 = CARTESIAN_POINT ( 'NONE',  ( 2.258463476536303638, -2.484972401833594358, -7.224688073723371851 ) ) ;
#46233 =( BOUNDED_SURFACE ( )  B_SPLINE_SURFACE ( 3, 1, ( 
 ( #35209, #24259 ),
 ( #40879, #64806 ),
 ( #25572, #9958 ),
 ( #45517, #40196 ) ),
 .UNSPECIFIED., .F., .F., .F. ) 
 B_SPLINE_SURFACE_WITH_KNOTS ( ( 4, 4 ),
 ( 2, 2 ),
 ( 0.000000000000000000, 1.000000000000000000 ),
 ( 0.000000000000000000, 1.000000000000000000 ),
 .UNSPECIFIED. ) 
 GEOMETRIC_REPRESENTATION_ITEM ( )  RATIONAL_B_SPLINE_SURFACE ( (
 ( 1.000000000000000000, 1.000000000000000000),
 ( 0.8716676215708681896, 0.8964445200148164483),
 ( 0.8716676215708681896, 0.8964445200148164483),
 ( 1.000000000000000000, 1.000000000000000000) ) ) 
 REPRESENTATION_ITEM ( '' )  SURFACE ( )  );
#46234 = ORIENTED_EDGE ( 'NONE', *, *, #2086, .T. ) ;
#46235 = DIRECTION ( 'NONE',  ( 1.000000000000000000, 0.000000000000000000, 0.000000000000000000 ) ) ;
#46236 = DIRECTION ( 'NONE',  ( 0.000000000000000000, -0.01356324068817991828, 0.9999080150203990547 ) ) ;
#46237 = DIRECTION ( 'NONE',  ( -1.000000000000000000, 0.000000000000000000, 0.000000000000000000 ) ) ;
#46238 = CIRCLE ( 'NONE', #4223, 12.18650000000000055 ) ;
#46239 = CARTESIAN_POINT ( 'NONE',  ( 5.520433897694421610, 0.01186170453199860732, 0.009283255140285660498 ) ) ;
#46240 = CARTESIAN_POINT ( 'NONE',  ( -29.68541646480307250, -1.416020129149132334, 25.00000000000000000 ) ) ;
#46241 = DIRECTION ( 'NONE',  ( -1.000000000000000000, 0.000000000000000000, 0.000000000000000000 ) ) ;
#46242 = VERTEX_POINT ( 'NONE', #27157 ) ;
#46243 = DIRECTION ( 'NONE',  ( 1.000000000000000000, -0.000000000000000000, 0.000000000000000000 ) ) ;
#46244 = EDGE_CURVE ( 'NONE', #62469, #34225, #54985, .T. ) ;
#46245 = AXIS2_PLACEMENT_3D ( 'NONE', #47552, #33569, #1997 ) ;
#46246 = VERTEX_POINT ( 'NONE', #899 ) ;
#46247 = CARTESIAN_POINT ( 'NONE',  ( -41.00000000000000711, -25.03188948156373073, -4.500000000000008882 ) ) ;
#46248 = CARTESIAN_POINT ( 'NONE',  ( -13.26546321032139986, -27.53582555932707976, -12.33704161722047488 ) ) ;
#46249 = CARTESIAN_POINT ( 'NONE',  ( 5.527856869237428583, -26.90719658711817885, 15.68471180892751526 ) ) ;
#46250 = FACE_OUTER_BOUND ( 'NONE', #28952, .T. ) ;
#46251 = DIRECTION ( 'NONE',  ( 0.000000000000000000, 0.000000000000000000, 1.000000000000000000 ) ) ;
#46252 = ORIENTED_EDGE ( 'NONE', *, *, #51640, .T. ) ;
#46253 = CARTESIAN_POINT ( 'NONE',  ( 22.57855258442565116, 3.026812727784649493, 25.00000000000000000 ) ) ;
#46254 = DIRECTION ( 'NONE',  ( 1.000000000000000000, 0.000000000000000000, 0.000000000000000000 ) ) ;
#46255 = CARTESIAN_POINT ( 'NONE',  ( 22.21785366982988918, 10.35091871611333936, -6.082120259086551073 ) ) ;
#46256 = CARTESIAN_POINT ( 'NONE',  ( 23.18962579211675390, -11.76234302143509680, -6.631918700726934901 ) ) ;
#46257 = B_SPLINE_CURVE_WITH_KNOTS ( 'NONE', 3,
 ( #34902, #60865, #14623, #354, #7, #35890, #20293, #39915, #20635, #55210, #55552, #51233, #5683, #9312 ),
 .UNSPECIFIED., .F., .F.,
 ( 4, 2, 2, 2, 2, 2, 4 ),
 ( 0.000000000000000000, 0.001702703996761801208, 0.002554055995142702137, 0.003405407993523602416, 0.004256759991904502695, 0.005108111990285404275, 0.006810815987047202230 ),
 .UNSPECIFIED. ) ;
#46258 = CIRCLE ( 'NONE', #51583, 5.000000000000000000 ) ;
#46259 = EDGE_CURVE ( 'NONE', #1482, #52904, #37454, .T. ) ;
#46260 = DIRECTION ( 'NONE',  ( 1.000000000000000000, -0.000000000000000000, 0.000000000000000000 ) ) ;
#46261 = LINE ( 'NONE', #15962, #51912 ) ;
#46263 = EDGE_CURVE ( 'NONE', #63438, #18084, #21173, .T. ) ;
#46262 = CARTESIAN_POINT ( 'NONE',  ( 5.520433897694421610, 0.007082458259338205234, 0.01329351892497965086 ) ) ;
#46264 = CARTESIAN_POINT ( 'NONE',  ( 1.937114397841935398, 9.228205347192574237, -8.920887662793379747 ) ) ;
#46265 = CARTESIAN_POINT ( 'NONE',  ( 5.536195898058073439, -0.004027525919832385289, -0.007485416011287845603 ) ) ;
#46266 = ADVANCED_FACE ( 'NONE', ( #33461 ), #53751, .T. ) ;
#46267 = VECTOR ( 'NONE', #46321, 1000.000000000000000 ) ;
#46268 = ORIENTED_EDGE ( 'NONE', *, *, #20837, .F. ) ;
#46269 = ORIENTED_EDGE ( 'NONE', *, *, #43826, .F. ) ;
#46270 = FACE_OUTER_BOUND ( 'NONE', #16628, .T. ) ;
#46271 = CARTESIAN_POINT ( 'NONE',  ( 48.45393016956177945, -0.3105270330721123240, -5.105971556042214310 ) ) ;
#46272 = CARTESIAN_POINT ( 'NONE',  ( 3.100650473569671828, -7.585586315875718633, 2.280184661131201107 ) ) ;
#46273 = CARTESIAN_POINT ( 'NONE',  ( 0.2958664285830423513, -1.910785783655658765, 12.10650684287254464 ) ) ;
#46274 = ORIENTED_EDGE ( 'NONE', *, *, #59393, .T. ) ;
#46275 = ORIENTED_EDGE ( 'NONE', *, *, #5727, .F. ) ;
#46276 = VERTEX_POINT ( 'NONE', #28789 ) ;
#46277 = CARTESIAN_POINT ( 'NONE',  ( 2.899286259009686617, 7.845618522360458869, 0.3564726075923687620 ) ) ;
#46278 = EDGE_CURVE ( 'NONE', #39065, #2509, #14570, .T. ) ;
#46279 = LINE ( 'NONE', #20977, #41710 ) ;
#46280 = ORIENTED_EDGE ( 'NONE', *, *, #33769, .F. ) ;
#46281 = CARTESIAN_POINT ( 'NONE',  ( 6.661533233520610331, -4.211056110068226666, 12.82664335996205196 ) ) ;
#46282 = DIRECTION ( 'NONE',  ( -1.000000000000000000, 0.000000000000000000, 0.000000000000000000 ) ) ;
#46283 = ORIENTED_EDGE ( 'NONE', *, *, #1748, .F. ) ;
#46284 = VECTOR ( 'NONE', #18544, 1000.000000000000000 ) ;
#46285 = CARTESIAN_POINT ( 'NONE',  ( 2.241317068080786346, 4.836852665784303618, -5.906676463196497195 ) ) ;
#46286 = CARTESIAN_POINT ( 'NONE',  ( 13.26995653566893019, -33.36016745060648958, -10.56634385159335388 ) ) ;
#46287 = CYLINDRICAL_SURFACE ( 'NONE', #44054, 10.70557198542813815 ) ;
#46288 = ORIENTED_EDGE ( 'NONE', *, *, #49803, .F. ) ;
#46289 = CARTESIAN_POINT ( 'NONE',  ( -25.75517367794919465, 7.863739964200370025, 10.97545609339454664 ) ) ;
#46290 = ORIENTED_EDGE ( 'NONE', *, *, #18450, .T. ) ;
#46291 = CARTESIAN_POINT ( 'NONE',  ( 0.6473888112830226138, 7.698027285532596409, -9.687359867659717239 ) ) ;
#46292 = EDGE_LOOP ( 'NONE', ( #4486, #35837, #61655, #8832 ) ) ;
#46293 = VERTEX_POINT ( 'NONE', #34432 ) ;
#46294 = DIRECTION ( 'NONE',  ( -1.000000000000000000, 0.000000000000000000, 0.000000000000000000 ) ) ;
#46295 = CARTESIAN_POINT ( 'NONE',  ( -7.228961821822758260, -32.07041743672118628, 13.19626196499948634 ) ) ;
#46296 = CARTESIAN_POINT ( 'NONE',  ( 2.273267844204863497, 3.952852893982297555, 6.543821324256898109 ) ) ;
#46297 = EDGE_CURVE ( 'NONE', #27860, #34161, #17832, .T. ) ;
#46298 = CARTESIAN_POINT ( 'NONE',  ( 36.00000000000000711, -3.473736367725341001, -12.26766708251990501 ) ) ;
#46299 = CYLINDRICAL_SURFACE ( 'NONE', #38875, 13.50000000000000178 ) ;
#46300 = CARTESIAN_POINT ( 'NONE',  ( 25.05309951391468459, -10.77522019223763827, -8.132934882857099979 ) ) ;
#46301 = CARTESIAN_POINT ( 'NONE',  ( 0.000000000000000000, 6.935703035393448346, -0.1051458740707923722 ) ) ;
#46302 = CARTESIAN_POINT ( 'NONE',  ( -37.00000000000000711, 0.06441628369853459601, -12.18632975068353197 ) ) ;
#46304 = EDGE_LOOP ( 'NONE', ( #43965, #5001, #59182, #44985 ) ) ;
#46303 = CARTESIAN_POINT ( 'NONE',  ( 3.459614771489464946, -11.09853614738469396, 7.685863346768216253 ) ) ;
#46305 = DIRECTION ( 'NONE',  ( 0.000000000000000000, -0.01356324068817991828, 0.9999080150203990547 ) ) ;
#46306 = ORIENTED_EDGE ( 'NONE', *, *, #22629, .F. ) ;
#46307 = CARTESIAN_POINT ( 'NONE',  ( 12.14944607613469429, -13.35043466913572452, -2.010111617055820421 ) ) ;
#46308 = CARTESIAN_POINT ( 'NONE',  ( -35.00000000000000000, 0.000000000000000000, 0.000000000000000000 ) ) ;
#46309 = B_SPLINE_CURVE_WITH_KNOTS ( 'NONE', 3,
 ( #56866, #51220, #50876, #45890, #6311, #60851, #989, #50559, #15290, #35569, #11290, #5003, #19949, #60508, #40220, #45540 ),
 .UNSPECIFIED., .F., .F.,
 ( 4, 3, 3, 3, 3, 4 ),
 ( 2.641088042841306632E-15, 0.0002126834539180078596, 0.0004253519300367007835, 0.0006380165497225274117, 0.0007442707582429536686, 0.0009453531351409383840 ),
 .UNSPECIFIED. ) ;
#46310 = ORIENTED_EDGE ( 'NONE', *, *, #16371, .F. ) ;
#46311 = CARTESIAN_POINT ( 'NONE',  ( 36.00000000000000711, -9.196955404009232282, 8.830544224263041642 ) ) ;
#46312 = DIRECTION ( 'NONE',  ( 0.000000000000000000, 0.5767582926624912343, 0.8169148498130317515 ) ) ;
#46313 = CARTESIAN_POINT ( 'NONE',  ( 36.00000000000000711, -6.950793414699864670, -10.68873102412840304 ) ) ;
#46314 = FACE_OUTER_BOUND ( 'NONE', #41463, .T. ) ;
#46315 = CARTESIAN_POINT ( 'NONE',  ( 0.000000000000000000, 0.4129979343798200753, -6.800241778083709221 ) ) ;
#46316 = ORIENTED_EDGE ( 'NONE', *, *, #5099, .T. ) ;
#46317 = CARTESIAN_POINT ( 'NONE',  ( -17.37691089814359913, -8.897415436183450765, -8.081796101290189327 ) ) ;
#46318 = EDGE_CURVE ( 'NONE', #45959, #19382, #65556, .T. ) ;
#46319 = VERTEX_POINT ( 'NONE', #19139 ) ;
#46320 = CARTESIAN_POINT ( 'NONE',  ( 2.524535260911693335, 0.2211075636757951768, 7.725637239510134258 ) ) ;
#46321 = DIRECTION ( 'NONE',  ( 1.000000000000000000, 0.000000000000000000, 0.000000000000000000 ) ) ;
#46322 = EDGE_CURVE ( 'NONE', #15001, #48921, #33772, .T. ) ;
#46323 = DIRECTION ( 'NONE',  ( -1.000000000000000000, 0.000000000000000000, 0.000000000000000000 ) ) ;
#46324 = ORIENTED_EDGE ( 'NONE', *, *, #44285, .F. ) ;
#46325 = CARTESIAN_POINT ( 'NONE',  ( -27.10422407540547241, -1.039355862229903282, 2.109093808474363119 ) ) ;
#46326 = EDGE_CURVE ( 'NONE', #57839, #9138, #13482, .T. ) ;
#46327 = AXIS2_PLACEMENT_3D ( 'NONE', #47365, #7106, #27380 ) ;
#46328 = CARTESIAN_POINT ( 'NONE',  ( 24.90014556888634800, -8.538933172091784485, -8.433831666448899256 ) ) ;
#46329 = CARTESIAN_POINT ( 'NONE',  ( 47.76247274761329464, -0.4463159248369739651, -10.36992351718251015 ) ) ;
#46330 = CARTESIAN_POINT ( 'NONE',  ( 35.00000000000000000, 4.705694406421931860E-17, -3.469127814946512892E-15 ) ) ;
#46331 = CARTESIAN_POINT ( 'NONE',  ( 0.2706063244538051693, -5.971590789837440738, -10.69357582853952948 ) ) ;
#46332 = CARTESIAN_POINT ( 'NONE',  ( 0.2651627682582902712, 2.039709641845743437, -12.07509313786331084 ) ) ;
#46333 = EDGE_CURVE ( 'NONE', #8848, #29500, #23174, .T. ) ;
#46334 = FACE_OUTER_BOUND ( 'NONE', #1885, .T. ) ;
#46335 = CARTESIAN_POINT ( 'NONE',  ( -35.00000000000000000, 0.000000000000000000, 0.000000000000000000 ) ) ;
#46336 = ORIENTED_EDGE ( 'NONE', *, *, #1642, .T. ) ;
#46337 = CARTESIAN_POINT ( 'NONE',  ( -15.80994330493005329, 7.912403392364937282, 10.93820572742344233 ) ) ;
#46338 = CARTESIAN_POINT ( 'NONE',  ( 18.50840396092215201, -8.755750366309635879, 10.29967764056247503 ) ) ;
#46339 = VERTEX_POINT ( 'NONE', #24133 ) ;
#46340 = CARTESIAN_POINT ( 'NONE',  ( 2.406456491625306615, -6.212289237906496453, 8.382123850280477129 ) ) ;
#46341 = CARTESIAN_POINT ( 'NONE',  ( 2.712198850443733100, 3.199880535692022576, -11.57168736659367703 ) ) ;
#46342 = CARTESIAN_POINT ( 'NONE',  ( 5.536195898058073439, -0.005266167600747551948, -0.006672323185952767910 ) ) ;
#46343 = EDGE_LOOP ( 'NONE', ( #12754, #55984, #18477, #60454 ) ) ;
#46344 = CARTESIAN_POINT ( 'NONE',  ( 2.000000000000001776, -5.888698556700742159, -3.665823448873470003 ) ) ;
#46345 = DIRECTION ( 'NONE',  ( 0.000000000000000000, 0.000000000000000000, 1.000000000000000000 ) ) ;
#46346 = VERTEX_POINT ( 'NONE', #38099 ) ;
#46347 = VERTEX_POINT ( 'NONE', #48111 ) ;
#46348 = ORIENTED_EDGE ( 'NONE', *, *, #38027, .F. ) ;
#46349 = CARTESIAN_POINT ( 'NONE',  ( -27.28563798457902578, -1.413023339712117910, -2.528380693767751097 ) ) ;
#46350 = EDGE_LOOP ( 'NONE', ( #31555, #39756, #33921, #26620 ) ) ;
#46351 = DIRECTION ( 'NONE',  ( 0.000000000000000000, 0.01356324068817998940, -0.9999080150203990547 ) ) ;
#46352 = CARTESIAN_POINT ( 'NONE',  ( -22.29978294495153435, -3.598607126810739132, 1.052446240539704814 ) ) ;
#46353 = CARTESIAN_POINT ( 'NONE',  ( 0.3675815128205912052, -3.951233083390393030, -11.62724744438069635 ) ) ;
#46354 = CARTESIAN_POINT ( 'NONE',  ( 1.459561108994131162, -0.6317018236577405244, -12.62847742794703443 ) ) ;
#46355 = ORIENTED_EDGE ( 'NONE', *, *, #48663, .F. ) ;
#46356 = DIRECTION ( 'NONE',  ( -0.000000000000000000, -1.000000000000000000, -0.000000000000000000 ) ) ;
#46357 = CARTESIAN_POINT ( 'NONE',  ( 5.268658153349320195, -26.03085267760928545, 15.19911252589913886 ) ) ;
#46358 = CARTESIAN_POINT ( 'NONE',  ( 37.00000000000000711, 3.916263239775349625, -11.07407352312214144 ) ) ;
#46360 = ORIENTED_EDGE ( 'NONE', *, *, #11135, .F. ) ;
#46359 = CARTESIAN_POINT ( 'NONE',  ( 35.00000000000000000, 10.25474254703961918, 6.584150480049438592 ) ) ;
#46361 = CARTESIAN_POINT ( 'NONE',  ( 2.241536586108913820, -2.605228657247397717, 7.176205604390200499 ) ) ;
#46362 = VERTEX_POINT ( 'NONE', #63691 ) ;
#46363 = CARTESIAN_POINT ( 'NONE',  ( 2.034671305879988790, 5.218565780488984451, 10.44529075078584590 ) ) ;
#46364 = VERTEX_POINT ( 'NONE', #13178 ) ;
#46365 = ORIENTED_EDGE ( 'NONE', *, *, #54796, .T. ) ;
#46366 = CARTESIAN_POINT ( 'NONE',  ( 35.00000000000000000, -8.029056188533749250, -8.573591947375291511 ) ) ;
#46367 = CARTESIAN_POINT ( 'NONE',  ( 3.643024398545848808, -28.29981509102552550, 13.54931501599828358 ) ) ;
#46368 = CARTESIAN_POINT ( 'NONE',  ( 2.242819959140645469, -7.634209046698942736, -0.1024002568250162587 ) ) ;
#46369 = EDGE_CURVE ( 'NONE', #52982, #52767, #7138, .T. ) ;
#46370 = ORIENTED_EDGE ( 'NONE', *, *, #55751, .F. ) ;
#46371 = DIRECTION ( 'NONE',  ( 1.000000000000000000, 0.000000000000000000, 0.000000000000000000 ) ) ;
#46372 = AXIS2_PLACEMENT_3D ( 'NONE', #3180, #27773, #28757 ) ;
#46373 = CARTESIAN_POINT ( 'NONE',  ( 0.5572780756280651948, -2.443667122521392177, 12.09922454589786156 ) ) ;
#46374 = ORIENTED_EDGE ( 'NONE', *, *, #10647, .F. ) ;
#46375 = ORIENTED_EDGE ( 'NONE', *, *, #13754, .T. ) ;
#46376 = CARTESIAN_POINT ( 'NONE',  ( 0.2956976708475452797, 12.02996380804954057, 2.344604179391455823 ) ) ;
#46377 = VERTEX_POINT ( 'NONE', #58407 ) ;
#46378 = ORIENTED_EDGE ( 'NONE', *, *, #63655, .F. ) ;
#46379 = DIRECTION ( 'NONE',  ( 0.000000000000000000, -0.01356324068817998940, 0.9999080150203990547 ) ) ;
#46380 = DIRECTION ( 'NONE',  ( 1.000000000000000000, 0.000000000000000000, -0.000000000000000000 ) ) ;
#46381 = DIRECTION ( 'NONE',  ( 1.000000000000000000, 0.000000000000000000, 0.000000000000000000 ) ) ;
#46382 = CARTESIAN_POINT ( 'NONE',  ( 2.305787727787084407, -1.164987321564681100, -7.566723232958083578 ) ) ;
#46383 = CARTESIAN_POINT ( 'NONE',  ( 35.00000000000000000, 7.717887834988244045, -8.854740511458876639 ) ) ;
#46384 = CARTESIAN_POINT ( 'NONE',  ( -36.00000000000000711, 11.32068061209295529, 5.865551165831118574 ) ) ;
#46385 = B_SPLINE_CURVE_WITH_KNOTS ( 'NONE', 3,
 ( #42469, #58130, #37169, #2625, #32824, #52806, #2276 ),
 .UNSPECIFIED., .F., .F.,
 ( 4, 3, 4 ),
 ( 4.352182061961988653E-15, 0.002398160485435415698, 0.005002426799387886536 ),
 .UNSPECIFIED. ) ;
#46386 = EDGE_CURVE ( 'NONE', #36091, #31267, #17835, .T. ) ;
#46387 = FACE_OUTER_BOUND ( 'NONE', #62460, .T. ) ;
#46388 = EDGE_CURVE ( 'NONE', #20539, #54418, #40073, .T. ) ;
#46389 = ORIENTED_EDGE ( 'NONE', *, *, #51478, .F. ) ;
#46390 = EDGE_CURVE ( 'NONE', #36996, #20105, #19868, .T. ) ;
#46391 = CYLINDRICAL_SURFACE ( 'NONE', #59360, 6.936499999999988120 ) ;
#46392 = CARTESIAN_POINT ( 'NONE',  ( 4.897912363208013709, -9.936743041242092289, 6.735674725481181291 ) ) ;
#46393 = DIRECTION ( 'NONE',  ( -1.000000000000000000, -0.000000000000000000, 0.000000000000000000 ) ) ;
#46394 = EDGE_CURVE ( 'NONE', #11939, #54645, #30935, .T. ) ;
#46395 = CARTESIAN_POINT ( 'NONE',  ( 24.07798446190206221, 1.048718167601086826, -13.46309495289836100 ) ) ;
#46396 = EDGE_CURVE ( 'NONE', #61330, #65638, #29489, .T. ) ;
#46397 = CARTESIAN_POINT ( 'NONE',  ( 3.925267077142222671, 5.821403683822743425, -10.49580640056087155 ) ) ;
#46398 = CARTESIAN_POINT ( 'NONE',  ( 9.743605816575051648, 1.293910771361904910, -11.93188251073744865 ) ) ;
#46399 = ORIENTED_EDGE ( 'NONE', *, *, #11770, .T. ) ;
#46400 = CYLINDRICAL_SURFACE ( 'NONE', #17623, 12.75000000000000178 ) ;
#46401 = DIRECTION ( 'NONE',  ( 0.000000000000000000, 0.3554799084908900619, 0.9346839223284567622 ) ) ;
#46402 = LINE ( 'NONE', #65672, #13154 ) ;
#46403 = AXIS2_PLACEMENT_3D ( 'NONE', #16998, #6718, #47597 ) ;
#46404 = B_SPLINE_CURVE_WITH_KNOTS ( 'NONE', 3,
 ( #41360, #9796, #61646, #40372, #65330, #5834, #60676, #15110, #50050, #50394, #61322, #15757, #41038, #60338, #14764, #162 ),
 .UNSPECIFIED., .F., .F.,
 ( 4, 3, 3, 3, 3, 4 ),
 ( 4.336808689942017255E-19, 0.0002176109881720239428, 0.0004352086762394593656, 0.0006528017811446864237, 0.0007615147961451704337, 0.0009453342004946751554 ),
 .UNSPECIFIED. ) ;
#46405 = EDGE_CURVE ( 'NONE', #42318, #17913, #45718, .T. ) ;
#46406 = CARTESIAN_POINT ( 'NONE',  ( -25.25756445130008387, 9.783230075093738876, 6.955975781903453559 ) ) ;
#46407 = FACE_OUTER_BOUND ( 'NONE', #35568, .T. ) ;
#46408 =( BOUNDED_CURVE ( )  B_SPLINE_CURVE ( 3, ( #14021, #28665, #63913, #23702 ),
 .UNSPECIFIED., .F., .F. ) 
 B_SPLINE_CURVE_WITH_KNOTS ( ( 4, 4 ),
 ( 4.526278477422524205, 4.545842283345725932 ),
 .UNSPECIFIED. ) 
 CURVE ( )  GEOMETRIC_REPRESENTATION_ITEM ( )  RATIONAL_B_SPLINE_CURVE ( ( 1.000000000000000000, 0.9999681050458084641, 0.9999681050458084641, 1.000000000000000000 ) ) 
 REPRESENTATION_ITEM ( '' )  );
#46409 = ORIENTED_EDGE ( 'NONE', *, *, #44011, .F. ) ;
#46410 = CARTESIAN_POINT ( 'NONE',  ( 2.241509619876138171, 7.634391113243451876, 0.03828218718772713469 ) ) ;
#46411 = DIRECTION ( 'NONE',  ( -0.000000000000000000, -1.000000000000000000, -0.000000000000000000 ) ) ;
#46413 = EDGE_CURVE ( 'NONE', #57223, #61765, #5074, .T. ) ;
#46412 = CARTESIAN_POINT ( 'NONE',  ( 8.309432179406254448, -32.38110954670829500, -12.75850010368669629 ) ) ;
#46414 = ORIENTED_EDGE ( 'NONE', *, *, #14830, .F. ) ;
#46415 = CARTESIAN_POINT ( 'NONE',  ( -9.351388602708162523, -12.99278190472486827, -3.665735721005250358 ) ) ;
#46416 = CARTESIAN_POINT ( 'NONE',  ( 5.516018279890452902, 0.003580555109620875767, -0.005752102158674359499 ) ) ;
#46417 = DIRECTION ( 'NONE',  ( 0.000000000000000000, 0.01356324068817998940, -0.9999080150203990547 ) ) ;
#46419 = VERTEX_POINT ( 'NONE', #45386 ) ;
#46418 = FACE_OUTER_BOUND ( 'NONE', #47194, .T. ) ;
#46420 = CARTESIAN_POINT ( 'NONE',  ( 35.00000000000000000, 4.705694406421931860E-17, -3.469127814946512892E-15 ) ) ;
#46421 = CARTESIAN_POINT ( 'NONE',  ( -27.35552965826137140, -3.094132632038958608, -0.2619431035392160156 ) ) ;
#46422 = ORIENTED_EDGE ( 'NONE', *, *, #20872, .T. ) ;
#46423 = CARTESIAN_POINT ( 'NONE',  ( -35.04709527796842394, -0.001003525937983557048, 0.01232256164995608472 ) ) ;
#46424 = DIRECTION ( 'NONE',  ( 1.000000000000000000, 0.000000000000000000, 0.000000000000000000 ) ) ;
#46425 = CARTESIAN_POINT ( 'NONE',  ( 35.00000000000000000, 9.677500615117898164, -6.657191900728355094 ) ) ;
#46426 = CARTESIAN_POINT ( 'NONE',  ( -35.00000000000000000, -12.14284015767849390, -1.030638227056693834 ) ) ;
#46427 = CARTESIAN_POINT ( 'NONE',  ( 0.2706063244538050583, -11.44820198696412739, -4.353289770698342664 ) ) ;
#46428 = CARTESIAN_POINT ( 'NONE',  ( 2.241528039335008327, 2.625917297988483945, -7.168649579907096836 ) ) ;
#46430 = ORIENTED_EDGE ( 'NONE', *, *, #5525, .F. ) ;
#46429 = CARTESIAN_POINT ( 'NONE',  ( 0.7400311444011723472, 0.3548322008127070548, 12.39937114182724542 ) ) ;
#46431 = ORIENTED_EDGE ( 'NONE', *, *, #46090, .T. ) ;
#46432 = CARTESIAN_POINT ( 'NONE',  ( 2.298277635560276089, -5.044791616846968196, 5.755367168477987683 ) ) ;
#46433 = ORIENTED_EDGE ( 'NONE', *, *, #64611, .T. ) ;
#46434 = CARTESIAN_POINT ( 'NONE',  ( 37.00000000000000711, 3.645068577060024850, -11.16627499335656815 ) ) ;
#46435 = CARTESIAN_POINT ( 'NONE',  ( 2.941278708680199916, -4.788765081995656203, 3.842273877444545960 ) ) ;
#46436 = EDGE_CURVE ( 'NONE', #32874, #10092, #35831, .T. ) ;
#46437 = DIRECTION ( 'NONE',  ( 0.000000000000000000, 0.4198891015602657650, -0.9075754196709565624 ) ) ;
#46438 = ORIENTED_EDGE ( 'NONE', *, *, #34931, .F. ) ;
#46439 = CARTESIAN_POINT ( 'NONE',  ( 3.152665057734040488, 0.000000000000000000, 0.000000000000000000 ) ) ;
#46440 = DIRECTION ( 'NONE',  ( 0.000000000000000000, -0.01356324068817991828, 0.9999080150203990547 ) ) ;
#46441 = FACE_BOUND ( 'NONE', #3269, .T. ) ;
#46442 = ORIENTED_EDGE ( 'NONE', *, *, #46604, .F. ) ;
#46443 = ORIENTED_EDGE ( 'NONE', *, *, #44915, .T. ) ;
#46444 = CARTESIAN_POINT ( 'NONE',  ( 3.291290029914074378, 8.250315036047103590, 25.00000000000000000 ) ) ;
#46445 = ADVANCED_FACE ( 'NONE', ( #179 ), #9468, .T. ) ;
#46446 = ORIENTED_EDGE ( 'NONE', *, *, #29158, .F. ) ;
#46447 = CARTESIAN_POINT ( 'NONE',  ( 0.2638984909335720941, 2.322601104020666885, 12.02508546958697266 ) ) ;
#46448 = CARTESIAN_POINT ( 'NONE',  ( -27.08850691366480135, 0.5697889027535644191, -2.232573186527720743 ) ) ;
#46449 = CARTESIAN_POINT ( 'NONE',  ( -35.00000000000000000, 11.91791701451266405, 2.544412758415886877 ) ) ;
#46450 = CYLINDRICAL_SURFACE ( 'NONE', #31588, 12.74999999999999822 ) ;
#46451 = FACE_OUTER_BOUND ( 'NONE', #13318, .T. ) ;
#46452 = CARTESIAN_POINT ( 'NONE',  ( 2.770579946183334474, -7.739026583264747572, 1.056759439485547514 ) ) ;
#46453 = EDGE_CURVE ( 'NONE', #40758, #53254, #1886, .T. ) ;
#46454 = VECTOR ( 'NONE', #57007, 1000.000000000000000 ) ;
#46455 = LINE ( 'NONE', #6564, #64146 ) ;
#46456 = EDGE_LOOP ( 'NONE', ( #33025, #20611, #52026, #40610 ) ) ;
#46457 = CARTESIAN_POINT ( 'NONE',  ( 1.194176325881340706, 12.54527478469375623, -0.5141316333311681808 ) ) ;
#46458 = CARTESIAN_POINT ( 'NONE',  ( 2.373367633546871858, 3.994744114396181267, -6.557448619657597177 ) ) ;
#46459 = ADVANCED_FACE ( 'NONE', ( #5510 ), #38446, .F. ) ;
#46460 = FACE_OUTER_BOUND ( 'NONE', #13506, .T. ) ;
#46461 = DIRECTION ( 'NONE',  ( 1.000000000000000000, 0.000000000000000000, 0.000000000000000000 ) ) ;
#46462 = DIRECTION ( 'NONE',  ( 0.000000000000000000, -0.01356324068817998940, 0.9999080150203990547 ) ) ;
#46463 = DIRECTION ( 'NONE',  ( -1.000000000000000000, 0.000000000000000000, 0.000000000000000000 ) ) ;
#46464 = DIRECTION ( 'NONE',  ( 0.000000000000000000, 0.000000000000000000, 1.000000000000000000 ) ) ;
#46465 = ORIENTED_EDGE ( 'NONE', *, *, #23340, .F. ) ;
#46466 = B_SPLINE_CURVE_WITH_KNOTS ( 'NONE', 3,
 ( #57365, #30757, #51419, #41071, #61350, #26773, #47071, #11789, #6498, #1183, #46089, #1529, #26126, #10481, #1839, #10818 ),
 .UNSPECIFIED., .F., .F.,
 ( 4, 3, 3, 3, 3, 4 ),
 ( 3.697854792267728832E-15, 0.0002126834539179605613, 0.0004253519300366067832, 0.0006380165497223873328, 0.0007442707582427906046, 0.0009453531351420190083 ),
 .UNSPECIFIED. ) ;
#46467 = ORIENTED_EDGE ( 'NONE', *, *, #23504, .T. ) ;
#46468 = DIRECTION ( 'NONE',  ( 0.000000000000000000, -0.01356324068817998940, 0.9999080150203990547 ) ) ;
#46469 = ORIENTED_EDGE ( 'NONE', *, *, #9217, .T. ) ;
#46470 = CARTESIAN_POINT ( 'NONE',  ( 37.00000000000000711, 4.705694406421931860E-17, -3.469127814946512892E-15 ) ) ;
#46471 = ADVANCED_FACE ( 'NONE', ( #51715 ), #41372, .T. ) ;
#46472 = LINE ( 'NONE', #51805, #11226 ) ;
#46473 = CARTESIAN_POINT ( 'NONE',  ( 2.241352910868910531, 5.901537464758519036, -4.843133558968066410 ) ) ;
#46474 = CARTESIAN_POINT ( 'NONE',  ( 5.536195898058073439, 0.005266167600748165173, -0.006672323185952934443 ) ) ;
#46475 = EDGE_CURVE ( 'NONE', #23572, #62927, #47555, .T. ) ;
#46476 = EDGE_LOOP ( 'NONE', ( #47609, #7994, #31158, #9973, #62149, #33830 ) ) ;
#46477 = DIRECTION ( 'NONE',  ( 0.000000000000000000, 0.9868265225415265851, -0.1617819965527618475 ) ) ;
#46478 = CARTESIAN_POINT ( 'NONE',  ( 1.000000000000000888, -0.8935325819928070512, -7.446583077151393226 ) ) ;
#46479 = B_SPLINE_CURVE_WITH_KNOTS ( 'NONE', 3,
 ( #41335, #51995, #46349, #790, #27048, #57307 ),
 .UNSPECIFIED., .F., .F.,
 ( 4, 2, 4 ),
 ( 0.0001654224980408343251, 0.0006219428995476489370, 0.001078463301054463468 ),
 .UNSPECIFIED. ) ;
#46480 = CARTESIAN_POINT ( 'NONE',  ( 1.109979610370654290, -12.41172293674659421, 1.701361252868953455 ) ) ;
#46481 = CARTESIAN_POINT ( 'NONE',  ( 1.719304012341582588, 7.017415949614099979, -10.62216384465570762 ) ) ;
#46482 = EDGE_CURVE ( 'NONE', #34740, #51848, #36403, .T. ) ;
#46483 = AXIS2_PLACEMENT_3D ( 'NONE', #36205, #5997, #62153 ) ;
#46484 = EDGE_CURVE ( 'NONE', #19993, #59672, #18883, .T. ) ;
#46485 = CARTESIAN_POINT ( 'NONE',  ( 0.3278977287071215274, 6.347150352417455288, -10.49733767381175653 ) ) ;
#46486 = LINE ( 'NONE', #15876, #45701 ) ;
#46487 = VECTOR ( 'NONE', #27475, 1000.000000000000000 ) ;
#46488 = ORIENTED_EDGE ( 'NONE', *, *, #36342, .T. ) ;
#46490 = EDGE_CURVE ( 'NONE', #9134, #48396, #56029, .T. ) ;
#46489 = DIRECTION ( 'NONE',  ( 0.000000000000000000, -0.01356324068817998940, 0.9999080150203990547 ) ) ;
#46491 = ORIENTED_EDGE ( 'NONE', *, *, #20555, .T. ) ;
#46492 = CARTESIAN_POINT ( 'NONE',  ( 35.00000000000000000, -12.05416472667166516, -1.791059740004382617 ) ) ;
#46493 = DIRECTION ( 'NONE',  ( -1.000000000000000000, 0.000000000000000000, 0.000000000000000000 ) ) ;
#46494 = B_SPLINE_CURVE_WITH_KNOTS ( 'NONE', 3,
 ( #24361, #20361, #9077, #35645, #19057, #40641, #4092 ),
 .UNSPECIFIED., .F., .F.,
 ( 4, 3, 4 ),
 ( 0.000000000000000000, 0.001700533616330624290, 0.005002426799371293906 ),
 .UNSPECIFIED. ) ;
#46495 = AXIS2_PLACEMENT_3D ( 'NONE', #37375, #56350, #41714 ) ;
#46496 = CARTESIAN_POINT ( 'NONE',  ( -35.04683013664716640, 0.01075274318001804771, 0.006090538653935762686 ) ) ;
#46497 = CARTESIAN_POINT ( 'NONE',  ( 0.3218525148189880225, -11.60666749448226120, 3.964374483810605643 ) ) ;
#46498 = ORIENTED_EDGE ( 'NONE', *, *, #57607, .T. ) ;
#46499 = ORIENTED_EDGE ( 'NONE', *, *, #61348, .T. ) ;
#46500 = CARTESIAN_POINT ( 'NONE',  ( 5.516018279890452902, 0.006286471671802441874, 0.002527316374434314221 ) ) ;
#46501 = ORIENTED_EDGE ( 'NONE', *, *, #6592, .F. ) ;
#46502 = DIRECTION ( 'NONE',  ( 0.000000000000000000, 0.3807014730195220631, -0.9246979985058721985 ) ) ;
#46503 = CARTESIAN_POINT ( 'NONE',  ( -22.31328051695926007, 2.608921479762127849, -2.748895659348120635 ) ) ;
#46504 = DIRECTION ( 'NONE',  ( 1.000000000000000000, 0.000000000000000000, -0.000000000000000000 ) ) ;
#46505 = DIRECTION ( 'NONE',  ( -0.9606638835031803270, 0.1984016392583671240, -0.1943236796486234874 ) ) ;
#46506 = CARTESIAN_POINT ( 'NONE',  ( 0.3675815128205894289, -7.689697408877210094, -9.574637318042043432 ) ) ;
#46507 = CARTESIAN_POINT ( 'NONE',  ( 10.75853767213705225, 7.830989516993144051, -9.092612561015865680 ) ) ;
#46508 = CARTESIAN_POINT ( 'NONE',  ( -11.40165637463000081, -7.157122913318663571, 9.642566250083232759 ) ) ;
#46509 = ORIENTED_EDGE ( 'NONE', *, *, #8169, .T. ) ;
#46510 = CARTESIAN_POINT ( 'NONE',  ( 37.00000000000000711, 4.705694406421931860E-17, -3.469127814946512892E-15 ) ) ;
#46511 = EDGE_LOOP ( 'NONE', ( #44526, #34542, #50099, #45644 ) ) ;
#46512 = CARTESIAN_POINT ( 'NONE',  ( 0.000000000000000000, 1.145812388885126820, 6.715725538143592743 ) ) ;
#46513 = CARTESIAN_POINT ( 'NONE',  ( -27.05874794189610455, 1.734723475976807094E-15, -8.673617379884035472E-15 ) ) ;
#46514 = EDGE_CURVE ( 'NONE', #48534, #54954, #829, .T. ) ;
#46515 = ORIENTED_EDGE ( 'NONE', *, *, #48874, .F. ) ;
#46516 = CARTESIAN_POINT ( 'NONE',  ( 41.00000000000000000, -25.34319448863032065, -3.012683490291701016 ) ) ;
#46517 = CARTESIAN_POINT ( 'NONE',  ( -17.05023968204110574, -34.50000000000000000, 4.356789313881320957 ) ) ;
#46518 = ORIENTED_EDGE ( 'NONE', *, *, #22801, .T. ) ;
#46519 = CYLINDRICAL_SURFACE ( 'NONE', #29080, 5.000000000000000888 ) ;
#46520 = CARTESIAN_POINT ( 'NONE',  ( -12.11665614333000462, -29.85821820039411278, -8.776459307919635577 ) ) ;
#46521 = FACE_OUTER_BOUND ( 'NONE', #17244, .T. ) ;
#46522 = VERTEX_POINT ( 'NONE', #11143 ) ;
#46523 = ORIENTED_EDGE ( 'NONE', *, *, #29208, .F. ) ;
#46524 = DIRECTION ( 'NONE',  ( -1.000000000000000000, 0.000000000000000000, 0.000000000000000000 ) ) ;
#46525 = ORIENTED_EDGE ( 'NONE', *, *, #14446, .T. ) ;
#46526 = CYLINDRICAL_SURFACE ( 'NONE', #53942, 5.000000000000000888 ) ;
#46527 = ORIENTED_EDGE ( 'NONE', *, *, #65726, .T. ) ;
#46528 = EDGE_CURVE ( 'NONE', #3374, #62061, #52867, .T. ) ;
#46529 = EDGE_LOOP ( 'NONE', ( #64420, #27044 ) ) ;
#46530 = ORIENTED_EDGE ( 'NONE', *, *, #39954, .T. ) ;
#46531 = DIRECTION ( 'NONE',  ( -1.000000000000000000, 0.000000000000000000, 0.000000000000000000 ) ) ;
#46533 = AXIS2_PLACEMENT_3D ( 'NONE', #6966, #36885, #27236 ) ;
#46532 = CARTESIAN_POINT ( 'NONE',  ( 0.5572780756278360448, 11.49107179558535385, 4.507550621618145570 ) ) ;
#46534 = CARTESIAN_POINT ( 'NONE',  ( 0.2655924914740778742, -4.147079829127330974, 11.52280271232869424 ) ) ;
#46535 = DIRECTION ( 'NONE',  ( -1.000000000000000000, -0.000000000000000000, -0.000000000000000000 ) ) ;
#46536 = CARTESIAN_POINT ( 'NONE',  ( -35.00000000000000000, -10.43555801961479190, 5.391785509270926369 ) ) ;
#46537 = ORIENTED_EDGE ( 'NONE', *, *, #45335, .F. ) ;
#46538 = CARTESIAN_POINT ( 'NONE',  ( -37.00000000000000711, -12.74613886779085270, 0.3137578094508789439 ) ) ;
#46539 = CIRCLE ( 'NONE', #7274, 12.18650000000000055 ) ;
#46540 = VERTEX_POINT ( 'NONE', #52031 ) ;
#46541 = CARTESIAN_POINT ( 'NONE',  ( 4.308196110052892319E-12, -30.53649492335491189, 15.30974548841782656 ) ) ;
#46542 = CARTESIAN_POINT ( 'NONE',  ( -27.09833916700227263, 0.6583442518269375654, 2.238843247505173828 ) ) ;
#46543 = VECTOR ( 'NONE', #21433, 1000.000000000000114 ) ;
#46544 = DIRECTION ( 'NONE',  ( 0.000000000000000000, 0.000000000000000000, -1.000000000000000000 ) ) ;
#46545 = ADVANCED_FACE ( 'NONE', ( #26422 ), #31721, .T. ) ;
#46546 = B_SPLINE_CURVE_WITH_KNOTS ( 'NONE', 3,
 ( #51162, #5617, #46173, #51503, #26207, #6912, #62742, #2913, #63717, #52787, #18197, #38467, #58108, #8213, #11880, #52477 ),
 .UNSPECIFIED., .F., .F.,
 ( 4, 3, 3, 3, 3, 4 ),
 ( 2.559284012420599289E-15, 0.0002126834539179633531, 0.0004253519300366116079, 0.0006380165497223953559, 0.0007442707582428000372, 0.0009453531351419522215 ),
 .UNSPECIFIED. ) ;
#46547 = CARTESIAN_POINT ( 'NONE',  ( 0.2648978790185593790, -2.256510822326224464, 12.03635331166811540 ) ) ;
#46548 = DIRECTION ( 'NONE',  ( 0.000000000000000000, 0.01356324068818000328, -0.9999080150203990547 ) ) ;
#46549 = DIRECTION ( 'NONE',  ( 0.000000000000000000, 0.000000000000000000, 1.000000000000000000 ) ) ;
#46550 = CIRCLE ( 'NONE', #2999, 5.000000000000000000 ) ;
#46551 = EDGE_CURVE ( 'NONE', #11376, #37516, #32652, .T. ) ;
#46552 = ORIENTED_EDGE ( 'NONE', *, *, #11490, .F. ) ;
#46553 = CARTESIAN_POINT ( 'NONE',  ( -35.00000000000000000, -4.725891942574680371, -10.75351884295732496 ) ) ;
#46554 = ORIENTED_EDGE ( 'NONE', *, *, #52857, .T. ) ;
#46555 = CARTESIAN_POINT ( 'NONE',  ( 5.516018279890452902, -0.004180585980735018921, -0.005331956019561697423 ) ) ;
#46556 = CARTESIAN_POINT ( 'NONE',  ( 13.26780778037858433, -27.53645921949369679, -12.33502842928022325 ) ) ;
#46557 = DIRECTION ( 'NONE',  ( -0.2475719085175098477, 0.000000000000000000, -0.9688695217174486674 ) ) ;
#46558 = DIRECTION ( 'NONE',  ( -1.000000000000000000, 0.000000000000000000, 0.000000000000000000 ) ) ;
#46559 = CARTESIAN_POINT ( 'NONE',  ( 2.241537034860906275, 7.517665055736011404, 1.330359961362312493 ) ) ;
#46560 = VERTEX_POINT ( 'NONE', #21443 ) ;
#46561 = DIRECTION ( 'NONE',  ( 0.000000000000000000, -0.5767582926625031137, -0.8169148498130233138 ) ) ;
#46562 = CARTESIAN_POINT ( 'NONE',  ( -37.00000000000000711, 4.041347439435861943, 11.02904044024210428 ) ) ;
#46563 = CARTESIAN_POINT ( 'NONE',  ( -37.00000000000000711, 11.74614673114903951, 0.01609748574465447862 ) ) ;
#46564 = CARTESIAN_POINT ( 'NONE',  ( 21.94480751494469573, -13.23013732071854065, -2.711352612237130977 ) ) ;
#46565 = ADVANCED_FACE ( 'NONE', ( #62629 ), #52371, .T. ) ;
#46566 = CIRCLE ( 'NONE', #48707, 12.18650000000000233 ) ;
#46567 = ADVANCED_FACE ( 'NONE', ( #26755 ), #52692, .T. ) ;
#46568 = CARTESIAN_POINT ( 'NONE',  ( 0.9232058338315048962, -10.98407661738932894, 5.905985151448110315 ) ) ;
#46569 = VECTOR ( 'NONE', #3720, 1000.000000000000114 ) ;
#46571 = EDGE_CURVE ( 'NONE', #56112, #3010, #1508, .T. ) ;
#46570 = CARTESIAN_POINT ( 'NONE',  ( 5.536195898058073439, -0.008496323383586251374, -0.0002547682446687694544 ) ) ;
#46572 = LINE ( 'NONE', #12962, #56448 ) ;
#46573 = CARTESIAN_POINT ( 'NONE',  ( -27.08423923533013422, 1.832018136655364282, -1.376387618994801887 ) ) ;
#46574 = CARTESIAN_POINT ( 'NONE',  ( 35.00000000000000000, 2.346765782874432382, -11.95840593935202278 ) ) ;
#46575 = AXIS2_PLACEMENT_3D ( 'NONE', #38780, #63057, #59078 ) ;
#46576 = EDGE_CURVE ( 'NONE', #13308, #46362, #43300, .T. ) ;
#46577 = ORIENTED_EDGE ( 'NONE', *, *, #57768, .F. ) ;
#46578 = AXIS2_PLACEMENT_3D ( 'NONE', #32325, #47967, #48626 ) ;
#46579 = EDGE_LOOP ( 'NONE', ( #56012, #12060, #7220, #50244 ) ) ;
#46580 = CARTESIAN_POINT ( 'NONE',  ( 2.969415267404832193, -6.619534278261622440, 4.269695207293495720 ) ) ;
#46581 = CARTESIAN_POINT ( 'NONE',  ( 47.77118093457289660, -0.4451837999798747281, 7.743266003128067787 ) ) ;
#46582 = LINE ( 'NONE', #9684, #19423 ) ;
#46583 = AXIS2_PLACEMENT_3D ( 'NONE', #7351, #2051, #17351 ) ;
#46584 = CARTESIAN_POINT ( 'NONE',  ( 0.2801149460245125900, -1.933835447580712685, 12.09752788490058073 ) ) ;
#46585 = ORIENTED_EDGE ( 'NONE', *, *, #24430, .F. ) ;
#46586 = ORIENTED_EDGE ( 'NONE', *, *, #51761, .T. ) ;
#46587 = AXIS2_PLACEMENT_3D ( 'NONE', #58419, #19148, #23158 ) ;
#46588 = VERTEX_POINT ( 'NONE', #37042 ) ;
#46589 = CARTESIAN_POINT ( 'NONE',  ( 28.16540852905778181, -10.96212297253492807, 4.899974118361737574 ) ) ;
#46590 = CARTESIAN_POINT ( 'NONE',  ( 35.00000000000000000, 8.534258022646096009, -8.699265615723016154 ) ) ;
#46591 = VERTEX_POINT ( 'NONE', #11768 ) ;
#46592 = CARTESIAN_POINT ( 'NONE',  ( -37.00000000000000711, -5.428340790341781741, 10.91072401419408777 ) ) ;
#46593 = DIRECTION ( 'NONE',  ( 1.000000000000000000, 0.000000000000000000, 0.000000000000000000 ) ) ;
#46594 = EDGE_CURVE ( 'NONE', #65174, #26729, #25279, .T. ) ;
#46595 = ORIENTED_EDGE ( 'NONE', *, *, #11703, .T. ) ;
#46596 =( BOUNDED_SURFACE ( )  B_SPLINE_SURFACE ( 3, 1, ( 
 ( #58354, #41740 ),
 ( #11471, #48395 ),
 ( #31747, #12775 ),
 ( #57050, #22440 ) ),
 .UNSPECIFIED., .F., .F., .F. ) 
 B_SPLINE_SURFACE_WITH_KNOTS ( ( 4, 4 ),
 ( 2, 2 ),
 ( 0.000000000000000000, 1.000000000000000000 ),
 ( 0.000000000000000000, 1.000000000000000000 ),
 .UNSPECIFIED. ) 
 GEOMETRIC_REPRESENTATION_ITEM ( )  RATIONAL_B_SPLINE_SURFACE ( (
 ( 1.000000000000000000, 1.000000000000000000),
 ( 0.6933888150995267674, 0.9895912004443193632),
 ( 0.6933888150995267674, 0.9895912004443193632),
 ( 1.000000000000000000, 1.000000000000000000) ) ) 
 REPRESENTATION_ITEM ( '' )  SURFACE ( )  );
#46597 = CARTESIAN_POINT ( 'NONE',  ( 2.288423627607774957, 4.792733268640427369, -5.962686897379307460 ) ) ;
#46598 = CARTESIAN_POINT ( 'NONE',  ( 8.617947477505378373, -29.08580380500674778, -11.66524603227210122 ) ) ;
#46599 = DIRECTION ( 'NONE',  ( 0.000000000000000000, 0.01356324068817992175, -0.9999080150203990547 ) ) ;
#46600 = ORIENTED_EDGE ( 'NONE', *, *, #18650, .T. ) ;
#46601 = DIRECTION ( 'NONE',  ( -1.000000000000000000, 0.000000000000000000, 0.000000000000000000 ) ) ;
#46602 = ORIENTED_EDGE ( 'NONE', *, *, #14071, .F. ) ;
#46603 = CYLINDRICAL_SURFACE ( 'NONE', #11395, 4.999999999999999112 ) ;
#46604 = EDGE_CURVE ( 'NONE', #45916, #36640, #34018, .T. ) ;
#46605 = CARTESIAN_POINT ( 'NONE',  ( 9.687175622948609899, -11.98570860552670325, -0.5854820436212360146 ) ) ;
#46606 = DIRECTION ( 'NONE',  ( -1.000000000000000000, 0.000000000000000000, 0.000000000000000000 ) ) ;
#46607 = DIRECTION ( 'NONE',  ( 0.000000000000000000, 0.000000000000000000, 1.000000000000000000 ) ) ;
#46608 = DIRECTION ( 'NONE',  ( -1.000000000000000000, 0.000000000000000000, 0.000000000000000000 ) ) ;
#46610 = CARTESIAN_POINT ( 'NONE',  ( 35.00000000000000000, 4.705694406421931860E-17, -3.469127814946512892E-15 ) ) ;
#46609 = AXIS2_PLACEMENT_3D ( 'NONE', #60213, #44261, #14635 ) ;
#46611 = CARTESIAN_POINT ( 'NONE',  ( 3.152665057734040488, 0.000000000000000000, 0.000000000000000000 ) ) ;
#46612 = CARTESIAN_POINT ( 'NONE',  ( 0.9296196016852266153, 6.590257778218349571, -10.58347995892882487 ) ) ;
#46613 = CARTESIAN_POINT ( 'NONE',  ( 5.514970785353741078, -0.003262412238248737269, -0.003415090918276127412 ) ) ;
#46615 = ORIENTED_EDGE ( 'NONE', *, *, #13674, .T. ) ;
#46614 = CARTESIAN_POINT ( 'NONE',  ( 7.043522766805570434, -7.889587943819550198, 10.96282566889193966 ) ) ;
#46616 = DIRECTION ( 'NONE',  ( -1.000000000000000000, 0.000000000000000000, 0.000000000000000000 ) ) ;
#46617 = ORIENTED_EDGE ( 'NONE', *, *, #62763, .F. ) ;
#46618 = CIRCLE ( 'NONE', #28524, 6.936499999999988120 ) ;
#46619 = CYLINDRICAL_SURFACE ( 'NONE', #14714, 2.899999999999994582 ) ;
#46620 = DIRECTION ( 'NONE',  ( 0.000000000000000000, 0.000000000000000000, 1.000000000000000000 ) ) ;
#46621 = EDGE_CURVE ( 'NONE', #19062, #65236, #44324, .T. ) ;
#46622 = ADVANCED_FACE ( 'NONE', ( #59002 ), #35896, .F. ) ;
#46623 = ORIENTED_EDGE ( 'NONE', *, *, #58258, .F. ) ;
#46624 = CARTESIAN_POINT ( 'NONE',  ( 2.305787727787084407, 7.249469779319909435, 2.461236246751095536 ) ) ;
#46625 = CARTESIAN_POINT ( 'NONE',  ( 1.462291587751557653, 12.08418494300955004, -3.724645088506112423 ) ) ;
#46626 = DIRECTION ( 'NONE',  ( -1.000000000000000000, 0.000000000000000000, -0.000000000000000000 ) ) ;
#46627 = LINE ( 'NONE', #56953, #1929 ) ;
#46628 = AXIS2_PLACEMENT_3D ( 'NONE', #26105, #6812, #1818 ) ;
#46629 = ADVANCED_FACE ( 'NONE', ( #64291 ), #13735, .T. ) ;
#46630 = AXIS2_PLACEMENT_3D ( 'NONE', #1930, #22199, #37830 ) ;
#46631 = CARTESIAN_POINT ( 'NONE',  ( 0.2655924914740778187, 10.62761259256425284, -6.084990060696399361 ) ) ;
#46632 = ORIENTED_EDGE ( 'NONE', *, *, #30455, .T. ) ;
#46633 = CARTESIAN_POINT ( 'NONE',  ( 36.00000000000000711, -11.32068061209299259, -5.865551165831042191 ) ) ;
#46634 = VERTEX_POINT ( 'NONE', #54335 ) ;
#46635 = CARTESIAN_POINT ( 'NONE',  ( -22.27218376572352554, 0.9173404081777805086, -3.566922835983788787 ) ) ;
#46636 = CARTESIAN_POINT ( 'NONE',  ( -35.00000000000000000, 5.644643009979071202, 10.30098186818251982 ) ) ;
#46637 = CARTESIAN_POINT ( 'NONE',  ( 37.00000000000000711, -10.49591321039684289, -5.273331777780305707 ) ) ;
#46638 = VERTEX_POINT ( 'NONE', #58010 ) ;
#46639 = CIRCLE ( 'NONE', #56174, 5.000000000000001776 ) ;
#46640 = CARTESIAN_POINT ( 'NONE',  ( -27.09483304420744076, -1.013994808269844228, 2.090133548855273027 ) ) ;
#46641 = EDGE_CURVE ( 'NONE', #50238, #1113, #33037, .T. ) ;
#46642 = DIRECTION ( 'NONE',  ( 1.826024711554533420E-16, 0.000000000000000000, -1.000000000000000000 ) ) ;
#46643 = CARTESIAN_POINT ( 'NONE',  ( 1.948354844646952744, 0.7204626209691127325, 11.94326855455485514 ) ) ;
#46644 = LINE ( 'NONE', #57286, #44810 ) ;
#46645 = CARTESIAN_POINT ( 'NONE',  ( 0.3537226245948364434, -5.910416419900456297, -10.75912040401515313 ) ) ;
#46646 = CARTESIAN_POINT ( 'NONE',  ( 37.00000000000000711, 3.511814412392283646, 11.66953048682395355 ) ) ;
#46647 = CARTESIAN_POINT ( 'NONE',  ( 2.297017764050090616, -5.755222757172079540, 5.044319338147345455 ) ) ;
#46648 = CARTESIAN_POINT ( 'NONE',  ( -26.43258404273187523, -1.987083010659168592, 2.854888342447762906 ) ) ;
#46649 = ADVANCED_FACE ( 'NONE', ( #49023 ), #12420, .T. ) ;
#46650 = CIRCLE ( 'NONE', #53015, 12.18649999999999878 ) ;
#46651 = EDGE_LOOP ( 'NONE', ( #30225, #626, #42892, #58794 ) ) ;
#46652 = CARTESIAN_POINT ( 'NONE',  ( -16.26295706671148977, 7.784749528947430441, 11.02953652074824653 ) ) ;
#46653 = CARTESIAN_POINT ( 'NONE',  ( -35.00000000000000000, -8.954052073409537016, -9.076753354954094632 ) ) ;
#46654 = ORIENTED_EDGE ( 'NONE', *, *, #52632, .T. ) ;
#46655 = CARTESIAN_POINT ( 'NONE',  ( 1.948354844646782214, -7.125078658760747530, 9.612178954899706085 ) ) ;
#46656 = DIRECTION ( 'NONE',  ( -1.000000000000000000, 0.000000000000000000, -0.000000000000000000 ) ) ;
#46657 = CARTESIAN_POINT ( 'NONE',  ( 9.272947129449288894, 6.113238480130934960, -10.33161780435538724 ) ) ;
#46658 = VERTEX_POINT ( 'NONE', #23081 ) ;
#46659 = CARTESIAN_POINT ( 'NONE',  ( 2.247112776671470247, -6.554209700764000779, 3.918650674719086346 ) ) ;
#46660 = DIRECTION ( 'NONE',  ( 0.000000000000000000, 0.01356324068817998940, -0.9999080150203990547 ) ) ;
#46661 = ORIENTED_EDGE ( 'NONE', *, *, #821, .T. ) ;
#46662 = CARTESIAN_POINT ( 'NONE',  ( 0.3223008802179245236, -5.919638939520659449, 10.74209118105755145 ) ) ;
#46663 = VERTEX_POINT ( 'NONE', #32691 ) ;
#46664 = ORIENTED_EDGE ( 'NONE', *, *, #57349, .T. ) ;
#46665 = CYLINDRICAL_SURFACE ( 'NONE', #26313, 13.50000000000000178 ) ;
#46666 = ORIENTED_EDGE ( 'NONE', *, *, #57973, .T. ) ;
#46667 = CARTESIAN_POINT ( 'NONE',  ( -35.00000000000000000, 0.000000000000000000, 0.000000000000000000 ) ) ;
#46668 = CARTESIAN_POINT ( 'NONE',  ( -22.28694879868232448, -3.570244315741558871, 1.011812214896726791 ) ) ;
#46669 = CIRCLE ( 'NONE', #25451, 12.75000000000000178 ) ;
#46670 = DIRECTION ( 'NONE',  ( -1.000000000000000000, -0.000000000000000000, 0.000000000000000000 ) ) ;
#46671 = CARTESIAN_POINT ( 'NONE',  ( 0.4613984246114872789, -0.2828900474739520221, -12.30830943644279962 ) ) ;
#46672 = EDGE_CURVE ( 'NONE', #61242, #20003, #55036, .T. ) ;
#46673 = ORIENTED_EDGE ( 'NONE', *, *, #27161, .T. ) ;
#46674 = DIRECTION ( 'NONE',  ( 1.000000000000000000, 0.000000000000000000, 0.000000000000000000 ) ) ;
#46675 = CARTESIAN_POINT ( 'NONE',  ( 2.128776824815522772, -25.76454106360162299, 15.60647423695309222 ) ) ;
#46676 = FACE_OUTER_BOUND ( 'NONE', #6366, .T. ) ;
#46678 = ORIENTED_EDGE ( 'NONE', *, *, #32633, .F. ) ;
#46677 = DIRECTION ( 'NONE',  ( -0.000000000000000000, -0.000000000000000000, -1.000000000000000000 ) ) ;
#46679 = ADVANCED_FACE ( 'NONE', ( #3481 ), #53005, .T. ) ;
#46680 = CARTESIAN_POINT ( 'NONE',  ( 5.536195898058073439, -0.005656495196971037670, -0.006344799443924007722 ) ) ;
#46681 = ORIENTED_EDGE ( 'NONE', *, *, #50156, .T. ) ;
#46682 = DIRECTION ( 'NONE',  ( -1.000000000000000000, 0.000000000000000000, 0.000000000000000000 ) ) ;
#46683 = VECTOR ( 'NONE', #42165, 1000.000000000000000 ) ;
#46684 = ORIENTED_EDGE ( 'NONE', *, *, #25201, .T. ) ;
#46685 = CYLINDRICAL_SURFACE ( 'NONE', #54949, 4.999999999999999112 ) ;
#46686 = CARTESIAN_POINT ( 'NONE',  ( 3.152665057735335452, -7.719888720907720270, 1.848755561853250295 ) ) ;
#46687 = DIRECTION ( 'NONE',  ( 0.000000000000000000, -0.1118654143051685257, -0.9937233664769753450 ) ) ;
#46688 = ORIENTED_EDGE ( 'NONE', *, *, #13218, .F. ) ;
#46689 = EDGE_CURVE ( 'NONE', #16670, #40781, #13100, .T. ) ;
#46690 = DIRECTION ( 'NONE',  ( 1.000000000000000000, 0.000000000000000000, 0.000000000000000000 ) ) ;
#46691 = CARTESIAN_POINT ( 'NONE',  ( -20.33921151711751207, 11.75255037028624017, -2.499576093431243873 ) ) ;
#46692 = CARTESIAN_POINT ( 'NONE',  ( 0.2646305136544065406, -11.55263159009961527, 4.064188116014508800 ) ) ;
#46693 = EDGE_LOOP ( 'NONE', ( #9305, #35808, #3245, #40126 ) ) ;
#46694 = B_SPLINE_CURVE_WITH_KNOTS ( 'NONE', 3,
 ( #54263, #6489, #8705, #26767, #44577, #19341, #25, #65514, #4043, #30293 ),
 .UNSPECIFIED., .F., .F.,
 ( 4, 3, 3, 4 ),
 ( 1.563658610346375379E-18, 6.607638129004486172E-05, 9.911389841680535810E-05, 0.0001667630577588616607 ),
 .UNSPECIFIED. ) ;
#46695 = VERTEX_POINT ( 'NONE', #48372 ) ;
#46696 = CYLINDRICAL_SURFACE ( 'NONE', #12531, 10.20557198542813815 ) ;
#46697 = ORIENTED_EDGE ( 'NONE', *, *, #17039, .F. ) ;
#46698 = VERTEX_POINT ( 'NONE', #33380 ) ;
#46699 = DIRECTION ( 'NONE',  ( 0.000000000000000000, 0.000000000000000000, -1.000000000000000000 ) ) ;
#46700 = DIRECTION ( 'NONE',  ( -1.000000000000000000, 0.000000000000000000, 0.000000000000000000 ) ) ;
#46701 = CARTESIAN_POINT ( 'NONE',  ( 2.241352910868908754, -7.202080440908725123, -2.532612177304514933 ) ) ;
#46702 = FACE_OUTER_BOUND ( 'NONE', #30800, .T. ) ;
#46703 = DIRECTION ( 'NONE',  ( 0.000000000000000000, 0.000000000000000000, 1.000000000000000000 ) ) ;
#46704 = DIRECTION ( 'NONE',  ( 0.000000000000000000, 1.000000000000000000, 0.000000000000000000 ) ) ;
#46705 = CIRCLE ( 'NONE', #20125, 12.18649999999999878 ) ;
#46706 = AXIS2_PLACEMENT_3D ( 'NONE', #15213, #50490, #30820 ) ;
#46707 = DIRECTION ( 'NONE',  ( 0.000000000000000000, 0.01356324068817991481, -0.9999080150203990547 ) ) ;
#46708 = AXIS2_PLACEMENT_3D ( 'NONE', #30670, #31344, #15053 ) ;
#46709 = ORIENTED_EDGE ( 'NONE', *, *, #18619, .T. ) ;
#46710 = CARTESIAN_POINT ( 'NONE',  ( 2.941278708680199916, -5.383216837018920842, -2.952340773940166141 ) ) ;
#46711 =( NAMED_UNIT ( * ) PLANE_ANGLE_UNIT ( ) SI_UNIT ( $, .RADIAN. ) );
#46712 = B_SPLINE_CURVE_WITH_KNOTS ( 'NONE', 3,
 ( #50514, #11246, #9935, #5623, #4957, #299, #55488, #14889, #25220, #55823, #5278, #625, #25548, #15563, #15880, #45494, #35826, #41156, #40854 ),
 .UNSPECIFIED., .F., .F.,
 ( 4, 3, 3, 3, 3, 3, 4 ),
 ( 0.000000000000000000, 2.832085443685182426E-05, 4.217789847592154422E-05, 5.603488375296287891E-05, 6.989180858882558772E-05, 9.821094830335149047E-05, 0.0001178165571463608645 ),
 .UNSPECIFIED. ) ;
#46713 = AXIS2_PLACEMENT_3D ( 'NONE', #41502, #40873, #1304 ) ;
#46714 = DIRECTION ( 'NONE',  ( 1.000000000000000000, -0.000000000000000000, 0.000000000000000000 ) ) ;
#46715 = LINE ( 'NONE', #26118, #14091 ) ;
#46716 = AXIS2_PLACEMENT_3D ( 'NONE', #29551, #44860, #19275 ) ;
#46717 = CARTESIAN_POINT ( 'NONE',  ( 5.515188684475870851, 0.005339000964282161060, -0.0003622115669626908038 ) ) ;
#46718 = CARTESIAN_POINT ( 'NONE',  ( -35.00000000000000000, 12.74068829017553917, 0.4871980014161916284 ) ) ;
#46719 = DIRECTION ( 'NONE',  ( 0.000000000000000000, 0.01356324068817998940, -0.9999080150203990547 ) ) ;
#46720 = ORIENTED_EDGE ( 'NONE', *, *, #48774, .F. ) ;
#46721 = DIRECTION ( 'NONE',  ( -1.000000000000000000, 0.000000000000000000, 0.000000000000000000 ) ) ;
#46722 = ADVANCED_FACE ( 'NONE', ( #2822 ), #29536, .T. ) ;
#46723 = CARTESIAN_POINT ( 'NONE',  ( 3.152665057735194232, -3.161213418914472051, -7.281573230474045921 ) ) ;
#46724 = CARTESIAN_POINT ( 'NONE',  ( 2.000000000000001776, -3.152010634611648321, -6.039758645301327000 ) ) ;
#46725 = CYLINDRICAL_SURFACE ( 'NONE', #26967, 13.50000000000000178 ) ;
#46726 = AXIS2_PLACEMENT_3D ( 'NONE', #39563, #14928, #59866 ) ;
#46727 = EDGE_CURVE ( 'NONE', #48921, #52081, #43022, .T. ) ;
#46728 = DIRECTION ( 'NONE',  ( -1.000000000000000000, 0.000000000000000000, 0.000000000000000000 ) ) ;
#46729 = CARTESIAN_POINT ( 'NONE',  ( 2.781367136452508326, -7.232043329634210593, 2.960151187465072109 ) ) ;
#46730 = EDGE_LOOP ( 'NONE', ( #58466, #25614, #56921, #47250 ) ) ;
#46731 = DIRECTION ( 'NONE',  ( -1.000000000000000000, 0.000000000000000000, 0.000000000000000000 ) ) ;
#46732 = DIRECTION ( 'NONE',  ( 0.000000000000000000, 0.6269146997507929475, 0.7790879021242551605 ) ) ;
#46733 = CARTESIAN_POINT ( 'NONE',  ( 1.633930747252547944, -12.61425129500178421, -1.494486044209151432 ) ) ;
#46734 = EDGE_LOOP ( 'NONE', ( #10578, #50515, #31195, #28050 ) ) ;
#46735 = CARTESIAN_POINT ( 'NONE',  ( 2.844750968616099662, 6.946006365803938820, 3.626176236708051004 ) ) ;
#46736 = FACE_OUTER_BOUND ( 'NONE', #65537, .T. ) ;
#46737 = DIRECTION ( 'NONE',  ( 0.000000000000000000, -0.01356324068817991828, 0.9999080150203990547 ) ) ;
#46739 = ORIENTED_EDGE ( 'NONE', *, *, #9383, .F. ) ;
#46738 = CARTESIAN_POINT ( 'NONE',  ( -35.00000000000000000, -11.17622378668009020, 3.614449339633449387 ) ) ;
#46740 = CYLINDRICAL_SURFACE ( 'NONE', #20355, 2.899999999999994582 ) ;
#46741 = VECTOR ( 'NONE', #33884, 1000.000000000000000 ) ;
#46742 = ADVANCED_FACE ( 'NONE', ( #38022 ), #6613, .F. ) ;
#46743 = COLOUR_RGB ( '', 0.31764706, 0.68627451, 0.89019608) ;
#46744 = AXIS2_PLACEMENT_3D ( 'NONE', #40692, #45347, #55668 ) ;
#46745 = CARTESIAN_POINT ( 'NONE',  ( 0.2655924914740778742, 9.352877839710711072, -7.905499957109142883 ) ) ;
#46746 = VERTEX_POINT ( 'NONE', #23749 ) ;
#46747 = CARTESIAN_POINT ( 'NONE',  ( -35.00000000000000000, 0.000000000000000000, 0.000000000000000000 ) ) ;
#46748 = DIRECTION ( 'NONE',  ( 0.000000000000000000, -0.8696919319575238116, -0.4935949184179166949 ) ) ;
#46749 = CARTESIAN_POINT ( 'NONE',  ( 0.2653519789438758547, -7.854827495960873485, 9.395292406847904232 ) ) ;
#46750 = CARTESIAN_POINT ( 'NONE',  ( -3.986346267772003404, -10.46471259782063967, 8.566942944689746042 ) ) ;
#46751 = EDGE_CURVE ( 'NONE', #32447, #63134, #65599, .T. ) ;
#46752 = CARTESIAN_POINT ( 'NONE',  ( -8.294914047376659383, 6.473484522924868756, -10.13498875827578516 ) ) ;
#46753 = DIRECTION ( 'NONE',  ( -0.000000000000000000, -0.000000000000000000, -1.000000000000000000 ) ) ;
#46755 = ORIENTED_EDGE ( 'NONE', *, *, #27251, .F. ) ;
#46754 = CARTESIAN_POINT ( 'NONE',  ( 36.00000000000000711, -11.73555825188272905, 4.983891302653701061 ) ) ;
#46756 = EDGE_CURVE ( 'NONE', #32028, #10291, #30661, .T. ) ;
#46757 = ORIENTED_EDGE ( 'NONE', *, *, #32975, .F. ) ;
#46758 = CARTESIAN_POINT ( 'NONE',  ( -35.00000000000000000, -10.39746860227885428, -7.379373053628982326 ) ) ;
#46759 = ORIENTED_EDGE ( 'NONE', *, *, #36622, .F. ) ;
#46760 = CARTESIAN_POINT ( 'NONE',  ( -25.00000000000000355, -9.999999999999998224, 5.000000000000000888 ) ) ;
#46761 = AXIS2_PLACEMENT_3D ( 'NONE', #10590, #20902, #31223 ) ;
#46762 = CARTESIAN_POINT ( 'NONE',  ( 5.516018279890452902, -0.0009545156522407517155, -0.006707902355169297580 ) ) ;
#46763 = EDGE_CURVE ( 'NONE', #3878, #61089, #45441, .T. ) ;
#46764 = FACE_OUTER_BOUND ( 'NONE', #50071, .T. ) ;
#46766 = ORIENTED_EDGE ( 'NONE', *, *, #4285, .T. ) ;
#46765 = CIRCLE ( 'NONE', #10632, 1.500000000000000222 ) ;
#46767 = DIRECTION ( 'NONE',  ( -1.000000000000000000, 0.000000000000000000, 0.000000000000000000 ) ) ;
#46768 = CARTESIAN_POINT ( 'NONE',  ( 0.000000000000000000, 6.767909380267589370, 0.7805499053121639497 ) ) ;
#46770 = EDGE_CURVE ( 'NONE', #54645, #32746, #12668, .T. ) ;
#46769 = DIRECTION ( 'NONE',  ( 1.000000000000000000, 0.000000000000000000, 0.000000000000000000 ) ) ;
#46771 = ORIENTED_EDGE ( 'NONE', *, *, #22245, .T. ) ;
#46772 = EDGE_LOOP ( 'NONE', ( #27718, #53119 ) ) ;
#46773 = DIRECTION ( 'NONE',  ( 0.9207114435679737419, 0.000000000000000000, -0.3902440745007897949 ) ) ;
#46774 = VERTEX_POINT ( 'NONE', #25359 ) ;
#46775 = CIRCLE ( 'NONE', #18111, 7.938172270156617749 ) ;
#46776 = CARTESIAN_POINT ( 'NONE',  ( 35.00000000000000000, 4.705694406421931860E-17, -3.469127814946512892E-15 ) ) ;
#46777 = CARTESIAN_POINT ( 'NONE',  ( 0.2646305136544065406, 6.008537389229416270, 10.67138229758231738 ) ) ;
#46778 = CARTESIAN_POINT ( 'NONE',  ( 10.28770264580773741, 1.469485120472078465, 13.42064909261541317 ) ) ;
#46779 = FACE_OUTER_BOUND ( 'NONE', #60553, .T. ) ;
#46780 = CARTESIAN_POINT ( 'NONE',  ( 37.00000000000000711, -9.700295462048712736, -7.376655759824850556 ) ) ;
#46781 = DIRECTION ( 'NONE',  ( -1.000000000000000000, -0.000000000000000000, -0.000000000000000000 ) ) ;
#46782 = EDGE_CURVE ( 'NONE', #60035, #40488, #52905, .T. ) ;
#46783 = DIRECTION ( 'NONE',  ( 0.000000000000000000, -0.2006870767258747690, 0.9796553971857770993 ) ) ;
#46784 = VERTEX_POINT ( 'NONE', #34668 ) ;
#46785 = CARTESIAN_POINT ( 'NONE',  ( 0.6473888112830267216, 12.36914475328377350, -0.3298838684459264869 ) ) ;
#46786 = VERTEX_POINT ( 'NONE', #64929 ) ;
#46787 = CARTESIAN_POINT ( 'NONE',  ( 22.36482863261543486, 11.96441317219527889, -0.9234811557364158707 ) ) ;
#46788 = DIRECTION ( 'NONE',  ( 0.3939253465568944290, -0.5833358547425091523, -0.7103112711423471559 ) ) ;
#46789 = CARTESIAN_POINT ( 'NONE',  ( 0.3665391374699464300, 2.392238720110619443, -12.04754782681754932 ) ) ;
#46790 = CARTESIAN_POINT ( 'NONE',  ( 3.092491956585373014, -3.124176487319987761, -7.275786042219477778 ) ) ;
#46791 = DIRECTION ( 'NONE',  ( -1.000000000000000000, 0.000000000000000000, 0.000000000000000000 ) ) ;
#46792 = ORIENTED_EDGE ( 'NONE', *, *, #37238, .T. ) ;
#46793 = CIRCLE ( 'NONE', #38288, 17.59807621135332312 ) ;
#46794 = EDGE_LOOP ( 'NONE', ( #58241, #19365, #50345, #27460 ) ) ;
#46795 = VECTOR ( 'NONE', #63740, 1000.000000000000000 ) ;
#46796 = CARTESIAN_POINT ( 'NONE',  ( 25.00000000000000355, -9.999999999999998224, -25.00000000000000000 ) ) ;
#46797 =( BOUNDED_SURFACE ( )  B_SPLINE_SURFACE ( 3, 1, ( 
 ( #3420, #23688 ),
 ( #43960, #53284 ),
 ( #64233, #13682 ),
 ( #2768, #28017 ) ),
 .UNSPECIFIED., .F., .F., .F. ) 
 B_SPLINE_SURFACE_WITH_KNOTS ( ( 4, 4 ),
 ( 2, 2 ),
 ( 0.000000000000000000, 1.000000000000000000 ),
 ( 0.000000000000000000, 1.000000000000000000 ),
 .UNSPECIFIED. ) 
 GEOMETRIC_REPRESENTATION_ITEM ( )  RATIONAL_B_SPLINE_SURFACE ( (
 ( 1.000000000000000000, 1.000000000000000000),
 ( 0.6933888150995267674, 0.9895912004443193632),
 ( 0.6933888150995267674, 0.9895912004443193632),
 ( 1.000000000000000000, 1.000000000000000000) ) ) 
 REPRESENTATION_ITEM ( '' )  SURFACE ( )  );
#46798 = VERTEX_POINT ( 'NONE', #19409 ) ;
#46799 = CARTESIAN_POINT ( 'NONE',  ( -22.28939870658739864, -3.707376022556851503, 0.2834927284407648407 ) ) ;
#46800 = CARTESIAN_POINT ( 'NONE',  ( 2.305787727787083519, 5.756228004061526349, -5.047606869482997638 ) ) ;
#46801 = CARTESIAN_POINT ( 'NONE',  ( 2.241311220309556429, 4.835827934491015334, 5.907514893712945359 ) ) ;
#46802 = CARTESIAN_POINT ( 'NONE',  ( 0.9232058338315048962, -5.905985151448073012, -10.98407661738934848 ) ) ;
#46803 = VERTEX_POINT ( 'NONE', #24718 ) ;
#46804 = CYLINDRICAL_SURFACE ( 'NONE', #22939, 2.899999999999994582 ) ;
#46805 = DIRECTION ( 'NONE',  ( 0.000000000000000000, 0.01356324068817998940, -0.9999080150203989437 ) ) ;
#46806 = CARTESIAN_POINT ( 'NONE',  ( 0.8375941296801170388, -12.30893872205250439, 1.780036797758517864 ) ) ;
#46807 = FACE_OUTER_BOUND ( 'NONE', #63064, .T. ) ;
#46808 = AXIS2_PLACEMENT_3D ( 'NONE', #58378, #22469, #63027 ) ;
#46809 = EDGE_CURVE ( 'NONE', #25218, #47218, #6167, .T. ) ;
#46810 = CIRCLE ( 'NONE', #47909, 5.000000000000000888 ) ;
#46811 = VECTOR ( 'NONE', #3567, 1000.000000000000000 ) ;
#46812 = CARTESIAN_POINT ( 'NONE',  ( 37.00000000000000711, 12.26766708251991567, -3.473736367725300145 ) ) ;
#46813 = VECTOR ( 'NONE', #39976, 1000.000000000000114 ) ;
#46814 = CARTESIAN_POINT ( 'NONE',  ( 2.241317068080776576, 2.696905536171296358, 7.142175514530098468 ) ) ;
#46815 = ORIENTED_EDGE ( 'NONE', *, *, #36881, .T. ) ;
#46816 = FACE_OUTER_BOUND ( 'NONE', #21869, .T. ) ;
#46817 = ORIENTED_EDGE ( 'NONE', *, *, #59126, .F. ) ;
#46818 = CARTESIAN_POINT ( 'NONE',  ( -37.00000000000000711, -2.080187960898652655, 12.57916205664480636 ) ) ;
#46819 = CARTESIAN_POINT ( 'NONE',  ( -37.00000000000000711, -8.258652103341496797, 8.352657516904644197 ) ) ;
#46820 = DIRECTION ( 'NONE',  ( 1.000000000000000000, 0.000000000000000000, 0.000000000000000000 ) ) ;
#46821 = AXIS2_PLACEMENT_3D ( 'NONE', #14944, #24619, #35235 ) ;
#46822 = CARTESIAN_POINT ( 'NONE',  ( 0.2638984909335720941, -9.252728947331126719, 8.023974293733148855 ) ) ;
#46823 = DIRECTION ( 'NONE',  ( 0.000000000000000000, 0.01356324068817998940, -0.9999080150203989437 ) ) ;
#46824 = EDGE_CURVE ( 'NONE', #12277, #7851, #4446, .T. ) ;
#46825 = ORIENTED_EDGE ( 'NONE', *, *, #53688, .F. ) ;
#46826 = ORIENTED_EDGE ( 'NONE', *, *, #50266, .F. ) ;
#46827 = FACE_OUTER_BOUND ( 'NONE', #6629, .T. ) ;
#46828 = EDGE_LOOP ( 'NONE', ( #4947, #45452 ) ) ;
#46829 = CIRCLE ( 'NONE', #18174, 12.18650000000000055 ) ;
#46830 = LINE ( 'NONE', #5970, #36192 ) ;
#46831 = CARTESIAN_POINT ( 'NONE',  ( 2.305787727787083519, 3.971363876084056166, -6.545285700970486786 ) ) ;
#46832 = CARTESIAN_POINT ( 'NONE',  ( 2.000000000000001776, 1.225832621831852931, 6.827324998361547159 ) ) ;
#46833 = CARTESIAN_POINT ( 'NONE',  ( 37.00000000000000711, -12.17626345777663310, 0.4993900848168664752 ) ) ;
#46834 = CYLINDRICAL_SURFACE ( 'NONE', #10966, 12.75000000000000178 ) ;
#46835 = EDGE_CURVE ( 'NONE', #51873, #18418, #9352, .T. ) ;
#46836 = CARTESIAN_POINT ( 'NONE',  ( 0.000000000000000000, -1.225832621831797420, -6.827324998361596009 ) ) ;
#46837 = DIRECTION ( 'NONE',  ( 0.000000000000000000, 0.000000000000000000, 1.000000000000000000 ) ) ;
#46838 = ORIENTED_EDGE ( 'NONE', *, *, #36964, .T. ) ;
#46839 = AXIS2_PLACEMENT_3D ( 'NONE', #27119, #6847, #22449 ) ;
#46840 = EDGE_CURVE ( 'NONE', #55692, #48877, #50335, .T. ) ;
#46841 = CARTESIAN_POINT ( 'NONE',  ( 0.3675815128205894289, -5.910255304480521055, 10.76447900494938459 ) ) ;
#46842 = ORIENTED_EDGE ( 'NONE', *, *, #50230, .T. ) ;
#46843 = LINE ( 'NONE', #1308, #64140 ) ;
#46845 = CARTESIAN_POINT ( 'NONE',  ( 1.719304012341629884, 8.755325027796281745, -9.242227816402079910 ) ) ;
#46844 = CIRCLE ( 'NONE', #28752, 12.18650000000000055 ) ;
#46846 = VECTOR ( 'NONE', #1521, 1000.000000000000000 ) ;
#46847 = CIRCLE ( 'NONE', #13882, 4.999999999999999112 ) ;
#46848 = CYLINDRICAL_SURFACE ( 'NONE', #39395, 4.999999999999999112 ) ;
#46849 = ORIENTED_EDGE ( 'NONE', *, *, #7887, .T. ) ;
#46850 = LINE ( 'NONE', #56855, #52450 ) ;
#46851 = CARTESIAN_POINT ( 'NONE',  ( -22.65996813707686641, 2.607318832796713171, -4.069902221062751124 ) ) ;
#46852 = CIRCLE ( 'NONE', #26678, 4.999999999999999112 ) ;
#46854 = EDGE_CURVE ( 'NONE', #38347, #64141, #46550, .T. ) ;
#46853 = LINE ( 'NONE', #21594, #19105 ) ;
#46855 = ORIENTED_EDGE ( 'NONE', *, *, #6676, .T. ) ;
#46856 = ORIENTED_EDGE ( 'NONE', *, *, #30741, .F. ) ;
#46857 = CARTESIAN_POINT ( 'NONE',  ( 2.846142546918067229, 3.504604795492467062, 13.04310330258398487 ) ) ;
#46859 = ORIENTED_EDGE ( 'NONE', *, *, #8355, .T. ) ;
#46858 = ADVANCED_FACE ( 'NONE', ( #10076 ), #45640, .T. ) ;
#46860 = DIRECTION ( 'NONE',  ( 0.000000000000000000, -0.6943713148249690548, 0.7196168960969744344 ) ) ;
#46861 = ORIENTED_EDGE ( 'NONE', *, *, #46079, .T. ) ;
#46862 = EDGE_LOOP ( 'NONE', ( #3935, #45380, #24822, #12425 ) ) ;
#46864 = EDGE_CURVE ( 'NONE', #43014, #31870, #20374, .T. ) ;
#46863 = ORIENTED_EDGE ( 'NONE', *, *, #7054, .F. ) ;
#46865 = AXIS2_PLACEMENT_3D ( 'NONE', #42484, #51847, #62142 ) ;
#46866 = CARTESIAN_POINT ( 'NONE',  ( -22.27711351828769892, -2.657880562424684179, 2.547249869018247015 ) ) ;
#46867 = CARTESIAN_POINT ( 'NONE',  ( 2.268878695252937394, 5.025754889198752906, -5.759001817705959425 ) ) ;
#46868 = CIRCLE ( 'NONE', #161, 5.000000000000000000 ) ;
#46869 = CARTESIAN_POINT ( 'NONE',  ( 5.514624014163232779, 0.0005510299962881775801, -0.004104370840204391718 ) ) ;
#46870 = CARTESIAN_POINT ( 'NONE',  ( 5.536195898058073439, -0.005266167600748119203, 0.006672323185952970005 ) ) ;
#46871 = CARTESIAN_POINT ( 'NONE',  ( -35.00000000000000000, 4.545979934229578134, -11.30684963584384128 ) ) ;
#46872 = EDGE_LOOP ( 'NONE', ( #25936, #15101, #1797, #34866 ) ) ;
#46874 = ADVANCED_FACE ( 'NONE', ( #15387 ), #35658, .T. ) ;
#46873 = AXIS2_PLACEMENT_3D ( 'NONE', #25788, #32960, #22329 ) ;
#46875 = DIRECTION ( 'NONE',  ( 0.000000000000000000, 0.1081190184239352453, 0.9941379571543603744 ) ) ;
#46876 = EDGE_LOOP ( 'NONE', ( #51292, #22326, #23227, #53650 ) ) ;
#46877 = CARTESIAN_POINT ( 'NONE',  ( -10.48620311856347875, -9.720786832536937538, -9.367833439828894271 ) ) ;
#46878 = DIRECTION ( 'NONE',  ( 1.000000000000000000, 0.000000000000000000, -0.000000000000000000 ) ) ;
#46879 = VECTOR ( 'NONE', #54305, 1000.000000000000000 ) ;
#46880 = EDGE_CURVE ( 'NONE', #34055, #53931, #46627, .T. ) ;
#46881 = DIRECTION ( 'NONE',  ( 0.000000000000000000, 0.01356324068817992175, -0.9999080150203990547 ) ) ;
#46882 = CARTESIAN_POINT ( 'NONE',  ( 0.2869720083484330053, -2.332746648244278465, 12.02930764912520445 ) ) ;
#46883 = CARTESIAN_POINT ( 'NONE',  ( 1.719304012340734822, -5.690355757825686922, -11.38834240361529737 ) ) ;
#46884 = CARTESIAN_POINT ( 'NONE',  ( 1.719304012340549859, -10.62216384465898500, -7.017415949616274240 ) ) ;
#46885 = ORIENTED_EDGE ( 'NONE', *, *, #45284, .F. ) ;
#46886 = CARTESIAN_POINT ( 'NONE',  ( 0.2646305136544072623, 12.03696649559618059, -2.256625640822192747 ) ) ;
#46887 = AXIS2_PLACEMENT_3D ( 'NONE', #14939, #10612, #30898 ) ;
#46888 = VERTEX_POINT ( 'NONE', #36962 ) ;
#46889 = CARTESIAN_POINT ( 'NONE',  ( 0.000000000000000000, -6.767909380267597363, 2.119450094687866049 ) ) ;
#46890 = CARTESIAN_POINT ( 'NONE',  ( -14.88966238093840744, -27.95127710492162620, -11.23339344092910252 ) ) ;
#46891 = CARTESIAN_POINT ( 'NONE',  ( 2.507146904658098752, 6.052884339496489297, -4.796593924427919653 ) ) ;
#46892 = AXIS2_PLACEMENT_3D ( 'NONE', #13389, #54933, #29648 ) ;
#46894 = AXIS2_PLACEMENT_3D ( 'NONE', #50201, #46504, #36179 ) ;
#46893 = CARTESIAN_POINT ( 'NONE',  ( 1.948354844646345452, 7.125078658759951722, -9.612178954897759198 ) ) ;
#46895 = DIRECTION ( 'NONE',  ( -0.000000000000000000, -0.000000000000000000, -1.000000000000000000 ) ) ;
#46896 = ORIENTED_EDGE ( 'NONE', *, *, #40017, .F. ) ;
#46897 = CARTESIAN_POINT ( 'NONE',  ( 0.000000000000000000, 6.160607635185406217, 4.277489166005578269 ) ) ;
#46898 = CARTESIAN_POINT ( 'NONE',  ( 0.3002738374340817029, 2.350339881555103982, -12.03040002643109574 ) ) ;
#46899 = CARTESIAN_POINT ( 'NONE',  ( 24.17631672541061150, 8.757354005739776071, -8.209550701608334222 ) ) ;
#46900 = CARTESIAN_POINT ( 'NONE',  ( 2.507146904658097419, 3.672650549645667617, 6.793847219607461518 ) ) ;
#46901 = CIRCLE ( 'NONE', #36248, 4.999999999999999112 ) ;
#46902 = EDGE_CURVE ( 'NONE', #13538, #23831, #39082, .T. ) ;
#46903 = AXIS2_PLACEMENT_3D ( 'NONE', #62801, #42178, #52838 ) ;
#46904 = VECTOR ( 'NONE', #36512, 1000.000000000000114 ) ;
#46905 = FACE_OUTER_BOUND ( 'NONE', #53908, .T. ) ;
#46906 = CARTESIAN_POINT ( 'NONE',  ( 2.241536586108913376, 2.617055111126449063, 7.171901127201301129 ) ) ;
#46907 = CARTESIAN_POINT ( 'NONE',  ( 1.719304012340734822, -5.690355757825686922, -11.38834240361529737 ) ) ;
#46908 = CARTESIAN_POINT ( 'NONE',  ( -19.89498410467781753, -11.69391641137695181, -2.712006120889818739 ) ) ;
#46909 = CARTESIAN_POINT ( 'NONE',  ( 2.305787727787084407, -4.792270232040854339, -5.970480882365271746 ) ) ;
#46910 = ADVANCED_FACE ( 'NONE', ( #15691 ), #10865, .F. ) ;
#46911 = AXIS2_PLACEMENT_3D ( 'NONE', #47114, #32116, #52434 ) ;
#46912 = EDGE_CURVE ( 'NONE', #26984, #42603, #40117, .T. ) ;
#46913 = ORIENTED_EDGE ( 'NONE', *, *, #29698, .T. ) ;
#46914 = AXIS2_PLACEMENT_3D ( 'NONE', #35167, #39848, #5265 ) ;
#46915 = B_SPLINE_CURVE_WITH_KNOTS ( 'NONE', 3,
 ( #39339, #39679, #34020, #34359, #64292, #18759, #39015, #54672, #13737, #59976, #54338, #8773, #59643, #29059, #3812, #24065, #34987, #44326, #64597 ),
 .UNSPECIFIED., .F., .F.,
 ( 4, 3, 3, 3, 3, 3, 4 ),
 ( 7.470971189404981089E-18, 4.457896483015255922E-05, 6.639290541542495041E-05, 8.820687556479337235E-05, 0.0001100173248778935222, 0.0001545671401658117229, 0.0001830328308068584142 ),
 .UNSPECIFIED. ) ;
#46916 = ORIENTED_EDGE ( 'NONE', *, *, #51659, .T. ) ;
#46917 = CARTESIAN_POINT ( 'NONE',  ( 2.589278595513663461, -6.588350318048504128, 4.081908913132012984 ) ) ;
#46918 = CARTESIAN_POINT ( 'NONE',  ( 48.68114316863541546, -0.2655233219083136254, 3.919294168552611257 ) ) ;
#46919 = DIRECTION ( 'NONE',  ( 1.000000000000000000, -0.000000000000000000, 0.000000000000000000 ) ) ;
#46920 = CARTESIAN_POINT ( 'NONE',  ( -35.00000000000000000, 7.376655759825023750, -9.700295462048581285 ) ) ;
#46921 = ORIENTED_EDGE ( 'NONE', *, *, #52569, .T. ) ;
#46922 = EDGE_CURVE ( 'NONE', #23985, #62968, #41631, .T. ) ;
#46923 = AXIS2_PLACEMENT_3D ( 'NONE', #12421, #52374, #2137 ) ;
#46924 = ORIENTED_EDGE ( 'NONE', *, *, #59174, .F. ) ;
#46925 = ORIENTED_EDGE ( 'NONE', *, *, #27999, .F. ) ;
#46926 = CARTESIAN_POINT ( 'NONE',  ( 2.705197763288548440, 7.783989928191466845, 0.2797837188786633789 ) ) ;
#46927 = DIRECTION ( 'NONE',  ( -0.3162277663656185012, -0.1673616205762862574, -0.9338040949457712125 ) ) ;
#46928 = EDGE_LOOP ( 'NONE', ( #3135, #54311, #1966, #25014 ) ) ;
#46929 = CARTESIAN_POINT ( 'NONE',  ( 36.00000000000000711, -11.39945968423467448, 5.710938531231827042 ) ) ;
#46930 = AXIS2_PLACEMENT_3D ( 'NONE', #5682, #40909, #24717 ) ;
#46931 = CARTESIAN_POINT ( 'NONE',  ( 37.00000000000000711, 10.75351884295727345, -4.725891942574794058 ) ) ;
#46932 = ORIENTED_EDGE ( 'NONE', *, *, #54912, .F. ) ;
#46933 = DIRECTION ( 'NONE',  ( -0.000000000000000000, -0.000000000000000000, -1.000000000000000000 ) ) ;
#46934 = CARTESIAN_POINT ( 'NONE',  ( 14.48396081724352769, -30.02861890643281839, -3.972401191364113515 ) ) ;
#46935 = CARTESIAN_POINT ( 'NONE',  ( 23.19453373513495720, -4.581577854755520818, 11.09405916972947814 ) ) ;
#46936 = ORIENTED_EDGE ( 'NONE', *, *, #52715, .T. ) ;
#46937 = CARTESIAN_POINT ( 'NONE',  ( -37.00000000000000711, 9.896810808925497582, -7.110831038798171910 ) ) ;
#46938 = ORIENTED_EDGE ( 'NONE', *, *, #17641, .T. ) ;
#46939 = DIRECTION ( 'NONE',  ( 0.000000000000000000, 0.01356324068817998940, -0.9999080150203989437 ) ) ;
#46940 = B_SPLINE_CURVE_WITH_KNOTS ( 'NONE', 3,
 ( #17022, #37302, #32311, #52626, #44257, #44569, #2756 ),
 .UNSPECIFIED., .F., .F.,
 ( 4, 3, 4 ),
 ( 0.000000000000000000, 0.001700533616330547528, 0.005002426799371374570 ),
 .UNSPECIFIED. ) ;
#46941 = DIRECTION ( 'NONE',  ( 0.000000000000000000, 0.000000000000000000, 1.000000000000000000 ) ) ;
#46942 = ADVANCED_FACE ( 'NONE', ( #62243 ), #40985, .T. ) ;
#46943 = CARTESIAN_POINT ( 'NONE',  ( -11.32744364968265138, -33.39367328239647748, 11.05351320890950362 ) ) ;
#46944 = DIRECTION ( 'NONE',  ( -1.000000000000000000, -0.000000000000000000, 0.000000000000000000 ) ) ;
#46945 = AXIS2_PLACEMENT_3D ( 'NONE', #51438, #35758, #46111 ) ;
#46946 = AXIS2_PLACEMENT_3D ( 'NONE', #51472, #35136, #41117 ) ;
#46948 = CIRCLE ( 'NONE', #54359, 5.000000000000000000 ) ;
#46947 = CARTESIAN_POINT ( 'NONE',  ( 5.515188684475870851, -0.005339000964281801972, -0.0003622115669623841372 ) ) ;
#46949 = LINE ( 'NONE', #57592, #15956 ) ;
#46950 = CARTESIAN_POINT ( 'NONE',  ( -27.35552965826137140, -2.548625910254533888, -1.773915698030580357 ) ) ;
#46951 = CARTESIAN_POINT ( 'NONE',  ( 0.2653141334712546540, 4.229817350136413800, 11.49252672845885037 ) ) ;
#46952 = ORIENTED_EDGE ( 'NONE', *, *, #53392, .T. ) ;
#46953 = EDGE_CURVE ( 'NONE', #49753, #11283, #22929, .T. ) ;
#46954 = CARTESIAN_POINT ( 'NONE',  ( -7.489022030332961322, 25.00000000000000000, -10.84914964302385521 ) ) ;
#46955 = VERTEX_POINT ( 'NONE', #16380 ) ;
#46956 = DIRECTION ( 'NONE',  ( 0.000000000000000000, -0.01356324068817999114, 0.9999080150203989437 ) ) ;
#46957 = CARTESIAN_POINT ( 'NONE',  ( 2.705197763288551549, -5.783040721897899417, -5.217779042888505359 ) ) ;
#46958 = ADVANCED_FACE ( 'NONE', ( #46314 ), #31003, .T. ) ;
#46959 = VERTEX_POINT ( 'NONE', #26342 ) ;
#46960 = CARTESIAN_POINT ( 'NONE',  ( 37.00000000000000711, 7.094637218249506994, 10.59380114696461916 ) ) ;
#46961 = CARTESIAN_POINT ( 'NONE',  ( 5.530133899448235191, 0.01111090067015088091, -0.01149180883054549095 ) ) ;
#46962 = CARTESIAN_POINT ( 'NONE',  ( -35.00000000000000000, 0.000000000000000000, 0.000000000000000000 ) ) ;
#46964 = VECTOR ( 'NONE', #35646, 1000.000000000000000 ) ;
#46963 = DIRECTION ( 'NONE',  ( 1.000000000000000000, 0.000000000000000000, 0.000000000000000000 ) ) ;
#46965 = ORIENTED_EDGE ( 'NONE', *, *, #13093, .F. ) ;
#46966 = AXIS2_PLACEMENT_3D ( 'NONE', #65372, #15160, #59413 ) ;
#46967 = CARTESIAN_POINT ( 'NONE',  ( 2.781367136452345790, -4.171010984503056740, -6.608147481822085112 ) ) ;
#46968 = ORIENTED_EDGE ( 'NONE', *, *, #3804, .F. ) ;
#46969 = CARTESIAN_POINT ( 'NONE',  ( -35.00000000000000000, 0.000000000000000000, 0.000000000000000000 ) ) ;
#46970 = VERTEX_POINT ( 'NONE', #56622 ) ;
#46971 = DIRECTION ( 'NONE',  ( -1.000000000000000000, 0.000000000000000000, 0.000000000000000000 ) ) ;
#46972 = AXIS2_PLACEMENT_3D ( 'NONE', #47590, #2035, #42569 ) ;
#46973 = DIRECTION ( 'NONE',  ( 1.000000000000000000, 0.000000000000000000, 0.000000000000000000 ) ) ;
#46974 = B_SPLINE_CURVE_WITH_KNOTS ( 'NONE', 3,
 ( #61563, #22307, #21994, #56604, #61906, #21687, #41942 ),
 .UNSPECIFIED., .F., .F.,
 ( 4, 3, 4 ),
 ( 0.000000000000000000, 0.001700533616330530615, 0.005002426799371309518 ),
 .UNSPECIFIED. ) ;
#46975 = DIRECTION ( 'NONE',  ( 0.000000000000000000, -1.000000000000000000, 0.000000000000000000 ) ) ;
#46976 = ORIENTED_EDGE ( 'NONE', *, *, #41849, .T. ) ;
#46977 = B_SPLINE_CURVE_WITH_KNOTS ( 'NONE', 3,
 ( #56520, #35874, #40221, #5670, #45541, #25941, #46227, #10964, #31251, #668, #60509, #20928, #51556, #46532, #41531, #58158 ),
 .UNSPECIFIED., .F., .F.,
 ( 4, 3, 3, 3, 3, 4 ),
 ( 0.000000000000000000, 0.0002999043160757217824, 0.0005998071753050755218, 0.0008997092107374187820, 0.001204458948194616187, 0.001510329163474478670 ),
 .UNSPECIFIED. ) ;
#46978 = CARTESIAN_POINT ( 'NONE',  ( -27.09602251845158705, -1.018053071731303660, 2.092130925171132638 ) ) ;
#46979 = ADVANCED_FACE ( 'NONE', ( #26031 ), #63106, .F. ) ;
#46980 = AXIS2_PLACEMENT_3D ( 'NONE', #37208, #47536, #1982 ) ;
#46981 = EDGE_CURVE ( 'NONE', #25112, #9350, #27404, .T. ) ;
#46982 = CARTESIAN_POINT ( 'NONE',  ( -22.51237073810381162, -3.719289647955757783, 2.395115314842892751 ) ) ;
#46983 = DIRECTION ( 'NONE',  ( 1.000000000000000000, 0.000000000000000000, 0.000000000000000000 ) ) ;
#46984 = CARTESIAN_POINT ( 'NONE',  ( 0.000000000000000000, -0.2704997240204360387, -6.931223712253490987 ) ) ;
#46985 = CARTESIAN_POINT ( 'NONE',  ( 0.2648321136542687859, -5.999882851577401865, -10.67551415837656492 ) ) ;
#46986 = CARTESIAN_POINT ( 'NONE',  ( -9.351388602708162523, 25.00000000000000000, -3.665735721005252135 ) ) ;
#46987 = LINE ( 'NONE', #26696, #9908 ) ;
#46988 = EDGE_CURVE ( 'NONE', #3801, #40116, #12536, .T. ) ;
#46989 = CIRCLE ( 'NONE', #60798, 12.73084802173761787 ) ;
#46990 = AXIS2_PLACEMENT_3D ( 'NONE', #13768, #64633, #49063 ) ;
#46991 = CIRCLE ( 'NONE', #44845, 5.000000000000000888 ) ;
#46992 = B_SPLINE_CURVE_WITH_KNOTS ( 'NONE', 3,
 ( #57263, #11688, #62890, #11369, #31641, #52922, #57603, #27005, #51953, #27638, #38945, #53259, #44249, #4027, #7705, #38616, #29293, #59233, #12666, #54585, #54247, #13655, #37949, #13341 ),
 .UNSPECIFIED., .F., .F.,
 ( 4, 2, 2, 2, 2, 2, 2, 2, 2, 2, 2, 4 ),
 ( 0.003159056194143415250, 0.004024695253672650602, 0.004890334313201885087, 0.005755973372731119572, 0.006621612432260354925, 0.007054431962024973468, 0.007487251491789592879, 0.007920071021554212290, 0.008352890551318830833, 0.008785710081083440703, 0.009218529610848048839, 0.01008416867037726684 ),
 .UNSPECIFIED. ) ;
#46993 = ORIENTED_EDGE ( 'NONE', *, *, #22042, .T. ) ;
#46994 = CARTESIAN_POINT ( 'NONE',  ( -16.58214495380866893, 7.650095523388448449, 11.12376028359556557 ) ) ;
#46995 = CARTESIAN_POINT ( 'NONE',  ( -37.00000000000000711, 0.000000000000000000, 0.000000000000000000 ) ) ;
#46996 =( BOUNDED_CURVE ( )  B_SPLINE_CURVE ( 3, ( #39493, #45148, #64431, #59457 ),
 .UNSPECIFIED., .F., .F. ) 
 B_SPLINE_CURVE_WITH_KNOTS ( ( 4, 4 ),
 ( 5.598218072871999240, 5.645776840021275333 ),
 .UNSPECIFIED. ) 
 CURVE ( )  GEOMETRIC_REPRESENTATION_ITEM ( )  RATIONAL_B_SPLINE_CURVE ( ( 1.000000000000000000, 0.9998115225205463918, 0.9998115225205463918, 1.000000000000000000 ) ) 
 REPRESENTATION_ITEM ( '' )  );
#46997 = VERTEX_POINT ( 'NONE', #21702 ) ;
#46998 = CARTESIAN_POINT ( 'NONE',  ( -35.00000000000000000, 11.78745411414839594, 3.093009498343968211 ) ) ;
#46999 = CARTESIAN_POINT ( 'NONE',  ( 1.375507693220495042, -9.273955665125749093, -8.553661013313396566 ) ) ;
#47000 = B_SPLINE_CURVE_WITH_KNOTS ( 'NONE', 3,
 ( #29009, #4060, #24023, #64552, #19027, #39292, #59591, #14020, #34308, #9044, #44593, #39626, #50283, #29974, #46272, #20000 ),
 .UNSPECIFIED., .F., .F.,
 ( 4, 3, 3, 3, 3, 4 ),
 ( 8.673617379884035472E-19, 0.0002176109881720227231, 0.0004352086762394592571, 0.0006528017811446877247, 0.0007615147961451714095, 0.0009453342004946414367 ),
 .UNSPECIFIED. ) ;
#47001 = ORIENTED_EDGE ( 'NONE', *, *, #54726, .T. ) ;
#47002 = CYLINDRICAL_SURFACE ( 'NONE', #32006, 4.999999999999999112 ) ;
#47003 = ORIENTED_EDGE ( 'NONE', *, *, #55933, .F. ) ;
#47004 = EDGE_CURVE ( 'NONE', #16340, #38810, #21038, .T. ) ;
#47005 = ADVANCED_FACE ( 'NONE', ( #51315 ), #754, .T. ) ;
#47006 = CARTESIAN_POINT ( 'NONE',  ( 0.3675815128205894289, -5.910255304480521055, 10.76447900494938459 ) ) ;
#47007 = ORIENTED_EDGE ( 'NONE', *, *, #12539, .F. ) ;
#47008 = VERTEX_POINT ( 'NONE', #48527 ) ;
#47009 = EDGE_CURVE ( 'NONE', #65324, #40853, #45489, .T. ) ;
#47010 = AXIS2_PLACEMENT_3D ( 'NONE', #30542, #29554, #19613 ) ;
#47011 = CARTESIAN_POINT ( 'NONE',  ( 2.305787727787083519, -7.135468203930003028, 2.774453000917123990 ) ) ;
#47012 = VERTEX_POINT ( 'NONE', #3649 ) ;
#47013 = CARTESIAN_POINT ( 'NONE',  ( -25.11474465335534489, -9.573234766864146650, 7.237578467736122789 ) ) ;
#47014 = DIRECTION ( 'NONE',  ( 0.000000000000000000, 0.000000000000000000, 1.000000000000000000 ) ) ;
#47015 = FACE_OUTER_BOUND ( 'NONE', #8752, .T. ) ;
#47016 = DIRECTION ( 'NONE',  ( 0.000000000000000000, -0.8827602140260264463, 0.4698238015817460256 ) ) ;
#47017 = ORIENTED_EDGE ( 'NONE', *, *, #56725, .F. ) ;
#47018 = AXIS2_PLACEMENT_3D ( 'NONE', #9613, #29265, #40541 ) ;
#47019 = CYLINDRICAL_SURFACE ( 'NONE', #9837, 17.75474371510546234 ) ;
#47020 = AXIS2_PLACEMENT_3D ( 'NONE', #51466, #21514, #46773 ) ;
#47021 = CARTESIAN_POINT ( 'NONE',  ( -0.4223990570890304164, -27.81390085543024426, 12.58355210400704394 ) ) ;
#47022 = DIRECTION ( 'NONE',  ( -0.3865475372811021937, 0.1410344188397524012, -0.9114221272958256126 ) ) ;
#47024 = ORIENTED_EDGE ( 'NONE', *, *, #55196, .F. ) ;
#47023 = CARTESIAN_POINT ( 'NONE',  ( -27.19357181888462094, 10.84410562793473431, 5.138615876886901468 ) ) ;
#47025 = DIRECTION ( 'NONE',  ( -0.000000000000000000, -1.000000000000000000, -0.000000000000000000 ) ) ;
#47026 = ORIENTED_EDGE ( 'NONE', *, *, #7061, .F. ) ;
#47027 = DIRECTION ( 'NONE',  ( -1.000000000000000000, 0.000000000000000000, 0.000000000000000000 ) ) ;
#47028 = EDGE_LOOP ( 'NONE', ( #2228, #65107, #33663, #22641 ) ) ;
#47029 = CARTESIAN_POINT ( 'NONE',  ( -35.00000000000000000, 0.000000000000000000, 0.000000000000000000 ) ) ;
#47030 = CARTESIAN_POINT ( 'NONE',  ( 2.000000000000001776, 0.000000000000000000, 0.000000000000000000 ) ) ;
#47031 = EDGE_CURVE ( 'NONE', #17645, #42662, #21096, .T. ) ;
#47032 = CARTESIAN_POINT ( 'NONE',  ( 2.290907136833252089, -7.649199419879184170, -0.1622757685885879708 ) ) ;
#47033 = ORIENTED_EDGE ( 'NONE', *, *, #20214, .F. ) ;
#47034 = CARTESIAN_POINT ( 'NONE',  ( -37.00000000000000711, -6.265926637539413591, -11.10408318471066380 ) ) ;
#47035 = CARTESIAN_POINT ( 'NONE',  ( -35.00000000000000000, 5.710938531231712467, 11.39945968423473310 ) ) ;
#47036 = CARTESIAN_POINT ( 'NONE',  ( 0.2648978790185602672, -12.03635331166813494, 2.256510822326103671 ) ) ;
#47037 = VERTEX_POINT ( 'NONE', #3302 ) ;
#47038 = EDGE_CURVE ( 'NONE', #32432, #44286, #4268, .T. ) ;
#47039 = CIRCLE ( 'NONE', #1370, 12.75000000000000178 ) ;
#47040 = EDGE_LOOP ( 'NONE', ( #29329, #60841, #26222, #1378 ) ) ;
#47041 = CARTESIAN_POINT ( 'NONE',  ( 2.373367633546869637, 7.528269033630156315, 1.511052049479944648 ) ) ;
#47042 = ORIENTED_EDGE ( 'NONE', *, *, #38198, .T. ) ;
#47043 = AXIS2_PLACEMENT_3D ( 'NONE', #26883, #57816, #37511 ) ;
#47044 = ORIENTED_EDGE ( 'NONE', *, *, #54845, .F. ) ;
#47046 = AXIS2_PLACEMENT_3D ( 'NONE', #17248, #37522, #27878 ) ;
#47045 = DIRECTION ( 'NONE',  ( -1.000000000000000000, 0.000000000000000000, 0.000000000000000000 ) ) ;
#47047 = LINE ( 'NONE', #57024, #21117 ) ;
#47048 = CARTESIAN_POINT ( 'NONE',  ( 2.990245332647878840, -7.075286609974364538, -4.676740826320321176 ) ) ;
#47049 = CARTESIAN_POINT ( 'NONE',  ( 2.000000000000001776, -5.217815162096861137, 5.387430271863535403 ) ) ;
#47050 = DIRECTION ( 'NONE',  ( 0.000000000000000000, 0.01356324068817998940, -0.9999080150203990547 ) ) ;
#47051 = AXIS2_PLACEMENT_3D ( 'NONE', #31741, #32071, #46401 ) ;
#47052 = DIRECTION ( 'NONE',  ( 1.000000000000000000, 0.000000000000000000, 0.000000000000000000 ) ) ;
#47053 = VECTOR ( 'NONE', #50605, 1000.000000000000000 ) ;
#47054 = EDGE_CURVE ( 'NONE', #64495, #6128, #51883, .T. ) ;
#47055 = CARTESIAN_POINT ( 'NONE',  ( -37.00000000000000711, -10.70999494708496869, 5.814360711498252954 ) ) ;
#47056 = ORIENTED_EDGE ( 'NONE', *, *, #1681, .F. ) ;
#47057 = AXIS2_PLACEMENT_3D ( 'NONE', #41551, #46243, #55882 ) ;
#47058 = FACE_OUTER_BOUND ( 'NONE', #8782, .T. ) ;
#47059 = CARTESIAN_POINT ( 'NONE',  ( -3.818603701402922823, -10.58165328604947319, 5.676754050214040781 ) ) ;
#47060 = CIRCLE ( 'NONE', #38551, 12.74999999999999822 ) ;
#47061 = CIRCLE ( 'NONE', #29017, 2.899999999999995470 ) ;
#47062 = CARTESIAN_POINT ( 'NONE',  ( 0.2648978790185593790, 4.312320170909392125, -11.46165506714223703 ) ) ;
#47063 = CYLINDRICAL_SURFACE ( 'NONE', #22614, 12.18650000000000055 ) ;
#47064 = EDGE_CURVE ( 'NONE', #62523, #28210, #54816, .T. ) ;
#47065 = CARTESIAN_POINT ( 'NONE',  ( 0.2650492433740059828, 12.04046084639676373, -2.234874822562773478 ) ) ;
#47066 = VECTOR ( 'NONE', #56945, 1000.000000000000000 ) ;
#47067 = LINE ( 'NONE', #42049, #48017 ) ;
#47068 = ORIENTED_EDGE ( 'NONE', *, *, #1550, .T. ) ;
#47069 = CARTESIAN_POINT ( 'NONE',  ( -27.08426504710140392, 0.5533780324190830102, 2.223709847896192748 ) ) ;
#47070 = CARTESIAN_POINT ( 'NONE',  ( 0.2759803524722213575, -1.940323823244580081, -12.09509972435083114 ) ) ;
#47071 = CARTESIAN_POINT ( 'NONE',  ( 2.781367136452763233, 1.052455537429629606, -7.743208838465648114 ) ) ;
#47072 = CARTESIAN_POINT ( 'NONE',  ( 2.969415267405037362, -1.748187016698512952, -7.680649281077315038 ) ) ;
#47073 = ADVANCED_FACE ( 'NONE', ( #33550 ), #24541, .T. ) ;
#47074 = CIRCLE ( 'NONE', #40697, 6.936499999999989896 ) ;
#47075 = DIRECTION ( 'NONE',  ( -1.000000000000000000, -0.000000000000000000, 0.000000000000000000 ) ) ;
#47076 = CARTESIAN_POINT ( 'NONE',  ( -27.10970334550012595, -12.25602637579915033, 5.660463253225340274 ) ) ;
#47077 = ORIENTED_EDGE ( 'NONE', *, *, #54950, .T. ) ;
#47078 = CARTESIAN_POINT ( 'NONE',  ( -37.00000000000000711, -4.725891942574680371, -10.75351884295732496 ) ) ;
#47079 = DIRECTION ( 'NONE',  ( 0.000000000000000000, 0.01356324068817998940, -0.9999080150203989437 ) ) ;
#47080 = CARTESIAN_POINT ( 'NONE',  ( -35.05012975565874456, 0.01296790604419477931, 0.005092487515914018679 ) ) ;
#47081 = EDGE_LOOP ( 'NONE', ( #23562, #34763, #20743, #36906 ) ) ;
#47082 = DIRECTION ( 'NONE',  ( -1.000000000000000000, 0.000000000000000000, 0.000000000000000000 ) ) ;
#47083 = DIRECTION ( 'NONE',  ( 0.000000000000000000, 0.1081190184239353008, 0.9941379571543603744 ) ) ;
#47084 = CARTESIAN_POINT ( 'NONE',  ( -35.00000000000000000, 11.16627499335650242, 3.645068577060221582 ) ) ;
#47085 = EDGE_CURVE ( 'NONE', #54640, #35397, #34890, .T. ) ;
#47086 = AXIS2_PLACEMENT_3D ( 'NONE', #46197, #5294, #41843 ) ;
#47087 = CIRCLE ( 'NONE', #30074, 5.000000000000000000 ) ;
#47089 = ORIENTED_EDGE ( 'NONE', *, *, #65675, .F. ) ;
#47088 = CARTESIAN_POINT ( 'NONE',  ( 0.2652384529303140615, -12.24598125395191417, 0.06607367983849406212 ) ) ;
#47090 = DIRECTION ( 'NONE',  ( -1.000000000000000000, 0.000000000000000000, 0.000000000000000000 ) ) ;
#47091 = ADVANCED_FACE ( 'NONE', ( #33859 ), #23240, .T. ) ;
#47092 = AXIS2_PLACEMENT_3D ( 'NONE', #50992, #1102, #5786 ) ;
#47093 = CIRCLE ( 'NONE', #43900, 4.999999999999999112 ) ;
#47094 = FACE_OUTER_BOUND ( 'NONE', #52951, .T. ) ;
#47095 = VERTEX_POINT ( 'NONE', #18268 ) ;
#47096 = CARTESIAN_POINT ( 'NONE',  ( -35.00000000000000000, -8.029056188533626681, -8.573591947375405198 ) ) ;
#47097 = CARTESIAN_POINT ( 'NONE',  ( -27.10719052120871098, 1.714424047991082389, 1.622102031466668093 ) ) ;
#47098 = CARTESIAN_POINT ( 'NONE',  ( 0.2652384770603670727, -7.922175044417039125, 9.338499095996397159 ) ) ;
#47099 = FACE_OUTER_BOUND ( 'NONE', #61716, .T. ) ;
#47100 = DIRECTION ( 'NONE',  ( -0.5446691071471760903, 0.8386510381079236298, 0.000000000000000000 ) ) ;
#47101 = VECTOR ( 'NONE', #2060, 1000.000000000000000 ) ;
#47102 = CARTESIAN_POINT ( 'NONE',  ( 0.2833330754217406877, 5.950193237802404944, 10.71034013638380067 ) ) ;
#47104 = ORIENTED_EDGE ( 'NONE', *, *, #23767, .T. ) ;
#47103 = CARTESIAN_POINT ( 'NONE',  ( 0.2801149460245167533, 11.44368419510491108, -4.374013318106434234 ) ) ;
#47105 = VERTEX_POINT ( 'NONE', #13269 ) ;
#47106 = CARTESIAN_POINT ( 'NONE',  ( -29.43980975494970309, -3.641506875706030488, 12.99959336572439561 ) ) ;
#47107 = AXIS2_PLACEMENT_3D ( 'NONE', #4289, #24562, #44842 ) ;
#47108 = EDGE_LOOP ( 'NONE', ( #18971, #31575, #36234, #64555 ) ) ;
#47109 = APPLICATION_PROTOCOL_DEFINITION ( 'draft international standard', 'automotive_design', 1998, #20477 ) ;
#47110 = CARTESIAN_POINT ( 'NONE',  ( 1.194176325881340039, -11.61285876598809175, 4.773862381874691252 ) ) ;
#47111 = EDGE_CURVE ( 'NONE', #59819, #29583, #56121, .T. ) ;
#47112 = CIRCLE ( 'NONE', #54570, 12.18649999999999878 ) ;
#47113 = CARTESIAN_POINT ( 'NONE',  ( 2.827825597296805160, 1.027532345921684742, 8.965636292765712057 ) ) ;
#47114 = CARTESIAN_POINT ( 'NONE',  ( 37.00000000000000711, 4.705694406421931860E-17, -3.469127814946512892E-15 ) ) ;
#47115 = ORIENTED_EDGE ( 'NONE', *, *, #31424, .F. ) ;
#47116 = CYLINDRICAL_SURFACE ( 'NONE', #60600, 2.899999999999994582 ) ;
#47117 = CARTESIAN_POINT ( 'NONE',  ( -27.35552965826137140, -1.773915698030568366, 2.548625910254532112 ) ) ;
#47118 = DIRECTION ( 'NONE',  ( -1.000000000000000000, -1.836970198721029688E-16, -0.000000000000000000 ) ) ;
#47119 = ORIENTED_EDGE ( 'NONE', *, *, #63792, .T. ) ;
#47120 = AXIS2_PLACEMENT_3D ( 'NONE', #6650, #32220, #46875 ) ;
#47121 = ORIENTED_EDGE ( 'NONE', *, *, #27671, .F. ) ;
#47122 = CYLINDRICAL_SURFACE ( 'NONE', #38509, 25.00000000000000000 ) ;
#47123 = VERTEX_POINT ( 'NONE', #44173 ) ;
#47124 = CARTESIAN_POINT ( 'NONE',  ( 2.241526690369555208, 1.308664175663869500, -7.521460607153586331 ) ) ;
#47125 = CARTESIAN_POINT ( 'NONE',  ( 37.00000000000000711, 5.921969905510355403, -10.14408668126215929 ) ) ;
#47126 = CARTESIAN_POINT ( 'NONE',  ( -36.00000000000000711, -1.113475361586399925, -12.70128625845194215 ) ) ;
#47127 = CARTESIAN_POINT ( 'NONE',  ( 1.459561108992491141, 12.54631635028832548, 1.570807238541433115 ) ) ;
#47128 = EDGE_CURVE ( 'NONE', #10479, #37783, #6260, .T. ) ;
#47129 = DIRECTION ( 'NONE',  ( 1.000000000000000000, 0.000000000000000000, 0.000000000000000000 ) ) ;
#47130 = DIRECTION ( 'NONE',  ( -1.000000000000000000, 0.000000000000000000, 0.000000000000000000 ) ) ;
#47131 = CIRCLE ( 'NONE', #23773, 12.74999999999999822 ) ;
#47132 = LINE ( 'NONE', #56434, #46075 ) ;
#47133 = ORIENTED_EDGE ( 'NONE', *, *, #38267, .F. ) ;
#47134 = CARTESIAN_POINT ( 'NONE',  ( -35.00000000000000000, -11.44858830469742017, 2.627174906296871448 ) ) ;
#47135 = VERTEX_POINT ( 'NONE', #24212 ) ;
#47136 = LINE ( 'NONE', #57773, #26846 ) ;
#47137 = DIRECTION ( 'NONE',  ( 0.000000000000000000, 0.01356324068817998940, -0.9999080150203990547 ) ) ;
#47139 = CARTESIAN_POINT ( 'NONE',  ( -7.594175326315255603, 6.461734609435446863, -10.13293342493276761 ) ) ;
#47138 = AXIS2_PLACEMENT_3D ( 'NONE', #17775, #7129, #37387 ) ;
#47140 = CARTESIAN_POINT ( 'NONE',  ( 2.247206125382828823, -3.917979829727955110, 6.554642244888448488 ) ) ;
#47141 = CARTESIAN_POINT ( 'NONE',  ( 0.2717059086739051499, -10.69429229731972519, -5.971041827598930318 ) ) ;
#47142 = VECTOR ( 'NONE', #5078, 1000.000000000000000 ) ;
#47143 = DIRECTION ( 'NONE',  ( 0.000000000000000000, -0.01356324068818000328, 0.9999080150203990547 ) ) ;
#47144 = VERTEX_POINT ( 'NONE', #49511 ) ;
#47145 = VECTOR ( 'NONE', #45929, 1000.000000000000000 ) ;
#47146 = ORIENTED_EDGE ( 'NONE', *, *, #62381, .F. ) ;
#47147 = DIRECTION ( 'NONE',  ( 1.000000000000000000, 0.000000000000000000, 0.000000000000000000 ) ) ;
#47148 = EDGE_CURVE ( 'NONE', #31240, #46242, #14717, .T. ) ;
#47149 = ORIENTED_EDGE ( 'NONE', *, *, #51730, .F. ) ;
#47150 = DIRECTION ( 'NONE',  ( 0.000000000000000000, -0.9246979985058764173, -0.3807014730195119045 ) ) ;
#47151 = DIRECTION ( 'NONE',  ( -1.000000000000000000, 0.000000000000000000, 0.000000000000000000 ) ) ;
#47152 = CIRCLE ( 'NONE', #20560, 5.000000000000000000 ) ;
#47153 = CARTESIAN_POINT ( 'NONE',  ( 2.258463476536662462, 4.806099079317524669, 5.939075453322714360 ) ) ;
#47154 = ADVANCED_FACE ( 'NONE', ( #8274 ), #31269, .F. ) ;
#47155 = DIRECTION ( 'NONE',  ( 0.000000000000000000, 0.01356324068817998940, -0.9999080150203989437 ) ) ;
#47156 = ORIENTED_EDGE ( 'NONE', *, *, #3009, .F. ) ;
#47157 = CIRCLE ( 'NONE', #3651, 2.899999999999995470 ) ;
#47158 = CARTESIAN_POINT ( 'NONE',  ( 0.2801149460245144773, 12.09752788490057895, 1.933835447580672495 ) ) ;
#47159 = FACE_OUTER_BOUND ( 'NONE', #48867, .T. ) ;
#47160 = CARTESIAN_POINT ( 'NONE',  ( 0.6473888112830256114, -1.823007254467038596, 12.23851338376148234 ) ) ;
#47161 = CARTESIAN_POINT ( 'NONE',  ( -33.02316666837518255, -2.861627175174543680, 23.69173491641419105 ) ) ;
#47162 = VECTOR ( 'NONE', #19375, 1000.000000000000000 ) ;
#47164 = EDGE_CURVE ( 'NONE', #36560, #39587, #64757, .T. ) ;
#47163 = B_SPLINE_CURVE_WITH_KNOTS ( 'NONE', 3,
 ( #20765, #24775, #60026, #35708, #45054, #4165 ),
 .UNSPECIFIED., .F., .F.,
 ( 4, 2, 4 ),
 ( 0.000000000000000000, 0.0004528561986909421331, 0.0009057123973818842662 ),
 .UNSPECIFIED. ) ;
#47165 = CARTESIAN_POINT ( 'NONE',  ( 35.00000000000000000, 4.705694406421931860E-17, -3.469127814946512892E-15 ) ) ;
#47166 = CARTESIAN_POINT ( 'NONE',  ( 3.152665057733966769, 0.9030954876739563097, 7.886634106564108571 ) ) ;
#47167 = VERTEX_POINT ( 'NONE', #39504 ) ;
#47168 = AXIS2_PLACEMENT_3D ( 'NONE', #34436, #64671, #55718 ) ;
#47169 = DIRECTION ( 'NONE',  ( 0.000000000000000000, 0.6269146997507986097, 0.7790879021242506086 ) ) ;
#47170 = ORIENTED_EDGE ( 'NONE', *, *, #19228, .F. ) ;
#47171 = CARTESIAN_POINT ( 'NONE',  ( 10.48620311856346454, 8.250315036047107142, -10.68561190601526789 ) ) ;
#47172 = CARTESIAN_POINT ( 'NONE',  ( 2.241537034860904942, 7.172440248506164018, 2.615577641485550497 ) ) ;
#47173 = DIRECTION ( 'NONE',  ( -1.000000000000000000, -0.000000000000000000, -0.000000000000000000 ) ) ;
#47174 = ADVANCED_FACE ( 'NONE', ( #59797 ), #14230, .T. ) ;
#47175 = CARTESIAN_POINT ( 'NONE',  ( -22.30625920655495165, -3.635849356906410534, 1.076742202099151946 ) ) ;
#47176 = DIRECTION ( 'NONE',  ( 0.000000000000000000, 0.01356324068817998940, -0.9999080150203990547 ) ) ;
#47177 = EDGE_LOOP ( 'NONE', ( #31076, #14386, #10591, #15518 ) ) ;
#47178 = ORIENTED_EDGE ( 'NONE', *, *, #1799, .T. ) ;
#47180 = EDGE_CURVE ( 'NONE', #38246, #433, #25320, .T. ) ;
#47179 = CARTESIAN_POINT ( 'NONE',  ( 2.000000000000001776, 0.000000000000000000, 0.000000000000000000 ) ) ;
#47181 = ORIENTED_EDGE ( 'NONE', *, *, #44443, .F. ) ;
#47182 = DIRECTION ( 'NONE',  ( -1.000000000000000000, -0.000000000000000000, 0.000000000000000000 ) ) ;
#47183 = CARTESIAN_POINT ( 'NONE',  ( 2.000000000000001776, 0.000000000000000000, 0.000000000000000000 ) ) ;
#47184 = CYLINDRICAL_SURFACE ( 'NONE', #2282, 4.999999999999999112 ) ;
#47185 = CARTESIAN_POINT ( 'NONE',  ( 2.241534463349552198, 0.005244187652470188102, -7.634462073473343935 ) ) ;
#47186 = CARTESIAN_POINT ( 'NONE',  ( 1.634816307077033182, -7.601181930720684043, -10.17753964889855567 ) ) ;
#47187 = CARTESIAN_POINT ( 'NONE',  ( 2.297017764050091504, -1.166330442180224747, 7.563558677601593061 ) ) ;
#47188 = CARTESIAN_POINT ( 'NONE',  ( 1.462291587753156152, 12.54737685278498738, -1.569662666435215126 ) ) ;
#47189 = ORIENTED_EDGE ( 'NONE', *, *, #48260, .F. ) ;
#47190 = AXIS2_PLACEMENT_3D ( 'NONE', #47096, #52072, #57064 ) ;
#47191 = B_SPLINE_CURVE_WITH_KNOTS ( 'NONE', 3,
 ( #8519, #51069, #9172, #30753, #49751, #45737, #60058, #15144, #40081, #35427, #39768, #55731, #65668, #24810, #10161, #34754 ),
 .UNSPECIFIED., .F., .F.,
 ( 4, 3, 3, 3, 3, 4 ),
 ( 2.030687410393290492E-15, 0.0002126834539180011104, 0.0004253519300366869599, 0.0006380165497225099560, 0.0007442707582429343698, 0.0009453531351411225900 ),
 .UNSPECIFIED. ) ;
#47192 = VECTOR ( 'NONE', #6922, 1000.000000000000000 ) ;
#47193 = CARTESIAN_POINT ( 'NONE',  ( -27.32337605527168023, 1.175835497775001626, 2.771816950947462832 ) ) ;
#47194 = EDGE_LOOP ( 'NONE', ( #35839, #33851, #29343, #30324 ) ) ;
#47195 = DIRECTION ( 'NONE',  ( 0.000000000000000000, -0.01356324068817991481, 0.9999080150203990547 ) ) ;
#47196 = CARTESIAN_POINT ( 'NONE',  ( -9.197504613504071003, 11.40546504581822695, -3.730959538268481257 ) ) ;
#47197 = CARTESIAN_POINT ( 'NONE',  ( 0.6511581176974240437, 8.205008037407228727, -9.263557799003033111 ) ) ;
#47198 = DIRECTION ( 'NONE',  ( -1.000000000000000000, 0.000000000000000000, 0.000000000000000000 ) ) ;
#47199 = ORIENTED_EDGE ( 'NONE', *, *, #26044, .T. ) ;
#47200 = DIRECTION ( 'NONE',  ( -1.000000000000000000, -0.000000000000000000, 0.000000000000000000 ) ) ;
#47201 = CARTESIAN_POINT ( 'NONE',  ( -22.31328051695926007, 1.671726071983979711, -3.401210163132561082 ) ) ;
#47202 = DIRECTION ( 'NONE',  ( 0.000000000000000000, 0.9999080150203989437, 0.01356324068817649567 ) ) ;
#47203 = ORIENTED_EDGE ( 'NONE', *, *, #28693, .F. ) ;
#47204 = ORIENTED_EDGE ( 'NONE', *, *, #10910, .F. ) ;
#47205 = CARTESIAN_POINT ( 'NONE',  ( -37.00000000000000711, 5.814360711498292034, 10.70999494708494737 ) ) ;
#47206 = VERTEX_POINT ( 'NONE', #40479 ) ;
#47207 = ORIENTED_EDGE ( 'NONE', *, *, #60729, .T. ) ;
#47208 = VECTOR ( 'NONE', #38705, 1000.000000000000000 ) ;
#47209 = VERTEX_POINT ( 'NONE', #15211 ) ;
#47210 = ORIENTED_EDGE ( 'NONE', *, *, #65425, .T. ) ;
#47211 = CARTESIAN_POINT ( 'NONE',  ( 0.3341166715381296282, 4.432780143632490066, 11.44035855572976423 ) ) ;
#47212 = CIRCLE ( 'NONE', #63136, 12.75000000000000178 ) ;
#47213 = CARTESIAN_POINT ( 'NONE',  ( 2.247206125382661845, 4.996658593544773375, -5.774712443419645957 ) ) ;
#47214 = ADVANCED_FACE ( 'NONE', ( #24880 ), #13388, .F. ) ;
#47215 = DIRECTION ( 'NONE',  ( -0.000000000000000000, -0.000000000000000000, -1.000000000000000000 ) ) ;
#47216 = DIRECTION ( 'NONE',  ( -1.000000000000000000, -0.000000000000000000, -0.000000000000000000 ) ) ;
#47217 = FACE_OUTER_BOUND ( 'NONE', #59035, .T. ) ;
#47218 = VERTEX_POINT ( 'NONE', #30818 ) ;
#47219 = CARTESIAN_POINT ( 'NONE',  ( -22.65996813707687707, -4.069902221062768000, -2.607318832796705177 ) ) ;
#47220 = EDGE_LOOP ( 'NONE', ( #63803, #9857, #13155, #38952 ) ) ;
#47221 =( BOUNDED_CURVE ( )  B_SPLINE_CURVE ( 3, ( #52666, #37011, #11737, #32024 ),
 .UNSPECIFIED., .F., .F. ) 
 B_SPLINE_CURVE_WITH_KNOTS ( ( 4, 4 ),
 ( 4.594111722311771118, 4.635963600959730258 ),
 .UNSPECIFIED. ) 
 CURVE ( )  GEOMETRIC_REPRESENTATION_ITEM ( )  RATIONAL_B_SPLINE_CURVE ( ( 1.000000000000000000, 0.9998540403475023597, 0.9998540403475023597, 1.000000000000000000 ) ) 
 REPRESENTATION_ITEM ( '' )  );
#47222 = FACE_BOUND ( 'NONE', #6080, .T. ) ;
#47223 = AXIS2_PLACEMENT_3D ( 'NONE', #21667, #61539, #15982 ) ;
#47224 = CARTESIAN_POINT ( 'NONE',  ( 47.00000000000000711, 4.705694406421931860E-17, -3.469127814946512892E-15 ) ) ;
#47225 = CARTESIAN_POINT ( 'NONE',  ( 2.241352910868909643, 3.744764251557084922, -6.652881166698471738 ) ) ;
#47226 = LINE ( 'NONE', #11304, #3154 ) ;
#47227 = FACE_OUTER_BOUND ( 'NONE', #17725, .T. ) ;
#47228 = CARTESIAN_POINT ( 'NONE',  ( 2.931247277082682512, -7.855653518374111854, -0.3703309885897621556 ) ) ;
#47229 = CIRCLE ( 'NONE', #55716, 5.000000000000000888 ) ;
#47230 = EDGE_CURVE ( 'NONE', #52387, #26102, #64269, .T. ) ;
#47231 = ORIENTED_EDGE ( 'NONE', *, *, #14242, .F. ) ;
#47232 = CARTESIAN_POINT ( 'NONE',  ( -37.00000000000000711, 0.000000000000000000, 0.000000000000000000 ) ) ;
#47233 = ORIENTED_EDGE ( 'NONE', *, *, #14028, .T. ) ;
#47234 = EDGE_CURVE ( 'NONE', #64575, #6120, #24075, .T. ) ;
#47235 = FACE_OUTER_BOUND ( 'NONE', #18592, .T. ) ;
#47236 = CARTESIAN_POINT ( 'NONE',  ( 14.88292245651501666, -27.94758995389113210, -11.26211297105861142 ) ) ;
#47237 = CARTESIAN_POINT ( 'NONE',  ( 3.152665057734130638, 7.609997527621177760, -2.258875078502145861 ) ) ;
#47238 = CARTESIAN_POINT ( 'NONE',  ( -27.08639648637141661, -0.6092497698725154454, -2.215564006614442416 ) ) ;
#47239 = EDGE_CURVE ( 'NONE', #17397, #28779, #50824, .T. ) ;
#47240 = CARTESIAN_POINT ( 'NONE',  ( 2.639814597422738718, -4.793557287999591132, -6.111633106000479820 ) ) ;
#47241 = EDGE_LOOP ( 'NONE', ( #30884, #13322, #39432, #63158 ) ) ;
#47242 = CIRCLE ( 'NONE', #33402, 5.000000000000000000 ) ;
#47243 = LINE ( 'NONE', #6337, #41947 ) ;
#47244 = DIRECTION ( 'NONE',  ( -0.000000000000000000, -1.000000000000000000, -0.000000000000000000 ) ) ;
#47245 = CARTESIAN_POINT ( 'NONE',  ( 23.59428955459845412, 9.152238998900841693, -7.766884395375215355 ) ) ;
#47246 = DIRECTION ( 'NONE',  ( 0.000000000000000000, 0.2355298848897517117, 0.9718671068226459875 ) ) ;
#47247 = EDGE_CURVE ( 'NONE', #16971, #13636, #54005, .T. ) ;
#47248 = CARTESIAN_POINT ( 'NONE',  ( 0.2648978790185602672, 12.24533305150758089, -0.1321385342562831633 ) ) ;
#47249 = AXIS2_PLACEMENT_3D ( 'NONE', #39762, #60054, #25129 ) ;
#47250 = ORIENTED_EDGE ( 'NONE', *, *, #63538, .T. ) ;
#47251 = EDGE_CURVE ( 'NONE', #51616, #55813, #9900, .T. ) ;
#47252 = CARTESIAN_POINT ( 'NONE',  ( 2.907497136250241976, -0.3592423305251857268, -7.848280798452723417 ) ) ;
#47253 = CARTESIAN_POINT ( 'NONE',  ( 0.2653519890518185043, -2.126521162241138185, 12.06015162724940382 ) ) ;
#47254 = AXIS2_PLACEMENT_3D ( 'NONE', #33289, #3050, #43576 ) ;
#47255 = ADVANCED_FACE ( 'NONE', ( #30186 ), #5930, .T. ) ;
#47256 = AXIS2_PLACEMENT_3D ( 'NONE', #7240, #27869, #48178 ) ;
#47257 = ORIENTED_EDGE ( 'NONE', *, *, #21113, .T. ) ;
#47258 = EDGE_CURVE ( 'NONE', #13243, #36795, #65733, .T. ) ;
#47259 = VERTEX_POINT ( 'NONE', #15535 ) ;
#47260 = DIRECTION ( 'NONE',  ( -1.000000000000000000, -0.000000000000000000, 0.000000000000000000 ) ) ;
#47261 = CARTESIAN_POINT ( 'NONE',  ( 48.79774903324594248, -0.2423453535664415182, 3.134413741627073868 ) ) ;
#47262 = DIRECTION ( 'NONE',  ( -0.000000000000000000, -0.000000000000000000, -1.000000000000000000 ) ) ;
#47263 = EDGE_CURVE ( 'NONE', #16108, #9767, #56099, .T. ) ;
#47264 = CARTESIAN_POINT ( 'NONE',  ( 0.2915757698887287974, -1.916267336493256757, 12.10419100255479563 ) ) ;
#47265 = VERTEX_POINT ( 'NONE', #600 ) ;
#47266 = B_SPLINE_CURVE_WITH_KNOTS ( 'NONE', 3,
 ( #35143, #5589, #24531, #60112, #55453, #45459, #34508, #65727, #40819, #56093, #20197, #9889, #35489 ),
 .UNSPECIFIED., .F., .F.,
 ( 4, 3, 3, 3, 4 ),
 ( 3.878959614448864246E-18, 6.607593386745442947E-05, 0.0001321518677373505364, 0.0001982171734706177969, 0.0002642860854759470366 ),
 .UNSPECIFIED. ) ;
#47267 = ORIENTED_EDGE ( 'NONE', *, *, #57411, .F. ) ;
#47268 = VERTEX_POINT ( 'NONE', #20861 ) ;
#47269 = DIRECTION ( 'NONE',  ( 1.000000000000000000, 0.000000000000000000, 0.000000000000000000 ) ) ;
#47270 = CIRCLE ( 'NONE', #51557, 5.000000000000001776 ) ;
#47271 = CARTESIAN_POINT ( 'NONE',  ( 10.48620311856346454, 8.250315036047107142, 8.713914264323181058 ) ) ;
#47272 = ORIENTED_EDGE ( 'NONE', *, *, #5950, .T. ) ;
#47273 = CARTESIAN_POINT ( 'NONE',  ( 37.25000000000000711, -27.32965888902624840, 3.759436751556509915 ) ) ;
#47274 = DIRECTION ( 'NONE',  ( 0.000000000000000000, -0.01356324068817991828, 0.9999080150203990547 ) ) ;
#47275 = VERTEX_POINT ( 'NONE', #41129 ) ;
#47276 = CARTESIAN_POINT ( 'NONE',  ( 0.2652384529303143390, 11.48485968917279365, -4.250461213012427741 ) ) ;
#47277 = CARTESIAN_POINT ( 'NONE',  ( 13.56792483472022681, -30.10715271124523440, -6.611461891173261662 ) ) ;
#47278 = CARTESIAN_POINT ( 'NONE',  ( -35.00000000000000000, 12.60630747491665815, -1.908798535168240607 ) ) ;
#47279 = VERTEX_POINT ( 'NONE', #61411 ) ;
#47280 = LINE ( 'NONE', #57581, #15054 ) ;
#47281 = ORIENTED_EDGE ( 'NONE', *, *, #20910, .T. ) ;
#47282 = AXIS2_PLACEMENT_3D ( 'NONE', #22371, #12387, #42637 ) ;
#47283 = CARTESIAN_POINT ( 'NONE',  ( 12.47628546223243617, 0.000000000000000000, -13.50000000000000178 ) ) ;
#47284 = CARTESIAN_POINT ( 'NONE',  ( -17.85006501957281699, -6.222042789639135485, 11.98374378373027582 ) ) ;
#47285 = CARTESIAN_POINT ( 'NONE',  ( 15.04427341496945481, -34.74416750921023578, -6.992747701485109602 ) ) ;
#47286 = DIRECTION ( 'NONE',  ( 0.000000000000000000, -0.2618041379715496664, 0.9651210252299831094 ) ) ;
#47287 = EDGE_CURVE ( 'NONE', #8090, #49536, #15850, .T. ) ;
#47288 = ADVANCED_FACE ( 'NONE', ( #46460 ), #28727, .F. ) ;
#47289 = DIRECTION ( 'NONE',  ( 0.000000000000000000, 0.5243256840888563808, 0.8515178078024867592 ) ) ;
#47290 = CARTESIAN_POINT ( 'NONE',  ( 1.719304012338199517, 0.000000000000000000, 0.000000000000000000 ) ) ;
#47291 = CARTESIAN_POINT ( 'NONE',  ( 0.2646305136544065406, -6.237419468587153126, 10.53923716745244832 ) ) ;
#47292 = CARTESIAN_POINT ( 'NONE',  ( 5.516018279890452902, -0.006286471671802459221, -0.002527316374434270853 ) ) ;
#47293 = ORIENTED_EDGE ( 'NONE', *, *, #25341, .F. ) ;
#47294 = CARTESIAN_POINT ( 'NONE',  ( 35.00000000000000000, -12.18632975068352664, -0.06441628369832411161 ) ) ;
#47295 = AXIS2_PLACEMENT_3D ( 'NONE', #44925, #34917, #55226 ) ;
#47296 = EDGE_LOOP ( 'NONE', ( #39130, #27674, #16486, #19557 ) ) ;
#47297 = CARTESIAN_POINT ( 'NONE',  ( 2.000000000000001776, -4.976357229393820525, -4.652926418895619420 ) ) ;
#47298 = DIRECTION ( 'NONE',  ( 0.000000000000000000, 0.01356324068817998940, -0.9999080150203990547 ) ) ;
#47299 = VERTEX_POINT ( 'NONE', #42107 ) ;
#47300 = EDGE_CURVE ( 'NONE', #42662, #56972, #28496, .T. ) ;
#47301 = CARTESIAN_POINT ( 'NONE',  ( 3.092491956585768254, 7.581757403488332159, 2.283527081234053568 ) ) ;
#47302 = CARTESIAN_POINT ( 'NONE',  ( 0.2648978790185602672, 6.237101853238547378, 10.53870023327865901 ) ) ;
#47303 = DIRECTION ( 'NONE',  ( -1.000000000000000000, -0.000000000000000000, -0.000000000000000000 ) ) ;
#47304 = ORIENTED_EDGE ( 'NONE', *, *, #48984, .F. ) ;
#47305 = EDGE_CURVE ( 'NONE', #13727, #35208, #32138, .T. ) ;
#47306 = ORIENTED_EDGE ( 'NONE', *, *, #46172, .F. ) ;
#47307 = CARTESIAN_POINT ( 'NONE',  ( -17.16021277067101281, -7.891355405082562058, -9.047158298165973278 ) ) ;
#47308 = ORIENTED_EDGE ( 'NONE', *, *, #24219, .F. ) ;
#47309 = PLANE ( 'NONE',  #54016 ) ;
#47310 = CARTESIAN_POINT ( 'NONE',  ( 2.000000000000001776, 0.000000000000000000, 0.000000000000000000 ) ) ;
#47311 = CARTESIAN_POINT ( 'NONE',  ( -2.532614230583023041, -12.88560382747352584, 4.026315189028235153 ) ) ;
#47312 = DIRECTION ( 'NONE',  ( 0.000000000000000000, -0.3193015301359669600, -0.9476531711828067861 ) ) ;
#47313 = EDGE_CURVE ( 'NONE', #30591, #34726, #62481, .T. ) ;
#47314 = CARTESIAN_POINT ( 'NONE',  ( -17.65431273644522392, -7.797115439854604979, 9.126847883897077907 ) ) ;
#47315 = VERTEX_POINT ( 'NONE', #11220 ) ;
#47316 = CYLINDRICAL_SURFACE ( 'NONE', #41209, 12.18650000000000055 ) ;
#47317 = AXIS2_PLACEMENT_3D ( 'NONE', #47310, #37303, #57616 ) ;
#47318 = CYLINDRICAL_SURFACE ( 'NONE', #34101, 3.309571291727934295 ) ;
#47319 = EDGE_CURVE ( 'NONE', #28687, #34363, #26501, .T. ) ;
#47320 = DIRECTION ( 'NONE',  ( 0.000000000000000000, 0.000000000000000000, 1.000000000000000000 ) ) ;
#47321 = CARTESIAN_POINT ( 'NONE',  ( 0.3218525148189865237, -5.919623386703263712, -10.74192973049794375 ) ) ;
#47322 = EDGE_CURVE ( 'NONE', #32142, #48941, #1251, .T. ) ;
#47323 = LINE ( 'NONE', #52947, #11809 ) ;
#47324 = DIRECTION ( 'NONE',  ( -1.000000000000000000, 0.000000000000000000, 0.000000000000000000 ) ) ;
#47325 = CARTESIAN_POINT ( 'NONE',  ( -22.27710395300133328, -2.585700543510490501, -2.620347679538754360 ) ) ;
#47326 = ADVANCED_FACE ( 'NONE', ( #7198 ), #20183, .F. ) ;
#47327 = ORIENTED_EDGE ( 'NONE', *, *, #60423, .F. ) ;
#47328 = EDGE_CURVE ( 'NONE', #13395, #34161, #57197, .T. ) ;
#47329 = CARTESIAN_POINT ( 'NONE',  ( 35.00000000000000000, 11.95840593935204765, 2.346765782874299155 ) ) ;
#47330 = CARTESIAN_POINT ( 'NONE',  ( 0.000000000000000000, 6.777474576704068276, 0.6925993764990892032 ) ) ;
#47331 = AXIS2_PLACEMENT_3D ( 'NONE', #50821, #46170, #26205 ) ;
#47332 = ORIENTED_EDGE ( 'NONE', *, *, #7064, .F. ) ;
#47333 = DIRECTION ( 'NONE',  ( 0.000000000000000000, 0.9635499925192236859, -0.2675283385292183680 ) ) ;
#47334 = CARTESIAN_POINT ( 'NONE',  ( 1.634816307076947695, -9.253014110596202713, -8.702988562442458331 ) ) ;
#47335 = ORIENTED_EDGE ( 'NONE', *, *, #23088, .F. ) ;
#47336 = EDGE_CURVE ( 'NONE', #53158, #42300, #32463, .T. ) ;
#47337 = DIRECTION ( 'NONE',  ( 1.000000000000000000, -0.000000000000000000, 0.000000000000000000 ) ) ;
#47338 = ORIENTED_EDGE ( 'NONE', *, *, #63275, .F. ) ;
#47339 = CARTESIAN_POINT ( 'NONE',  ( 0.3341166715381302943, -5.914486946113987287, 10.74942732659230238 ) ) ;
#47340 = ORIENTED_EDGE ( 'NONE', *, *, #5519, .T. ) ;
#47341 = ORIENTED_EDGE ( 'NONE', *, *, #30587, .F. ) ;
#47342 = VECTOR ( 'NONE', #64498, 1000.000000000000000 ) ;
#47343 = CARTESIAN_POINT ( 'NONE',  ( -27.08423923533013777, -1.832018136655359841, 1.376387618994798112 ) ) ;
#47344 = ORIENTED_EDGE ( 'NONE', *, *, #27047, .F. ) ;
#47345 = CARTESIAN_POINT ( 'NONE',  ( 37.00000000000000711, -11.73463472867578261, -3.287724142101374536 ) ) ;
#47346 = CARTESIAN_POINT ( 'NONE',  ( -22.28073302975500880, -3.560599703067827360, 0.9769664947681129252 ) ) ;
#47347 = DIRECTION ( 'NONE',  ( 1.000000000000000000, 0.000000000000000000, 0.000000000000000000 ) ) ;
#47348 = CARTESIAN_POINT ( 'NONE',  ( 35.00000000000000000, -2.497432891016756251, 11.47758908105696740 ) ) ;
#47349 = ORIENTED_EDGE ( 'NONE', *, *, #11023, .T. ) ;
#47350 = CARTESIAN_POINT ( 'NONE',  ( 0.2717059086739005425, -7.737372654246648551, 9.494961435243668646 ) ) ;
#47351 = CARTESIAN_POINT ( 'NONE',  ( 4.682340427901537261, -31.48164499408211014, 13.94155213824621953 ) ) ;
#47352 = CARTESIAN_POINT ( 'NONE',  ( 37.00000000000000711, 10.14433819232443490, 6.753013023069604159 ) ) ;
#47354 = ORIENTED_EDGE ( 'NONE', *, *, #7007, .T. ) ;
#47353 = LINE ( 'NONE', #18066, #55254 ) ;
#47355 = CARTESIAN_POINT ( 'NONE',  ( -28.21004269438542522, 10.37327567629658631, -6.041082299521756127 ) ) ;
#47356 = ORIENTED_EDGE ( 'NONE', *, *, #54678, .T. ) ;
#47357 = CARTESIAN_POINT ( 'NONE',  ( 0.2653519789438749110, 9.366970421692881743, -7.888580323518779025 ) ) ;
#47358 = ORIENTED_EDGE ( 'NONE', *, *, #8392, .T. ) ;
#47359 = CARTESIAN_POINT ( 'NONE',  ( 37.00000000000000711, -12.60630747491661374, 1.908798535168511057 ) ) ;
#47360 = CYLINDRICAL_SURFACE ( 'NONE', #62899, 4.999999999999999112 ) ;
#47361 = CARTESIAN_POINT ( 'NONE',  ( 0.7446945582510989814, -4.576048078258570406, 11.53120448859754887 ) ) ;
#47362 = CIRCLE ( 'NONE', #36578, 4.999999999999999112 ) ;
#47364 = EDGE_CURVE ( 'NONE', #20627, #50714, #1170, .T. ) ;
#47363 = VERTEX_POINT ( 'NONE', #22169 ) ;
#47365 = CARTESIAN_POINT ( 'NONE',  ( -37.00000000000000711, 6.280308599560139093, 9.926225166347048656 ) ) ;
#47366 = CARTESIAN_POINT ( 'NONE',  ( 0.3040950598368152291, 12.02925914197708757, -2.376091969481093358 ) ) ;
#47367 = CARTESIAN_POINT ( 'NONE',  ( -22.27878402819508352, -3.562981801125738368, -0.9457981527432679503 ) ) ;
#47368 = ORIENTED_EDGE ( 'NONE', *, *, #26702, .T. ) ;
#47369 = ADVANCED_FACE ( 'NONE', ( #53090 ), #7529, .T. ) ;
#47370 = ORIENTED_EDGE ( 'NONE', *, *, #62641, .T. ) ;
#47371 = CARTESIAN_POINT ( 'NONE',  ( 2.899286259009684397, 7.664525129300157502, 1.713434346771250283 ) ) ;
#47372 = ORIENTED_EDGE ( 'NONE', *, *, #22162, .T. ) ;
#47373 = EDGE_LOOP ( 'NONE', ( #36329, #55417, #52718, #22401, #47349, #5957, #47431 ) ) ;
#47374 = EDGE_CURVE ( 'NONE', #19607, #14001, #27451, .T. ) ;
#47375 = DIRECTION ( 'NONE',  ( 0.000000000000000000, 0.01356324068817998940, -0.9999080150203990547 ) ) ;
#47376 = DIRECTION ( 'NONE',  ( 1.000000000000000000, -0.000000000000000000, 0.000000000000000000 ) ) ;
#47377 = CARTESIAN_POINT ( 'NONE',  ( 2.241528039335008327, -7.168649579907108382, -2.625917297988457744 ) ) ;
#47378 = DIRECTION ( 'NONE',  ( -1.000000000000000000, 0.000000000000000000, 0.000000000000000000 ) ) ;
#47379 = CARTESIAN_POINT ( 'NONE',  ( 5.515539859299206427, -0.002251761459665569190, 0.005618668168217179175 ) ) ;
#47380 = CARTESIAN_POINT ( 'NONE',  ( 5.536195898058073439, 0.005656495196970890219, -0.006344799443923454345 ) ) ;
#47381 = AXIS2_PLACEMENT_3D ( 'NONE', #53668, #28375, #39321 ) ;
#47382 = CARTESIAN_POINT ( 'NONE',  ( 36.00000000000000711, -8.954052073409666690, -9.076753354953966735 ) ) ;
#47383 = VECTOR ( 'NONE', #14089, 1000.000000000000000 ) ;
#47384 = ORIENTED_EDGE ( 'NONE', *, *, #51224, .F. ) ;
#47385 = CARTESIAN_POINT ( 'NONE',  ( 22.57855258442565116, 3.026812727784649493, -13.15630665159948975 ) ) ;
#47386 = B_SPLINE_CURVE_WITH_KNOTS ( 'NONE', 3,
 ( #14382, #9076, #29355, #49652, #64917, #39661, #34654, #54951, #24702, #41282, #14690, #4774, #21000, #44981, #16011, #10061, #35644, #15033, #10370 ),
 .UNSPECIFIED., .F., .F.,
 ( 4, 3, 3, 3, 3, 3, 4 ),
 ( 0.000000000000000000, 2.836829842860636775E-05, 4.224792512343439213E-05, 5.612066614708047458E-05, 6.998859278151889341E-05, 9.832141287888834162E-05, 0.0001178161482480083770 ),
 .UNSPECIFIED. ) ;
#47387 = DIRECTION ( 'NONE',  ( -0.000000000000000000, -1.000000000000000000, -0.000000000000000000 ) ) ;
#47388 = EDGE_CURVE ( 'NONE', #30904, #25281, #64610, .T. ) ;
#47389 = B_SPLINE_CURVE_WITH_KNOTS ( 'NONE', 3,
 ( #36508, #51812, #25886, #15870, #292, #30519, #31511, #46480, #6259, #50823, #46806, #31198, #21880, #56120, #6590, #36154 ),
 .UNSPECIFIED., .F., .F.,
 ( 4, 3, 3, 3, 3, 4 ),
 ( 0.000000000000000000, 0.0002999043160757332749, 0.0005998071753050982901, 0.0008997092107374523922, 0.001204458948195600426, 0.001510329163476426982 ),
 .UNSPECIFIED. ) ;
#47390 = EDGE_CURVE ( 'NONE', #57717, #61894, #28465, .T. ) ;
#47391 = VECTOR ( 'NONE', #4091, 1000.000000000000114 ) ;
#47392 = CARTESIAN_POINT ( 'NONE',  ( 0.2759803524722223012, 4.367180139677484085, -11.44482553421627280 ) ) ;
#47393 = DIRECTION ( 'NONE',  ( 0.000000000000000000, -0.8515178078024923103, 0.5243256840888473880 ) ) ;
#47394 = CARTESIAN_POINT ( 'NONE',  ( 0.9232058338315058954, -9.306586124266649662, 8.301689855530135276 ) ) ;
#47395 =( BOUNDED_SURFACE ( )  B_SPLINE_SURFACE ( 3, 1, ( 
 ( #11699, #6741 ),
 ( #16700, #52629 ),
 ( #36661, #12036 ),
 ( #26040, #31014 ) ),
 .UNSPECIFIED., .F., .F., .F. ) 
 B_SPLINE_SURFACE_WITH_KNOTS ( ( 4, 4 ),
 ( 2, 2 ),
 ( 0.000000000000000000, 1.000000000000000000 ),
 ( 0.000000000000000000, 1.000000000000000000 ),
 .UNSPECIFIED. ) 
 GEOMETRIC_REPRESENTATION_ITEM ( )  RATIONAL_B_SPLINE_SURFACE ( (
 ( 1.000000000000000000, 1.000000000000000000),
 ( 0.6933888150995267674, 0.9895912004443193632),
 ( 0.6933888150995267674, 0.9895912004443193632),
 ( 1.000000000000000000, 1.000000000000000000) ) ) 
 REPRESENTATION_ITEM ( '' )  SURFACE ( )  );
#47396 = CARTESIAN_POINT ( 'NONE',  ( 0.2650492594609233366, 12.07870403910584223, -2.017987075343835368 ) ) ;
#47397 = DIRECTION ( 'NONE',  ( 1.000000000000000000, 0.000000000000000000, 0.000000000000000000 ) ) ;
#47398 = VERTEX_POINT ( 'NONE', #23489 ) ;
#47399 = CARTESIAN_POINT ( 'NONE',  ( -28.41827485489077532, 3.509237424706437292, 25.00000000000000000 ) ) ;
#47400 = CARTESIAN_POINT ( 'NONE',  ( 2.941278708680199916, -5.383216837018962586, 2.952340773940090646 ) ) ;
#47401 = DIRECTION ( 'NONE',  ( 1.000000000000000000, -0.000000000000000000, 0.000000000000000000 ) ) ;
#47402 = CARTESIAN_POINT ( 'NONE',  ( 3.031336079629848523, -1.779751109289636979, -7.694633165537411834 ) ) ;
#47403 = EDGE_CURVE ( 'NONE', #29168, #27894, #7285, .T. ) ;
#47404 = EDGE_CURVE ( 'NONE', #6123, #23282, #61431, .T. ) ;
#47405 = CARTESIAN_POINT ( 'NONE',  ( -24.79507913871908542, 8.359778566926882704, 8.617069398609862318 ) ) ;
#47406 = CARTESIAN_POINT ( 'NONE',  ( -24.92180037670109627, -9.674391025304601044, 9.421401640134503097 ) ) ;
#47407 = ORIENTED_EDGE ( 'NONE', *, *, #31523, .F. ) ;
#47408 = DIRECTION ( 'NONE',  ( 0.000000000000000000, 0.01356324068817991828, -0.9999080150203990547 ) ) ;
#47409 = FACE_OUTER_BOUND ( 'NONE', #14453, .T. ) ;
#47410 = CARTESIAN_POINT ( 'NONE',  ( 2.242819959140598840, -4.828731837260408888, -5.913965034148014333 ) ) ;
#47411 = CARTESIAN_POINT ( 'NONE',  ( -35.04683013664716640, -0.007968230201740866825, 0.009445816769446301053 ) ) ;
#47412 = VERTEX_POINT ( 'NONE', #3220 ) ;
#47413 = EDGE_CURVE ( 'NONE', #3865, #60104, #43195, .T. ) ;
#47414 = CARTESIAN_POINT ( 'NONE',  ( 0.2717059086739021523, 2.300075171420234099, 12.03041489115252638 ) ) ;
#47415 = CARTESIAN_POINT ( 'NONE',  ( 37.00000000000000711, 4.705694406421931860E-17, -3.469127814946512892E-15 ) ) ;
#47417 = ORIENTED_EDGE ( 'NONE', *, *, #49601, .F. ) ;
#47416 = DIRECTION ( 'NONE',  ( 0.000000000000000000, 0.6478160128811947249, -0.7617968321374878338 ) ) ;
#47418 = CARTESIAN_POINT ( 'NONE',  ( -37.00000000000000711, 0.4871980014163251882, -12.74068829017553561 ) ) ;
#47419 = EDGE_CURVE ( 'NONE', #33111, #60601, #37670, .T. ) ;
#47420 = AXIS2_PLACEMENT_3D ( 'NONE', #41021, #11107, #487 ) ;
#47421 = FACE_OUTER_BOUND ( 'NONE', #47108, .T. ) ;
#47422 = VERTEX_POINT ( 'NONE', #8849 ) ;
#47423 = DIRECTION ( 'NONE',  ( 1.000000000000000000, 0.000000000000000000, 0.000000000000000000 ) ) ;
#47424 = DIRECTION ( 'NONE',  ( 1.000000000000000000, 0.000000000000000000, 0.000000000000000000 ) ) ;
#47426 = AXIS2_PLACEMENT_3D ( 'NONE', #24319, #34297, #8717 ) ;
#47425 = CARTESIAN_POINT ( 'NONE',  ( 24.39609475304860453, -1.096898803462643457, -11.95519569193159803 ) ) ;
#47427 = CARTESIAN_POINT ( 'NONE',  ( -3.090922707259200930, -7.896884802510032664, 10.95603262241157161 ) ) ;
#47428 = LINE ( 'NONE', #1863, #23600 ) ;
#47429 = CARTESIAN_POINT ( 'NONE',  ( 0.3106921474978465714, 5.925601485921673905, 10.73438344699973435 ) ) ;
#47431 = ORIENTED_EDGE ( 'NONE', *, *, #7305, .T. ) ;
#47430 = CYLINDRICAL_SURFACE ( 'NONE', #38298, 6.936499999999988120 ) ;
#47432 = CARTESIAN_POINT ( 'NONE',  ( -18.08686583997241115, 5.151216734910855521, 10.83812558286605920 ) ) ;
#47433 = ORIENTED_EDGE ( 'NONE', *, *, #38711, .T. ) ;
#47434 = DIRECTION ( 'NONE',  ( 0.000000000000000000, -0.8369827122275287357, -0.5472293298355359603 ) ) ;
#47435 = ORIENTED_EDGE ( 'NONE', *, *, #2863, .F. ) ;
#47436 = CARTESIAN_POINT ( 'NONE',  ( 1.633930747251797211, -11.67150509329678698, 5.012862767614018722 ) ) ;
#47437 = CARTESIAN_POINT ( 'NONE',  ( 5.536195898058073439, -0.007485416011288131832, -0.004027525919832926522 ) ) ;
#47438 = CARTESIAN_POINT ( 'NONE',  ( -38.94999461337798152, -1.999059167504504630, 19.54503265464386885 ) ) ;
#47439 = CARTESIAN_POINT ( 'NONE',  ( 36.00000000000000711, 12.63095688309029008, -1.738225594540043772 ) ) ;
#47440 = VERTEX_POINT ( 'NONE', #54077 ) ;
#47441 = EDGE_CURVE ( 'NONE', #44318, #57839, #935, .T. ) ;
#47442 = CARTESIAN_POINT ( 'NONE',  ( -25.19729880547092549, -5.013571510455943958, 10.93379378137424496 ) ) ;
#47443 = CARTESIAN_POINT ( 'NONE',  ( 2.269879328256731554, 5.759117113708073887, -5.026125315665156634 ) ) ;
#47444 = ORIENTED_EDGE ( 'NONE', *, *, #54179, .T. ) ;
#47445 = ORIENTED_EDGE ( 'NONE', *, *, #48623, .T. ) ;
#47446 = CARTESIAN_POINT ( 'NONE',  ( 2.242418902651939216, -7.207816731001386756, -2.517330194228364793 ) ) ;
#47447 = EDGE_LOOP ( 'NONE', ( #4683, #46885, #17336, #41223 ) ) ;
#47448 = DIRECTION ( 'NONE',  ( 1.000000000000000000, 0.000000000000000000, 0.000000000000000000 ) ) ;
#47449 = B_SPLINE_CURVE_WITH_KNOTS ( 'NONE', 3,
 ( #25257, #34887, #50227, #45223, #4687, #24949, #65799, #35227, #55529, #9976, #30258, #31556, #17826, #33109, #20615, #46222, #37779, #61819, #58073 ),
 .UNSPECIFIED., .F., .F.,
 ( 4, 3, 3, 3, 3, 3, 4 ),
 ( 9.891822368120406898E-18, 4.457896483014692814E-05, 6.639290541541845875E-05, 8.820687556478574228E-05, 0.0001100173248778870305, 0.0001545671401658038353, 0.0001830328308068570318 ),
 .UNSPECIFIED. ) ;
#47450 = CARTESIAN_POINT ( 'NONE',  ( 37.00000000000000711, 8.295159312811978936, 8.927548052240801724 ) ) ;
#47451 = CARTESIAN_POINT ( 'NONE',  ( -35.00000000000000000, -5.391785509270885512, -10.43555801961481677 ) ) ;
#47452 = CARTESIAN_POINT ( 'NONE',  ( -37.00000000000000711, 0.000000000000000000, 0.000000000000000000 ) ) ;
#47453 = CARTESIAN_POINT ( 'NONE',  ( 5.516018279890452902, -0.006629829924290480368, 0.001397286410094396563 ) ) ;
#47454 = LINE ( 'NONE', #52449, #49811 ) ;
#47455 = CARTESIAN_POINT ( 'NONE',  ( -35.00000000000000000, -10.49591321039677005, -5.273331777780449592 ) ) ;
#47456 = ORIENTED_EDGE ( 'NONE', *, *, #62470, .T. ) ;
#47457 = CARTESIAN_POINT ( 'NONE',  ( 2.000000000000001776, 0.000000000000000000, 0.000000000000000000 ) ) ;
#47458 = VERTEX_POINT ( 'NONE', #28798 ) ;
#47459 = DIRECTION ( 'NONE',  ( -1.000000000000000000, 0.000000000000000000, 0.000000000000000000 ) ) ;
#47460 = EDGE_CURVE ( 'NONE', #9681, #19811, #49110, .T. ) ;
#47461 = CARTESIAN_POINT ( 'NONE',  ( -22.30625920655495165, -2.610366806364689651, 2.750410778797883982 ) ) ;
#47462 = CARTESIAN_POINT ( 'NONE',  ( 2.241352910868910531, -3.889181972941495147, 6.569501556381427854 ) ) ;
#47463 = CIRCLE ( 'NONE', #18789, 6.936499999999989896 ) ;
#47464 = CARTESIAN_POINT ( 'NONE',  ( -35.00000000000000000, -6.475373545682229448, -10.32377448871674908 ) ) ;
#47465 = EDGE_CURVE ( 'NONE', #24124, #37122, #49772, .T. ) ;
#47466 = ORIENTED_EDGE ( 'NONE', *, *, #37901, .T. ) ;
#47467 = ORIENTED_EDGE ( 'NONE', *, *, #22429, .F. ) ;
#47468 = CARTESIAN_POINT ( 'NONE',  ( -35.00000000000000000, 0.000000000000000000, 0.000000000000000000 ) ) ;
#47469 = EDGE_LOOP ( 'NONE', ( #29018, #9801, #15224, #49565 ) ) ;
#47470 = CARTESIAN_POINT ( 'NONE',  ( 35.00000000000000000, -11.74614673114903596, -0.01609748574441245694 ) ) ;
#47471 = CARTESIAN_POINT ( 'NONE',  ( -28.71071236259718162, 3.670376459565066085, -11.42521152978763155 ) ) ;
#47472 = CARTESIAN_POINT ( 'NONE',  ( 37.00000000000000711, -5.300372733891562049, 11.59605747147791810 ) ) ;
#47473 = CARTESIAN_POINT ( 'NONE',  ( 0.2653141435805210224, -0.04404957080773672096, -12.24612531649368030 ) ) ;
#47474 = ORIENTED_EDGE ( 'NONE', *, *, #40593, .F. ) ;
#47475 = CARTESIAN_POINT ( 'NONE',  ( 0.3341166715381312935, 12.12403120948088109, 1.881279064087884256 ) ) ;
#47476 = LINE ( 'NONE', #51811, #4565 ) ;
#47477 = CARTESIAN_POINT ( 'NONE',  ( -29.68541646480311869, -1.416020129149132334, -13.42553116244736877 ) ) ;
#47478 = CARTESIAN_POINT ( 'NONE',  ( 8.937200413558842982, 4.476360154859214902, 12.73625532737129795 ) ) ;
#47479 = EDGE_CURVE ( 'NONE', #15336, #38388, #9404, .T. ) ;
#47480 = CARTESIAN_POINT ( 'NONE',  ( -35.00000000000000000, -9.217970097227665249, -7.971186206369574201 ) ) ;
#47481 = CARTESIAN_POINT ( 'NONE',  ( 37.00000000000000711, 4.705694406421931860E-17, -3.469127814946512892E-15 ) ) ;
#47482 = ORIENTED_EDGE ( 'NONE', *, *, #19662, .F. ) ;
#47483 = CARTESIAN_POINT ( 'NONE',  ( -15.66605021877826331, -34.92947327577397942, -5.825441821991796942 ) ) ;
#47484 = ORIENTED_EDGE ( 'NONE', *, *, #12239, .T. ) ;
#47485 = DIRECTION ( 'NONE',  ( 0.000000000000000000, 0.000000000000000000, 1.000000000000000000 ) ) ;
#47486 = DIRECTION ( 'NONE',  ( 0.000000000000000000, -0.01356324068817991828, 0.9999080150203990547 ) ) ;
#47487 = DIRECTION ( 'NONE',  ( 0.000000000000000000, -0.01356324068817998940, 0.9999080150203990547 ) ) ;
#47488 = DIRECTION ( 'NONE',  ( 0.000000000000000000, -0.2006870767258747690, 0.9796553971857770993 ) ) ;
#47489 = CARTESIAN_POINT ( 'NONE',  ( 3.459614771489464946, -11.09853614738469396, 7.685863346768216253 ) ) ;
#47490 = ADVANCED_FACE ( 'NONE', ( #39419 ), #33130, .T. ) ;
#47491 = ORIENTED_EDGE ( 'NONE', *, *, #36810, .F. ) ;
#47492 = VERTEX_POINT ( 'NONE', #44733 ) ;
#47493 = CARTESIAN_POINT ( 'NONE',  ( 0.3218525148189838592, 1.888670068297651383, 12.11874253990390038 ) ) ;
#47494 = ORIENTED_EDGE ( 'NONE', *, *, #26258, .T. ) ;
#47495 = CARTESIAN_POINT ( 'NONE',  ( -27.08423805673873019, -2.229265646063320894, 0.5302040644010340698 ) ) ;
#47496 = LINE ( 'NONE', #31530, #55557 ) ;
#47497 = DIRECTION ( 'NONE',  ( -0.3939253465568944290, 0.3052156353794439614, -0.8669868725995526493 ) ) ;
#47498 = VECTOR ( 'NONE', #4783, 1000.000000000000000 ) ;
#47499 = CYLINDRICAL_SURFACE ( 'NONE', #48197, 10.20557198542813815 ) ;
#47500 = DIRECTION ( 'NONE',  ( 1.000000000000000000, 0.000000000000000000, 0.000000000000000000 ) ) ;
#47501 = CARTESIAN_POINT ( 'NONE',  ( -22.27706485742869091, -3.662257305743835012, 0.3729136217356029959 ) ) ;
#47502 = DIRECTION ( 'NONE',  ( -1.000000000000000000, 0.000000000000000000, 0.000000000000000000 ) ) ;
#47503 = ORIENTED_EDGE ( 'NONE', *, *, #46079, .F. ) ;
#47504 = ORIENTED_EDGE ( 'NONE', *, *, #20784, .T. ) ;
#47505 = CARTESIAN_POINT ( 'NONE',  ( -20.79170840334646542, -11.34110549087206898, -3.921648409140116698 ) ) ;
#47506 = ORIENTED_EDGE ( 'NONE', *, *, #25721, .F. ) ;
#47507 = AXIS2_PLACEMENT_3D ( 'NONE', #18253, #33538, #53828 ) ;
#47508 = PRESENTATION_STYLE_ASSIGNMENT (( #27531 ) ) ;
#47509 = CARTESIAN_POINT ( 'NONE',  ( 22.19144544426022492, -12.08131399901154701, -6.034850276811086545 ) ) ;
#47510 = DIRECTION ( 'NONE',  ( 0.000000000000000000, 0.01356324068817998940, -0.9999080150203990547 ) ) ;
#47511 = AXIS2_PLACEMENT_3D ( 'NONE', #54051, #44070, #64339 ) ;
#47512 = DIRECTION ( 'NONE',  ( 1.000000000000000000, 0.000000000000000000, -0.000000000000000000 ) ) ;
#47513 = ORIENTED_EDGE ( 'NONE', *, *, #34677, .F. ) ;
#47514 = CARTESIAN_POINT ( 'NONE',  ( -36.00000000000000711, 3.640372113593720371, -12.21925492305358496 ) ) ;
#47515 = EDGE_CURVE ( 'NONE', #61407, #48793, #14760, .T. ) ;
#47516 = CARTESIAN_POINT ( 'NONE',  ( -22.59983133926798260, 2.378226455340867851, -3.996991822164138064 ) ) ;
#47517 = CARTESIAN_POINT ( 'NONE',  ( -35.04683013664716640, 0.007968230201774052085, -0.009445816769469006849 ) ) ;
#47518 = ORIENTED_EDGE ( 'NONE', *, *, #26117, .T. ) ;
#47519 = ORIENTED_EDGE ( 'NONE', *, *, #29848, .F. ) ;
#47520 = DIRECTION ( 'NONE',  ( -1.000000000000000000, -0.000000000000000000, -0.000000000000000000 ) ) ;
#47521 = ADVANCED_FACE ( 'NONE', ( #48452 ), #43422, .T. ) ;
#47522 = ORIENTED_EDGE ( 'NONE', *, *, #21882, .F. ) ;
#47523 = ORIENTED_EDGE ( 'NONE', *, *, #44011, .T. ) ;
#47524 = VERTEX_POINT ( 'NONE', #41060 ) ;
#47525 = EDGE_LOOP ( 'NONE', ( #28067, #42083, #48836, #15809 ) ) ;
#47526 = CARTESIAN_POINT ( 'NONE',  ( 0.3006302518452020345, 4.404090606399880592, 11.43947177966003537 ) ) ;
#47527 = DIRECTION ( 'NONE',  ( -1.000000000000000000, 0.000000000000000000, 0.000000000000000000 ) ) ;
#47528 = DIRECTION ( 'NONE',  ( -1.000000000000000000, 0.000000000000000000, 0.000000000000000000 ) ) ;
#47530 = EDGE_CURVE ( 'NONE', #58982, #23316, #9449, .T. ) ;
#47529 = CARTESIAN_POINT ( 'NONE',  ( 2.284126774967661255, 2.764365694977889198, -7.131638985093283090 ) ) ;
#47531 = DIRECTION ( 'NONE',  ( -1.000000000000000000, -0.000000000000000000, -0.000000000000000000 ) ) ;
#47532 = DIRECTION ( 'NONE',  ( -1.000000000000000000, 0.000000000000000000, 0.000000000000000000 ) ) ;
#47533 = ORIENTED_EDGE ( 'NONE', *, *, #54448, .F. ) ;
#47534 = CARTESIAN_POINT ( 'NONE',  ( -4.975205859172452172, -1.416020129149132778, 11.91616074890920451 ) ) ;
#47535 = CARTESIAN_POINT ( 'NONE',  ( 2.507146904658053455, 4.796593924427980049, 6.052884339496421795 ) ) ;
#47536 = DIRECTION ( 'NONE',  ( 1.000000000000000000, 0.000000000000000000, 0.000000000000000000 ) ) ;
#47537 = EDGE_CURVE ( 'NONE', #60604, #58714, #57231, .T. ) ;
#47538 = CARTESIAN_POINT ( 'NONE',  ( 0.2676618633000437675, -2.284744117040155675, 12.03196378632210362 ) ) ;
#47539 = DIRECTION ( 'NONE',  ( 1.000000000000000000, 0.000000000000000000, -0.000000000000000000 ) ) ;
#47540 = CYLINDRICAL_SURFACE ( 'NONE', #49377, 2.899999999999994582 ) ;
#47541 = AXIS2_PLACEMENT_3D ( 'NONE', #33014, #49341, #48007 ) ;
#47542 = ORIENTED_EDGE ( 'NONE', *, *, #48536, .T. ) ;
#47543 = DIRECTION ( 'NONE',  ( -1.000000000000000000, 0.000000000000000000, 0.000000000000000000 ) ) ;
#47544 = AXIS2_PLACEMENT_3D ( 'NONE', #6011, #41541, #21266 ) ;
#47545 = ORIENTED_EDGE ( 'NONE', *, *, #56412, .F. ) ;
#47546 = CARTESIAN_POINT ( 'NONE',  ( -35.00000000000000000, -6.547236723514086698, 9.752226076388870624 ) ) ;
#47547 = CARTESIAN_POINT ( 'NONE',  ( 2.241352910868910531, 5.901537464758519036, -4.843133558968066410 ) ) ;
#47548 = CARTESIAN_POINT ( 'NONE',  ( 15.74859868605385138, -29.13321728093752938, 10.87107032828077102 ) ) ;
#47549 = FACE_OUTER_BOUND ( 'NONE', #30992, .T. ) ;
#47550 = DIRECTION ( 'NONE',  ( -1.000000000000000000, 0.000000000000000000, 0.000000000000000000 ) ) ;
#47551 = ORIENTED_EDGE ( 'NONE', *, *, #32455, .F. ) ;
#47552 = CARTESIAN_POINT ( 'NONE',  ( 37.00000000000000711, -3.213188559034160452, 11.29812557209479706 ) ) ;
#47553 = DIRECTION ( 'NONE',  ( 1.000000000000000000, 0.000000000000000000, 0.000000000000000000 ) ) ;
#47554 = CARTESIAN_POINT ( 'NONE',  ( 35.00000000000000000, -6.946017217730008575, -10.01317267707884184 ) ) ;
#47555 = CIRCLE ( 'NONE', #46495, 12.18649999999999878 ) ;
#47556 = CARTESIAN_POINT ( 'NONE',  ( 0.2652384529303135619, -2.191562200667102722, -12.04846370803831235 ) ) ;
#47557 = FACE_OUTER_BOUND ( 'NONE', #6866, .T. ) ;
#47558 = ORIENTED_EDGE ( 'NONE', *, *, #51358, .F. ) ;
#47559 = CARTESIAN_POINT ( 'NONE',  ( 2.889800649504073782, -2.030191121417175726, 5.774917447012991367 ) ) ;
#47560 = CARTESIAN_POINT ( 'NONE',  ( 1.287602823387599571, -5.809161206980071768, -11.16629420487849345 ) ) ;
#47561 = B_SPLINE_CURVE_WITH_KNOTS ( 'NONE', 3,
 ( #27448, #41766, #36782, #42733, #58058, #26806, #37097 ),
 .UNSPECIFIED., .F., .F.,
 ( 4, 3, 4 ),
 ( 8.338150981378363025E-05, 9.911389841680508705E-05, 0.0001667630577588621215 ),
 .UNSPECIFIED. ) ;
#47562 = EDGE_CURVE ( 'NONE', #52191, #35667, #8382, .T. ) ;
#47563 = ORIENTED_EDGE ( 'NONE', *, *, #48375, .T. ) ;
#47564 =( BOUNDED_SURFACE ( )  B_SPLINE_SURFACE ( 3, 1, ( 
 ( #21387, #25727 ),
 ( #26704, #62267 ),
 ( #61956, #62584 ),
 ( #20740, #21735 ) ),
 .UNSPECIFIED., .F., .F., .F. ) 
 B_SPLINE_SURFACE_WITH_KNOTS ( ( 4, 4 ),
 ( 2, 2 ),
 ( 0.000000000000000000, 1.000000000000000000 ),
 ( 0.000000000000000000, 1.000000000000000000 ),
 .UNSPECIFIED. ) 
 GEOMETRIC_REPRESENTATION_ITEM ( )  RATIONAL_B_SPLINE_SURFACE ( (
 ( 1.000000000000000000, 1.000000000000000000),
 ( 0.6933888150995267674, 0.9895912004443193632),
 ( 0.6933888150995267674, 0.9895912004443193632),
 ( 1.000000000000000000, 1.000000000000000000) ) ) 
 REPRESENTATION_ITEM ( '' )  SURFACE ( )  );
#47565 = ORIENTED_EDGE ( 'NONE', *, *, #58648, .T. ) ;
#47566 = LINE ( 'NONE', #11978, #8795 ) ;
#47567 = CARTESIAN_POINT ( 'NONE',  ( 25.00000000000000355, -3.797884998337192286, 23.99999999999999289 ) ) ;
#47568 = CARTESIAN_POINT ( 'NONE',  ( 0.6473888112830271657, -7.698027285532536013, 9.687359867659774082 ) ) ;
#47569 = LINE ( 'NONE', #15977, #62593 ) ;
#47570 = VERTEX_POINT ( 'NONE', #9817 ) ;
#47571 = EDGE_LOOP ( 'NONE', ( #46678, #34027, #34439, #47042 ) ) ;
#47572 = VERTEX_POINT ( 'NONE', #5854 ) ;
#47573 = CARTESIAN_POINT ( 'NONE',  ( 2.963017218115628459, 7.865565884553440412, 0.3847317984105586564 ) ) ;
#47574 = AXIS2_PLACEMENT_3D ( 'NONE', #33758, #13169, #65001 ) ;
#47575 = DIRECTION ( 'NONE',  ( 1.000000000000000000, 0.000000000000000000, 0.000000000000000000 ) ) ;
#47576 = ADVANCED_FACE ( 'NONE', ( #836 ), #30432, .T. ) ;
#47577 = ORIENTED_EDGE ( 'NONE', *, *, #51967, .T. ) ;
#47578 = CARTESIAN_POINT ( 'NONE',  ( -35.00000000000000000, -5.273331777780412288, 10.49591321039678959 ) ) ;
#47579 = CARTESIAN_POINT ( 'NONE',  ( 2.251139882113957658, -7.542197031254636030, 1.203816215709523796 ) ) ;
#47581 = ORIENTED_EDGE ( 'NONE', *, *, #44829, .T. ) ;
#47580 = CIRCLE ( 'NONE', #23138, 5.000000000000001776 ) ;
#47582 = CYLINDRICAL_SURFACE ( 'NONE', #29040, 5.000000000000001776 ) ;
#47583 =( BOUNDED_SURFACE ( )  B_SPLINE_SURFACE ( 3, 1, ( 
 ( #43021, #63295 ),
 ( #34667, #30915 ),
 ( #61190, #49664 ),
 ( #15937, #35889 ) ),
 .UNSPECIFIED., .F., .F., .F. ) 
 B_SPLINE_SURFACE_WITH_KNOTS ( ( 4, 4 ),
 ( 2, 2 ),
 ( 0.000000000000000000, 1.000000000000000000 ),
 ( 0.000000000000000000, 1.000000000000000000 ),
 .UNSPECIFIED. ) 
 GEOMETRIC_REPRESENTATION_ITEM ( )  RATIONAL_B_SPLINE_SURFACE ( (
 ( 1.000000000000000000, 1.000000000000000000),
 ( 0.9942764183789327692, 0.8450855930916585379),
 ( 0.9942764183789327692, 0.8450855930916585379),
 ( 1.000000000000000000, 1.000000000000000000) ) ) 
 REPRESENTATION_ITEM ( '' )  SURFACE ( )  );
#47584 = ADVANCED_FACE ( 'NONE', ( #60050 ), #46076, .T. ) ;
#47585 = CARTESIAN_POINT ( 'NONE',  ( 9.730232070128620236, -27.62176360438186506, -14.46115055101679125 ) ) ;
#47586 = CARTESIAN_POINT ( 'NONE',  ( 23.47346277817274185, -4.308697950774896590, 11.20435082111871417 ) ) ;
#47587 = EDGE_LOOP ( 'NONE', ( #33044, #45, #733, #21696 ) ) ;
#47588 = ORIENTED_EDGE ( 'NONE', *, *, #21566, .T. ) ;
#47589 = AXIS2_PLACEMENT_3D ( 'NONE', #52363, #6149, #42025 ) ;
#47590 = CARTESIAN_POINT ( 'NONE',  ( 3.152665057734040488, 0.000000000000000000, 0.000000000000000000 ) ) ;
#47591 = EDGE_CURVE ( 'NONE', #17671, #45297, #25126, .T. ) ;
#47592 = ORIENTED_EDGE ( 'NONE', *, *, #45680, .T. ) ;
#47593 = CYLINDRICAL_SURFACE ( 'NONE', #31711, 2.899999999999994582 ) ;
#47594 = VECTOR ( 'NONE', #36315, 1000.000000000000000 ) ;
#47595 = CARTESIAN_POINT ( 'NONE',  ( -19.69476066079020171, -4.201994156881551312, 12.82938989607585789 ) ) ;
#47596 = CARTESIAN_POINT ( 'NONE',  ( -19.55198024779261701, -3.902068674853255814, 11.34897822738861528 ) ) ;
#47597 = DIRECTION ( 'NONE',  ( 0.000000000000000000, 0.000000000000000000, -1.000000000000000000 ) ) ;
#47598 = CARTESIAN_POINT ( 'NONE',  ( 0.2648978790185602672, 0.1321385342562404197, 12.24533305150758089 ) ) ;
#47600 = EDGE_CURVE ( 'NONE', #16758, #47785, #40218, .T. ) ;
#47599 = DIRECTION ( 'NONE',  ( 0.000000000000000000, 0.01356324068817998940, -0.9999080150203990547 ) ) ;
#47601 = CARTESIAN_POINT ( 'NONE',  ( 5.514970785353741078, -0.0003039746380528647075, -0.004713149585127535644 ) ) ;
#47602 = CYLINDRICAL_SURFACE ( 'NONE', #49102, 12.18650000000000055 ) ;
#47603 = ORIENTED_EDGE ( 'NONE', *, *, #28990, .F. ) ;
#47604 = FACE_OUTER_BOUND ( 'NONE', #30350, .T. ) ;
#47605 = ORIENTED_EDGE ( 'NONE', *, *, #38376, .F. ) ;
#47606 = DIRECTION ( 'NONE',  ( 0.000000000000000000, -0.01356324068817999114, 0.9999080150203989437 ) ) ;
#47607 = ADVANCED_FACE ( 'NONE', ( #45081 ), #39758, .T. ) ;
#47608 = DIRECTION ( 'NONE',  ( -1.000000000000000000, 0.000000000000000000, 0.000000000000000000 ) ) ;
#47609 = ORIENTED_EDGE ( 'NONE', *, *, #13570, .T. ) ;
#47610 = FACE_OUTER_BOUND ( 'NONE', #9815, .T. ) ;
#47611 = CARTESIAN_POINT ( 'NONE',  ( -27.27855387000350262, 12.26939275170278343, 5.631341004100471892 ) ) ;
#47612 = CYLINDRICAL_SURFACE ( 'NONE', #43978, 4.999999999999999112 ) ;
#47613 = ORIENTED_EDGE ( 'NONE', *, *, #43442, .T. ) ;
#47614 = ORIENTED_EDGE ( 'NONE', *, *, #26966, .T. ) ;
#47615 = FACE_OUTER_BOUND ( 'NONE', #61230, .T. ) ;
#47616 = EDGE_CURVE ( 'NONE', #40241, #8833, #2021, .T. ) ;
#47617 = AXIS2_PLACEMENT_3D ( 'NONE', #22154, #7184, #16838 ) ;
#47618 = ORIENTED_EDGE ( 'NONE', *, *, #2018, .T. ) ;
#47619 = DIRECTION ( 'NONE',  ( 0.000000000000000000, -0.01356324068817998940, 0.9999080150203990547 ) ) ;
#47620 = DIRECTION ( 'NONE',  ( -1.000000000000000000, 0.000000000000000000, 0.000000000000000000 ) ) ;
#47621 = CARTESIAN_POINT ( 'NONE',  ( -27.05874794189610455, 0.3907329275428126913, 2.180117559290193796 ) ) ;
#47622 = CYLINDRICAL_SURFACE ( 'NONE', #51237, 2.899999999999994582 ) ;
#47623 = ORIENTED_EDGE ( 'NONE', *, *, #53102, .F. ) ;
#47624 = CYLINDRICAL_SURFACE ( 'NONE', #63466, 12.75000000000000178 ) ;
#47625 = CIRCLE ( 'NONE', #18964, 7.938172270156617749 ) ;
#47626 = CIRCLE ( 'NONE', #18966, 12.18650000000000055 ) ;
#47627 = CARTESIAN_POINT ( 'NONE',  ( 37.00000000000000711, 4.705694406421931860E-17, -3.469127814946512892E-15 ) ) ;
#47628 = DIRECTION ( 'NONE',  ( -1.000000000000000000, 0.000000000000000000, 0.000000000000000000 ) ) ;
#47629 = CARTESIAN_POINT ( 'NONE',  ( 2.903928887688517424, -2.496183838365630514, 8.407112942776095110 ) ) ;
#47631 = AXIS2_PLACEMENT_3D ( 'NONE', #49585, #4024, #24292 ) ;
#47630 = CARTESIAN_POINT ( 'NONE',  ( 0.2648978790185584908, 12.03635331166812250, 2.256510822326184940 ) ) ;
#47632 = CARTESIAN_POINT ( 'NONE',  ( -37.00000000000000711, 0.000000000000000000, 0.000000000000000000 ) ) ;
#47633 = CYLINDRICAL_SURFACE ( 'NONE', #26153, 12.18650000000000055 ) ;
#47634 = CARTESIAN_POINT ( 'NONE',  ( -22.27706089016750468, -2.583072118615362012, -2.622757446538691806 ) ) ;
#47635 = EDGE_CURVE ( 'NONE', #29113, #25350, #50413, .T. ) ;
#47636 = ORIENTED_EDGE ( 'NONE', *, *, #11944, .T. ) ;
#47637 = CARTESIAN_POINT ( 'NONE',  ( 35.00000000000000000, 10.14433819232443490, 6.753013023069603271 ) ) ;
#47638 = CARTESIAN_POINT ( 'NONE',  ( 35.00000000000000000, 4.237174932027400587, 12.02534193257715600 ) ) ;
#47639 = VERTEX_POINT ( 'NONE', #60701 ) ;
#47640 = EDGE_CURVE ( 'NONE', #52961, #19077, #15133, .T. ) ;
#47641 = CARTESIAN_POINT ( 'NONE',  ( 2.000000000000001776, 0.000000000000000000, 0.000000000000000000 ) ) ;
#47642 = CARTESIAN_POINT ( 'NONE',  ( 0.3675815128205912052, -9.235491948679950269, -8.093875121226169256 ) ) ;
#47643 = ORIENTED_EDGE ( 'NONE', *, *, #19213, .F. ) ;
#47644 = DIRECTION ( 'NONE',  ( -1.000000000000000000, 0.000000000000000000, 0.000000000000000000 ) ) ;
#47645 = ORIENTED_EDGE ( 'NONE', *, *, #15248, .F. ) ;
#47646 = EDGE_CURVE ( 'NONE', #50397, #56080, #13685, .T. ) ;
#47647 = CARTESIAN_POINT ( 'NONE',  ( 0.3654063281920725270, -5.910280591919130799, 10.76363796011283469 ) ) ;
#47648 = VERTEX_POINT ( 'NONE', #188 ) ;
#47649 = ORIENTED_EDGE ( 'NONE', *, *, #25734, .F. ) ;
#47650 = DIRECTION ( 'NONE',  ( 0.000000000000000000, -0.01356324068818000328, 0.9999080150203990547 ) ) ;
#47651 = AXIS2_PLACEMENT_3D ( 'NONE', #7716, #1749, #6405 ) ;
#47652 = EDGE_CURVE ( 'NONE', #55512, #9384, #41308, .T. ) ;
#47653 = ORIENTED_EDGE ( 'NONE', *, *, #47148, .T. ) ;
#47654 = DIRECTION ( 'NONE',  ( -1.000000000000000000, 0.000000000000000000, 0.000000000000000000 ) ) ;
#47655 = CARTESIAN_POINT ( 'NONE',  ( 0.9963060071168140519, 0.1253731440146732823, 13.50289960222859875 ) ) ;
#47656 = CARTESIAN_POINT ( 'NONE',  ( 145.1370849898475797, 3.309064568108273190E-14, 0.000000000000000000 ) ) ;
#47657 = CARTESIAN_POINT ( 'NONE',  ( 1.104777566491144114, -0.4777483965052850556, -12.51694124543052133 ) ) ;
#47658 = ORIENTED_EDGE ( 'NONE', *, *, #10166, .F. ) ;
#47659 = CARTESIAN_POINT ( 'NONE',  ( 0.2915757698887281313, -7.711631695122908248, 9.524403232224839755 ) ) ;
#47660 = VECTOR ( 'NONE', #33376, 1000.000000000000000 ) ;
#47661 = ADVANCED_FACE ( 'NONE', ( #10803 ), #46391, .T. ) ;
#47662 = CARTESIAN_POINT ( 'NONE',  ( 10.51584247049436449, -29.12274881419789807, 8.353506175201449224 ) ) ;
#47663 = DIRECTION ( 'NONE',  ( 0.000000000000000000, -0.1081190184239280011, -0.9941379571543611515 ) ) ;
#47665 = ORIENTED_EDGE ( 'NONE', *, *, #28396, .T. ) ;
#47664 = CARTESIAN_POINT ( 'NONE',  ( -24.33622492195127407, 7.892808082209504583, 9.041745503709938347 ) ) ;
#47666 = DIRECTION ( 'NONE',  ( 0.000000000000000000, 0.000000000000000000, 1.000000000000000000 ) ) ;
#47667 = EDGE_CURVE ( 'NONE', #33621, #59239, #50075, .T. ) ;
#47668 = ORIENTED_EDGE ( 'NONE', *, *, #28571, .F. ) ;
#47669 = CARTESIAN_POINT ( 'NONE',  ( 5.514624014163232779, -0.001255375129358104504, -0.003946330869974997921 ) ) ;
#47670 = ORIENTED_EDGE ( 'NONE', *, *, #19231, .F. ) ;
#47671 = CARTESIAN_POINT ( 'NONE',  ( 35.00000000000000000, -0.4993900848168272288, -12.17626345777663488 ) ) ;
#47672 = CARTESIAN_POINT ( 'NONE',  ( 2.241526690369557429, -4.920579984890920855, -5.837196604699895985 ) ) ;
#47673 = AXIS2_PLACEMENT_3D ( 'NONE', #40190, #34557, #55169 ) ;
#47674 = CARTESIAN_POINT ( 'NONE',  ( 2.241311220309554209, -7.633829235838274663, -0.09281826062103946950 ) ) ;
#47675 = EDGE_LOOP ( 'NONE', ( #13055, #16222, #53384, #43824 ) ) ;
#47676 = CYLINDRICAL_SURFACE ( 'NONE', #2825, 12.74999999999999822 ) ;
#47677 = CARTESIAN_POINT ( 'NONE',  ( -35.04643116707788408, 0.01135624435143721411, 0.004425962698848331933 ) ) ;
#47678 = CARTESIAN_POINT ( 'NONE',  ( 13.11132293240999758, 11.59456066430334609, -6.918089050757264324 ) ) ;
#47679 = ORIENTED_EDGE ( 'NONE', *, *, #42349, .F. ) ;
#47680 = VECTOR ( 'NONE', #37316, 1000.000000000000000 ) ;
#47681 = EDGE_LOOP ( 'NONE', ( #37469, #50498, #3683, #8363 ) ) ;
#47682 = CARTESIAN_POINT ( 'NONE',  ( 2.994568964204206818, 7.686291764591511644, 1.761139509856855856 ) ) ;
#47683 = ORIENTED_EDGE ( 'NONE', *, *, #57411, .T. ) ;
#47684 = EDGE_CURVE ( 'NONE', #9977, #41254, #25373, .T. ) ;
#47685 = AXIS2_PLACEMENT_3D ( 'NONE', #45152, #30499, #25514 ) ;
#47686 = ADVANCED_FACE ( 'NONE', ( #47058 ), #21448, .T. ) ;
#47687 = ORIENTED_EDGE ( 'NONE', *, *, #1987, .T. ) ;
#47688 = LINE ( 'NONE', #33032, #37012 ) ;
#47689 = CARTESIAN_POINT ( 'NONE',  ( -18.49080574448680991, -12.00000000000057909, -4.407108900774715188E-13 ) ) ;
#47690 = DIRECTION ( 'NONE',  ( 0.000000000000000000, 0.000000000000000000, -1.000000000000000000 ) ) ;
#47691 = CARTESIAN_POINT ( 'NONE',  ( -47.00000000000000711, 0.000000000000000000, 0.000000000000000000 ) ) ;
#47692 = ADVANCED_FACE ( 'NONE', ( #62324 ), #8742, .F. ) ;
#47693 = DIRECTION ( 'NONE',  ( 0.000000000000000000, 0.4134677391718512562, 0.9105187689795954942 ) ) ;
#47694 = CARTESIAN_POINT ( 'NONE',  ( 5.520433897694421610, 0.003119431460922221164, -0.01473594271720233932 ) ) ;
#47695 = ADVANCED_FACE ( 'NONE', ( #36738 ), #57031, .F. ) ;
#47696 = CARTESIAN_POINT ( 'NONE',  ( 2.941278708680199916, 4.788765081995683737, -3.842273877444514429 ) ) ;
#47697 = ADVANCED_FACE ( 'NONE', ( #37381 ), #21103, .F. ) ;
#47698 = ORIENTED_EDGE ( 'NONE', *, *, #24835, .T. ) ;
#47699 = EDGE_CURVE ( 'NONE', #23038, #54088, #11776, .T. ) ;
#47700 = CYLINDRICAL_SURFACE ( 'NONE', #20723, 2.899999999999994582 ) ;
#47701 = CARTESIAN_POINT ( 'NONE',  ( -37.00000000000000711, -7.817610399097453922, -8.766823244862070652 ) ) ;
#47702 = CARTESIAN_POINT ( 'NONE',  ( -22.27834755396594346, 0.7418417409069284485, 3.610802913011835980 ) ) ;
#47703 = DIRECTION ( 'NONE',  ( 0.000000000000000000, 0.01356324068817991828, -0.9999080150203990547 ) ) ;
#47704 = AXIS2_PLACEMENT_3D ( 'NONE', #20557, #45478, #14245 ) ;
#47705 = FACE_OUTER_BOUND ( 'NONE', #3784, .T. ) ;
#47706 = AXIS2_PLACEMENT_3D ( 'NONE', #56619, #61917, #1740 ) ;
#47707 = CARTESIAN_POINT ( 'NONE',  ( 0.2653141617321017609, 12.06772699408311489, -2.083144498805149514 ) ) ;
#47708 = CARTESIAN_POINT ( 'NONE',  ( 10.27842187895016224, 1.477547723869735874, -11.90968538141293998 ) ) ;
#47709 = ORIENTED_EDGE ( 'NONE', *, *, #58350, .F. ) ;
#47710 = CARTESIAN_POINT ( 'NONE',  ( -35.00000000000000000, 0.000000000000000000, 0.000000000000000000 ) ) ;
#47711 = CARTESIAN_POINT ( 'NONE',  ( 0.3002738374340833682, -1.906042098268937446, -12.10874171309341563 ) ) ;
#47712 = CARTESIAN_POINT ( 'NONE',  ( 47.00000000000000711, 4.705694406421931860E-17, -3.469127814946512892E-15 ) ) ;
#47713 = CARTESIAN_POINT ( 'NONE',  ( 2.524535260913002510, -1.559291270914674232, -7.569872524929103008 ) ) ;
#47714 = AXIS2_PLACEMENT_3D ( 'NONE', #20157, #56389, #40429 ) ;
#47715 = EDGE_CURVE ( 'NONE', #46658, #24785, #52038, .T. ) ;
#47716 = CARTESIAN_POINT ( 'NONE',  ( 2.000000000000001776, 0.000000000000000000, 0.000000000000000000 ) ) ;
#47717 = CYLINDRICAL_SURFACE ( 'NONE', #58537, 12.75000000000000178 ) ;
#47718 = VECTOR ( 'NONE', #31205, 1000.000000000000000 ) ;
#47719 = ORIENTED_EDGE ( 'NONE', *, *, #65343, .T. ) ;
#47720 = DIRECTION ( 'NONE',  ( 1.000000000000000000, 0.000000000000000000, 0.000000000000000000 ) ) ;
#47721 = FACE_OUTER_BOUND ( 'NONE', #62619, .T. ) ;
#47722 = CARTESIAN_POINT ( 'NONE',  ( 0.2706063244538063350, 9.268878137104398007, 8.006269958070639348 ) ) ;
#47723 = CARTESIAN_POINT ( 'NONE',  ( -22.30625920655495165, -0.8854385781085337692, 3.687109008463850479 ) ) ;
#47724 = ORIENTED_EDGE ( 'NONE', *, *, #29507, .F. ) ;
#47725 = CARTESIAN_POINT ( 'NONE',  ( 0.3675815128205894289, -3.951233083390547129, 11.62724744438064306 ) ) ;
#47726 = CARTESIAN_POINT ( 'NONE',  ( 5.514970785353741078, 0.002093325033904021564, 0.004233694591582523939 ) ) ;
#47727 = VERTEX_POINT ( 'NONE', #1826 ) ;
#47728 = EDGE_CURVE ( 'NONE', #35944, #47492, #54288, .T. ) ;
#47729 = AXIS2_PLACEMENT_3D ( 'NONE', #51324, #46323, #56960 ) ;
#47730 = ORIENTED_EDGE ( 'NONE', *, *, #2808, .T. ) ;
#47731 = CARTESIAN_POINT ( 'NONE',  ( -4.989057617119011745, -0.9162120371760335003, -11.96497202265568660 ) ) ;
#47732 = DIRECTION ( 'NONE',  ( 1.000000000000000000, 0.000000000000000000, -0.000000000000000000 ) ) ;
#47733 = ORIENTED_EDGE ( 'NONE', *, *, #21091, .T. ) ;
#47734 = CIRCLE ( 'NONE', #56218, 1.499999999999997780 ) ;
#47735 = CARTESIAN_POINT ( 'NONE',  ( 0.2706063244538005619, -9.494160524941746004, 7.737788863017279972 ) ) ;
#47736 = B_SPLINE_CURVE_WITH_KNOTS ( 'NONE', 3,
 ( #51223, #42504, #21929, #11294, #51866, #15930, #61827, #15611, #52536, #41534, #6965, #35877, #27235, #36215, #36565, #47529, #5673, #56523, #25943 ),
 .UNSPECIFIED., .F., .F.,
 ( 4, 3, 3, 3, 3, 3, 4 ),
 ( 4.336808689942017736E-19, 2.831840207499626523E-05, 4.217266859840494790E-05, 5.602024318396020829E-05, 6.290810167969150990E-05, 9.120440630945391260E-05, 0.0001153103026479759813 ),
 .UNSPECIFIED. ) ;
#47737 = DIRECTION ( 'NONE',  ( 0.000000000000000000, -0.01356324068817998940, 0.9999080150203990547 ) ) ;
#47738 = CARTESIAN_POINT ( 'NONE',  ( 0.000000000000000000, 0.000000000000000000, 0.000000000000000000 ) ) ;
#47739 = CARTESIAN_POINT ( 'NONE',  ( -2.952869152607111136, -7.581333670610126418, 11.17020052527586138 ) ) ;
#47740 = CARTESIAN_POINT ( 'NONE',  ( 26.34661844826604593, 13.08594712317291986, 3.317828791472332117 ) ) ;
#47742 = ORIENTED_EDGE ( 'NONE', *, *, #51177, .F. ) ;
#47741 = LINE ( 'NONE', #53051, #25490 ) ;
#47743 = DIRECTION ( 'NONE',  ( 0.000000000000000000, 0.000000000000000000, 1.000000000000000000 ) ) ;
#47744 = EDGE_CURVE ( 'NONE', #39914, #14488, #46639, .T. ) ;
#47745 = ORIENTED_EDGE ( 'NONE', *, *, #30914, .F. ) ;
#47746 = CARTESIAN_POINT ( 'NONE',  ( -37.00000000000000711, 9.390600770287994337, 8.624332853796092380 ) ) ;
#47747 = EDGE_LOOP ( 'NONE', ( #33611, #46252, #14426, #58804 ) ) ;
#47748 = ORIENTED_EDGE ( 'NONE', *, *, #44600, .T. ) ;
#47749 = APPLICATION_PROTOCOL_DEFINITION ( 'draft international standard', 'automotive_design', 1998, #12786 ) ;
#47750 = CARTESIAN_POINT ( 'NONE',  ( 0.3675815128205912052, -11.44679196252412368, 4.447030445008141264 ) ) ;
#47751 = CARTESIAN_POINT ( 'NONE',  ( -18.19295774167957092, -29.77901320112238892, 7.993354913176278664 ) ) ;
#47752 = CARTESIAN_POINT ( 'NONE',  ( 3.152665057733966769, 0.9030954876739563097, 7.886634106564108571 ) ) ;
#47753 = CIRCLE ( 'NONE', #32872, 5.000000000000000000 ) ;
#47754 = CARTESIAN_POINT ( 'NONE',  ( -45.37278721346743282, -0.8995687559121183785, -12.71067884230443923 ) ) ;
#47755 = CARTESIAN_POINT ( 'NONE',  ( 22.78386511336923093, 3.290201280387628824, 13.09362067330721757 ) ) ;
#47756 = ORIENTED_EDGE ( 'NONE', *, *, #26475, .F. ) ;
#47757 = CARTESIAN_POINT ( 'NONE',  ( -24.31546255402668422, -8.695390788176707630, 8.272891244190285320 ) ) ;
#47758 = CIRCLE ( 'NONE', #59427, 12.75000000000000178 ) ;
#47759 = CARTESIAN_POINT ( 'NONE',  ( 1.719304012338836563, -3.626341562670527985, 12.20344780066003487 ) ) ;
#47760 = ORIENTED_EDGE ( 'NONE', *, *, #33076, .F. ) ;
#47761 = VERTEX_POINT ( 'NONE', #22417 ) ;
#47762 = CARTESIAN_POINT ( 'NONE',  ( -37.00000000000000711, -9.430788938294107027, 7.718225330433774900 ) ) ;
#47763 = EDGE_LOOP ( 'NONE', ( #41248, #46190, #64848, #38144 ) ) ;
#47764 = CARTESIAN_POINT ( 'NONE',  ( -37.00000000000000711, 0.000000000000000000, 0.000000000000000000 ) ) ;
#47765 = CARTESIAN_POINT ( 'NONE',  ( 5.515539859299206427, 0.005751553894234952106, -0.001886660928063908999 ) ) ;
#47766 = CARTESIAN_POINT ( 'NONE',  ( 8.937200413558842982, 4.476360154859214902, 12.73625532737129795 ) ) ;
#47767 = ADVANCED_FACE ( 'NONE', ( #62985 ), #12427, .T. ) ;
#47769 = VECTOR ( 'NONE', #8011, 1000.000000000000000 ) ;
#47768 = CARTESIAN_POINT ( 'NONE',  ( 1.719304012338199295, 12.64775761152512423, 1.452142814150486183 ) ) ;
#47770 = DIRECTION ( 'NONE',  ( 0.000000000000000000, 0.5243256840888563808, 0.8515178078024867592 ) ) ;
#47771 = CARTESIAN_POINT ( 'NONE',  ( -27.09729107899852352, -1.932259710108171324, 1.302895495071016985 ) ) ;
#47772 = EDGE_CURVE ( 'NONE', #29225, #51071, #7318, .T. ) ;
#47773 = CARTESIAN_POINT ( 'NONE',  ( 2.262775599886257538, 7.499645832851604688, 1.465770593192917470 ) ) ;
#47774 = CIRCLE ( 'NONE', #4244, 2.899999999999995914 ) ;
#47775 = ORIENTED_EDGE ( 'NONE', *, *, #34808, .T. ) ;
#47776 =( BOUNDED_CURVE ( )  B_SPLINE_CURVE ( 3, ( #49016, #18750, #39007, #13726 ),
 .UNSPECIFIED., .F., .F. ) 
 B_SPLINE_CURVE_WITH_KNOTS ( ( 4, 4 ),
 ( 4.607305308089706841, 4.644469214066985430 ),
 .UNSPECIFIED. ) 
 CURVE ( )  GEOMETRIC_REPRESENTATION_ITEM ( )  RATIONAL_B_SPLINE_CURVE ( ( 1.000000000000000000, 0.9998849069861288630, 0.9998849069861288630, 1.000000000000000000 ) ) 
 REPRESENTATION_ITEM ( '' )  );
#47777 = ORIENTED_EDGE ( 'NONE', *, *, #9405, .F. ) ;
#47778 = EDGE_CURVE ( 'NONE', #13458, #20614, #44847, .T. ) ;
#47779 = CARTESIAN_POINT ( 'NONE',  ( 0.2650492594609251684, -6.218173512054836927, 10.54996119777443297 ) ) ;
#47780 = CARTESIAN_POINT ( 'NONE',  ( -9.183025528901289647, -11.31491075083350495, -7.371853674845621818 ) ) ;
#47781 = CARTESIAN_POINT ( 'NONE',  ( 2.589278595513088366, -2.875840518181322913, -7.197074516942284284 ) ) ;
#47782 = AXIS2_PLACEMENT_3D ( 'NONE', #978, #11281, #36199 ) ;
#47783 = CARTESIAN_POINT ( 'NONE',  ( -37.00000000000000711, -4.946702696913093611, -11.13736569743279681 ) ) ;
#47784 = ORIENTED_EDGE ( 'NONE', *, *, #38674, .F. ) ;
#47785 = VERTEX_POINT ( 'NONE', #7799 ) ;
#47786 = DIRECTION ( 'NONE',  ( 1.000000000000000000, 0.000000000000000000, 0.000000000000000000 ) ) ;
#47787 = ORIENTED_EDGE ( 'NONE', *, *, #26628, .T. ) ;
#47788 = CARTESIAN_POINT ( 'NONE',  ( 0.2872850955227761460, 7.715220952083361006, -9.519656861923639468 ) ) ;
#47789 = LINE ( 'NONE', #63077, #42017 ) ;
#47790 = DIRECTION ( 'NONE',  ( 0.000000000000000000, 0.01356324068817991828, -0.9999080150203990547 ) ) ;
#47791 = CARTESIAN_POINT ( 'NONE',  ( 2.305787727787083519, 1.493241775258524084, -7.508843116234142911 ) ) ;
#47792 = ORIENTED_EDGE ( 'NONE', *, *, #47460, .T. ) ;
#47793 = CARTESIAN_POINT ( 'NONE',  ( 0.3164563675027646794, 12.11636128244742672, 1.892265234253155182 ) ) ;
#47794 = DIRECTION ( 'NONE',  ( 0.000000000000000000, -0.1118654143051685396, -0.9937233664769753450 ) ) ;
#47795 = CARTESIAN_POINT ( 'NONE',  ( -35.00000000000000000, -12.74068829017553384, -0.4871980014162800021 ) ) ;
#47796 = CARTESIAN_POINT ( 'NONE',  ( -36.06679944573490104, -2.440416481716451091, 22.47657575504853256 ) ) ;
#47797 = AXIS2_PLACEMENT_3D ( 'NONE', #6677, #56559, #26948 ) ;
#47798 = EDGE_CURVE ( 'NONE', #3402, #53501, #29624, .T. ) ;
#47799 = AXIS2_PLACEMENT_3D ( 'NONE', #11861, #48124, #37128 ) ;
#47800 = DIRECTION ( 'NONE',  ( 0.000000000000000000, -0.4935949184179134752, 0.8696919319575254770 ) ) ;
#47801 = EDGE_CURVE ( 'NONE', #54960, #50930, #15807, .T. ) ;
#47802 = DIRECTION ( 'NONE',  ( 0.000000000000000000, -0.1081190184239279733, -0.9941379571543611515 ) ) ;
#47803 = VERTEX_POINT ( 'NONE', #39025 ) ;
#47804 = EDGE_LOOP ( 'NONE', ( #42651, #26113, #2281, #60487 ) ) ;
#47805 = DIRECTION ( 'NONE',  ( 1.000000000000000000, -0.000000000000000000, 0.000000000000000000 ) ) ;
#47806 = CARTESIAN_POINT ( 'NONE',  ( 18.84867683979356201, -5.944105725974474730, 12.12095735156416509 ) ) ;
#47807 = CARTESIAN_POINT ( 'NONE',  ( 35.00000000000000000, 4.705694406421931860E-17, -3.469127814946512892E-15 ) ) ;
#47808 = EDGE_CURVE ( 'NONE', #54991, #44256, #61484, .T. ) ;
#47809 = CARTESIAN_POINT ( 'NONE',  ( 37.00000000000000711, -8.146229107149464355, -9.063649021438928699 ) ) ;
#47810 = CARTESIAN_POINT ( 'NONE',  ( 0.2717059086739033180, -11.44824199474646420, 4.354191483751232106 ) ) ;
#47811 = ORIENTED_EDGE ( 'NONE', *, *, #26966, .F. ) ;
#47812 = ORIENTED_EDGE ( 'NONE', *, *, #32203, .F. ) ;
#47813 = FACE_OUTER_BOUND ( 'NONE', #2577, .T. ) ;
#47814 = EDGE_LOOP ( 'NONE', ( #62788, #53184, #64098, #26221 ) ) ;
#47815 = CARTESIAN_POINT ( 'NONE',  ( -1.734723475976807094E-15, -3.469446951953614189E-15, 12.00000000000000178 ) ) ;
#47816 = FACE_OUTER_BOUND ( 'NONE', #16390, .T. ) ;
#47817 = DIRECTION ( 'NONE',  ( 0.000000000000000000, 0.01356324068817992175, -0.9999080150203990547 ) ) ;
#47818 = CARTESIAN_POINT ( 'NONE',  ( 0.7400311444011756778, 3.907401494355078331, -11.77295732453929844 ) ) ;
#47819 = DIRECTION ( 'NONE',  ( 0.000000000000000000, -0.01356324068817992522, 0.9999080150203990547 ) ) ;
#47820 = CARTESIAN_POINT ( 'NONE',  ( 2.269879328256732443, 7.552124491910172210, 1.181008584585979682 ) ) ;
#47821 = DIRECTION ( 'NONE',  ( 0.000000000000000000, 0.8835120444460207167, 0.4684084406997939265 ) ) ;
#47822 = ORIENTED_EDGE ( 'NONE', *, *, #17408, .F. ) ;
#47823 = EDGE_CURVE ( 'NONE', #31374, #57610, #43684, .T. ) ;
#47824 = ADVANCED_FACE ( 'NONE', ( #2831 ), #49034, .T. ) ;
#47825 = ORIENTED_EDGE ( 'NONE', *, *, #60566, .F. ) ;
#47826 = CARTESIAN_POINT ( 'NONE',  ( 2.000000000000001776, -5.107597897712309098, -4.693343793638478978 ) ) ;
#47827 = AXIS2_PLACEMENT_3D ( 'NONE', #26481, #46769, #36793 ) ;
#47828 = ORIENTED_EDGE ( 'NONE', *, *, #11464, .T. ) ;
#47829 = FILL_AREA_STYLE ('',( #32189 ) ) ;
#47830 = EDGE_CURVE ( 'NONE', #27180, #19660, #33390, .T. ) ;
#47831 = CARTESIAN_POINT ( 'NONE',  ( 21.44386431903875234, -13.23489694407720663, -2.693023235911562452 ) ) ;
#47832 = CARTESIAN_POINT ( 'NONE',  ( 17.22995070708839904, 10.79921756342612404, 8.109772993617433201 ) ) ;
#47833 = CARTESIAN_POINT ( 'NONE',  ( -22.27706485742869091, -1.508175983031604606, 3.358064672837097753 ) ) ;
#47834 = VERTEX_POINT ( 'NONE', #14077 ) ;
#47836 = DIRECTION ( 'NONE',  ( 0.8914382917301157949, 0.000000000000000000, -0.4531421102008653112 ) ) ;
#47835 = AXIS2_PLACEMENT_3D ( 'NONE', #28058, #2806, #23068 ) ;
#47837 = CYLINDRICAL_SURFACE ( 'NONE', #29676, 12.74999999999999822 ) ;
#47838 = LINE ( 'NONE', #53817, #4255 ) ;
#47839 = ORIENTED_EDGE ( 'NONE', *, *, #56783, .T. ) ;
#47840 = ORIENTED_EDGE ( 'NONE', *, *, #53422, .F. ) ;
#47841 = DIRECTION ( 'NONE',  ( -1.000000000000000000, -0.000000000000000000, -0.000000000000000000 ) ) ;
#47842 = VECTOR ( 'NONE', #17149, 999.9999999999998863 ) ;
#47843 = ORIENTED_EDGE ( 'NONE', *, *, #64670, .T. ) ;
#47844 = ORIENTED_EDGE ( 'NONE', *, *, #41479, .F. ) ;
#47845 = CARTESIAN_POINT ( 'NONE',  ( 35.00000000000000000, -11.29812557209478996, -3.213188559034203529 ) ) ;
#47846 = ORIENTED_EDGE ( 'NONE', *, *, #15300, .F. ) ;
#47847 = ORIENTED_EDGE ( 'NONE', *, *, #57282, .T. ) ;
#47848 = DIRECTION ( 'NONE',  ( 1.000000000000000000, 0.000000000000000000, 0.000000000000000000 ) ) ;
#47849 = ADVANCED_FACE ( 'NONE', ( #18452 ), #40580, .F. ) ;
#47850 = CARTESIAN_POINT ( 'NONE',  ( 2.000000000000001776, 4.976357229393855164, 4.652926418895560801 ) ) ;
#47851 = CIRCLE ( 'NONE', #7477, 12.18649999999999878 ) ;
#47853 = VECTOR ( 'NONE', #5023, 1000.000000000000000 ) ;
#47852 = CYLINDRICAL_SURFACE ( 'NONE', #32014, 6.936499999999988120 ) ;
#47854 = DIRECTION ( 'NONE',  ( 0.000000000000000000, -0.01356324068817991828, 0.9999080150203990547 ) ) ;
#47855 = FACE_OUTER_BOUND ( 'NONE', #8250, .T. ) ;
#47856 = VECTOR ( 'NONE', #59844, 1000.000000000000000 ) ;
#47857 = EDGE_CURVE ( 'NONE', #60345, #44318, #987, .T. ) ;
#47858 = CARTESIAN_POINT ( 'NONE',  ( -35.00000000000000000, 9.240395740215735287, -7.251710744571480127 ) ) ;
#47859 = ORIENTED_EDGE ( 'NONE', *, *, #64538, .T. ) ;
#47860 = DIRECTION ( 'NONE',  ( 0.000000000000000000, 0.000000000000000000, 1.000000000000000000 ) ) ;
#47861 = CARTESIAN_POINT ( 'NONE',  ( -22.27711653538342773, 2.958138731383647801, -2.191780254295670805 ) ) ;
#47862 = CARTESIAN_POINT ( 'NONE',  ( 29.71521259808911353, 6.759044707574296318, 9.927718093057791293 ) ) ;
#47863 = DIRECTION ( 'NONE',  ( -1.000000000000000000, 0.000000000000000000, 0.000000000000000000 ) ) ;
#47864 = DIRECTION ( 'NONE',  ( 0.000000000000000000, -0.6478160128811839558, 0.7617968321374970486 ) ) ;
#47865 = AXIS2_PLACEMENT_3D ( 'NONE', #24107, #23799, #49410 ) ;
#47866 = ORIENTED_EDGE ( 'NONE', *, *, #59913, .F. ) ;
#47867 = CARTESIAN_POINT ( 'NONE',  ( 2.573738926104373714, -7.194322927777932364, -2.868819712476781358 ) ) ;
#47868 = VECTOR ( 'NONE', #59388, 1000.000000000000000 ) ;
#47869 = AXIS2_PLACEMENT_3D ( 'NONE', #49346, #39317, #53663 ) ;
#47870 = EDGE_LOOP ( 'NONE', ( #11336, #13248, #54921, #58427 ) ) ;
#47871 = CARTESIAN_POINT ( 'NONE',  ( 37.00000000000000711, 0.01609748574445066943, -11.74614673114903773 ) ) ;
#47872 = CARTESIAN_POINT ( 'NONE',  ( 0.3106921474978496800, -0.2354703039888949578, 12.25904950202576416 ) ) ;
#47873 = FACE_OUTER_BOUND ( 'NONE', #20974, .T. ) ;
#47874 = VECTOR ( 'NONE', #26343, 1000.000000000000000 ) ;
#47875 = CARTESIAN_POINT ( 'NONE',  ( -27.08776759928964495, -0.6183458186125521117, -2.217308861843124035 ) ) ;
#47876 = CARTESIAN_POINT ( 'NONE',  ( 2.899286259009687505, -4.769992516330196608, -6.239228647238621583 ) ) ;
#47877 = VERTEX_POINT ( 'NONE', #3149 ) ;
#47878 = DIRECTION ( 'NONE',  ( 0.000000000000000000, -0.9651210252299822212, -0.2618041379715529970 ) ) ;
#47880 = VECTOR ( 'NONE', #39582, 1000.000000000000000 ) ;
#47879 = CARTESIAN_POINT ( 'NONE',  ( -37.00000000000000711, 9.217970097227725645, 7.971186206369506699 ) ) ;
#47881 = CARTESIAN_POINT ( 'NONE',  ( -18.04458733766117362, -12.91933584589293282, 3.916728392552376370 ) ) ;
#47882 = DIRECTION ( 'NONE',  ( -0.000000000000000000, -1.000000000000000000, -0.000000000000000000 ) ) ;
#47883 = AXIS2_PLACEMENT_3D ( 'NONE', #54878, #44237, #13329 ) ;
#47884 = EDGE_CURVE ( 'NONE', #8663, #5051, #63614, .T. ) ;
#47885 = CARTESIAN_POINT ( 'NONE',  ( -22.46225619532221529, -1.978788174090782226, 3.746472695305350875 ) ) ;
#47886 = ORIENTED_EDGE ( 'NONE', *, *, #18619, .F. ) ;
#47887 = UNCERTAINTY_MEASURE_WITH_UNIT (LENGTH_MEASURE( 1.000000000000000082E-05 ), #34154, 'distance_accuracy_value', 'NONE');
#47888 = FACE_OUTER_BOUND ( 'NONE', #23467, .T. ) ;
#47889 = CIRCLE ( 'NONE', #38331, 5.000000000000000000 ) ;
#47890 = CARTESIAN_POINT ( 'NONE',  ( -4.578562111148198888, -30.90741127680383471, 14.86059354493743179 ) ) ;
#47891 = TOROIDAL_SURFACE ( 'NONE', #4427, 5.000000000000000888, 20.00000000000000000 ) ;
#47892 = AXIS2_PLACEMENT_3D ( 'NONE', #1910, #62402, #47150 ) ;
#47893 = EDGE_CURVE ( 'NONE', #42133, #40353, #33708, .T. ) ;
#47894 = VECTOR ( 'NONE', #37837, 1000.000000000000000 ) ;
#47895 = ORIENTED_EDGE ( 'NONE', *, *, #4518, .T. ) ;
#47896 = CARTESIAN_POINT ( 'NONE',  ( 10.75853767213705225, 7.830989516993144051, -9.092612561015865680 ) ) ;
#47897 = ORIENTED_EDGE ( 'NONE', *, *, #4890, .F. ) ;
#47898 = CARTESIAN_POINT ( 'NONE',  ( 0.3665391374699464300, 10.50279796150436695, 6.368473106897166502 ) ) ;
#47899 = CARTESIAN_POINT ( 'NONE',  ( 5.515539859299206427, -0.004037661319611337077, -0.004509673239148472360 ) ) ;
#47900 = AXIS2_PLACEMENT_3D ( 'NONE', #20456, #51049, #25119 ) ;
#47901 = CARTESIAN_POINT ( 'NONE',  ( -27.08702828306176613, -1.639744581304558801, -1.612407531674189709 ) ) ;
#47902 = CARTESIAN_POINT ( 'NONE',  ( 0.000000000000000000, 3.341639490130761114, 6.078525953551427996 ) ) ;
#47903 = CARTESIAN_POINT ( 'NONE',  ( -22.29479313954897535, -2.096782908204890550, -3.090162644873553077 ) ) ;
#47904 = ORIENTED_EDGE ( 'NONE', *, *, #12556, .F. ) ;
#47905 = EDGE_LOOP ( 'NONE', ( #21459, #6302, #65080, #62760 ) ) ;
#47906 = ORIENTED_EDGE ( 'NONE', *, *, #49450, .F. ) ;
#47907 = DIRECTION ( 'NONE',  ( 0.000000000000000000, -0.6269146997508042718, -0.7790879021242460567 ) ) ;
#47908 = AXIS2_PLACEMENT_3D ( 'NONE', #7940, #37852, #57830 ) ;
#47909 = AXIS2_PLACEMENT_3D ( 'NONE', #58697, #44034, #64306 ) ;
#47910 = FACE_OUTER_BOUND ( 'NONE', #6010, .T. ) ;
#47911 = ORIENTED_EDGE ( 'NONE', *, *, #55567, .T. ) ;
#47912 = LINE ( 'NONE', #2372, #1808 ) ;
#47913 = AXIS2_PLACEMENT_3D ( 'NONE', #31901, #11631, #1994 ) ;
#47914 = LINE ( 'NONE', #2374, #52341 ) ;
#47915 = ORIENTED_EDGE ( 'NONE', *, *, #56603, .T. ) ;
#47916 = CARTESIAN_POINT ( 'NONE',  ( -37.00000000000000711, -8.839356091079983102, -8.389074212634382022 ) ) ;
#47917 = DIRECTION ( 'NONE',  ( 1.000000000000000000, 0.000000000000000000, 0.000000000000000000 ) ) ;
#47918 = CARTESIAN_POINT ( 'NONE',  ( 24.19646710323674554, 1.946597173898756861, 11.84653191271039852 ) ) ;
#47919 = ORIENTED_EDGE ( 'NONE', *, *, #4589, .F. ) ;
#47920 = VERTEX_POINT ( 'NONE', #54004 ) ;
#47921 = DIRECTION ( 'NONE',  ( 0.000000000000000000, 0.9346839223284553189, -0.3554799084908935036 ) ) ;
#47922 = VERTEX_POINT ( 'NONE', #8444 ) ;
#47923 = CARTESIAN_POINT ( 'NONE',  ( -35.00000000000000000, 0.000000000000000000, 0.000000000000000000 ) ) ;
#47924 = ORIENTED_EDGE ( 'NONE', *, *, #13804, .T. ) ;
#47925 = AXIS2_PLACEMENT_3D ( 'NONE', #21174, #52104, #61738 ) ;
#47926 = CARTESIAN_POINT ( 'NONE',  ( 2.276198483117263915, 3.688810392808549832, 6.697332984100271780 ) ) ;
#47927 = CARTESIAN_POINT ( 'NONE',  ( 3.474089039505902754, -31.27092243478551126, -14.18576039181806614 ) ) ;
#47928 = EDGE_CURVE ( 'NONE', #54691, #56717, #15402, .T. ) ;
#47929 = FACE_OUTER_BOUND ( 'NONE', #56117, .T. ) ;
#47930 = CARTESIAN_POINT ( 'NONE',  ( -22.29195009621226831, 3.616122380634898992, 0.8975732442595152349 ) ) ;
#47931 = DIRECTION ( 'NONE',  ( -0.000000000000000000, -1.000000000000000000, -0.000000000000000000 ) ) ;
#47932 = CARTESIAN_POINT ( 'NONE',  ( 0.7446945582530690722, 6.508900271376239388, -10.56139717223440933 ) ) ;
#47933 = DIRECTION ( 'NONE',  ( -1.000000000000000000, 0.000000000000000000, 0.000000000000000000 ) ) ;
#47934 = ORIENTED_EDGE ( 'NONE', *, *, #59126, .T. ) ;
#47935 = CARTESIAN_POINT ( 'NONE',  ( -22.66110217412718697, -4.192227617777427362, -2.622110956932569348 ) ) ;
#47936 = AXIS2_PLACEMENT_3D ( 'NONE', #47451, #11208, #31485 ) ;
#47937 = ORIENTED_EDGE ( 'NONE', *, *, #37764, .T. ) ;
#47938 = CARTESIAN_POINT ( 'NONE',  ( 2.242819959140644137, -2.707278038035121792, 7.138786956204155487 ) ) ;
#47939 = LINE ( 'NONE', #42940, #21315 ) ;
#47940 = AXIS2_PLACEMENT_3D ( 'NONE', #478, #51988, #1115 ) ;
#47941 = ORIENTED_EDGE ( 'NONE', *, *, #53963, .F. ) ;
#47942 = CARTESIAN_POINT ( 'NONE',  ( 1.372161826076382374, -12.60140585080803177, 0.5897614319403238214 ) ) ;
#47943 = CARTESIAN_POINT ( 'NONE',  ( 0.2648978790185619880, 12.03635331166815270, -2.256510822326019738 ) ) ;
#47944 = CARTESIAN_POINT ( 'NONE',  ( -35.04660725145885891, -0.001288602543478920958, -0.01223081933020915557 ) ) ;
#47946 = ADVANCED_FACE ( 'NONE', ( #10392 ), #4794, .T. ) ;
#47945 = ORIENTED_EDGE ( 'NONE', *, *, #36135, .T. ) ;
#47947 = CIRCLE ( 'NONE', #34100, 2.899999999999995026 ) ;
#47948 = CIRCLE ( 'NONE', #56430, 4.999999999999999112 ) ;
#47949 = AXIS2_PLACEMENT_3D ( 'NONE', #47716, #6503, #22439 ) ;
#47950 = ORIENTED_EDGE ( 'NONE', *, *, #6223, .T. ) ;
#47951 = FACE_OUTER_BOUND ( 'NONE', #13782, .T. ) ;
#47952 = VERTEX_POINT ( 'NONE', #40006 ) ;
#47953 = CARTESIAN_POINT ( 'NONE',  ( 3.047904605210380424, -6.318654123925923294, 4.747272783555632536 ) ) ;
#47954 = DIRECTION ( 'NONE',  ( 1.000000000000000000, 0.000000000000000000, 0.000000000000000000 ) ) ;
#47955 = FACE_OUTER_BOUND ( 'NONE', #39209, .T. ) ;
#47956 = CARTESIAN_POINT ( 'NONE',  ( -7.291047549687194262, 5.640864668324928388, -10.59540170654024749 ) ) ;
#47957 = B_SPLINE_CURVE_WITH_KNOTS ( 'NONE', 3,
 ( #56238, #31617, #46597, #41604, #25016, #55608, #10681, #65546, #10045, #15356, #61235, #20015, #726, #51283, #5733, #56587, #26001, #46285, #50941 ),
 .UNSPECIFIED., .F., .F.,
 ( 4, 3, 3, 3, 3, 3, 4 ),
 ( 5.502793334042459344E-18, 2.825908398782625081E-05, 4.208813692417807169E-05, 5.591713746860116585E-05, 6.279584083139550150E-05, 9.105792820166967901E-05, 0.0001153131102489458491 ),
 .UNSPECIFIED. ) ;
#47958 = ORIENTED_EDGE ( 'NONE', *, *, #46129, .F. ) ;
#47959 = DIRECTION ( 'NONE',  ( -1.000000000000000000, 0.000000000000000000, -0.000000000000000000 ) ) ;
#47960 = VECTOR ( 'NONE', #33024, 1000.000000000000000 ) ;
#47961 = AXIS2_PLACEMENT_3D ( 'NONE', #30205, #20561, #49834 ) ;
#47962 = EDGE_CURVE ( 'NONE', #49787, #21262, #24128, .T. ) ;
#47963 = DIRECTION ( 'NONE',  ( 0.9606638835031803270, -0.2249116044183857577, 0.1629100154396148359 ) ) ;
#47964 = CARTESIAN_POINT ( 'NONE',  ( -37.00000000000000711, 0.000000000000000000, 0.000000000000000000 ) ) ;
#47965 = AXIS2_PLACEMENT_3D ( 'NONE', #48005, #11742, #37350 ) ;
#47966 = CARTESIAN_POINT ( 'NONE',  ( 22.46858150504636242, 12.34520901837059448, -5.474447245564200593 ) ) ;
#47967 = DIRECTION ( 'NONE',  ( 1.000000000000000000, 0.000000000000000000, 0.000000000000000000 ) ) ;
#47968 = ADVANCED_FACE ( 'NONE', ( #20059 ), #35980, .T. ) ;
#47969 = FACE_OUTER_BOUND ( 'NONE', #18596, .T. ) ;
#47970 = CARTESIAN_POINT ( 'NONE',  ( 22.00000000000000711, -20.00000000000000000, 2.449293598294706907E-15 ) ) ;
#47971 = CARTESIAN_POINT ( 'NONE',  ( 1.719304012338210619, 10.62216384465585328, 7.017415949611872428 ) ) ;
#47972 = AXIS2_PLACEMENT_3D ( 'NONE', #57028, #46072, #36051 ) ;
#47973 = EDGE_CURVE ( 'NONE', #29718, #40530, #55927, .T. ) ;
#47974 = VERTEX_POINT ( 'NONE', #450 ) ;
#47975 = DIRECTION ( 'NONE',  ( 1.000000000000000000, 0.000000000000000000, 0.000000000000000000 ) ) ;
#47976 = CARTESIAN_POINT ( 'NONE',  ( 6.023978964358256860, -8.806351789236446237, 10.23755192329234553 ) ) ;
#47977 = CIRCLE ( 'NONE', #24623, 4.999999999999999112 ) ;
#47978 = ORIENTED_EDGE ( 'NONE', *, *, #6347, .F. ) ;
#47979 = CARTESIAN_POINT ( 'NONE',  ( -22.31099767395441091, 3.774495463598467548, -0.2534174342804001445 ) ) ;
#47980 = CARTESIAN_POINT ( 'NONE',  ( -22.59969328935897082, 3.618004136135768878, 2.921971394153407342 ) ) ;
#47981 = ORIENTED_EDGE ( 'NONE', *, *, #13925, .T. ) ;
#47982 = CIRCLE ( 'NONE', #28700, 1.750000000000000000 ) ;
#47983 = AXIS2_PLACEMENT_3D ( 'NONE', #53134, #7577, #27866 ) ;
#47984 = CYLINDRICAL_SURFACE ( 'NONE', #30974, 5.000000000000000888 ) ;
#47985 = ORIENTED_EDGE ( 'NONE', *, *, #15250, .F. ) ;
#47986 = EDGE_CURVE ( 'NONE', #31670, #22816, #60978, .T. ) ;
#47987 = DIRECTION ( 'NONE',  ( 1.000000000000000000, 0.000000000000000000, 0.000000000000000000 ) ) ;
#47988 = VERTEX_POINT ( 'NONE', #55649 ) ;
#47989 = VERTEX_POINT ( 'NONE', #60961 ) ;
#47990 = CARTESIAN_POINT ( 'NONE',  ( -22.28350523959500862, -3.346230442873233013, -1.580062893038987948 ) ) ;
#47991 = CIRCLE ( 'NONE', #63876, 12.18650000000000055 ) ;
#47992 = VECTOR ( 'NONE', #30687, 1000.000000000000000 ) ;
#47993 = ORIENTED_EDGE ( 'NONE', *, *, #24056, .F. ) ;
#47994 = EDGE_CURVE ( 'NONE', #22369, #62776, #15396, .T. ) ;
#47995 = CARTESIAN_POINT ( 'NONE',  ( -24.94425671793833388, -9.239554407049443085, 7.659171101073906307 ) ) ;
#47996 = CARTESIAN_POINT ( 'NONE',  ( 0.6525221082932635142, -0.1557174252009511373, 13.50151297108246595 ) ) ;
#47997 = DIRECTION ( 'NONE',  ( -1.000000000000000000, -0.000000000000000000, 0.000000000000000000 ) ) ;
#47998 = DIRECTION ( 'NONE',  ( 0.000000000000000000, -0.01356324068817998940, 0.9999080150203990547 ) ) ;
#47999 = VERTEX_POINT ( 'NONE', #5434 ) ;
#48000 = CARTESIAN_POINT ( 'NONE',  ( 0.2872850955227740366, -7.715220952083302386, 9.519656861923696312 ) ) ;
#48001 = CARTESIAN_POINT ( 'NONE',  ( 16.21117406328132304, -34.99999999999999289, 4.142385751841744401 ) ) ;
#48002 = DIRECTION ( 'NONE',  ( -1.000000000000000000, 0.000000000000000000, 0.000000000000000000 ) ) ;
#48004 = ORIENTED_EDGE ( 'NONE', *, *, #3153, .T. ) ;
#48003 = DIRECTION ( 'NONE',  ( -1.000000000000000000, 0.000000000000000000, 0.000000000000000000 ) ) ;
#48005 = CARTESIAN_POINT ( 'NONE',  ( -25.00000000000000355, -9.999999999999998224, 5.000000000000000888 ) ) ;
#48006 = VERTEX_POINT ( 'NONE', #25707 ) ;
#48007 = DIRECTION ( 'NONE',  ( 0.000000000000000000, 0.3193015301359742875, 0.9476531711828043436 ) ) ;
#48008 = EDGE_LOOP ( 'NONE', ( #13968, #14056, #60725, #24384 ) ) ;
#48009 = CARTESIAN_POINT ( 'NONE',  ( 2.241352910868909643, 7.145045428366612050, -2.689314586382279604 ) ) ;
#48010 = AXIS2_PLACEMENT_3D ( 'NONE', #76, #56607, #21002 ) ;
#48011 = CARTESIAN_POINT ( 'NONE',  ( 0.3675815128205894289, 3.951233083390626177, -11.62724744438061641 ) ) ;
#48012 = CARTESIAN_POINT ( 'NONE',  ( 0.2739690278137243973, -4.016979056590845865, 11.57167385487631961 ) ) ;
#48013 = AXIS2_PLACEMENT_3D ( 'NONE', #12533, #27851, #32812 ) ;
#48014 = PLANE ( 'NONE',  #40839 ) ;
#48015 = CARTESIAN_POINT ( 'NONE',  ( 2.655192694323964098, -9.539062147542258785, -1.093661162899928430 ) ) ;
#48016 = DIRECTION ( 'NONE',  ( -1.000000000000000000, 0.000000000000000000, 0.000000000000000000 ) ) ;
#48018 = ORIENTED_EDGE ( 'NONE', *, *, #25299, .F. ) ;
#48017 = VECTOR ( 'NONE', #47397, 1000.000000000000000 ) ;
#48019 = VERTEX_POINT ( 'NONE', #20720 ) ;
#48020 = CARTESIAN_POINT ( 'NONE',  ( 0.2833330754217378566, 12.02930703389100131, 2.326361469893271305 ) ) ;
#48021 = ORIENTED_EDGE ( 'NONE', *, *, #51569, .F. ) ;
#48022 = VECTOR ( 'NONE', #7024, 1000.000000000000000 ) ;
#48023 = VERTEX_POINT ( 'NONE', #39686 ) ;
#48024 = DIRECTION ( 'NONE',  ( 0.000000000000000000, -0.5987040770935561085, 0.8009703041134255130 ) ) ;
#48025 = CARTESIAN_POINT ( 'NONE',  ( -22.28236030719477867, 3.345835236227605147, 1.572829798448300176 ) ) ;
#48026 = DIRECTION ( 'NONE',  ( 1.000000000000000000, 0.000000000000000000, 0.000000000000000000 ) ) ;
#48027 = CARTESIAN_POINT ( 'NONE',  ( -22.29290468048228036, 2.097193667172415399, 3.083035815361880427 ) ) ;
#48028 = CARTESIAN_POINT ( 'NONE',  ( 145.1370849898475797, 3.309064568108273190E-14, 0.000000000000000000 ) ) ;
#48029 = EDGE_CURVE ( 'NONE', #57274, #43036, #30719, .T. ) ;
#48030 = CARTESIAN_POINT ( 'NONE',  ( 36.00000000000000711, 12.26766708251991567, -3.473736367725301033 ) ) ;
#48031 = DIRECTION ( 'NONE',  ( 0.000000000000000000, 0.000000000000000000, 1.000000000000000000 ) ) ;
#48032 = AXIS2_PLACEMENT_3D ( 'NONE', #59378, #18169, #38777 ) ;
#48033 = VERTEX_POINT ( 'NONE', #11072 ) ;
#48034 = LINE ( 'NONE', #25521, #34473 ) ;
#48035 = CARTESIAN_POINT ( 'NONE',  ( 0.2638984909335720941, 6.295352574288986425, 10.50550771760521940 ) ) ;
#48036 = CIRCLE ( 'NONE', #27854, 24.00000000000000000 ) ;
#48037 = CIRCLE ( 'NONE', #28906, 2.899999999999997247 ) ;
#48038 = CARTESIAN_POINT ( 'NONE',  ( 2.276905613633655623, -4.795880183929603469, 5.955225895210576326 ) ) ;
#48039 = LINE ( 'NONE', #1829, #63012 ) ;
#48040 = B_SPLINE_CURVE_WITH_KNOTS ( 'NONE', 3,
 ( #41990, #62270, #62588, #36997, #32007, #52328, #17050, #18047, #33338, #59846, #37982, #9273, #7745, #58631, #44864, #17396, #28031, #22717, #37672 ),
 .UNSPECIFIED., .F., .F.,
 ( 4, 3, 3, 3, 3, 3, 4 ),
 ( 4.336808689942017736E-19, 2.831840207625253706E-05, 4.217266860012148388E-05, 5.602024318565883461E-05, 6.290810168138159136E-05, 9.120440631110341779E-05, 0.0001153103026478300612 ),
 .UNSPECIFIED. ) ;
#48041 = AXIS2_PLACEMENT_3D ( 'NONE', #7824, #38053, #27424 ) ;
#48042 = EDGE_CURVE ( 'NONE', #58393, #13080, #18024, .T. ) ;
#48043 = DIRECTION ( 'NONE',  ( -1.000000000000000000, 0.000000000000000000, 0.000000000000000000 ) ) ;
#48044 = CARTESIAN_POINT ( 'NONE',  ( -37.00000000000000711, 0.000000000000000000, 0.000000000000000000 ) ) ;
#48045 = EDGE_CURVE ( 'NONE', #33727, #42381, #21712, .T. ) ;
#48046 = CARTESIAN_POINT ( 'NONE',  ( 10.67051787153030595, 1.171189490780102593, -11.94370412967601780 ) ) ;
#48047 = EDGE_CURVE ( 'NONE', #22824, #46888, #38174, .T. ) ;
#48048 = VERTEX_POINT ( 'NONE', #31981 ) ;
#48049 = CARTESIAN_POINT ( 'NONE',  ( 37.00000000000000711, 4.705694406421931860E-17, -3.469127814946512892E-15 ) ) ;
#48050 = CARTESIAN_POINT ( 'NONE',  ( -19.47984447937493613, -3.750539801530005768, 25.00000000000000000 ) ) ;
#48051 = CYLINDRICAL_SURFACE ( 'NONE', #14125, 12.74999999999999822 ) ;
#48052 = CARTESIAN_POINT ( 'NONE',  ( 35.00000000000000000, -0.7536123767497623360, 11.72195762423410237 ) ) ;
#48053 = AXIS2_PLACEMENT_3D ( 'NONE', #48088, #57396, #52427 ) ;
#48054 = AXIS2_PLACEMENT_3D ( 'NONE', #11480, #52062, #6511 ) ;
#48055 = ADVANCED_FACE ( 'NONE', ( #11382 ), #57278, .T. ) ;
#48056 = DIRECTION ( 'NONE',  ( -1.000000000000000000, 0.000000000000000000, -0.000000000000000000 ) ) ;
#48057 = DIRECTION ( 'NONE',  ( 0.000000000000000000, 0.000000000000000000, 1.000000000000000000 ) ) ;
#48058 = AXIS2_PLACEMENT_3D ( 'NONE', #3701, #23963, #13951 ) ;
#48059 = ORIENTED_EDGE ( 'NONE', *, *, #33853, .T. ) ;
#48060 = CARTESIAN_POINT ( 'NONE',  ( 17.82596851127161841, -8.594641745053730020, 8.387315214446159573 ) ) ;
#48061 = FACE_OUTER_BOUND ( 'NONE', #22789, .T. ) ;
#48062 = ADVANCED_FACE ( 'NONE', ( #1092 ), #47395, .F. ) ;
#48063 = CARTESIAN_POINT ( 'NONE',  ( 10.75853767213705048, 7.830989516993144051, 10.99661780661416088 ) ) ;
#48064 = CARTESIAN_POINT ( 'NONE',  ( 3.152665057735613008, -6.378477742801520023, -4.725420687649700469 ) ) ;
#48065 = ORIENTED_EDGE ( 'NONE', *, *, #54223, .T. ) ;
#48066 = DIRECTION ( 'NONE',  ( -1.000000000000000000, -1.836970198721029688E-16, 0.000000000000000000 ) ) ;
#48067 = DIRECTION ( 'NONE',  ( 0.000000000000000000, 0.01356324068817998940, -0.9999080150203989437 ) ) ;
#48068 = EDGE_LOOP ( 'NONE', ( #30950, #731, #33305, #38201 ) ) ;
#48069 = ORIENTED_EDGE ( 'NONE', *, *, #58682, .T. ) ;
#48070 = LINE ( 'NONE', #27431, #7645 ) ;
#48071 = EDGE_CURVE ( 'NONE', #63981, #4532, #21187, .T. ) ;
#48072 = DIRECTION ( 'NONE',  ( -1.000000000000000000, 0.000000000000000000, 0.000000000000000000 ) ) ;
#48073 = VERTEX_POINT ( 'NONE', #763 ) ;
#48074 = EDGE_CURVE ( 'NONE', #26195, #50843, #62564, .T. ) ;
#48075 = DIRECTION ( 'NONE',  ( -1.000000000000000000, 0.000000000000000000, 0.000000000000000000 ) ) ;
#48076 = CIRCLE ( 'NONE', #10897, 4.999999999999999112 ) ;
#48077 = CARTESIAN_POINT ( 'NONE',  ( 37.00000000000000711, 6.946017217730083182, 10.01317267707878678 ) ) ;
#48078 = CARTESIAN_POINT ( 'NONE',  ( -37.00000000000000711, -4.237620530777717498, -11.42599468261433771 ) ) ;
#48079 = CARTESIAN_POINT ( 'NONE',  ( -35.00000000000000000, 3.916263239775508165, -11.07407352312208459 ) ) ;
#48080 = CARTESIAN_POINT ( 'NONE',  ( -27.39656561727367290, 9.459410533876226879, -7.405734381554731627 ) ) ;
#48081 = ADVANCED_FACE ( 'NONE', ( #31652 ), #1753, .T. ) ;
#48082 = CARTESIAN_POINT ( 'NONE',  ( 0.3053067050349160261, 5.928821939311931466, 10.73055518945190023 ) ) ;
#48084 = ORIENTED_EDGE ( 'NONE', *, *, #7609, .T. ) ;
#48083 = CYLINDRICAL_SURFACE ( 'NONE', #45665, 4.999999999999998224 ) ;
#48085 = CARTESIAN_POINT ( 'NONE',  ( 0.7446945582529681529, 4.576048078259359109, -11.53120448859789882 ) ) ;
#48086 = ORIENTED_EDGE ( 'NONE', *, *, #40388, .F. ) ;
#48087 = CIRCLE ( 'NONE', #39717, 2.899999999999995026 ) ;
#48088 = CARTESIAN_POINT ( 'NONE',  ( 37.00000000000000711, 4.705694406421931860E-17, -3.469127814946512892E-15 ) ) ;
#48089 = ORIENTED_EDGE ( 'NONE', *, *, #12043, .F. ) ;
#48090 = CIRCLE ( 'NONE', #291, 1.499999999999998224 ) ;
#48091 = ORIENTED_EDGE ( 'NONE', *, *, #18952, .F. ) ;
#48092 = CONTEXT_DEPENDENT_SHAPE_REPRESENTATION ( #30656, #17527 ) ;
#48093 = CARTESIAN_POINT ( 'NONE',  ( -14.64443717355071151, 8.412151427010677196, 10.55874966731845710 ) ) ;
#48094 = CARTESIAN_POINT ( 'NONE',  ( -17.34314652423584491, -29.56569286319672685, 9.163921882790974749 ) ) ;
#48095 = CARTESIAN_POINT ( 'NONE',  ( 2.368238019615373169, 1.509700170844646250, 7.526794520527686494 ) ) ;
#48096 = AXIS2_PLACEMENT_3D ( 'NONE', #34938, #18719, #34624 ) ;
#48097 = CARTESIAN_POINT ( 'NONE',  ( -49.00067463083242103, -0.2018647702350209738, -0.7653472444253763829 ) ) ;
#48098 = CARTESIAN_POINT ( 'NONE',  ( -27.08417473062937120, 0.7460375461499409999, -2.166271322019588830 ) ) ;
#48099 = ORIENTED_EDGE ( 'NONE', *, *, #46689, .T. ) ;
#48100 = DIRECTION ( 'NONE',  ( 1.000000000000000000, 0.000000000000000000, 0.000000000000000000 ) ) ;
#48101 = DIRECTION ( 'NONE',  ( 0.000000000000000000, -0.01356324068817998940, 0.9999080150203990547 ) ) ;
#48103 = VERTEX_POINT ( 'NONE', #6407 ) ;
#48102 = CARTESIAN_POINT ( 'NONE',  ( 37.00000000000000711, 2.527899948230813987, 12.49688848680881037 ) ) ;
#48104 = ORIENTED_EDGE ( 'NONE', *, *, #1493, .T. ) ;
#48105 = CARTESIAN_POINT ( 'NONE',  ( 2.000000000000001776, 0.000000000000000000, 0.000000000000000000 ) ) ;
#48106 = ORIENTED_EDGE ( 'NONE', *, *, #27487, .T. ) ;
#48107 = CIRCLE ( 'NONE', #50246, 12.18649999999999878 ) ;
#48108 = CARTESIAN_POINT ( 'NONE',  ( -35.00000000000000000, 11.67026961469348123, 4.564151185897117102 ) ) ;
#48109 = CARTESIAN_POINT ( 'NONE',  ( 0.3040950598368152291, -3.956873563689608631, 11.60568999039893257 ) ) ;
#48110 = CARTESIAN_POINT ( 'NONE',  ( 36.00000000000000711, 11.10408318471059452, -6.265926637539535271 ) ) ;
#48111 = CARTESIAN_POINT ( 'NONE',  ( -37.00000000000000711, -3.033604067594665388, 12.38385022362080967 ) ) ;
#48112 = CIRCLE ( 'NONE', #65069, 2.899999999999995470 ) ;
#48113 = ADVANCED_FACE ( 'NONE', ( #42270 ), #21364, .T. ) ;
#48114 = EDGE_CURVE ( 'NONE', #5549, #44780, #41965, .T. ) ;
#48115 = CARTESIAN_POINT ( 'NONE',  ( 2.000000000000001776, 0.000000000000000000, 0.000000000000000000 ) ) ;
#48116 = CARTESIAN_POINT ( 'NONE',  ( -27.09602251845210930, -1.927725285107524611, 1.302811993375579069 ) ) ;
#48117 = CARTESIAN_POINT ( 'NONE',  ( -35.00000000000000000, 9.821084925794572484, 7.215058775251292467 ) ) ;
#48118 = ORIENTED_EDGE ( 'NONE', *, *, #22198, .F. ) ;
#48119 = LINE ( 'NONE', #2896, #44382 ) ;
#48120 = ORIENTED_EDGE ( 'NONE', *, *, #24861, .T. ) ;
#48121 = AXIS2_PLACEMENT_3D ( 'NONE', #38772, #53745, #53073 ) ;
#48122 = DIRECTION ( 'NONE',  ( 1.000000000000000000, 0.000000000000000000, 0.000000000000000000 ) ) ;
#48123 = DIRECTION ( 'NONE',  ( 1.000000000000000000, 0.000000000000000000, -0.000000000000000000 ) ) ;
#48124 = DIRECTION ( 'NONE',  ( 1.000000000000000000, 0.000000000000000000, 0.000000000000000000 ) ) ;
#48125 = EDGE_CURVE ( 'NONE', #32242, #6535, #15855, .T. ) ;
#48126 = CARTESIAN_POINT ( 'NONE',  ( 29.51976981715666781, 4.571419055710094881, 11.09513982864076276 ) ) ;
#48127 = ORIENTED_EDGE ( 'NONE', *, *, #10807, .F. ) ;
#48128 = ORIENTED_EDGE ( 'NONE', *, *, #52269, .F. ) ;
#48129 = AXIS2_PLACEMENT_3D ( 'NONE', #50085, #34752, #9827 ) ;
#48130 = EDGE_CURVE ( 'NONE', #22014, #62401, #57618, .T. ) ;
#48131 = CARTESIAN_POINT ( 'NONE',  ( -27.08430418657511751, 0.2231435303617252952, 2.280643121250616190 ) ) ;
#48132 = ORIENTED_EDGE ( 'NONE', *, *, #31753, .F. ) ;
#48133 = CARTESIAN_POINT ( 'NONE',  ( -35.00000000000000000, 0.000000000000000000, 0.000000000000000000 ) ) ;
#48134 = CARTESIAN_POINT ( 'NONE',  ( 37.00000000000000711, 4.705694406421931860E-17, -3.469127814946512892E-15 ) ) ;
#48135 = CARTESIAN_POINT ( 'NONE',  ( -22.27706485742869091, -3.547445275915918295, -0.9832726768967802178 ) ) ;
#48136 = CARTESIAN_POINT ( 'NONE',  ( 2.251139882113958546, 1.448366094935513937, -7.499076289418090013 ) ) ;
#48137 = ADVANCED_FACE ( 'NONE', ( #19634 ), #15914, .T. ) ;
#48138 = EDGE_LOOP ( 'NONE', ( #12349, #24096, #25618, #19917 ) ) ;
#48139 = AXIS2_PLACEMENT_3D ( 'NONE', #24327, #54625, #44592 ) ;
#48140 = CARTESIAN_POINT ( 'NONE',  ( 2.440552418640494103, 2.447453236303825719, 7.301551120181771992 ) ) ;
#48141 = CARTESIAN_POINT ( 'NONE',  ( -22.29382655386184453, -2.586160974799824874, 2.689927793811020429 ) ) ;
#48142 = CIRCLE ( 'NONE', #31121, 5.000000000000000000 ) ;
#48143 = CARTESIAN_POINT ( 'NONE',  ( -23.41523303002442091, 0.3963225057405129759, -4.681453266967039006 ) ) ;
#48144 = DIRECTION ( 'NONE',  ( -1.000000000000000000, 0.000000000000000000, 0.000000000000000000 ) ) ;
#48145 = CIRCLE ( 'NONE', #1437, 12.74999999999999822 ) ;
#48146 = CIRCLE ( 'NONE', #37488, 4.999999999999998224 ) ;
#48147 = CARTESIAN_POINT ( 'NONE',  ( 2.244591118396558116, -0.1074970442783618058, -7.634724215899730382 ) ) ;
#48148 = CARTESIAN_POINT ( 'NONE',  ( 3.152665057736261822, -7.102135024647099115, -3.546019893114602972 ) ) ;
#48149 = ORIENTED_EDGE ( 'NONE', *, *, #19207, .F. ) ;
#48150 = CARTESIAN_POINT ( 'NONE',  ( -35.00000000000000000, -12.01765980939843281, 2.021542716731355771 ) ) ;
#48151 = CARTESIAN_POINT ( 'NONE',  ( 29.68049421394466236, 10.47771764608172695, 8.515736641621126424 ) ) ;
#48152 = EDGE_CURVE ( 'NONE', #15867, #4408, #23338, .T. ) ;
#48153 = AXIS2_PLACEMENT_3D ( 'NONE', #59558, #9647, #24973 ) ;
#48154 = FACE_OUTER_BOUND ( 'NONE', #47373, .T. ) ;
#48155 = ORIENTED_EDGE ( 'NONE', *, *, #23379, .F. ) ;
#48156 = CARTESIAN_POINT ( 'NONE',  ( -11.37097780465418140, -6.763195055119394006, -11.69186615500488280 ) ) ;
#48157 = CARTESIAN_POINT ( 'NONE',  ( 0.8375941296801004965, -8.285008510335032383, 9.275620596396437989 ) ) ;
#48158 = CARTESIAN_POINT ( 'NONE',  ( 3.152665057734040488, 0.000000000000000000, 0.000000000000000000 ) ) ;
#48159 = CIRCLE ( 'NONE', #57744, 2.899999999999994582 ) ;
#48160 = B_SPLINE_CURVE_WITH_KNOTS ( 'NONE', 3,
 ( #15379, #35650, #10377, #51307, #30653, #5412, #20702, #61255, #56613, #32608, #41289, #21693, #7038, #27307, #747, #6078, #11685, #32298, #52917 ),
 .UNSPECIFIED., .F., .F.,
 ( 4, 3, 3, 3, 3, 3, 4 ),
 ( 8.911587868699592868E-18, 4.457896483015155633E-05, 6.639290541542550606E-05, 8.820687556479513418E-05, 0.0001100173248778960430, 0.0001545671401658155718, 0.0001830328308068577907 ),
 .UNSPECIFIED. ) ;
#48161 = CARTESIAN_POINT ( 'NONE',  ( -29.06964327085373156, 3.363168872084723038, -13.08058491801428680 ) ) ;
#48162 = CARTESIAN_POINT ( 'NONE',  ( 0.2956976708475475002, -11.59055635407404594, 3.984495122852534710 ) ) ;
#48163 = ADVANCED_FACE ( 'NONE', ( #24605 ), #46214, .T. ) ;
#48164 = CIRCLE ( 'NONE', #56651, 12.18650000000000055 ) ;
#48165 = ORIENTED_EDGE ( 'NONE', *, *, #58276, .T. ) ;
#48166 = VERTEX_POINT ( 'NONE', #329 ) ;
#48167 = DIRECTION ( 'NONE',  ( -0.9688695217174487784, 0.000000000000000000, -0.2475719085175095702 ) ) ;
#48168 = EDGE_CURVE ( 'NONE', #42404, #35654, #45876, .T. ) ;
#48169 = VERTEX_POINT ( 'NONE', #60174 ) ;
#48170 = CARTESIAN_POINT ( 'NONE',  ( -27.08429572838383947, -2.217805374070538349, 0.5764601019425888984 ) ) ;
#48171 = DIRECTION ( 'NONE',  ( 0.000000000000000000, -0.01356324068817991828, 0.9999080150203990547 ) ) ;
#48172 = CARTESIAN_POINT ( 'NONE',  ( 0.000000000000000000, 0.000000000000000000, 0.000000000000000000 ) ) ;
#48173 = DIRECTION ( 'NONE',  ( 0.000000000000000000, 0.4935949184179261318, -0.8696919319575183716 ) ) ;
#48174 = CARTESIAN_POINT ( 'NONE',  ( 2.241536586108913820, -3.811784405792396857, 6.614789707676452579 ) ) ;
#48175 = B_SPLINE_CURVE_WITH_KNOTS ( 'NONE', 3,
 ( #58118, #38137, #12532, #43450, #58795, #28828, #53466, #13835, #32811, #58446 ),
 .UNSPECIFIED., .F., .F.,
 ( 4, 2, 2, 2, 4 ),
 ( 1.734723475976807094E-18, 0.0006656689435785632762, 0.001331337887157124818, 0.001997006830735686359, 0.002662675774314247901 ),
 .UNSPECIFIED. ) ;
#48176 = CIRCLE ( 'NONE', #22676, 5.000000000000000888 ) ;
#48177 = EDGE_CURVE ( 'NONE', #24790, #43796, #59816, .T. ) ;
#48178 = DIRECTION ( 'NONE',  ( -1.000000000000000000, 0.000000000000000000, 0.000000000000000000 ) ) ;
#48179 = CARTESIAN_POINT ( 'NONE',  ( -37.00000000000000711, -1.791059740004510070, 12.05416472667165273 ) ) ;
#48180 = ORIENTED_EDGE ( 'NONE', *, *, #6269, .F. ) ;
#48181 = ORIENTED_EDGE ( 'NONE', *, *, #59830, .T. ) ;
#48182 = CYLINDRICAL_SURFACE ( 'NONE', #10874, 12.18650000000000055 ) ;
#48183 = ORIENTED_EDGE ( 'NONE', *, *, #33124, .T. ) ;
#48184 = CARTESIAN_POINT ( 'NONE',  ( -22.28694879868232803, 2.586016167700817991, -2.661377239830745367 ) ) ;
#48185 = FACE_OUTER_BOUND ( 'NONE', #15321, .T. ) ;
#48186 = AXIS2_PLACEMENT_3D ( 'NONE', #23633, #64496, #4331 ) ;
#48187 = DIRECTION ( 'NONE',  ( 1.000000000000000000, 0.000000000000000000, 0.000000000000000000 ) ) ;
#48188 = ORIENTED_EDGE ( 'NONE', *, *, #32247, .F. ) ;
#48189 = DIRECTION ( 'NONE',  ( -1.000000000000000000, 0.000000000000000000, -0.000000000000000000 ) ) ;
#48190 =( BOUNDED_SURFACE ( )  B_SPLINE_SURFACE ( 3, 1, ( 
 ( #32969, #33321 ),
 ( #23343, #53283 ),
 ( #18029, #7727 ),
 ( #23025, #43280 ) ),
 .UNSPECIFIED., .F., .F., .F. ) 
 B_SPLINE_SURFACE_WITH_KNOTS ( ( 4, 4 ),
 ( 2, 2 ),
 ( 0.000000000000000000, 1.000000000000000000 ),
 ( 0.000000000000000000, 1.000000000000000000 ),
 .UNSPECIFIED. ) 
 GEOMETRIC_REPRESENTATION_ITEM ( )  RATIONAL_B_SPLINE_SURFACE ( (
 ( 1.000000000000000000, 1.000000000000000000),
 ( 0.9942764183789327692, 0.8450855930916585379),
 ( 0.9942764183789327692, 0.8450855930916585379),
 ( 1.000000000000000000, 1.000000000000000000) ) ) 
 REPRESENTATION_ITEM ( '' )  SURFACE ( )  );
#48191 = FACE_OUTER_BOUND ( 'NONE', #3272, .T. ) ;
#48192 = DIRECTION ( 'NONE',  ( -1.000000000000000000, -0.000000000000000000, -0.000000000000000000 ) ) ;
#48193 = ORIENTED_EDGE ( 'NONE', *, *, #56293, .T. ) ;
#48194 = EDGE_LOOP ( 'NONE', ( #38274, #40055, #64254, #47687 ) ) ;
#48195 = DIRECTION ( 'NONE',  ( -1.000000000000000000, 0.000000000000000000, 0.000000000000000000 ) ) ;
#48196 = EDGE_LOOP ( 'NONE', ( #39425, #29902, #17551, #2464 ) ) ;
#48198 = CARTESIAN_POINT ( 'NONE',  ( 35.00000000000000000, -4.732539170486179003, 11.23004253107769124 ) ) ;
#48197 = AXIS2_PLACEMENT_3D ( 'NONE', #2626, #22889, #53482 ) ;
#48199 = ORIENTED_EDGE ( 'NONE', *, *, #36887, .T. ) ;
#48200 = ORIENTED_EDGE ( 'NONE', *, *, #37912, .F. ) ;
#48201 = CARTESIAN_POINT ( 'NONE',  ( 2.241526690369558317, -7.168108047190856702, 2.627393882429291061 ) ) ;
#48202 = DIRECTION ( 'NONE',  ( 1.000000000000000000, 0.000000000000000000, 0.000000000000000000 ) ) ;
#48203 = AXIS2_PLACEMENT_3D ( 'NONE', #14340, #4389, #65215 ) ;
#48204 = ADVANCED_FACE ( 'NONE', ( #15278 ), #7371, .T. ) ;
#48205 = DIRECTION ( 'NONE',  ( -0.000000000000000000, -0.000000000000000000, -1.000000000000000000 ) ) ;
#48206 = CARTESIAN_POINT ( 'NONE',  ( 0.3401186441510247738, 8.081824149807820490, -9.233880480307224303 ) ) ;
#48207 = CARTESIAN_POINT ( 'NONE',  ( -27.10719052120871098, 2.355164825213508450, -0.1538293304135275597 ) ) ;
#48208 = CARTESIAN_POINT ( 'NONE',  ( 0.2958664285830391316, 11.59077733151255352, 3.984029505266609039 ) ) ;
#48209 = EDGE_CURVE ( 'NONE', #3036, #6695, #64695, .T. ) ;
#48210 = ORIENTED_EDGE ( 'NONE', *, *, #46902, .T. ) ;
#48211 = AXIS2_PLACEMENT_3D ( 'NONE', #4555, #13831, #8535 ) ;
#48212 = CARTESIAN_POINT ( 'NONE',  ( 37.00000000000000711, -9.063649021438894948, 8.146229107149494553 ) ) ;
#48214 = CYLINDRICAL_SURFACE ( 'NONE', #8516, 6.936499999999988120 ) ;
#48213 = VECTOR ( 'NONE', #59475, 1000.000000000000000 ) ;
#48215 = DIRECTION ( 'NONE',  ( -1.000000000000000000, -0.000000000000000000, -0.000000000000000000 ) ) ;
#48216 = DIRECTION ( 'NONE',  ( 1.000000000000000000, 0.000000000000000000, 0.000000000000000000 ) ) ;
#48217 = LINE ( 'NONE', #8275, #42353 ) ;
#48218 = AXIS2_PLACEMENT_3D ( 'NONE', #36646, #35964, #20704 ) ;
#48219 = DIRECTION ( 'NONE',  ( 1.000000000000000000, 0.000000000000000000, 0.000000000000000000 ) ) ;
#48220 = DIRECTION ( 'NONE',  ( 0.000000000000000000, 0.01356324068817992522, -0.9999080150203990547 ) ) ;
#48221 = CARTESIAN_POINT ( 'NONE',  ( 0.2958664285830437390, -11.59077733151253398, -3.984029505266682758 ) ) ;
#48222 = EDGE_CURVE ( 'NONE', #37848, #27274, #42376, .T. ) ;
#48223 = CARTESIAN_POINT ( 'NONE',  ( -27.45775109278351067, -10.51123867646838050, -8.471355351200609007 ) ) ;
#48224 = VECTOR ( 'NONE', #15428, 1000.000000000000000 ) ;
#48225 = ORIENTED_EDGE ( 'NONE', *, *, #57490, .F. ) ;
#48226 = DIRECTION ( 'NONE',  ( 0.000000000000000000, 0.01356324068817992175, -0.9999080150203990547 ) ) ;
#48227 = ORIENTED_EDGE ( 'NONE', *, *, #61812, .F. ) ;
#48228 = CARTESIAN_POINT ( 'NONE',  ( 5.516018279890452902, 0.002104829434640673614, -0.006440244342253036158 ) ) ;
#48229 = CARTESIAN_POINT ( 'NONE',  ( -19.56743653832046803, -28.99999999999999645, -4.999999999999997335 ) ) ;
#48230 = AXIS2_PLACEMENT_3D ( 'NONE', #39755, #60355, #24135 ) ;
#48231 = CARTESIAN_POINT ( 'NONE',  ( 35.00000000000000000, 4.705694406421931860E-17, -3.469127814946512892E-15 ) ) ;
#48232 = CARTESIAN_POINT ( 'NONE',  ( -35.04643116707788408, 0.002453861112619928897, 0.01193867652719490802 ) ) ;
#48233 = CARTESIAN_POINT ( 'NONE',  ( 2.440552418640494992, -4.797131306497530723, -6.024135401262425304 ) ) ;
#48234 = ADVANCED_FACE ( 'NONE', ( #24940 ), #656, .F. ) ;
#48235 = ORIENTED_EDGE ( 'NONE', *, *, #61088, .T. ) ;
#48236 = CARTESIAN_POINT ( 'NONE',  ( 1.014383007554942262, 10.59286224865790338, -6.628652139012797484 ) ) ;
#48237 = CARTESIAN_POINT ( 'NONE',  ( 22.57855258442564761, -4.427776684447072952, 12.75322679295976691 ) ) ;
#48238 = DIRECTION ( 'NONE',  ( 0.9486832985018464059, 3.872673197958701185E-17, 0.3162277646628405270 ) ) ;
#48239 = CARTESIAN_POINT ( 'NONE',  ( 22.00000000000000711, -20.00000000000000000, 2.449293598294706907E-15 ) ) ;
#48240 = ADVANCED_FACE ( 'NONE', ( #61471 ), #1938, .F. ) ;
#48241 = VECTOR ( 'NONE', #45214, 1000.000000000000000 ) ;
#48242 = CARTESIAN_POINT ( 'NONE',  ( -22.38932658256919339, -1.810630688302289348, 3.587092141214295093 ) ) ;
#48243 = EDGE_LOOP ( 'NONE', ( #41795, #54740, #38230, #34314 ) ) ;
#48244 = CARTESIAN_POINT ( 'NONE',  ( 3.152665057736049103, -0.4801242025610908959, -7.923639299008895520 ) ) ;
#48245 = CARTESIAN_POINT ( 'NONE',  ( 1.194176325881338263, -8.457794872459055924, -9.279760592562180221 ) ) ;
#48246 = CARTESIAN_POINT ( 'NONE',  ( 2.280717697723837922, -3.958470850374266270, -6.543326285614674553 ) ) ;
#48247 = AXIS2_PLACEMENT_3D ( 'NONE', #698, #55892, #8447 ) ;
#48248 = AXIS2_PLACEMENT_3D ( 'NONE', #31321, #51622, #27548 ) ;
#48249 = EDGE_CURVE ( 'NONE', #56931, #3747, #20104, .T. ) ;
#48250 = CIRCLE ( 'NONE', #28059, 12.18650000000000055 ) ;
#48251 = ORIENTED_EDGE ( 'NONE', *, *, #23159, .F. ) ;
#48252 = CARTESIAN_POINT ( 'NONE',  ( 8.937200413559445167, 4.820175079577382782, -10.99560042399104098 ) ) ;
#48253 = EDGE_CURVE ( 'NONE', #39576, #52203, #52825, .T. ) ;
#48254 = EDGE_LOOP ( 'NONE', ( #4238, #61381 ) ) ;
#48255 = CARTESIAN_POINT ( 'NONE',  ( 26.25882823526612597, -13.04980996862088638, 3.460358416528618530 ) ) ;
#48257 = VECTOR ( 'NONE', #25805, 1000.000000000000000 ) ;
#48256 = CARTESIAN_POINT ( 'NONE',  ( 35.00000000000000000, 4.705694406421931860E-17, -3.469127814946512892E-15 ) ) ;
#48258 = CARTESIAN_POINT ( 'NONE',  ( 37.00843563923471180, -2.297594674915183877, 20.79457751400812882 ) ) ;
#48259 = DIRECTION ( 'NONE',  ( -1.000000000000000000, -0.000000000000000000, -0.000000000000000000 ) ) ;
#48260 = EDGE_CURVE ( 'NONE', #55068, #11977, #977, .T. ) ;
#48261 = DIRECTION ( 'NONE',  ( -1.000000000000000000, 0.000000000000000000, 0.000000000000000000 ) ) ;
#48262 = VERTEX_POINT ( 'NONE', #16599 ) ;
#48263 = AXIS2_PLACEMENT_3D ( 'NONE', #17770, #38361, #44022 ) ;
#48264 = ORIENTED_EDGE ( 'NONE', *, *, #21455, .F. ) ;
#48265 = ORIENTED_EDGE ( 'NONE', *, *, #14745, .F. ) ;
#48266 = CARTESIAN_POINT ( 'NONE',  ( -10.00000000000000178, 0.000000000000000000, 0.000000000000000000 ) ) ;
#48267 = VECTOR ( 'NONE', #16784, 1000.000000000000000 ) ;
#48268 = ORIENTED_EDGE ( 'NONE', *, *, #20451, .F. ) ;
#48269 = DIRECTION ( 'NONE',  ( 1.000000000000000000, 0.000000000000000000, 0.000000000000000000 ) ) ;
#48270 = CARTESIAN_POINT ( 'NONE',  ( -22.31328051695926007, -0.2528478350593797996, -3.781397440874599614 ) ) ;
#48271 = VERTEX_POINT ( 'NONE', #52520 ) ;
#48272 = DIRECTION ( 'NONE',  ( 0.000000000000000000, 1.000000000000000000, 0.000000000000000000 ) ) ;
#48273 = AXIS2_PLACEMENT_3D ( 'NONE', #36613, #47269, #11341 ) ;
#48274 = CARTESIAN_POINT ( 'NONE',  ( -37.00000000000000711, 4.732539170486427693, -11.23004253107759176 ) ) ;
#48275 = CARTESIAN_POINT ( 'NONE',  ( 35.00000000000000000, 6.102719229070673990, -10.54834585426222304 ) ) ;
#48276 = EDGE_LOOP ( 'NONE', ( #7424, #29667, #10670, #11287 ) ) ;
#48277 = ORIENTED_EDGE ( 'NONE', *, *, #26494, .F. ) ;
#48278 = DIRECTION ( 'NONE',  ( 0.000000000000000000, -0.01356324068817999114, 0.9999080150203989437 ) ) ;
#48279 = ORIENTED_EDGE ( 'NONE', *, *, #47715, .T. ) ;
#48280 = DIRECTION ( 'NONE',  ( 0.000000000000000000, 0.000000000000000000, 1.000000000000000000 ) ) ;
#48281 = VERTEX_POINT ( 'NONE', #26900 ) ;
#48282 = CARTESIAN_POINT ( 'NONE',  ( 2.247206125382828379, 3.717496781928092631, 6.670391186503657366 ) ) ;
#48283 = CARTESIAN_POINT ( 'NONE',  ( 15.63877597542558107, -34.91516792956247173, -5.826750174076742006 ) ) ;
#48284 = FACE_OUTER_BOUND ( 'NONE', #18061, .T. ) ;
#48285 = CIRCLE ( 'NONE', #22776, 2.899999999999994582 ) ;
#48286 = CARTESIAN_POINT ( 'NONE',  ( 35.00000000000000000, -1.791059740004336875, 12.05416472667166694 ) ) ;
#48287 = LINE ( 'NONE', #28620, #8562 ) ;
#48288 = CARTESIAN_POINT ( 'NONE',  ( 1.462291587750105260, -0.6330131614655301053, 12.62932306616591482 ) ) ;
#48289 = CARTESIAN_POINT ( 'NONE',  ( -27.47719885066990742, -11.55823979936119450, -3.277255182065942574 ) ) ;
#48290 = ORIENTED_EDGE ( 'NONE', *, *, #4045, .F. ) ;
#48291 = CARTESIAN_POINT ( 'NONE',  ( 0.4613984246114875565, 10.80075367333622260, 5.909164750631071605 ) ) ;
#48292 = EDGE_CURVE ( 'NONE', #32746, #64838, #50285, .T. ) ;
#48293 = VERTEX_POINT ( 'NONE', #56856 ) ;
#48294 = PLANE ( 'NONE',  #4114 ) ;
#48295 = CARTESIAN_POINT ( 'NONE',  ( -35.00000000000000000, 11.65554240571059275, -1.456211999474221086 ) ) ;
#48296 = EDGE_LOOP ( 'NONE', ( #2125, #3511, #51229, #24143 ) ) ;
#48298 = AXIS2_PLACEMENT_3D ( 'NONE', #37410, #858, #41403 ) ;
#48297 = CARTESIAN_POINT ( 'NONE',  ( 0.000000000000000000, 6.662861565602072211, 1.421313227905651289 ) ) ;
#48299 = FACE_OUTER_BOUND ( 'NONE', #58384, .T. ) ;
#48300 = CARTESIAN_POINT ( 'NONE',  ( 0.2915757698887310734, -2.339174865979208207, -12.02962099476165925 ) ) ;
#48301 = ORIENTED_EDGE ( 'NONE', *, *, #23379, .T. ) ;
#48302 = VERTEX_POINT ( 'NONE', #1647 ) ;
#48303 = CARTESIAN_POINT ( 'NONE',  ( 2.491965175174603697, -6.787433375639562172, -3.673871285745604620 ) ) ;
#48304 = ORIENTED_EDGE ( 'NONE', *, *, #47515, .T. ) ;
#48305 = FACE_OUTER_BOUND ( 'NONE', #39638, .T. ) ;
#48306 = CARTESIAN_POINT ( 'NONE',  ( 35.00000000000000000, -11.68758509253247091, 1.171570255487570655 ) ) ;
#48307 = CARTESIAN_POINT ( 'NONE',  ( 2.241528039335009215, -1.310213701658539343, -7.521191296022434081 ) ) ;
#48308 = CARTESIAN_POINT ( 'NONE',  ( -22.23402523511428086, 0.6266381416564609230, 3.496364702451501216 ) ) ;
#48309 = CARTESIAN_POINT ( 'NONE',  ( -17.83799997667700055, -8.694692931027089955, 8.293044525567449199 ) ) ;
#48310 = ADVANCED_FACE ( 'NONE', ( #21916 ), #47837, .T. ) ;
#48311 = ORIENTED_EDGE ( 'NONE', *, *, #50128, .T. ) ;
#48312 = DIRECTION ( 'NONE',  ( 1.000000000000000000, 0.000000000000000000, -0.000000000000000000 ) ) ;
#48313 = EDGE_CURVE ( 'NONE', #34842, #15906, #37855, .T. ) ;
#48314 = CIRCLE ( 'NONE', #19626, 12.18649999999999878 ) ;
#48315 = CYLINDRICAL_SURFACE ( 'NONE', #26523, 2.899999999999994582 ) ;
#48316 = CARTESIAN_POINT ( 'NONE',  ( 22.22325956648730383, 13.44453809516076248, -1.271158126962866897 ) ) ;
#48317 = CARTESIAN_POINT ( 'NONE',  ( -27.08429572838383947, -0.6096735944848084010, 2.208905845566022208 ) ) ;
#48318 = DIRECTION ( 'NONE',  ( 1.000000000000000000, 0.000000000000000000, 0.000000000000000000 ) ) ;
#48319 = CARTESIAN_POINT ( 'NONE',  ( 3.100650473569707355, 5.429218121582431777, -5.767490999797057150 ) ) ;
#48320 = ADVANCED_FACE ( 'NONE', ( #57497 ), #42691, .F. ) ;
#48321 = CIRCLE ( 'NONE', #43024, 2.899999999999995026 ) ;
#48322 = ORIENTED_EDGE ( 'NONE', *, *, #45729, .T. ) ;
#48323 = CARTESIAN_POINT ( 'NONE',  ( 2.253265082352433168, -0.1282654837135236425, 7.637296367516834827 ) ) ;
#48324 = ORIENTED_EDGE ( 'NONE', *, *, #14834, .F. ) ;
#48325 = CARTESIAN_POINT ( 'NONE',  ( 0.2671309869109499413, 1.966882337881849407, -12.08782215308009711 ) ) ;
#48326 = DIRECTION ( 'NONE',  ( 1.000000000000000000, -0.000000000000000000, -0.000000000000000000 ) ) ;
#48327 = CARTESIAN_POINT ( 'NONE',  ( 1.719304012340653998, -9.242227816403676854, -8.755325027797448811 ) ) ;
#48328 = ORIENTED_EDGE ( 'NONE', *, *, #15262, .T. ) ;
#48329 = CARTESIAN_POINT ( 'NONE',  ( 2.241352910868908754, 4.843133558968205854, -5.901537464758406237 ) ) ;
#48330 = ORIENTED_EDGE ( 'NONE', *, *, #65790, .F. ) ;
#48331 = STYLED_ITEM ( 'NONE', ( #49790 ), #4012 ) ;
#48332 = DIRECTION ( 'NONE',  ( -1.000000000000000000, 0.000000000000000000, 0.000000000000000000 ) ) ;
#48333 = EDGE_LOOP ( 'NONE', ( #45895, #15738, #51427, #49258 ) ) ;
#48334 = EDGE_LOOP ( 'NONE', ( #11615, #12201, #52236, #53641 ) ) ;
#48335 = CARTESIAN_POINT ( 'NONE',  ( -10.71044032080790309, -9.069509059426344777, -7.875876655957959827 ) ) ;
#48336 = ADVANCED_FACE ( 'NONE', ( #57241 ), #11668, .T. ) ;
#48337 = DIRECTION ( 'NONE',  ( -1.000000000000000000, 0.000000000000000000, 0.000000000000000000 ) ) ;
#48338 = ORIENTED_EDGE ( 'NONE', *, *, #31160, .T. ) ;
#48339 = CARTESIAN_POINT ( 'NONE',  ( -22.27706485742869091, -2.154081322712202873, -2.985151051101508468 ) ) ;
#48340 = CARTESIAN_POINT ( 'NONE',  ( 3.128546914509915844, 2.910026699185261467, 13.18839757576990479 ) ) ;
#48341 = DIRECTION ( 'NONE',  ( 1.000000000000000000, 0.000000000000000000, -0.000000000000000000 ) ) ;
#48342 = CARTESIAN_POINT ( 'NONE',  ( -35.00000000000000000, 0.000000000000000000, 0.000000000000000000 ) ) ;
#48343 = ORIENTED_EDGE ( 'NONE', *, *, #21145, .F. ) ;
#48344 = CIRCLE ( 'NONE', #19665, 12.18649999999999878 ) ;
#48345 = CARTESIAN_POINT ( 'NONE',  ( 2.000000000000001776, 0.08317740279942427428, -7.499538753794372070 ) ) ;
#48346 = CARTESIAN_POINT ( 'NONE',  ( 16.10228578084485562, -34.99999999976227372, 4.568518662555822729 ) ) ;
#48347 = CARTESIAN_POINT ( 'NONE',  ( 2.241317068080777908, -1.415707718487463351, -7.501982551779205366 ) ) ;
#48349 = ORIENTED_EDGE ( 'NONE', *, *, #65732, .T. ) ;
#48348 = CYLINDRICAL_SURFACE ( 'NONE', #60564, 12.74999999999999822 ) ;
#48350 = CARTESIAN_POINT ( 'NONE',  ( 5.514970785353741078, -0.004233694591582531745, 0.002093325033904006385 ) ) ;
#48351 = ORIENTED_EDGE ( 'NONE', *, *, #1531, .F. ) ;
#48352 = DIRECTION ( 'NONE',  ( -1.000000000000000000, 0.000000000000000000, 0.000000000000000000 ) ) ;
#48353 = ORIENTED_EDGE ( 'NONE', *, *, #26868, .T. ) ;
#48354 = DIRECTION ( 'NONE',  ( 0.000000000000000000, 0.000000000000000000, 1.000000000000000000 ) ) ;
#48355 = CARTESIAN_POINT ( 'NONE',  ( 0.2801149460245144773, 4.005169813315260008, -11.57793225195133147 ) ) ;
#48356 = VECTOR ( 'NONE', #10433, 1000.000000000000000 ) ;
#48357 = CYLINDRICAL_SURFACE ( 'NONE', #4309, 12.75000000000000178 ) ;
#48358 = CARTESIAN_POINT ( 'NONE',  ( -2.532614230583022152, 11.30437021680556242, 4.026315189028233377 ) ) ;
#48359 = CARTESIAN_POINT ( 'NONE',  ( 0.2653519789438770760, -11.50012635727058452, 4.209148152332875981 ) ) ;
#48360 = CARTESIAN_POINT ( 'NONE',  ( 0.2646305136544065406, 12.03696649559617882, -2.256625640822194079 ) ) ;
#48361 = CARTESIAN_POINT ( 'NONE',  ( 2.241449424704146320, -5.808712090826644747, 4.954182807723320536 ) ) ;
#48362 = ADVANCED_FACE ( 'NONE', ( #16989 ), #37267, .T. ) ;
#48363 = VERTEX_POINT ( 'NONE', #52895 ) ;
#48364 = CARTESIAN_POINT ( 'NONE',  ( 5.530133899448235191, -0.003876417824003439323, -0.01550764871776274222 ) ) ;
#48365 = VERTEX_POINT ( 'NONE', #58907 ) ;
#48366 = EDGE_CURVE ( 'NONE', #51562, #26969, #33906, .T. ) ;
#48367 = ORIENTED_EDGE ( 'NONE', *, *, #23363, .T. ) ;
#48368 = CARTESIAN_POINT ( 'NONE',  ( 1.547277799339609405, 1.534072017332309246, -12.58038279313770680 ) ) ;
#48369 = DIRECTION ( 'NONE',  ( 0.000000000000000000, -1.000000000000000000, 0.000000000000000000 ) ) ;
#48370 = CARTESIAN_POINT ( 'NONE',  ( -37.00000000000000711, -12.02534193257724304, 4.237174932027182095 ) ) ;
#48371 = CARTESIAN_POINT ( 'NONE',  ( 0.3610902822527150557, -10.49957835860567279, 6.364812822043123930 ) ) ;
#48372 = CARTESIAN_POINT ( 'NONE',  ( -27.08429572838383947, -2.208905845566027537, -0.6096735944848257205 ) ) ;
#48373 = LINE ( 'NONE', #13101, #15058 ) ;
#48374 = CIRCLE ( 'NONE', #19687, 12.18650000000000411 ) ;
#48375 = EDGE_CURVE ( 'NONE', #13554, #32930, #54217, .T. ) ;
#48376 = CARTESIAN_POINT ( 'NONE',  ( -37.00000000000000711, -9.752226076388847531, -6.547236723514122225 ) ) ;
#48377 =( BOUNDED_SURFACE ( )  B_SPLINE_SURFACE ( 3, 1, ( 
 ( #59951, #48661 ),
 ( #14371, #63937 ),
 ( #38992, #43318 ),
 ( #43648, #64266 ) ),
 .UNSPECIFIED., .F., .F., .T. ) 
 B_SPLINE_SURFACE_WITH_KNOTS ( ( 4, 4 ),
 ( 2, 2 ),
 ( 0.000000000000000000, 1.000000000000000000 ),
 ( 0.000000000000000000, 1.000000000000000000 ),
 .UNSPECIFIED. ) 
 GEOMETRIC_REPRESENTATION_ITEM ( )  RATIONAL_B_SPLINE_SURFACE ( (
 ( 1.000000000000000000, 1.000000000000000000),
 ( 0.9942764183789327692, 0.8450855930916585379),
 ( 0.9942764183789327692, 0.8450855930916585379),
 ( 1.000000000000000000, 1.000000000000000000) ) ) 
 REPRESENTATION_ITEM ( '' )  SURFACE ( )  );
#48378 = VERTEX_POINT ( 'NONE', #59211 ) ;
#48379 = DIRECTION ( 'NONE',  ( 0.000000000000000000, 0.000000000000000000, 1.000000000000000000 ) ) ;
#48380 = DIRECTION ( 'NONE',  ( 1.000000000000000000, 0.000000000000000000, 0.000000000000000000 ) ) ;
#48381 = DIRECTION ( 'NONE',  ( 0.000000000000000000, -0.01356324068818000848, 0.9999080150203990547 ) ) ;
#48382 = EDGE_CURVE ( 'NONE', #8260, #10101, #35524, .T. ) ;
#48383 =( GEOMETRIC_REPRESENTATION_CONTEXT ( 3 ) GLOBAL_UNCERTAINTY_ASSIGNED_CONTEXT ( ( #27268 ) ) GLOBAL_UNIT_ASSIGNED_CONTEXT ( ( #60094, #40118, #40450 ) ) REPRESENTATION_CONTEXT ( 'NONE', 'WORKASPACE' ) );
#48384 = CARTESIAN_POINT ( 'NONE',  ( 2.000000000000001776, 3.937687286050817193, 6.383151168292468647 ) ) ;
#48385 = DIRECTION ( 'NONE',  ( 0.000000000000000000, -0.4935949184179136418, 0.8696919319575254770 ) ) ;
#48386 = AXIS2_PLACEMENT_3D ( 'NONE', #5354, #35904, #41899 ) ;
#48387 =( BOUNDED_SURFACE ( )  B_SPLINE_SURFACE ( 3, 1, ( 
 ( #54910, #29622 ),
 ( #56214, #5707 ),
 ( #24659, #63091 ),
 ( #33493, #6036 ) ),
 .UNSPECIFIED., .F., .F., .F. ) 
 B_SPLINE_SURFACE_WITH_KNOTS ( ( 4, 4 ),
 ( 2, 2 ),
 ( 0.000000000000000000, 1.000000000000000000 ),
 ( 0.000000000000000000, 1.000000000000000000 ),
 .UNSPECIFIED. ) 
 GEOMETRIC_REPRESENTATION_ITEM ( )  RATIONAL_B_SPLINE_SURFACE ( (
 ( 1.000000000000000000, 1.000000000000000000),
 ( 0.6933888150995267674, 0.9895912004443193632),
 ( 0.6933888150995267674, 0.9895912004443193632),
 ( 1.000000000000000000, 1.000000000000000000) ) ) 
 REPRESENTATION_ITEM ( '' )  SURFACE ( )  );
#48388 = DIRECTION ( 'NONE',  ( 0.000000000000000000, -0.01356324068817991307, 0.9999080150203990547 ) ) ;
#48389 = CARTESIAN_POINT ( 'NONE',  ( 5.536195898058073439, 0.001726268814999830630, -0.008323005098840517008 ) ) ;
#48390 = ORIENTED_EDGE ( 'NONE', *, *, #14629, .F. ) ;
#48391 = CARTESIAN_POINT ( 'NONE',  ( 0.000000000000000000, 0.000000000000000000, 0.000000000000000000 ) ) ;
#48392 = FACE_OUTER_BOUND ( 'NONE', #11225, .T. ) ;
#48393 = CARTESIAN_POINT ( 'NONE',  ( 5.530133899448235191, -0.01293763278443415231, 0.009387834778845282821 ) ) ;
#48394 = CARTESIAN_POINT ( 'NONE',  ( 35.00000000000000000, 4.705694406421931860E-17, -3.469127814946512892E-15 ) ) ;
#48395 = CARTESIAN_POINT ( 'NONE',  ( 1.452237505248555660, -6.833827325205244385, -10.65201107290474702 ) ) ;
#48396 = VERTEX_POINT ( 'NONE', #64191 ) ;
#48397 = CARTESIAN_POINT ( 'NONE',  ( 19.28625800530496903, -1.699513388191772778, 11.87904264843580471 ) ) ;
#48398 = CARTESIAN_POINT ( 'NONE',  ( 0.3053067050349199674, 9.241336250185357315, 8.055646999028040156 ) ) ;
#48399 = ORIENTED_EDGE ( 'NONE', *, *, #7271, .T. ) ;
#48400 = DIRECTION ( 'NONE',  ( -1.000000000000000000, 0.000000000000000000, 0.000000000000000000 ) ) ;
#48401 = CARTESIAN_POINT ( 'NONE',  ( 1.937114397841932290, 12.33981801388262589, -3.531416430611173052 ) ) ;
#48402 = VERTEX_POINT ( 'NONE', #13631 ) ;
#48403 = ORIENTED_EDGE ( 'NONE', *, *, #61102, .T. ) ;
#48404 = CARTESIAN_POINT ( 'NONE',  ( 2.000000000000001776, -1.145812388885151023, 6.715725538143585638 ) ) ;
#48405 = EDGE_CURVE ( 'NONE', #58225, #48073, #43065, .T. ) ;
#48406 = ORIENTED_EDGE ( 'NONE', *, *, #6526, .T. ) ;
#48407 = CYLINDRICAL_SURFACE ( 'NONE', #60987, 4.999999999999999112 ) ;
#48408 = CARTESIAN_POINT ( 'NONE',  ( 35.00000000000000000, -10.84030624090611106, -6.711949091238110121 ) ) ;
#48409 = CARTESIAN_POINT ( 'NONE',  ( 2.241451721903216399, 7.528807736569466336, -1.265761656830125315 ) ) ;
#48410 = CARTESIAN_POINT ( 'NONE',  ( 2.273267844204865273, -7.553702825375860463, -1.178226273333022212 ) ) ;
#48411 = CARTESIAN_POINT ( 'NONE',  ( 35.00000000000000000, 4.705694406421931860E-17, -3.469127814946512892E-15 ) ) ;
#48412 = DIRECTION ( 'NONE',  ( 0.000000000000000000, 0.7617968321374855023, 0.6478160128811972784 ) ) ;
#48414 = ORIENTED_EDGE ( 'NONE', *, *, #12249, .T. ) ;
#48413 = CARTESIAN_POINT ( 'NONE',  ( 1.194176325881340262, 0.5141316333311244380, 12.54527478469375801 ) ) ;
#48415 = CARTESIAN_POINT ( 'NONE',  ( 37.00000000000000711, 8.927548052240892318, -8.295159312811890118 ) ) ;
#48416 = VERTEX_POINT ( 'NONE', #42564 ) ;
#48417 = CARTESIAN_POINT ( 'NONE',  ( 0.2650492433740053722, 10.54996000109284005, -6.218175523534182680 ) ) ;
#48418 = VERTEX_POINT ( 'NONE', #48274 ) ;
#48419 = B_SPLINE_CURVE_WITH_KNOTS ( 'NONE', 3,
 ( #62627, #47048, #61658, #1506, #12103, #26106, #16114 ),
 .UNSPECIFIED., .F., .F.,
 ( 4, 3, 4 ),
 ( 0.000000000000000000, 0.001700533616330536252, 0.005002426799375401731 ),
 .UNSPECIFIED. ) ;
#48420 = ORIENTED_EDGE ( 'NONE', *, *, #49712, .F. ) ;
#48421 = SHAPE_DEFINITION_REPRESENTATION ( #43959, #39018 ) ;
#48422 = CARTESIAN_POINT ( 'NONE',  ( -25.01550185040246532, 11.25207016924878367, 7.460967861423081438 ) ) ;
#48423 = CARTESIAN_POINT ( 'NONE',  ( -12.36714175812590355, -29.91041276695339590, 8.471522614801738627 ) ) ;
#48424 = DIRECTION ( 'NONE',  ( 0.4622435816439406930, 0.000000000000000000, -0.8867529933577791290 ) ) ;
#48425 = EDGE_CURVE ( 'NONE', #7386, #13124, #31808, .T. ) ;
#48426 = DIRECTION ( 'NONE',  ( -1.000000000000000000, 0.000000000000000000, 0.000000000000000000 ) ) ;
#48427 = CIRCLE ( 'NONE', #24014, 5.000000000000000888 ) ;
#48428 = DIRECTION ( 'NONE',  ( 0.000000000000000000, 0.9105187689795940509, -0.4134677391718546424 ) ) ;
#48429 = ORIENTED_EDGE ( 'NONE', *, *, #20601, .T. ) ;
#48430 = CIRCLE ( 'NONE', #62177, 7.499999999999988454 ) ;
#48431 = CARTESIAN_POINT ( 'NONE',  ( -22.27721688985630522, -0.6032462375556635337, -3.631967556481321857 ) ) ;
#48432 = ADVANCED_FACE ( 'NONE', ( #22981 ), #62867, .T. ) ;
#48433 = CARTESIAN_POINT ( 'NONE',  ( -22.59969328935894239, -4.339503524536120871, 1.672297795813938892 ) ) ;
#48434 = CARTESIAN_POINT ( 'NONE',  ( 5.536195898058073439, -0.007230647766619658148, 0.004468797463753859146 ) ) ;
#48435 = VERTEX_POINT ( 'NONE', #43233 ) ;
#48436 = DIRECTION ( 'NONE',  ( 0.000000000000000000, -0.01356324068817998940, 0.9999080150203990547 ) ) ;
#48437 = ADVANCED_FACE ( 'NONE', ( #23298 ), #58565, .T. ) ;
#48438 = EDGE_LOOP ( 'NONE', ( #31843, #17400, #38976, #22883 ) ) ;
#48439 = CARTESIAN_POINT ( 'NONE',  ( 29.19808783025697707, -7.805332973316843059, 11.01506521398892069 ) ) ;
#48440 = CARTESIAN_POINT ( 'NONE',  ( 0.2676618633000451553, -10.52491907319757125, -6.262131165853840109 ) ) ;
#48441 = DIRECTION ( 'NONE',  ( 1.000000000000000000, 0.000000000000000000, 0.000000000000000000 ) ) ;
#48442 = AXIS2_PLACEMENT_3D ( 'NONE', #42327, #42021, #1809 ) ;
#48443 = CARTESIAN_POINT ( 'NONE',  ( 37.00000000000000711, -7.817610399097575602, -8.766823244861962294 ) ) ;
#48444 = DIRECTION ( 'NONE',  ( 0.000000000000000000, -0.6051742151937715697, 0.7960930657056388693 ) ) ;
#48445 = CARTESIAN_POINT ( 'NONE',  ( -29.68541646480307250, -1.416020129149132334, 13.42553116244733680 ) ) ;
#48446 = EDGE_CURVE ( 'NONE', #13869, #21040, #5256, .T. ) ;
#48447 = CARTESIAN_POINT ( 'NONE',  ( 36.00000000000000711, 9.196955404009292678, -8.830544224262981245 ) ) ;
#48448 = ORIENTED_EDGE ( 'NONE', *, *, #34116, .T. ) ;
#48449 = CARTESIAN_POINT ( 'NONE',  ( -25.00000000000000355, -3.797884998337192286, -24.99999999999999289 ) ) ;
#48450 = EDGE_CURVE ( 'NONE', #53140, #37516, #3033, .T. ) ;
#48451 = ORIENTED_EDGE ( 'NONE', *, *, #46756, .T. ) ;
#48452 = FACE_OUTER_BOUND ( 'NONE', #39591, .T. ) ;
#48453 = CARTESIAN_POINT ( 'NONE',  ( 2.268878695253354838, -3.949362208797108753, 6.544222817598203790 ) ) ;
#48454 = CARTESIAN_POINT ( 'NONE',  ( -37.00000000000000711, -1.738225594539907659, -12.63095688309031139 ) ) ;
#48455 = ORIENTED_EDGE ( 'NONE', *, *, #37814, .T. ) ;
#48456 = FACE_OUTER_BOUND ( 'NONE', #10509, .T. ) ;
#48457 = EDGE_CURVE ( 'NONE', #31241, #451, #59403, .T. ) ;
#48458 = ORIENTED_EDGE ( 'NONE', *, *, #24661, .T. ) ;
#48459 = CARTESIAN_POINT ( 'NONE',  ( 0.2648978790185602672, 7.769924372105329269, -9.465406350830530613 ) ) ;
#48460 = DIRECTION ( 'NONE',  ( -1.000000000000000000, 0.000000000000000000, 0.000000000000000000 ) ) ;
#48461 = EDGE_CURVE ( 'NONE', #9767, #46346, #44576, .T. ) ;
#48462 = CARTESIAN_POINT ( 'NONE',  ( -27.10719052120871098, -2.116547233941210138, -1.044362304621491377 ) ) ;
#48463 = CARTESIAN_POINT ( 'NONE',  ( 2.524535260912887491, -5.135322114975942043, -5.776056274541106816 ) ) ;
#48464 = VERTEX_POINT ( 'NONE', #43908 ) ;
#48465 = CARTESIAN_POINT ( 'NONE',  ( 0.2651627682582926027, -6.199212018117366441, -10.56115808354089225 ) ) ;
#48466 = CARTESIAN_POINT ( 'NONE',  ( -24.42101984568203932, -0.3620223918248232642, 4.276292373951984693 ) ) ;
#48467 = CARTESIAN_POINT ( 'NONE',  ( 35.00000000000000000, 4.705694406421931860E-17, -3.469127814946512892E-15 ) ) ;
#48468 = CARTESIAN_POINT ( 'NONE',  ( 2.889800649504073782, -5.728825117897722308, 2.156828754871448872 ) ) ;
#48469 = CARTESIAN_POINT ( 'NONE',  ( 2.589278595513194503, -3.664724287895325006, 6.829211973730497931 ) ) ;
#48470 = CARTESIAN_POINT ( 'NONE',  ( 2.000000000000001776, 3.073484823194340354, 6.841322316745045207 ) ) ;
#48471 = ORIENTED_EDGE ( 'NONE', *, *, #10221, .T. ) ;
#48472 = CYLINDRICAL_SURFACE ( 'NONE', #2588, 4.999999999999999112 ) ;
#48473 = LINE ( 'NONE', #17873, #1025 ) ;
#48474 = VERTEX_POINT ( 'NONE', #64497 ) ;
#48475 = CARTESIAN_POINT ( 'NONE',  ( -9.522095209522213111, -2.893068788992850138, -13.18738133420595027 ) ) ;
#48476 = DIRECTION ( 'NONE',  ( -0.3939253465568943735, -0.7910971609033234930, 0.4679616473074815763 ) ) ;
#48477 = CARTESIAN_POINT ( 'NONE',  ( -35.00000000000000000, -5.927257550915394191, 10.64792938439753378 ) ) ;
#48478 = CARTESIAN_POINT ( 'NONE',  ( 1.452237505248552996, 11.24427360515650420, -5.807998527925775534 ) ) ;
#48479 = CARTESIAN_POINT ( 'NONE',  ( 0.3164563675027611267, -11.43920928915628110, 4.419430877662304802 ) ) ;
#48480 = EDGE_CURVE ( 'NONE', #3315, #52686, #60539, .T. ) ;
#48481 = ORIENTED_EDGE ( 'NONE', *, *, #9527, .F. ) ;
#48482 = CARTESIAN_POINT ( 'NONE',  ( 35.00000000000000000, -3.307597835713330880, -12.31350058095522115 ) ) ;
#48483 = VERTEX_POINT ( 'NONE', #24272 ) ;
#48484 = CARTESIAN_POINT ( 'NONE',  ( 1.719304012338199517, 0.000000000000000000, 0.000000000000000000 ) ) ;
#48485 = CARTESIAN_POINT ( 'NONE',  ( 2.835339799623984192, 7.466040501142062524, -2.367573116406901601 ) ) ;
#48486 = CARTESIAN_POINT ( 'NONE',  ( 2.589278595513869963, -4.794929105510921552, 6.089088204449140562 ) ) ;
#48487 = DIRECTION ( 'NONE',  ( 0.000000000000000000, 0.000000000000000000, 1.000000000000000000 ) ) ;
#48488 = DIRECTION ( 'NONE',  ( 0.000000000000000000, 0.9970832820307036215, 0.07632122047556837152 ) ) ;
#48489 = CARTESIAN_POINT ( 'NONE',  ( 2.257661810676420355, 7.546014018371154819, 1.193649218120614641 ) ) ;
#48490 = CARTESIAN_POINT ( 'NONE',  ( 5.515539859299206427, -0.006049968793488818240, 0.0001942659352251156096 ) ) ;
#48491 = ORIENTED_EDGE ( 'NONE', *, *, #19638, .F. ) ;
#48492 = VERTEX_POINT ( 'NONE', #3706 ) ;
#48493 = EDGE_CURVE ( 'NONE', #53238, #22366, #5301, .T. ) ;
#48494 = SURFACE_STYLE_FILL_AREA ( #44142 ) ;
#48495 = ORIENTED_EDGE ( 'NONE', *, *, #10821, .T. ) ;
#48496 = PRESENTATION_STYLE_ASSIGNMENT (( #18231 ) ) ;
#48497 = CARTESIAN_POINT ( 'NONE',  ( -22.28073302975501235, 2.595086548180011832, -2.626377654649338922 ) ) ;
#48498 = CARTESIAN_POINT ( 'NONE',  ( 2.000000000000001776, -3.937687286050851831, 6.383151168292441113 ) ) ;
#48499 = EDGE_CURVE ( 'NONE', #60906, #22351, #14290, .T. ) ;
#48500 = DIRECTION ( 'NONE',  ( -1.000000000000000000, 0.000000000000000000, 0.000000000000000000 ) ) ;
#48501 = ORIENTED_EDGE ( 'NONE', *, *, #19984, .F. ) ;
#48502 = DIRECTION ( 'NONE',  ( 1.000000000000000000, 0.000000000000000000, 0.000000000000000000 ) ) ;
#48503 = CARTESIAN_POINT ( 'NONE',  ( 37.00000000000000711, 9.493370459201798894, 6.917234959366719060 ) ) ;
#48504 = CARTESIAN_POINT ( 'NONE',  ( 2.573738926104376823, -1.575954828885307801, 7.583190312075767103 ) ) ;
#48505 = VERTEX_POINT ( 'NONE', #18968 ) ;
#48506 = ORIENTED_EDGE ( 'NONE', *, *, #3698, .F. ) ;
#48507 = CARTESIAN_POINT ( 'NONE',  ( 35.00000000000000000, 4.705694406421931860E-17, -3.469127814946512892E-15 ) ) ;
#48508 = EDGE_CURVE ( 'NONE', #31872, #23983, #39272, .T. ) ;
#48509 = EDGE_LOOP ( 'NONE', ( #33745, #32487, #56933, #28000 ) ) ;
#48510 = FACE_OUTER_BOUND ( 'NONE', #58603, .T. ) ;
#48511 = ORIENTED_EDGE ( 'NONE', *, *, #22499, .T. ) ;
#48512 = CIRCLE ( 'NONE', #46403, 23.66025403784440329 ) ;
#48513 = ORIENTED_EDGE ( 'NONE', *, *, #685, .T. ) ;
#48514 = FACE_OUTER_BOUND ( 'NONE', #6921, .T. ) ;
#48515 = CARTESIAN_POINT ( 'NONE',  ( 35.00000000000000000, 6.036400161834703404, 10.07641281632170838 ) ) ;
#48516 = CARTESIAN_POINT ( 'NONE',  ( -27.08506889328343803, -2.284141197253890088, 0.2104793012480277725 ) ) ;
#48517 = CARTESIAN_POINT ( 'NONE',  ( -47.00000000000000711, 0.000000000000000000, 0.000000000000000000 ) ) ;
#48518 = DIRECTION ( 'NONE',  ( 0.000000000000000000, 0.000000000000000000, 1.000000000000000000 ) ) ;
#48519 = AXIS2_PLACEMENT_3D ( 'NONE', #44362, #60321, #51014 ) ;
#48520 = CARTESIAN_POINT ( 'NONE',  ( 2.990245332647836651, 5.049055049623246028, 6.814589384234954750 ) ) ;
#48521 = ORIENTED_EDGE ( 'NONE', *, *, #3057, .F. ) ;
#48522 = FACE_OUTER_BOUND ( 'NONE', #35015, .T. ) ;
#48523 = EDGE_CURVE ( 'NONE', #47458, #5728, #42428, .T. ) ;
#48524 = DIRECTION ( 'NONE',  ( 0.000000000000000000, -0.01356324068817999114, 0.9999080150203989437 ) ) ;
#48525 = CARTESIAN_POINT ( 'NONE',  ( 2.280717697724234938, 3.687451363405509941, -6.699799459371864607 ) ) ;
#48526 = EDGE_CURVE ( 'NONE', #1474, #26254, #27590, .T. ) ;
#48527 = CARTESIAN_POINT ( 'NONE',  ( 2.000000000000001776, -2.473437528934186780, 7.080403010454960899 ) ) ;
#48528 = CARTESIAN_POINT ( 'NONE',  ( -22.31328051695926007, 2.608921479762127849, -2.748895659348120635 ) ) ;
#48529 = DIRECTION ( 'NONE',  ( -1.000000000000000000, 0.000000000000000000, 0.000000000000000000 ) ) ;
#48530 = CYLINDRICAL_SURFACE ( 'NONE', #42668, 7.499999999999988454 ) ;
#48531 = CARTESIAN_POINT ( 'NONE',  ( 0.3109076770649089605, -11.60048803586496291, -3.971171685427508091 ) ) ;
#48532 = CARTESIAN_POINT ( 'NONE',  ( 0.3675815128205894289, -11.62724744438063063, -3.951233083390586209 ) ) ;
#48533 = ADVANCED_FACE ( 'NONE', ( #13955 ), #20146, .T. ) ;
#48534 = VERTEX_POINT ( 'NONE', #23966 ) ;
#48535 = CARTESIAN_POINT ( 'NONE',  ( 5.514624014163232779, -0.003830004412313187633, 0.001574979445069354207 ) ) ;
#48536 = EDGE_CURVE ( 'NONE', #2417, #57976, #64817, .T. ) ;
#48537 = EDGE_CURVE ( 'NONE', #45277, #57124, #26552, .T. ) ;
#48538 = ORIENTED_EDGE ( 'NONE', *, *, #13804, .F. ) ;
#48539 = DIRECTION ( 'NONE',  ( 0.000000000000000000, 0.9551603052523490733, -0.2960891610144476549 ) ) ;
#48540 = CARTESIAN_POINT ( 'NONE',  ( 0.3053067050349194123, -0.2307671807673114528, 12.25734436043223852 ) ) ;
#48541 = CARTESIAN_POINT ( 'NONE',  ( 3.152665057736074417, -6.622010822085853121, 4.377619405894153992 ) ) ;
#48542 = ADVANCED_FACE ( 'NONE', ( #19295 ), #37665, .F. ) ;
#48543 = DIRECTION ( 'NONE',  ( -1.000000000000000000, 0.000000000000000000, 0.000000000000000000 ) ) ;
#48544 = CARTESIAN_POINT ( 'NONE',  ( 2.653899356899187989, 7.694895988366112327, 1.091629880170703393 ) ) ;
#48545 = ORIENTED_EDGE ( 'NONE', *, *, #59614, .T. ) ;
#48546 = DIRECTION ( 'NONE',  ( 0.000000000000000000, 0.3193015301359806712, -0.9476531711828022342 ) ) ;
#48547 = CARTESIAN_POINT ( 'NONE',  ( -35.00000000000000000, 0.000000000000000000, 0.000000000000000000 ) ) ;
#48548 = CARTESIAN_POINT ( 'NONE',  ( -18.55833381744858457, -13.45545930202708007, 1.279848689959048658 ) ) ;
#48549 = CARTESIAN_POINT ( 'NONE',  ( 6.333770985417318755, -31.24637718315787183, -14.41548832156423998 ) ) ;
#48550 = B_SPLINE_CURVE_WITH_KNOTS ( 'NONE', 3,
 ( #64430, #23567, #38520, #54146, #30423, #56018, #63771, #58841, #33541, #18901, #30096, #2968, #43839, #25434, #175, #48516, #28871, #53829, #61021 ),
 .UNSPECIFIED., .F., .F.,
 ( 4, 3, 3, 3, 3, 3, 4 ),
 ( 0.000000000000000000, 2.836829842860534115E-05, 4.224792512343245412E-05, 5.612066614707884827E-05, 6.998859278151770078E-05, 9.832141287888560401E-05, 0.0001178161482480192461 ),
 .UNSPECIFIED. ) ;
#48551 = DIRECTION ( 'NONE',  ( 0.000000000000000000, 0.000000000000000000, 1.000000000000000000 ) ) ;
#48552 = CONICAL_SURFACE ( 'NONE', #19862, 7.938172270156617749, 1.280189991382167047 ) ;
#48553 = EDGE_LOOP ( 'NONE', ( #53756, #48738, #3841, #6942 ) ) ;
#48554 = CARTESIAN_POINT ( 'NONE',  ( 5.514624014163232779, 0.003668383633201373166, -0.001921576324372464796 ) ) ;
#48555 = DIRECTION ( 'NONE',  ( 0.000000000000000000, -0.1081190184239279872, -0.9941379571543611515 ) ) ;
#48556 = CARTESIAN_POINT ( 'NONE',  ( 2.269879328256732887, -3.949706986712154588, -6.544400685875864987 ) ) ;
#48557 = VECTOR ( 'NONE', #8342, 1000.000000000000227 ) ;
#48558 = ADVANCED_FACE ( 'NONE', ( #65161 ), #43535, .T. ) ;
#48559 = ORIENTED_EDGE ( 'NONE', *, *, #42991, .F. ) ;
#48560 = VECTOR ( 'NONE', #38238, 1000.000000000000000 ) ;
#48561 = ORIENTED_EDGE ( 'NONE', *, *, #40505, .T. ) ;
#48562 = CARTESIAN_POINT ( 'NONE',  ( -37.00000000000000711, -10.02106554660702820, -7.882940143791884680 ) ) ;
#48563 = ORIENTED_EDGE ( 'NONE', *, *, #18640, .F. ) ;
#48564 = CARTESIAN_POINT ( 'NONE',  ( 2.305787727787084407, 5.047606869483056258, 5.756228004061473946 ) ) ;
#48566 = DIRECTION ( 'NONE',  ( 1.000000000000000000, 0.000000000000000000, 0.000000000000000000 ) ) ;
#48565 =( BOUNDED_SURFACE ( )  B_SPLINE_SURFACE ( 3, 1, ( 
 ( #53169, #43174 ),
 ( #17605, #43495 ),
 ( #8585, #32859 ),
 ( #12577, #7615 ) ),
 .UNSPECIFIED., .F., .F., .F. ) 
 B_SPLINE_SURFACE_WITH_KNOTS ( ( 4, 4 ),
 ( 2, 2 ),
 ( 0.000000000000000000, 1.000000000000000000 ),
 ( 0.000000000000000000, 1.000000000000000000 ),
 .UNSPECIFIED. ) 
 GEOMETRIC_REPRESENTATION_ITEM ( )  RATIONAL_B_SPLINE_SURFACE ( (
 ( 1.000000000000000000, 1.000000000000000000),
 ( 0.9856612449720755231, 0.9999558406602322425),
 ( 0.9856612449720755231, 0.9999558406602322425),
 ( 1.000000000000000000, 1.000000000000000000) ) ) 
 REPRESENTATION_ITEM ( '' )  SURFACE ( )  );
#48567 = CARTESIAN_POINT ( 'NONE',  ( 28.93866847389637798, -3.371687389997651163, 23.68754010782029695 ) ) ;
#48568 = FACE_OUTER_BOUND ( 'NONE', #41090, .T. ) ;
#48569 = DIRECTION ( 'NONE',  ( 1.000000000000000000, 0.000000000000000000, 0.000000000000000000 ) ) ;
#48570 = ORIENTED_EDGE ( 'NONE', *, *, #38187, .F. ) ;
#48571 = EDGE_CURVE ( 'NONE', #36007, #29813, #55228, .T. ) ;
#48572 = EDGE_LOOP ( 'NONE', ( #46759, #47199, #1870, #4758 ) ) ;
#48573 = ORIENTED_EDGE ( 'NONE', *, *, #8955, .F. ) ;
#48574 = DIRECTION ( 'NONE',  ( 0.000000000000000000, 0.000000000000000000, 1.000000000000000000 ) ) ;
#48575 = CARTESIAN_POINT ( 'NONE',  ( 37.00000000000000711, -11.65554240571056077, 1.456211999474460672 ) ) ;
#48576 = ORIENTED_EDGE ( 'NONE', *, *, #44950, .F. ) ;
#48577 = CYLINDRICAL_SURFACE ( 'NONE', #12407, 5.000000000000002665 ) ;
#48578 = CARTESIAN_POINT ( 'NONE',  ( 3.152665057734129750, -7.102135024645910732, 3.546019893116286958 ) ) ;
#48579 = ORIENTED_EDGE ( 'NONE', *, *, #10380, .T. ) ;
#48580 = CARTESIAN_POINT ( 'NONE',  ( 0.000000000000000000, 2.469490258309515518, -6.482025155313297482 ) ) ;
#48581 = DIRECTION ( 'NONE',  ( 1.000000000000000000, -0.000000000000000000, 0.000000000000000000 ) ) ;
#48582 = DIRECTION ( 'NONE',  ( 1.000000000000000000, -0.000000000000000000, 0.000000000000000000 ) ) ;
#48583 = VERTEX_POINT ( 'NONE', #4679 ) ;
#48584 = ORIENTED_EDGE ( 'NONE', *, *, #54316, .F. ) ;
#48585 = DIRECTION ( 'NONE',  ( -0.3865475372811021382, -0.1410344188397464060, 0.9114221272958265008 ) ) ;
#48586 = EDGE_CURVE ( 'NONE', #26931, #10291, #51667, .T. ) ;
#48587 = ORIENTED_EDGE ( 'NONE', *, *, #58368, .F. ) ;
#48588 = CARTESIAN_POINT ( 'NONE',  ( -18.78798712546867122, 11.98387424500765697, -0.7129084681429045389 ) ) ;
#48589 = ORIENTED_EDGE ( 'NONE', *, *, #50382, .F. ) ;
#48590 = CARTESIAN_POINT ( 'NONE',  ( 2.242819959140645469, 3.728423299584983752, 6.662619100654757709 ) ) ;
#48591 = ADVANCED_FACE ( 'NONE', ( #50221 ), #19939, .T. ) ;
#48592 = CARTESIAN_POINT ( 'NONE',  ( -37.00000000000000711, -8.017674001891851532, 9.913596905230088296 ) ) ;
#48594 = MECHANICAL_DESIGN_GEOMETRIC_PRESENTATION_REPRESENTATION (  '', ( #22176 ), #31574 ) ;
#48593 = CARTESIAN_POINT ( 'NONE',  ( -19.26763262626407069, -29.00000000000000000, 5.969230316860641317 ) ) ;
#48595 = CYLINDRICAL_SURFACE ( 'NONE', #1712, 12.75000000000000178 ) ;
#48596 = CARTESIAN_POINT ( 'NONE',  ( 0.000000000000000000, 0.000000000000000000, 0.000000000000000000 ) ) ;
#48597 = DIRECTION ( 'NONE',  ( -1.000000000000000000, -0.000000000000000000, 0.000000000000000000 ) ) ;
#48598 = ORIENTED_EDGE ( 'NONE', *, *, #55672, .F. ) ;
#48599 = DIRECTION ( 'NONE',  ( 1.000000000000000000, -0.000000000000000000, -0.000000000000000000 ) ) ;
#48600 = EDGE_LOOP ( 'NONE', ( #49806, #64363, #10196, #44851 ) ) ;
#48601 = CARTESIAN_POINT ( 'NONE',  ( 2.268878695253352618, -2.752970156154534997, 7.130600918714371517 ) ) ;
#48602 = CARTESIAN_POINT ( 'NONE',  ( 2.273267844203306520, 6.695181685738918809, 3.690689057642454252 ) ) ;
#48603 = EDGE_LOOP ( 'NONE', ( #50701, #19199, #32952, #8332 ) ) ;
#48604 = CARTESIAN_POINT ( 'NONE',  ( 0.3665391374699464300, -5.911453292029527518, -10.76665847464318837 ) ) ;
#48605 = CARTESIAN_POINT ( 'NONE',  ( 0.3474126878361764592, 12.03947592323250149, -2.385599230261914894 ) ) ;
#48606 = CARTESIAN_POINT ( 'NONE',  ( 0.3006302518452102501, -2.350739146140512936, -12.03044280705495872 ) ) ;
#48607 = AXIS2_PLACEMENT_3D ( 'NONE', #260, #40133, #45457 ) ;
#48608 = EDGE_CURVE ( 'NONE', #10092, #32250, #60838, .T. ) ;
#48609 = ORIENTED_EDGE ( 'NONE', *, *, #64741, .F. ) ;
#48610 = VERTEX_POINT ( 'NONE', #45877 ) ;
#48611 = AXIS2_PLACEMENT_3D ( 'NONE', #10513, #30789, #5904 ) ;
#48612 = CARTESIAN_POINT ( 'NONE',  ( 2.524535260912908807, -6.801151891677258199, -3.671333852642867601 ) ) ;
#48613 = EDGE_CURVE ( 'NONE', #14694, #39894, #15915, .T. ) ;
#48614 = EDGE_LOOP ( 'NONE', ( #5246, #60356, #26808, #45254 ) ) ;
#48615 = CARTESIAN_POINT ( 'NONE',  ( -28.56462394502009516, 3.589878760083821341, 13.01421318288084450 ) ) ;
#48616 = CARTESIAN_POINT ( 'NONE',  ( 37.00000000000000711, 6.475373545682446164, 10.32377448871660519 ) ) ;
#48617 = DIRECTION ( 'NONE',  ( 0.000000000000000000, 0.2355298848897516562, 0.9718671068226458765 ) ) ;
#48618 = ADVANCED_FACE ( 'NONE', ( #46521 ), #11921, .T. ) ;
#48619 = CARTESIAN_POINT ( 'NONE',  ( -2.532614230583022152, 11.30437021680556242, 4.026315189028233377 ) ) ;
#48620 = FACE_OUTER_BOUND ( 'NONE', #5346, .T. ) ;
#48621 = ORIENTED_EDGE ( 'NONE', *, *, #55390, .T. ) ;
#48622 = CARTESIAN_POINT ( 'NONE',  ( 0.2648978790185593790, -12.03635331166810651, -2.256510822326266652 ) ) ;
#48623 = EDGE_CURVE ( 'NONE', #6133, #11272, #15596, .T. ) ;
#48624 = CARTESIAN_POINT ( 'NONE',  ( 2.994568964204210815, -7.686291764591495657, -1.761139509856907592 ) ) ;
#48625 = CARTESIAN_POINT ( 'NONE',  ( -35.00000000000000000, -11.26103545359858060, 3.340853584269496412 ) ) ;
#48626 = DIRECTION ( 'NONE',  ( 0.000000000000000000, 0.01356324068817998940, -0.9999080150203989437 ) ) ;
#48627 = CARTESIAN_POINT ( 'NONE',  ( 0.2652384529303158933, 7.922180393770671181, 9.338494547402412138 ) ) ;
#48628 = CARTESIAN_POINT ( 'NONE',  ( 7.006432388548472723, -4.543361190407962269, -11.11502132045045066 ) ) ;
#48629 = CARTESIAN_POINT ( 'NONE',  ( -22.46509356695199600, -0.8809186187926192346, 4.154553862421305865 ) ) ;
#48630 = VECTOR ( 'NONE', #9623, 1000.000000000000000 ) ;
#48631 = ORIENTED_EDGE ( 'NONE', *, *, #57442, .F. ) ;
#48632 = CARTESIAN_POINT ( 'NONE',  ( 11.74548640120467979, -8.775604215601116920, -8.184666801472349817 ) ) ;
#48633 = EDGE_CURVE ( 'NONE', #7338, #15890, #31855, .T. ) ;
#48634 = CIRCLE ( 'NONE', #29477, 12.75000000000000178 ) ;
#48635 = ORIENTED_EDGE ( 'NONE', *, *, #61486, .F. ) ;
#48636 = CARTESIAN_POINT ( 'NONE',  ( 0.2739690278137261181, 1.946552041163069013, -12.09341522051407480 ) ) ;
#48637 = CARTESIAN_POINT ( 'NONE',  ( 1.719304012340734378, -8.755325027794794934, -9.242227816401850760 ) ) ;
#48638 = DIRECTION ( 'NONE',  ( 1.000000000000000000, 0.000000000000000000, 0.000000000000000000 ) ) ;
#48639 = ORIENTED_EDGE ( 'NONE', *, *, #59193, .F. ) ;
#48640 = VECTOR ( 'NONE', #33693, 1000.000000000000000 ) ;
#48641 = FACE_BOUND ( 'NONE', #57439, .T. ) ;
#48642 = DIRECTION ( 'NONE',  ( -1.000000000000000000, 0.000000000000000000, 0.000000000000000000 ) ) ;
#48643 = ORIENTED_EDGE ( 'NONE', *, *, #41549, .T. ) ;
#48644 = ADVANCED_FACE ( 'NONE', ( #25926 ), #20609, .T. ) ;
#48645 = ORIENTED_EDGE ( 'NONE', *, *, #48366, .T. ) ;
#48646 = AXIS2_PLACEMENT_3D ( 'NONE', #55952, #20050, #34357 ) ;
#48647 = VERTEX_POINT ( 'NONE', #31238 ) ;
#48648 = CARTESIAN_POINT ( 'NONE',  ( 29.04793922789648875, -11.92654474506188222, 6.328478715807100308 ) ) ;
#48649 = CARTESIAN_POINT ( 'NONE',  ( -22.30078715814471835, -3.372109767220907273, -1.645949880549425037 ) ) ;
#48650 = VERTEX_POINT ( 'NONE', #21917 ) ;
#48651 = CARTESIAN_POINT ( 'NONE',  ( 37.00000000000000711, -6.415447294506781084, -11.01837265713071368 ) ) ;
#48652 = CARTESIAN_POINT ( 'NONE',  ( 1.719304012338199517, 12.70777170743846796, 0.7661785589580254463 ) ) ;
#48653 = FACE_OUTER_BOUND ( 'NONE', #36783, .T. ) ;
#48654 = CARTESIAN_POINT ( 'NONE',  ( 17.27839441901508621, 10.52068335315811076, 5.771933972472480967 ) ) ;
#48655 = ORIENTED_EDGE ( 'NONE', *, *, #51435, .F. ) ;
#48656 = DIRECTION ( 'NONE',  ( 0.000000000000000000, -0.01356324068817998940, 0.9999080150203990547 ) ) ;
#48657 = CARTESIAN_POINT ( 'NONE',  ( -37.00000000000000711, -2.185196060783795691, -11.54110654723651486 ) ) ;
#48658 = CARTESIAN_POINT ( 'NONE',  ( -29.43980975494970309, -3.641506875706030488, 11.43413432115373318 ) ) ;
#48660 = ORIENTED_EDGE ( 'NONE', *, *, #23182, .T. ) ;
#48659 = CARTESIAN_POINT ( 'NONE',  ( 1.937114397841932290, 3.111612666690241724, -12.45230409340478239 ) ) ;
#48661 = CARTESIAN_POINT ( 'NONE',  ( 0.3665391374699472626, 3.952034409876453047, -11.62960183138723025 ) ) ;
#48662 = EDGE_CURVE ( 'NONE', #44487, #58379, #20116, .T. ) ;
#48663 = EDGE_CURVE ( 'NONE', #21056, #266, #56267, .T. ) ;
#48664 = VERTEX_POINT ( 'NONE', #35860 ) ;
#48665 = CARTESIAN_POINT ( 'NONE',  ( 1.719304012338239485, 12.38166659046522788, 2.961219984258211202 ) ) ;
#48666 = ORIENTED_EDGE ( 'NONE', *, *, #38757, .F. ) ;
#48667 = CARTESIAN_POINT ( 'NONE',  ( -37.00000000000000711, 0.000000000000000000, 0.000000000000000000 ) ) ;
#48668 = CYLINDRICAL_SURFACE ( 'NONE', #50055, 12.18650000000000055 ) ;
#48669 = EDGE_CURVE ( 'NONE', #23832, #39632, #64743, .T. ) ;
#48670 = DIRECTION ( 'NONE',  ( 0.000000000000000000, 0.01356324068817998940, -0.9999080150203990547 ) ) ;
#48671 = CARTESIAN_POINT ( 'NONE',  ( 35.00000000000000000, 0.1652884326465054732, -12.18537902504609427 ) ) ;
#48672 = CARTESIAN_POINT ( 'NONE',  ( -42.50000000000000000, -2.710505431213761085E-17, 1.201363017033314212E-18 ) ) ;
#48673 = CARTESIAN_POINT ( 'NONE',  ( 37.00000000000000711, -9.506317355798431734, -8.496612874013129257 ) ) ;
#48674 = CARTESIAN_POINT ( 'NONE',  ( 2.241509619876138171, -5.872890204493053545, 4.877966158328288060 ) ) ;
#48675 = ORIENTED_EDGE ( 'NONE', *, *, #19577, .T. ) ;
#48676 = CIRCLE ( 'NONE', #57168, 7.499999999999988454 ) ;
#48677 = DIRECTION ( 'NONE',  ( -1.000000000000000000, 0.000000000000000000, 0.000000000000000000 ) ) ;
#48678 = ORIENTED_EDGE ( 'NONE', *, *, #55402, .T. ) ;
#48679 = VERTEX_POINT ( 'NONE', #36551 ) ;
#48680 = CARTESIAN_POINT ( 'NONE',  ( 5.514624014163232779, -0.002789935220458067931, 0.003060352188290767217 ) ) ;
#48681 = FACE_OUTER_BOUND ( 'NONE', #6919, .T. ) ;
#48682 = CYLINDRICAL_SURFACE ( 'NONE', #41518, 4.999999999999999112 ) ;
#48683 = CARTESIAN_POINT ( 'NONE',  ( -22.28284753389937123, 0.9912969289936786055, 3.563226652211039180 ) ) ;
#48684 = CARTESIAN_POINT ( 'NONE',  ( 1.937114397841935398, -11.53912442307251496, -5.620553190833097013 ) ) ;
#48685 = EDGE_CURVE ( 'NONE', #10035, #1393, #25584, .T. ) ;
#48686 = CIRCLE ( 'NONE', #53994, 7.499999999999988454 ) ;
#48687 = DIRECTION ( 'NONE',  ( -1.000000000000000000, 0.000000000000000000, 0.000000000000000000 ) ) ;
#48688 = FACE_OUTER_BOUND ( 'NONE', #35799, .T. ) ;
#48689 = EDGE_CURVE ( 'NONE', #12619, #46217, #46853, .T. ) ;
#48690 = CIRCLE ( 'NONE', #9340, 5.000000000000000888 ) ;
#48691 = AXIS2_PLACEMENT_3D ( 'NONE', #43390, #33744, #13153 ) ;
#48692 = ORIENTED_EDGE ( 'NONE', *, *, #34940, .F. ) ;
#48693 = DIRECTION ( 'NONE',  ( 1.000000000000000000, 0.000000000000000000, 0.000000000000000000 ) ) ;
#48694 = CARTESIAN_POINT ( 'NONE',  ( -35.00000000000000000, 4.561791185930587744, -11.90598845858528776 ) ) ;
#48695 = VECTOR ( 'NONE', #14310, 1000.000000000000000 ) ;
#48696 = DIRECTION ( 'NONE',  ( 1.000000000000000000, 0.000000000000000000, -0.000000000000000000 ) ) ;
#48697 = VECTOR ( 'NONE', #31493, 1000.000000000000000 ) ;
#48698 = DIRECTION ( 'NONE',  ( 1.000000000000000000, 0.000000000000000000, 0.000000000000000000 ) ) ;
#48699 = CARTESIAN_POINT ( 'NONE',  ( 2.889800649504073782, 4.645655809191420182, -3.986129653162600928 ) ) ;
#48700 = CARTESIAN_POINT ( 'NONE',  ( -5.434547206004880060, -0.9285584038156732278, 13.46803372541172195 ) ) ;
#48701 = CARTESIAN_POINT ( 'NONE',  ( 8.937200413559443390, 4.476360154859203355, -11.13383131558893346 ) ) ;
#48702 = ORIENTED_EDGE ( 'NONE', *, *, #21794, .F. ) ;
#48703 = FACE_OUTER_BOUND ( 'NONE', #4011, .T. ) ;
#48704 = CARTESIAN_POINT ( 'NONE',  ( -35.00000000000000000, 0.7214809346828596759, 11.72397916322012712 ) ) ;
#48705 = FACE_OUTER_BOUND ( 'NONE', #31800, .T. ) ;
#48706 = B_SPLINE_CURVE_WITH_KNOTS ( 'NONE', 3,
 ( #62404, #46801, #16868, #26516, #62105, #56456, #22181, #1268, #36825, #47153, #16218, #11549, #31817, #11875, #929, #26201, #36502, #61425, #26850 ),
 .UNSPECIFIED., .F., .F.,
 ( 4, 3, 3, 3, 3, 3, 4 ),
 ( 0.000000000000000000, 2.831840207501608918E-05, 4.217266859843136855E-05, 5.602024318398862116E-05, 6.290810167972007863E-05, 9.120440630948104476E-05, 0.0001153103026479716580 ),
 .UNSPECIFIED. ) ;
#48707 = AXIS2_PLACEMENT_3D ( 'NONE', #2989, #38879, #48539 ) ;
#48708 = CYLINDRICAL_SURFACE ( 'NONE', #41617, 12.18649999999999878 ) ;
#48709 = DIRECTION ( 'NONE',  ( 0.000000000000000000, 0.9987865678893277366, -0.04924826701374931254 ) ) ;
#48710 = EDGE_CURVE ( 'NONE', #38228, #45313, #62147, .T. ) ;
#48711 = EDGE_LOOP ( 'NONE', ( #6163, #49808, #56834, #43950 ) ) ;
#48712 = FACE_OUTER_BOUND ( 'NONE', #55090, .T. ) ;
#48713 = CARTESIAN_POINT ( 'NONE',  ( 2.249013661412013310, -4.816366775941638423, -5.926694833810301155 ) ) ;
#48714 = DIRECTION ( 'NONE',  ( -1.000000000000000000, 0.000000000000000000, -0.000000000000000000 ) ) ;
#48715 = ORIENTED_EDGE ( 'NONE', *, *, #27876, .T. ) ;
#48716 = CARTESIAN_POINT ( 'NONE',  ( 35.00000000000000000, -3.645068577059948911, 11.16627499335658413 ) ) ;
#48717 = CARTESIAN_POINT ( 'NONE',  ( -27.10719052120871098, -1.044362304621479165, 2.116547233941197703 ) ) ;
#48718 = ORIENTED_EDGE ( 'NONE', *, *, #19662, .T. ) ;
#48719 = EDGE_LOOP ( 'NONE', ( #48675, #59304, #49876, #50685 ) ) ;
#48720 = FACE_OUTER_BOUND ( 'NONE', #57826, .T. ) ;
#48721 = CIRCLE ( 'NONE', #21076, 12.18649999999999878 ) ;
#48722 = EDGE_CURVE ( 'NONE', #56593, #58586, #24409, .T. ) ;
#48723 = ORIENTED_EDGE ( 'NONE', *, *, #25753, .F. ) ;
#48724 = CYLINDRICAL_SURFACE ( 'NONE', #38719, 12.18649999999999878 ) ;
#48725 = CARTESIAN_POINT ( 'NONE',  ( -37.00000000000000711, -7.094637218249278732, -10.59380114696477904 ) ) ;
#48726 = VECTOR ( 'NONE', #18198, 1000.000000000000000 ) ;
#48727 = CARTESIAN_POINT ( 'NONE',  ( -35.00000000000000000, 8.029056188533687077, 8.573591947375351907 ) ) ;
#48728 = CIRCLE ( 'NONE', #13526, 5.000000000000000000 ) ;
#48729 = LINE ( 'NONE', #8476, #4319 ) ;
#48730 = CARTESIAN_POINT ( 'NONE',  ( 5.530133899448235191, 0.01149180883054601483, -0.01111090067015111857 ) ) ;
#48732 = ORIENTED_EDGE ( 'NONE', *, *, #30358, .F. ) ;
#48731 = CARTESIAN_POINT ( 'NONE',  ( 3.152665057734127974, -4.377619405892426485, 6.622010822086644488 ) ) ;
#48733 = CIRCLE ( 'NONE', #47544, 6.936499999999991672 ) ;
#48734 = DIRECTION ( 'NONE',  ( 0.000000000000000000, -0.01356324068817998073, 0.9999080150203990547 ) ) ;
#48735 = EDGE_CURVE ( 'NONE', #41230, #33435, #15905, .T. ) ;
#48736 = ORIENTED_EDGE ( 'NONE', *, *, #17613, .T. ) ;
#48737 = DIRECTION ( 'NONE',  ( 0.000000000000000000, -0.01356324068817991828, 0.9999080150203990547 ) ) ;
#48738 = ORIENTED_EDGE ( 'NONE', *, *, #18415, .F. ) ;
#48739 = AXIS2_PLACEMENT_3D ( 'NONE', #51059, #5517, #31093 ) ;
#48740 = ORIENTED_EDGE ( 'NONE', *, *, #2815, .F. ) ;
#48741 = CARTESIAN_POINT ( 'NONE',  ( -24.88582978492754805, 10.97013053255485104, 7.869802505931382086 ) ) ;
#48742 = CARTESIAN_POINT ( 'NONE',  ( 0.9290584433855317847, -28.11997881881914196, 13.91374373156083166 ) ) ;
#48743 = CARTESIAN_POINT ( 'NONE',  ( -4.020556197261224263, 8.897818130997190877, 8.054759335216724381 ) ) ;
#48744 = B_SPLINE_CURVE_WITH_KNOTS ( 'NONE', 3,
 ( #30543, #34857, #14904, #45196, #35539, #50846, #31219, #46196, #20244, #25236, #56485, #55505, #45508, #30865, #5293, #640, #5638, #29893, #21224, #25907, #20898, #65458 ),
 .UNSPECIFIED., .F., .F.,
 ( 4, 3, 3, 3, 3, 3, 3, 4 ),
 ( 0.000000000000000000, 6.990956068646571873E-05, 0.0001398191187764076656, 0.0002097286751720259625, 0.0002796382307041417933, 0.0003495477861619887723, 0.0004194573423310374110, 0.0005586102576333247961 ),
 .UNSPECIFIED. ) ;
#48745 = CARTESIAN_POINT ( 'NONE',  ( 5.514624014163232779, 0.003830004412313175489, -0.001574979445069380445 ) ) ;
#48746 = CARTESIAN_POINT ( 'NONE',  ( 2.000000000000001776, -5.860254403322002759, -3.474373880649873403 ) ) ;
#48747 = CARTESIAN_POINT ( 'NONE',  ( -27.08419642509983305, 0.7009209357102744731, -2.181485315953918924 ) ) ;
#48748 = ORIENTED_EDGE ( 'NONE', *, *, #36354, .F. ) ;
#48749 =( BOUNDED_SURFACE ( )  B_SPLINE_SURFACE ( 3, 1, ( 
 ( #16852, #43347 ),
 ( #11221, #2829 ),
 ( #51140, #28083 ),
 ( #61412, #46789 ) ),
 .UNSPECIFIED., .F., .F., .T. ) 
 B_SPLINE_SURFACE_WITH_KNOTS ( ( 4, 4 ),
 ( 2, 2 ),
 ( 0.000000000000000000, 1.000000000000000000 ),
 ( 0.000000000000000000, 1.000000000000000000 ),
 .UNSPECIFIED. ) 
 GEOMETRIC_REPRESENTATION_ITEM ( )  RATIONAL_B_SPLINE_SURFACE ( (
 ( 1.000000000000000000, 1.000000000000000000),
 ( 0.9942764183789327692, 0.8450855930916580938),
 ( 0.9942764183789327692, 0.8450855930916580938),
 ( 1.000000000000000000, 1.000000000000000000) ) ) 
 REPRESENTATION_ITEM ( '' )  SURFACE ( )  );
#48750 = CARTESIAN_POINT ( 'NONE',  ( -35.00000000000000000, 9.321877890560440250, 7.146664589317944127 ) ) ;
#48751 = CARTESIAN_POINT ( 'NONE',  ( 0.6473888112830240571, -3.920507224439165217, 11.73602097806018918 ) ) ;
#48752 = FACE_OUTER_BOUND ( 'NONE', #47571, .T. ) ;
#48753 = ORIENTED_EDGE ( 'NONE', *, *, #14802, .F. ) ;
#48754 = CARTESIAN_POINT ( 'NONE',  ( 37.00000000000000711, 0.4993900848169179896, 12.17626345777662777 ) ) ;
#48755 = ORIENTED_EDGE ( 'NONE', *, *, #64683, .F. ) ;
#48756 = CARTESIAN_POINT ( 'NONE',  ( 2.266490820343226353, -7.500072841116509181, 1.470039317404140622 ) ) ;
#48757 = CARTESIAN_POINT ( 'NONE',  ( 0.3537226245948354442, -10.49813096858605377, -6.362463382302378179 ) ) ;
#48758 = DIRECTION ( 'NONE',  ( -1.000000000000000000, -0.000000000000000000, -0.000000000000000000 ) ) ;
#48759 = DIRECTION ( 'NONE',  ( -1.000000000000000000, 0.000000000000000000, 0.000000000000000000 ) ) ;
#48760 = CYLINDRICAL_SURFACE ( 'NONE', #41591, 12.75000000000000178 ) ;
#48761 = CARTESIAN_POINT ( 'NONE',  ( -27.08579483061203064, -1.879952013015653289, 1.318128465624906154 ) ) ;
#48762 = CIRCLE ( 'NONE', #64669, 12.18650000000000055 ) ;
#48763 = CARTESIAN_POINT ( 'NONE',  ( 36.00000000000000711, -1.738225594540087293, -12.63095688309028652 ) ) ;
#48764 = VERTEX_POINT ( 'NONE', #1648 ) ;
#48765 = DIRECTION ( 'NONE',  ( 0.000000000000000000, -0.9985334138511233748, -0.05413890858542835804 ) ) ;
#48766 = CIRCLE ( 'NONE', #57259, 12.18650000000000055 ) ;
#48767 = VERTEX_POINT ( 'NONE', #17255 ) ;
#48768 = CARTESIAN_POINT ( 'NONE',  ( -27.35552965826137140, 1.320216934008397569, 2.810569013793730697 ) ) ;
#48769 = EDGE_CURVE ( 'NONE', #57005, #61089, #22573, .T. ) ;
#48770 = FACE_OUTER_BOUND ( 'NONE', #4098, .T. ) ;
#48771 = CARTESIAN_POINT ( 'NONE',  ( 35.00000000000000000, -12.14284015767850455, -1.030638227056526413 ) ) ;
#48772 = CIRCLE ( 'NONE', #20087, 12.75000000000000178 ) ;
#48773 = VECTOR ( 'NONE', #51091, 1000.000000000000000 ) ;
#48774 = EDGE_CURVE ( 'NONE', #18751, #12414, #29633, .T. ) ;
#48775 = LINE ( 'NONE', #28803, #21708 ) ;
#48776 = DIRECTION ( 'NONE',  ( -1.000000000000000000, 0.000000000000000000, 0.000000000000000000 ) ) ;
#48777 = CIRCLE ( 'NONE', #6296, 5.000000000000000000 ) ;
#48778 = ORIENTED_EDGE ( 'NONE', *, *, #34854, .F. ) ;
#48779 = DIRECTION ( 'NONE',  ( 1.000000000000000000, 0.000000000000000000, 0.000000000000000000 ) ) ;
#48780 = DIRECTION ( 'NONE',  ( 0.000000000000000000, 0.5987040770935622147, -0.8009703041134208501 ) ) ;
#48781 = CARTESIAN_POINT ( 'NONE',  ( -35.00000000000000000, 5.921969905510501064, -10.14408668126206869 ) ) ;
#48782 = CARTESIAN_POINT ( 'NONE',  ( 0.2851083653049504285, -0.4107471485392698018, 25.00000000000000000 ) ) ;
#48783 = ORIENTED_EDGE ( 'NONE', *, *, #20797, .T. ) ;
#48784 = CARTESIAN_POINT ( 'NONE',  ( 2.524535260911649814, -6.060306679218513182, -4.796565674004641622 ) ) ;
#48785 = CARTESIAN_POINT ( 'NONE',  ( -27.35552965826137140, -0.2619431035391951434, 3.094132632038943065 ) ) ;
#48786 = CARTESIAN_POINT ( 'NONE',  ( 0.2652384529303124516, -10.63836770010961885, -6.065769141714316248 ) ) ;
#48787 = AXIS2_PLACEMENT_3D ( 'NONE', #56630, #51966, #22019 ) ;
#48788 = DIRECTION ( 'NONE',  ( -1.000000000000000000, 0.000000000000000000, 0.000000000000000000 ) ) ;
#48789 = EDGE_CURVE ( 'NONE', #38911, #5091, #38507, .T. ) ;
#48790 = CARTESIAN_POINT ( 'NONE',  ( 2.524535260912295964, -3.671333852642895579, 6.801151891677007733 ) ) ;
#48791 = CARTESIAN_POINT ( 'NONE',  ( 0.6473888112830264996, -4.540486098228903700, -11.51036712212684421 ) ) ;
#48792 = EDGE_CURVE ( 'NONE', #659, #40350, #63703, .T. ) ;
#48793 = VERTEX_POINT ( 'NONE', #42489 ) ;
#48794 = EDGE_CURVE ( 'NONE', #35378, #853, #32896, .T. ) ;
#48795 = CARTESIAN_POINT ( 'NONE',  ( -20.55448987689497997, -11.44131724608703493, -3.631843722756310733 ) ) ;
#48796 = CARTESIAN_POINT ( 'NONE',  ( 35.00000000000000000, 4.705694406421931860E-17, -3.469127814946512892E-15 ) ) ;
#48797 = CARTESIAN_POINT ( 'NONE',  ( 4.225235259830817824, -25.92188032005471143, -15.36840686706593928 ) ) ;
#48798 = ORIENTED_EDGE ( 'NONE', *, *, #54223, .F. ) ;
#48799 = EDGE_CURVE ( 'NONE', #25571, #22630, #47838, .T. ) ;
#48800 = CARTESIAN_POINT ( 'NONE',  ( 1.000000000000000888, -0.08317740279924559776, -7.499538753794370294 ) ) ;
#48801 = DIRECTION ( 'NONE',  ( 0.000000000000000000, 0.6745969609292664648, 0.7381862504171951000 ) ) ;
#48802 = CARTESIAN_POINT ( 'NONE',  ( 37.00000000000000711, 4.705694406421931860E-17, -3.469127814946512892E-15 ) ) ;
#48803 = CARTESIAN_POINT ( 'NONE',  ( 47.00000000000000711, 4.705694406421931860E-17, -3.469127814946512892E-15 ) ) ;
#48804 = DIRECTION ( 'NONE',  ( -1.000000000000000000, -1.685093406416449860E-16, 1.011030131491573426E-17 ) ) ;
#48805 = AXIS2_PLACEMENT_3D ( 'NONE', #26202, #6254, #19897 ) ;
#48806 = EDGE_CURVE ( 'NONE', #37781, #34941, #41393, .T. ) ;
#48807 = DIRECTION ( 'NONE',  ( 1.000000000000000000, 0.000000000000000000, 0.000000000000000000 ) ) ;
#48808 = VERTEX_POINT ( 'NONE', #27885 ) ;
#48809 = DIRECTION ( 'NONE',  ( 0.000000000000000000, 0.000000000000000000, -1.000000000000000000 ) ) ;
#48810 = LINE ( 'NONE', #19187, #53207 ) ;
#48811 = CARTESIAN_POINT ( 'NONE',  ( 0.2648978790185619880, -9.465406350830555482, -7.769924372105300847 ) ) ;
#48812 = CARTESIAN_POINT ( 'NONE',  ( 37.00000000000000711, 4.705694406421931860E-17, -3.469127814946512892E-15 ) ) ;
#48813 = CARTESIAN_POINT ( 'NONE',  ( 2.241311220309555985, 7.533971938435861659, -1.234192392743096223 ) ) ;
#48815 = LINE ( 'NONE', #2938, #4521 ) ;
#48814 = CIRCLE ( 'NONE', #13706, 7.499999999999988454 ) ;
#48816 = ADVANCED_FACE ( 'NONE', ( #58828 ), #65242, .F. ) ;
#48817 = DIRECTION ( 'NONE',  ( 1.000000000000000000, 0.000000000000000000, 0.000000000000000000 ) ) ;
#48818 = DIRECTION ( 'NONE',  ( -1.000000000000000000, -0.000000000000000000, 0.000000000000000000 ) ) ;
#48819 = EDGE_LOOP ( 'NONE', ( #55617, #34462, #15380, #23210 ) ) ;
#48820 = ORIENTED_EDGE ( 'NONE', *, *, #29146, .T. ) ;
#48821 = CARTESIAN_POINT ( 'NONE',  ( -37.00000000000000711, 10.99909370905157502, 5.246972444134057945 ) ) ;
#48822 = ORIENTED_EDGE ( 'NONE', *, *, #41127, .F. ) ;
#48823 = CARTESIAN_POINT ( 'NONE',  ( -22.27756824490284515, 2.608445836294067899, -2.599719761044736899 ) ) ;
#48824 = AXIS2_PLACEMENT_3D ( 'NONE', #42377, #33976, #47416 ) ;
#48825 = DIRECTION ( 'NONE',  ( 0.3865475372811021382, 0.9114221272958279441, -0.1410344188397373577 ) ) ;
#48826 = EDGE_CURVE ( 'NONE', #31052, #15913, #11647, .T. ) ;
#48827 = DIRECTION ( 'NONE',  ( 0.000000000000000000, -0.01356324068817998940, 0.9999080150203990547 ) ) ;
#48829 = ORIENTED_EDGE ( 'NONE', *, *, #39437, .T. ) ;
#48828 = CIRCLE ( 'NONE', #18016, 12.18649999999999700 ) ;
#48830 = CARTESIAN_POINT ( 'NONE',  ( 0.3164563675027620149, 5.922187299605785604, -10.73846246126243109 ) ) ;
#48831 = CARTESIAN_POINT ( 'NONE',  ( 2.994568964204209038, 1.761139509856933127, -7.686291764591495657 ) ) ;
#48832 = CARTESIAN_POINT ( 'NONE',  ( 2.507146904658100084, -1.553587269793110126, 7.565123178000311199 ) ) ;
#48833 = ORIENTED_EDGE ( 'NONE', *, *, #55495, .F. ) ;
#48834 = ORIENTED_EDGE ( 'NONE', *, *, #62308, .F. ) ;
#48835 = DIRECTION ( 'NONE',  ( 0.000000000000000000, 0.000000000000000000, 1.000000000000000000 ) ) ;
#48836 = ORIENTED_EDGE ( 'NONE', *, *, #7322, .T. ) ;
#48837 = CARTESIAN_POINT ( 'NONE',  ( 35.00000000000000000, 0.06441628369836321921, -12.18632975068353019 ) ) ;
#48838 = VERTEX_POINT ( 'NONE', #43481 ) ;
#48839 = AXIS2_PLACEMENT_3D ( 'NONE', #10281, #44537, #30560 ) ;
#48840 = VERTEX_POINT ( 'NONE', #22229 ) ;
#48841 = DIRECTION ( 'NONE',  ( 0.000000000000000000, -0.01356324068817999114, 0.9999080150203989437 ) ) ;
#48842 = CARTESIAN_POINT ( 'NONE',  ( -27.08702828306202548, -1.612407531673535122, 1.639744581306259441 ) ) ;
#48843 = CARTESIAN_POINT ( 'NONE',  ( 0.3109076770649056853, 10.49874397806414272, -6.333869442011672568 ) ) ;
#48844 = DIRECTION ( 'NONE',  ( 0.000000000000000000, -0.07632122047555069122, 0.9970832820307048427 ) ) ;
#48845 = CARTESIAN_POINT ( 'NONE',  ( 0.2648978790185619880, -10.67083876753487637, -6.008231198269095685 ) ) ;
#48846 = FACE_OUTER_BOUND ( 'NONE', #24609, .T. ) ;
#48847 = ORIENTED_EDGE ( 'NONE', *, *, #19074, .F. ) ;
#48848 = CARTESIAN_POINT ( 'NONE',  ( 2.241352910868908310, -5.901537464758487062, 4.843133558968109043 ) ) ;
#48849 = CARTESIAN_POINT ( 'NONE',  ( -16.18260486426706279, 7.813572176425474858, 9.107691046539137858 ) ) ;
#48850 = CARTESIAN_POINT ( 'NONE',  ( -19.02967556479643463, -13.50000000000023803, -2.066764320408402454E-13 ) ) ;
#48851 = DIRECTION ( 'NONE',  ( -0.000000000000000000, -0.000000000000000000, -1.000000000000000000 ) ) ;
#48852 = CARTESIAN_POINT ( 'NONE',  ( 0.3654063281920749140, -8.093076148785975477, -9.235228056824000831 ) ) ;
#48853 = CARTESIAN_POINT ( 'NONE',  ( 23.76514404369831013, 1.691375342996074504, 13.39763565441737114 ) ) ;
#48854 = CARTESIAN_POINT ( 'NONE',  ( -27.08417473062937120, 1.503027223283688985, 1.729223128152638012 ) ) ;
#48855 = CARTESIAN_POINT ( 'NONE',  ( -35.00000000000000000, 0.9416912585474430664, 12.71517666308948513 ) ) ;
#48856 = PLANE ( 'NONE',  #1345 ) ;
#48857 = EDGE_CURVE ( 'NONE', #42299, #46364, #58422, .T. ) ;
#48858 = AXIS2_PLACEMENT_3D ( 'NONE', #61413, #30503, #10542 ) ;
#48859 = ORIENTED_EDGE ( 'NONE', *, *, #37826, .F. ) ;
#48860 = CARTESIAN_POINT ( 'NONE',  ( 0.3006302518452031447, 0.2259616664572240141, 12.25587491745529434 ) ) ;
#48861 = ORIENTED_EDGE ( 'NONE', *, *, #60782, .T. ) ;
#48862 = CARTESIAN_POINT ( 'NONE',  ( 35.00000000000000000, -8.052525312709825300, 8.551552972817161091 ) ) ;
#48863 = CARTESIAN_POINT ( 'NONE',  ( 0.2911222467163561700, -0.2144311696656475141, 12.25291251554514993 ) ) ;
#48864 = CARTESIAN_POINT ( 'NONE',  ( 11.90722734030137531, -13.26884457954574081, -2.492663574694747641 ) ) ;
#48865 = CARTESIAN_POINT ( 'NONE',  ( -22.28506771379528573, -2.697635452840746684, -2.571716811880571107 ) ) ;
#48866 = CARTESIAN_POINT ( 'NONE',  ( -37.00000000000000711, 0.000000000000000000, 0.000000000000000000 ) ) ;
#48867 = EDGE_LOOP ( 'NONE', ( #29907, #17592, #13900, #48120 ) ) ;
#48868 = DIRECTION ( 'NONE',  ( 0.000000000000000000, -0.8276889981568956722, 0.5611870653623750593 ) ) ;
#48869 = CARTESIAN_POINT ( 'NONE',  ( 37.00000000000000711, 8.954052073409734192, 9.076753354953895681 ) ) ;
#48870 = DIRECTION ( 'NONE',  ( -1.000000000000000000, 0.000000000000000000, -0.000000000000000000 ) ) ;
#48871 = CARTESIAN_POINT ( 'NONE',  ( -22.29978294495153790, 2.710748743830190932, 2.590262069787936827 ) ) ;
#48872 = AXIS2_PLACEMENT_3D ( 'NONE', #49480, #14829, #9865 ) ;
#48873 = B_SPLINE_CURVE_WITH_KNOTS ( 'NONE', 3,
 ( #34469, #65373, #9848, #65687, #60076, #30458, #20156, #24487, #40427, #15489, #60728, #10177, #44764, #50754, #19523, #5204, #25471, #39787, #45755, #34770, #20492, #40777 ),
 .UNSPECIFIED., .F., .F.,
 ( 4, 3, 3, 3, 3, 3, 3, 4 ),
 ( 0.000000000000000000, 4.455945684386670302E-05, 6.636307477203865976E-05, 8.816671873158680171E-05, 0.0001099660380492600289, 0.0001317545563165294228, 0.0001762613022895055323, 0.0001867992666138388333 ),
 .UNSPECIFIED. ) ;
#48874 = EDGE_CURVE ( 'NONE', #3473, #43566, #58478, .T. ) ;
#48875 = AXIS2_PLACEMENT_3D ( 'NONE', #41168, #15891, #62126 ) ;
#48876 = CARTESIAN_POINT ( 'NONE',  ( -35.00000000000000000, 8.573591947375437172, -8.029056188533592930 ) ) ;
#48877 = VERTEX_POINT ( 'NONE', #12910 ) ;
#48878 = EDGE_CURVE ( 'NONE', #20299, #12988, #32683, .T. ) ;
#48879 = DIRECTION ( 'NONE',  ( 1.000000000000000000, 0.000000000000000000, 0.000000000000000000 ) ) ;
#48880 = ADVANCED_FACE ( 'NONE', ( #13552 ), #25173, .T. ) ;
#48881 = CARTESIAN_POINT ( 'NONE',  ( -35.00000000000000000, 0.000000000000000000, 0.000000000000000000 ) ) ;
#48882 = DIRECTION ( 'NONE',  ( 0.000000000000000000, -0.01356324068817998940, 0.9999080150203990547 ) ) ;
#48883 = CIRCLE ( 'NONE', #32950, 2.899999999999996358 ) ;
#48884 = ORIENTED_EDGE ( 'NONE', *, *, #14472, .T. ) ;
#48886 = ORIENTED_EDGE ( 'NONE', *, *, #38456, .F. ) ;
#48885 = EDGE_CURVE ( 'NONE', #53880, #48166, #24193, .T. ) ;
#48887 = CARTESIAN_POINT ( 'NONE',  ( -22.31328051695926007, -1.671726071983958839, 3.401210163132545539 ) ) ;
#48888 = EDGE_LOOP ( 'NONE', ( #11133, #52996, #47017, #64116 ) ) ;
#48889 = CARTESIAN_POINT ( 'NONE',  ( 2.280717697723672277, 5.034569468898445699, 5.756537207046734217 ) ) ;
#48890 = CARTESIAN_POINT ( 'NONE',  ( 2.241506898688419458, -5.873558213059442146, -4.877157973187039808 ) ) ;
#48891 = CARTESIAN_POINT ( 'NONE',  ( -27.09569413923794556, -1.680421072125452664, -1.607816962454774901 ) ) ;
#48892 = CARTESIAN_POINT ( 'NONE',  ( 0.3665391374699467075, -11.44911061034383692, -4.447929964102962153 ) ) ;
#48893 = EDGE_CURVE ( 'NONE', #49332, #63687, #14847, .T. ) ;
#48894 = CARTESIAN_POINT ( 'NONE',  ( -35.04709527796842394, 0.01232256164996302361, 0.001003525937966209813 ) ) ;
#48895 = VERTEX_POINT ( 'NONE', #4248 ) ;
#48896 = EDGE_CURVE ( 'NONE', #30828, #64603, #4914, .T. ) ;
#48897 = ORIENTED_EDGE ( 'NONE', *, *, #46094, .F. ) ;
#48898 = EDGE_LOOP ( 'NONE', ( #8697, #7640, #39923, #23624 ) ) ;
#48899 = CARTESIAN_POINT ( 'NONE',  ( 35.00000000000000000, 9.493370459201798894, 6.917234959366719060 ) ) ;
#48900 = ADVANCED_FACE ( 'NONE', ( #64419 ), #20184, .T. ) ;
#48902 = CYLINDRICAL_SURFACE ( 'NONE', #59752, 12.18650000000000055 ) ;
#48901 = AXIS2_PLACEMENT_3D ( 'NONE', #34538, #3972, #59181 ) ;
#48903 = AXIS2_PLACEMENT_3D ( 'NONE', #60702, #15778, #36058 ) ;
#48904 = VECTOR ( 'NONE', #65772, 1000.000000000000000 ) ;
#48905 = ORIENTED_EDGE ( 'NONE', *, *, #48508, .F. ) ;
#48906 = B_SPLINE_CURVE_WITH_KNOTS ( 'NONE', 3,
 ( #20286, #5330, #19957, #65183, #50568, #60516, #55203, #5676, #4351, #46232, #45896, #34897, #55544, #5009, #45547, #61494, #25604, #30269, #35575 ),
 .UNSPECIFIED., .F., .F.,
 ( 4, 3, 3, 3, 3, 3, 4 ),
 ( 4.336808689942017736E-19, 2.831840207458012471E-05, 4.217266859783568754E-05, 5.602024318339777164E-05, 6.290810167913131619E-05, 9.120440630890396460E-05, 0.0001153103026480246755 ),
 .UNSPECIFIED. ) ;
#48907 = DIRECTION ( 'NONE',  ( -1.000000000000000000, 0.000000000000000000, 0.000000000000000000 ) ) ;
#48908 = EDGE_CURVE ( 'NONE', #19106, #1795, #13614, .T. ) ;
#48909 = CARTESIAN_POINT ( 'NONE',  ( -22.29677679919927868, -0.2674217835790838604, -3.730758197825084999 ) ) ;
#48910 = ORIENTED_EDGE ( 'NONE', *, *, #40179, .F. ) ;
#48911 = CARTESIAN_POINT ( 'NONE',  ( -35.00000000000000000, -12.08151691381193160, 4.074242145635959211 ) ) ;
#48912 = CARTESIAN_POINT ( 'NONE',  ( 2.000000000000001776, 0.000000000000000000, 0.000000000000000000 ) ) ;
#48913 = CARTESIAN_POINT ( 'NONE',  ( -4.590058209962335489, 6.612760447609789871, 25.00000000000000000 ) ) ;
#48914 = ORIENTED_EDGE ( 'NONE', *, *, #62247, .T. ) ;
#48916 = EDGE_CURVE ( 'NONE', #65629, #57005, #41439, .T. ) ;
#48915 = EDGE_LOOP ( 'NONE', ( #9357, #10284, #4213, #2837 ) ) ;
#48917 = CARTESIAN_POINT ( 'NONE',  ( -17.83419946441818027, -9.720786832536937538, 7.036071585506806336 ) ) ;
#48918 = B_SPLINE_CURVE_WITH_KNOTS ( 'NONE', 3,
 ( #51225, #34895, #55201, #4696, #24957, #672 ),
 .UNSPECIFIED., .F., .F.,
 ( 4, 2, 4 ),
 ( 0.0002637379172190560772, 0.0009975831966641396376, 0.001731428476109223144 ),
 .UNSPECIFIED. ) ;
#48919 = ORIENTED_EDGE ( 'NONE', *, *, #63618, .F. ) ;
#48920 = FACE_OUTER_BOUND ( 'NONE', #53311, .T. ) ;
#48921 = VERTEX_POINT ( 'NONE', #4590 ) ;
#48922 = ORIENTED_EDGE ( 'NONE', *, *, #61119, .T. ) ;
#48923 = CARTESIAN_POINT ( 'NONE',  ( 2.350038591457877413, 8.533611140766113934, -6.324706260080378506 ) ) ;
#48924 = DIRECTION ( 'NONE',  ( 1.000000000000000000, 0.000000000000000000, 0.000000000000000000 ) ) ;
#48925 = CARTESIAN_POINT ( 'NONE',  ( -13.93947072118801600, -33.60066931048471872, -9.878030726373578929 ) ) ;
#48926 = CARTESIAN_POINT ( 'NONE',  ( -22.28169757117799321, 3.576542310004398928, 0.9284931499057018645 ) ) ;
#48927 = DIRECTION ( 'NONE',  ( -1.000000000000000000, 0.000000000000000000, -0.000000000000000000 ) ) ;
#48928 = DIRECTION ( 'NONE',  ( 0.000000000000000000, 0.000000000000000000, 1.000000000000000000 ) ) ;
#48929 = ORIENTED_EDGE ( 'NONE', *, *, #8229, .F. ) ;
#48930 = VECTOR ( 'NONE', #3223, 1000.000000000000000 ) ;
#48931 = CARTESIAN_POINT ( 'NONE',  ( 2.261269890822071638, -7.131324074141565994, -2.744033622443687204 ) ) ;
#48932 = ORIENTED_EDGE ( 'NONE', *, *, #54618, .T. ) ;
#48933 = CARTESIAN_POINT ( 'NONE',  ( 2.241352910868908310, -2.689314586382399952, 7.145045428366567641 ) ) ;
#48934 = DIRECTION ( 'NONE',  ( 0.000000000000000000, -0.01356324068817998940, 0.9999080150203990547 ) ) ;
#48935 = VERTEX_POINT ( 'NONE', #24860 ) ;
#48936 = DIRECTION ( 'NONE',  ( -0.3939253465568943180, 0.9034404741085576562, -0.1691689424289672949 ) ) ;
#48937 = CARTESIAN_POINT ( 'NONE',  ( 0.3665391374699472626, -12.13918562134717760, -1.872534962004924086 ) ) ;
#48938 = CARTESIAN_POINT ( 'NONE',  ( 0.2872850955227762570, -2.333231805482910204, -12.02931961709053610 ) ) ;
#48939 = ORIENTED_EDGE ( 'NONE', *, *, #16819, .F. ) ;
#48940 = ADVANCED_FACE ( 'NONE', ( #45138 ), #14842, .T. ) ;
#48941 = VERTEX_POINT ( 'NONE', #9877 ) ;
#48942 = CARTESIAN_POINT ( 'NONE',  ( 3.031336079629770364, -7.038432939676141586, -3.582646412484407072 ) ) ;
#48943 = CIRCLE ( 'NONE', #51016, 5.000000000000000888 ) ;
#48944 = EDGE_LOOP ( 'NONE', ( #35930, #65173, #29594, #30651 ) ) ;
#48945 = CARTESIAN_POINT ( 'NONE',  ( -28.41827485489077532, 3.509237424706436403, 13.03592162821792222 ) ) ;
#48946 = CARTESIAN_POINT ( 'NONE',  ( -3.965961450091997964, -8.436165341159954423, 8.545892785218537568 ) ) ;
#48947 = CARTESIAN_POINT ( 'NONE',  ( 37.00000000000000711, 4.705694406421931860E-17, -3.469127814946512892E-15 ) ) ;
#48949 = CIRCLE ( 'NONE', #39330, 7.938172270156617749 ) ;
#48948 = DIRECTION ( 'NONE',  ( 0.000000000000000000, -0.9651210252299766701, -0.2618041379715732586 ) ) ;
#48950 = CARTESIAN_POINT ( 'NONE',  ( 0.4613984246114883336, -9.246873830555951912, 8.128335150814478993 ) ) ;
#48951 = EDGE_LOOP ( 'NONE', ( #34629, #62238, #60491, #55875 ) ) ;
#48952 = EDGE_CURVE ( 'NONE', #63399, #59829, #48883, .T. ) ;
#48953 = CARTESIAN_POINT ( 'NONE',  ( 0.3675815128205894289, 1.872154644482084684, 12.13672785388550679 ) ) ;
#48954 = CIRCLE ( 'NONE', #23441, 5.000000000000000000 ) ;
#48955 = AXIS2_PLACEMENT_3D ( 'NONE', #36447, #52073, #7159 ) ;
#48956 = EDGE_CURVE ( 'NONE', #1650, #25546, #17012, .T. ) ;
#48957 = DIRECTION ( 'NONE',  ( 1.000000000000000000, -0.000000000000000000, 0.000000000000000000 ) ) ;
#48958 =( BOUNDED_SURFACE ( )  B_SPLINE_SURFACE ( 3, 1, ( 
 ( #50528, #65457 ),
 ( #9948, #40185 ),
 ( #14274, #15575 ),
 ( #44519, #60819 ) ),
 .UNSPECIFIED., .F., .F., .T. ) 
 B_SPLINE_SURFACE_WITH_KNOTS ( ( 4, 4 ),
 ( 2, 2 ),
 ( 0.000000000000000000, 1.000000000000000000 ),
 ( 0.000000000000000000, 1.000000000000000000 ),
 .UNSPECIFIED. ) 
 GEOMETRIC_REPRESENTATION_ITEM ( )  RATIONAL_B_SPLINE_SURFACE ( (
 ( 1.000000000000000000, 1.000000000000000000),
 ( 0.9942764183789327692, 0.8450855930916585379),
 ( 0.9942764183789327692, 0.8450855930916585379),
 ( 1.000000000000000000, 1.000000000000000000) ) ) 
 REPRESENTATION_ITEM ( '' )  SURFACE ( )  );
#48959 = VECTOR ( 'NONE', #51396, 1000.000000000000000 ) ;
#48960 = DIRECTION ( 'NONE',  ( 0.000000000000000000, -0.1387779952735885280, 0.9903235168508540687 ) ) ;
#48961 = CARTESIAN_POINT ( 'NONE',  ( 37.00000000000000711, 4.705694406421931860E-17, -3.469127814946512892E-15 ) ) ;
#48962 = EDGE_CURVE ( 'NONE', #42103, #59964, #61211, .T. ) ;
#48963 = DIRECTION ( 'NONE',  ( -1.000000000000000000, -0.000000000000000000, 0.000000000000000000 ) ) ;
#48964 = CARTESIAN_POINT ( 'NONE',  ( -35.00000000000000000, 11.65554240571059275, -1.456211999474221086 ) ) ;
#48965 = DIRECTION ( 'NONE',  ( 0.000000000000000000, -0.2960891610144378849, -0.9551603052523519599 ) ) ;
#48966 = B_SPLINE_CURVE_WITH_KNOTS ( 'NONE', 3,
 ( #35221, #9290, #20266, #5312, #35559, #35862, #51208, #65163, #64818, #29915, #54868, #15597, #50222, #19296, #34879, #30561, #29576, #4993, #19940, #60497, #30252, #40208, #39565, #9618 ),
 .UNSPECIFIED., .F., .F.,
 ( 4, 2, 2, 2, 2, 2, 2, 2, 2, 2, 2, 4 ),
 ( 1.939479807224432123E-18, 0.001396101111889962859, 0.002094151667834941687, 0.002792202223779921381, 0.004188303335669874700, 0.005584404447559828018, 0.006980505559449781336, 0.008376606671339735521, 0.009074657227284713482, 0.009772707783229691442, 0.01047075833917466940, 0.01116880889511964736 ),
 .UNSPECIFIED. ) ;
#48967 = VECTOR ( 'NONE', #15013, 1000.000000000000000 ) ;
#48968 = VECTOR ( 'NONE', #25066, 1000.000000000000000 ) ;
#48969 = ORIENTED_EDGE ( 'NONE', *, *, #34232, .F. ) ;
#48970 = CARTESIAN_POINT ( 'NONE',  ( 12.75582872833425796, -11.27687878257490794, -4.107405482825274845 ) ) ;
#48971 = CIRCLE ( 'NONE', #28775, 4.999999999999999112 ) ;
#48972 = VECTOR ( 'NONE', #63523, 1000.000000000000000 ) ;
#48973 = ORIENTED_EDGE ( 'NONE', *, *, #12221, .F. ) ;
#48974 = CARTESIAN_POINT ( 'NONE',  ( -37.00000000000000711, -11.50504120060940316, -4.018060380616521599 ) ) ;
#48975 = CARTESIAN_POINT ( 'NONE',  ( -22.27704833740210333, 3.663709865074126881, -0.3581593033281141869 ) ) ;
#48976 = CARTESIAN_POINT ( 'NONE',  ( 0.2652384529303136174, 6.180212112237663646, 10.57229402027109977 ) ) ;
#48977 = CIRCLE ( 'NONE', #13907, 2.899999999999993694 ) ;
#48978 = DIRECTION ( 'NONE',  ( 0.000000000000000000, 0.000000000000000000, 1.000000000000000000 ) ) ;
#48979 = EDGE_LOOP ( 'NONE', ( #4586, #12840, #46525, #61171 ) ) ;
#48980 = CIRCLE ( 'NONE', #17052, 7.499999999999988454 ) ;
#48981 = ORIENTED_EDGE ( 'NONE', *, *, #11852, .F. ) ;
#48982 = ORIENTED_EDGE ( 'NONE', *, *, #35470, .T. ) ;
#48983 = CARTESIAN_POINT ( 'NONE',  ( -35.00000000000000000, 0.000000000000000000, 0.000000000000000000 ) ) ;
#48984 = EDGE_CURVE ( 'NONE', #26657, #40821, #61392, .T. ) ;
#48985 = CARTESIAN_POINT ( 'NONE',  ( -27.08429572838383947, 2.208905845566027537, 0.6096735944847788691 ) ) ;
#48986 = VERTEX_POINT ( 'NONE', #41776 ) ;
#48987 = EDGE_CURVE ( 'NONE', #17242, #17690, #59498, .T. ) ;
#48988 = DIRECTION ( 'NONE',  ( 1.000000000000000000, 0.000000000000000000, -0.000000000000000000 ) ) ;
#48989 = CARTESIAN_POINT ( 'NONE',  ( 2.994568964204211259, -3.069094401380829673, 7.263701055179717869 ) ) ;
#48990 = CARTESIAN_POINT ( 'NONE',  ( 0.3401186441510231084, 10.49699112323343542, 6.355596563012347211 ) ) ;
#48991 = AXIS2_PLACEMENT_3D ( 'NONE', #3717, #31560, #16278 ) ;
#48992 = CARTESIAN_POINT ( 'NONE',  ( 0.2655924914740778187, -11.52280271232873865, 4.147079829127216399 ) ) ;
#48993 = ORIENTED_EDGE ( 'NONE', *, *, #36917, .F. ) ;
#48994 = CARTESIAN_POINT ( 'NONE',  ( 37.00000000000000711, -8.954052073409666690, -9.076753354953966735 ) ) ;
#48995 = FACE_OUTER_BOUND ( 'NONE', #50820, .T. ) ;
#48996 = CARTESIAN_POINT ( 'NONE',  ( 27.62838931380291996, 25.00000000000000000, -3.066727421130092779 ) ) ;
#48998 = ORIENTED_EDGE ( 'NONE', *, *, #43430, .T. ) ;
#48997 = CARTESIAN_POINT ( 'NONE',  ( 11.99083905025487340, -8.556418439408641774, -8.415045165346302980 ) ) ;
#48999 = ADVANCED_FACE ( 'NONE', ( #62073 ), #51463, .T. ) ;
#49001 = VECTOR ( 'NONE', #50681, 1000.000000000000000 ) ;
#49000 = CARTESIAN_POINT ( 'NONE',  ( 5.516018279890452902, 0.002527316374434291236, -0.006286471671802449680 ) ) ;
#49002 = ORIENTED_EDGE ( 'NONE', *, *, #61162, .T. ) ;
#49003 = CARTESIAN_POINT ( 'NONE',  ( -20.79170840334646542, 12.91784323155722980, -3.921648409140116698 ) ) ;
#49004 = EDGE_LOOP ( 'NONE', ( #42023, #4164, #34741, #47056 ) ) ;
#49005 = CARTESIAN_POINT ( 'NONE',  ( 0.000000000000000000, 5.097042323172460421, 5.501832381651443171 ) ) ;
#49006 = CYLINDRICAL_SURFACE ( 'NONE', #9679, 12.74999999999999822 ) ;
#49007 = CARTESIAN_POINT ( 'NONE',  ( 35.00000000000000000, -6.303578524887018197, -10.42955799785318050 ) ) ;
#49008 = DIRECTION ( 'NONE',  ( 1.000000000000000000, 0.000000000000000000, 0.000000000000000000 ) ) ;
#49009 = VECTOR ( 'NONE', #13606, 1000.000000000000000 ) ;
#49010 = CIRCLE ( 'NONE', #10758, 4.999999999999999112 ) ;
#49012 = AXIS2_PLACEMENT_3D ( 'NONE', #23024, #43279, #18028 ) ;
#49011 = CARTESIAN_POINT ( 'NONE',  ( 35.00000000000000000, 10.64792938439763859, 5.927257550915197015 ) ) ;
#49013 = DIRECTION ( 'NONE',  ( -1.000000000000000000, 0.000000000000000000, 0.000000000000000000 ) ) ;
#49014 = LINE ( 'NONE', #14692, #18299 ) ;
#49015 = ORIENTED_EDGE ( 'NONE', *, *, #48789, .F. ) ;
#49016 = CARTESIAN_POINT ( 'NONE',  ( -4.975205859172449507, -1.416020129149132778, 13.42553116244733680 ) ) ;
#49017 = EDGE_LOOP ( 'NONE', ( #45711, #8346, #25603, #14806 ) ) ;
#49018 = EDGE_LOOP ( 'NONE', ( #16834, #28295, #46826, #8302 ) ) ;
#49019 = DIRECTION ( 'NONE',  ( 1.000000000000000000, 0.000000000000000000, 0.000000000000000000 ) ) ;
#49020 = CARTESIAN_POINT ( 'NONE',  ( 0.2646305136544065406, 12.08286001766535378, 1.996350543473033978 ) ) ;
#49021 = LINE ( 'NONE', #7433, #42546 ) ;
#49022 = CARTESIAN_POINT ( 'NONE',  ( -22.27706485742869091, 2.154081322712221969, 2.985151051101477382 ) ) ;
#49023 = FACE_OUTER_BOUND ( 'NONE', #48243, .T. ) ;
#49024 = CIRCLE ( 'NONE', #35156, 5.000000000000000888 ) ;
#49025 = DIRECTION ( 'NONE',  ( -0.000000000000000000, -0.000000000000000000, -1.000000000000000000 ) ) ;
#49026 = ADVANCED_FACE ( 'NONE', ( #30798, #41109, #36468, #46441, #15517, #890, #6545, #45788, #16523, #21164, #11514, #15195, #56778, #50781, #25498, #11201 ), #20524, .T. ) ;
#49027 = CARTESIAN_POINT ( 'NONE',  ( -36.00000000000000711, -12.57916205664480103, -2.080187960898693511 ) ) ;
#49028 = VECTOR ( 'NONE', #48543, 1000.000000000000000 ) ;
#49029 = EDGE_CURVE ( 'NONE', #11975, #60850, #39314, .T. ) ;
#49030 = ORIENTED_EDGE ( 'NONE', *, *, #37638, .F. ) ;
#49031 = DIRECTION ( 'NONE',  ( 1.000000000000000000, 0.000000000000000000, -0.000000000000000000 ) ) ;
#49032 = AXIS2_PLACEMENT_3D ( 'NONE', #4081, #2800, #3456 ) ;
#49033 = CARTESIAN_POINT ( 'NONE',  ( -27.08429572838383947, -1.608131779585707299, -1.632445743623455847 ) ) ;
#49034 = CYLINDRICAL_SURFACE ( 'NONE', #58329, 12.18650000000000055 ) ;
#49035 = VECTOR ( 'NONE', #45458, 1000.000000000000000 ) ;
#49036 = EDGE_CURVE ( 'NONE', #53488, #61135, #13811, .T. ) ;
#49037 = CARTESIAN_POINT ( 'NONE',  ( 35.00000000000000000, 11.44858830469736333, -2.627174906297124135 ) ) ;
#49038 = CARTESIAN_POINT ( 'NONE',  ( -37.00000000000000711, 0.000000000000000000, 0.000000000000000000 ) ) ;
#49039 = AXIS2_PLACEMENT_3D ( 'NONE', #53511, #47848, #17266 ) ;
#49040 = CARTESIAN_POINT ( 'NONE',  ( 2.241506898688418126, -2.648071636522685512, -7.160521809579523556 ) ) ;
#49041 = CARTESIAN_POINT ( 'NONE',  ( 9.039992663053343591, 3.544502836495995624, -11.46723145265938371 ) ) ;
#49042 = CIRCLE ( 'NONE', #15015, 12.74999999999999822 ) ;
#49043 = AXIS2_PLACEMENT_3D ( 'NONE', #52502, #16248, #11577 ) ;
#49045 = EDGE_LOOP ( 'NONE', ( #22381, #19871, #8162, #16034 ) ) ;
#49044 = ADVANCED_FACE ( 'NONE', ( #43083 ), #62701, .T. ) ;
#49046 = CARTESIAN_POINT ( 'NONE',  ( 9.687175622948609899, 11.98570860552671391, -0.5854820436212360146 ) ) ;
#49047 = DIRECTION ( 'NONE',  ( -1.000000000000000000, 0.000000000000000000, 0.000000000000000000 ) ) ;
#49048 = FACE_OUTER_BOUND ( 'NONE', #39241, .T. ) ;
#49049 = EDGE_CURVE ( 'NONE', #49777, #10064, #24008, .T. ) ;
#49050 = CIRCLE ( 'NONE', #16126, 5.000000000000000000 ) ;
#49051 = CIRCLE ( 'NONE', #60705, 12.18650000000000233 ) ;
#49052 = CYLINDRICAL_SURFACE ( 'NONE', #34158, 12.74999999999999822 ) ;
#49053 = LINE ( 'NONE', #13438, #64862 ) ;
#49054 = ORIENTED_EDGE ( 'NONE', *, *, #25875, .F. ) ;
#49055 = CARTESIAN_POINT ( 'NONE',  ( -16.98800322446194855, 2.922502605998049674, 13.17987020110344787 ) ) ;
#49056 = CARTESIAN_POINT ( 'NONE',  ( -9.689264015130110153, -9.446331388885504055, -7.412799815278878768 ) ) ;
#49057 = FACE_OUTER_BOUND ( 'NONE', #42263, .T. ) ;
#49058 = ORIENTED_EDGE ( 'NONE', *, *, #39024, .F. ) ;
#49059 = CARTESIAN_POINT ( 'NONE',  ( 23.30833610924781851, 11.22569009227929016, -7.505971052558499501 ) ) ;
#49060 = CARTESIAN_POINT ( 'NONE',  ( 0.2653519789438771870, -4.209148152332840453, -11.50012635727059696 ) ) ;
#49061 = EDGE_LOOP ( 'NONE', ( #44254, #13607, #14022, #5711, #22300, #33731 ) ) ;
#49062 = EDGE_LOOP ( 'NONE', ( #9079, #20173, #63669, #26467 ) ) ;
#49063 = DIRECTION ( 'NONE',  ( 0.000000000000000000, -0.07632122047555069122, 0.9970832820307048427 ) ) ;
#49064 = AXIS2_PLACEMENT_3D ( 'NONE', #6074, #30991, #51303 ) ;
#49065 = EDGE_CURVE ( 'NONE', #42272, #21980, #35031, .T. ) ;
#49066 = CIRCLE ( 'NONE', #14005, 2.899999999999994582 ) ;
#49067 = EDGE_LOOP ( 'NONE', ( #64355, #57986, #10184, #56003 ) ) ;
#49068 = CIRCLE ( 'NONE', #31009, 12.18649999999999878 ) ;
#49069 = EDGE_CURVE ( 'NONE', #7009, #7257, #27459, .T. ) ;
#49070 = CARTESIAN_POINT ( 'NONE',  ( 0.5572780756284498871, -12.09922454589796281, -2.443667122521545387 ) ) ;
#49071 = CARTESIAN_POINT ( 'NONE',  ( 2.241352910868908754, 3.889181972941541776, -6.569501556381402096 ) ) ;
#49072 = CYLINDRICAL_SURFACE ( 'NONE', #16300, 12.75000000000000178 ) ;
#49073 = DIRECTION ( 'NONE',  ( 0.000000000000000000, 1.000000000000000000, 0.000000000000000000 ) ) ;
#49074 = VECTOR ( 'NONE', #30892, 1000.000000000000000 ) ;
#49075 = CARTESIAN_POINT ( 'NONE',  ( -25.54417658651491863, 25.00000000000000000, 11.22596262356930197 ) ) ;
#49077 = VERTEX_POINT ( 'NONE', #63359 ) ;
#49076 = CARTESIAN_POINT ( 'NONE',  ( -35.00000000000000000, 0.000000000000000000, 0.000000000000000000 ) ) ;
#49078 = CYLINDRICAL_SURFACE ( 'NONE', #1214, 5.000000000000000888 ) ;
#49079 = ORIENTED_EDGE ( 'NONE', *, *, #41196, .T. ) ;
#49080 = CARTESIAN_POINT ( 'NONE',  ( -35.05175862995318425, -0.008837625261050655046, 0.008949502803489231550 ) ) ;
#49081 = VECTOR ( 'NONE', #35407, 1000.000000000000000 ) ;
#49082 = ORIENTED_EDGE ( 'NONE', *, *, #14337, .F. ) ;
#49083 = ORIENTED_EDGE ( 'NONE', *, *, #29888, .F. ) ;
#49084 = CARTESIAN_POINT ( 'NONE',  ( -25.47089039327535787, 11.72955104421914641, 6.684715474021441395 ) ) ;
#49085 = CARTESIAN_POINT ( 'NONE',  ( -12.82483530079774603, -29.99871789793389709, 7.856364084351554311 ) ) ;
#49086 = CARTESIAN_POINT ( 'NONE',  ( -25.32250750182991794, 7.778036012028926471, 11.03925478766256951 ) ) ;
#49087 = DIRECTION ( 'NONE',  ( -1.000000000000000000, 0.000000000000000000, 0.000000000000000000 ) ) ;
#49088 = DIRECTION ( 'NONE',  ( 0.000000000000000000, 0.9246979985058736418, 0.3807014730195186214 ) ) ;
#49089 = CARTESIAN_POINT ( 'NONE',  ( -47.00000000000000711, 0.000000000000000000, 0.000000000000000000 ) ) ;
#49090 = ORIENTED_EDGE ( 'NONE', *, *, #58494, .T. ) ;
#49091 = DIRECTION ( 'NONE',  ( -0.9582930651793754029, -0.2742293873734362175, 0.08045274594385933009 ) ) ;
#49092 = VERTEX_POINT ( 'NONE', #57407 ) ;
#49093 = CARTESIAN_POINT ( 'NONE',  ( 11.92180594182149456, 0.08356320926551469297, 11.99997121442060077 ) ) ;
#49094 = DIRECTION ( 'NONE',  ( 1.000000000000000000, 0.000000000000000000, -0.000000000000000000 ) ) ;
#49095 = CYLINDRICAL_SURFACE ( 'NONE', #61913, 12.18649999999999878 ) ;
#49096 = ORIENTED_EDGE ( 'NONE', *, *, #54618, .F. ) ;
#49098 = VECTOR ( 'NONE', #18223, 1000.000000000000000 ) ;
#49097 = CARTESIAN_POINT ( 'NONE',  ( 2.241352910868909643, -1.407733736974916772, 7.503490710578227585 ) ) ;
#49099 = DIRECTION ( 'NONE',  ( -1.000000000000000000, 0.000000000000000000, 0.000000000000000000 ) ) ;
#49100 = DIRECTION ( 'NONE',  ( -1.000000000000000000, 0.000000000000000000, 0.000000000000000000 ) ) ;
#49101 = CARTESIAN_POINT ( 'NONE',  ( -35.00000000000000000, 11.54110654723652196, -2.185196060783755279 ) ) ;
#49102 = AXIS2_PLACEMENT_3D ( 'NONE', #27630, #47933, #29202 ) ;
#49103 = CARTESIAN_POINT ( 'NONE',  ( 0.3675815128205894289, -12.04510820461660892, 2.391755495700564449 ) ) ;
#49104 = CARTESIAN_POINT ( 'NONE',  ( -29.65843796945371125, -0.5587665441277258616, 13.49517765288613980 ) ) ;
#49105 = CIRCLE ( 'NONE', #25722, 2.899999999999994582 ) ;
#49106 = CARTESIAN_POINT ( 'NONE',  ( -9.044148139924336860, 12.95551142774389319, -3.795959767731164725 ) ) ;
#49107 = EDGE_CURVE ( 'NONE', #11130, #34336, #18493, .T. ) ;
#49108 = ORIENTED_EDGE ( 'NONE', *, *, #60318, .F. ) ;
#49109 = ORIENTED_EDGE ( 'NONE', *, *, #26432, .T. ) ;
#49110 = LINE ( 'NONE', #24456, #4117 ) ;
#49111 = CARTESIAN_POINT ( 'NONE',  ( 2.781367136452587818, 4.783057651000514277, -6.179587792204545238 ) ) ;
#49112 = CARTESIAN_POINT ( 'NONE',  ( 35.00000000000000000, 4.705694406421931860E-17, -3.469127814946512892E-15 ) ) ;
#49113 = AXIS2_PLACEMENT_3D ( 'NONE', #51453, #56072, #20174 ) ;
#49114 = CIRCLE ( 'NONE', #53369, 6.936499999999990784 ) ;
#49115 = CARTESIAN_POINT ( 'NONE',  ( -37.00000000000000711, -11.32068061209291265, -5.865551165831199398 ) ) ;
#49116 = EDGE_CURVE ( 'NONE', #31052, #35667, #53142, .T. ) ;
#49117 = DIRECTION ( 'NONE',  ( 1.000000000000000000, 0.000000000000000000, 0.000000000000000000 ) ) ;
#49118 = AXIS2_PLACEMENT_3D ( 'NONE', #56924, #1050, #45953 ) ;
#49119 = LINE ( 'NONE', #20798, #26673 ) ;
#49120 = DIRECTION ( 'NONE',  ( 0.000000000000000000, -0.01356324068817998940, 0.9999080150203990547 ) ) ;
#49121 = CIRCLE ( 'NONE', #45925, 12.18650000000000233 ) ;
#49122 = CARTESIAN_POINT ( 'NONE',  ( -27.08456565417852602, -2.084650034355943315, -0.9533904527933274586 ) ) ;
#49123 = DIRECTION ( 'NONE',  ( 0.5702167306099040767, -0.8214942970785323872, 0.000000000000000000 ) ) ;
#49124 = ADVANCED_FACE ( 'NONE', ( #27799 ), #22827, .T. ) ;
#49125 = VERTEX_POINT ( 'NONE', #32119 ) ;
#49126 = CARTESIAN_POINT ( 'NONE',  ( -25.42680463514452427, -0.3277218550990526613, 3.871126486605850125 ) ) ;
#49127 = CYLINDRICAL_SURFACE ( 'NONE', #9978, 2.899999999999994582 ) ;
#49128 = EDGE_CURVE ( 'NONE', #30073, #50194, #56305, .T. ) ;
#49129 = CARTESIAN_POINT ( 'NONE',  ( 2.263328370261532108, -0.1420109704215282709, -7.640407877530313030 ) ) ;
#49130 = AXIS2_PLACEMENT_3D ( 'NONE', #43500, #62811, #7280 ) ;
#49131 = CARTESIAN_POINT ( 'NONE',  ( 2.258463476536644254, -5.939075453322711695, 4.806099079317522005 ) ) ;
#49132 = VERTEX_POINT ( 'NONE', #7862 ) ;
#49133 = CARTESIAN_POINT ( 'NONE',  ( -22.70624764888619751, 5.190207123845774539, 0.7939291279022917536 ) ) ;
#49134 = CARTESIAN_POINT ( 'NONE',  ( 29.72418321309294953, 10.03637985811942102, 9.031728217441806095 ) ) ;
#49135 = CARTESIAN_POINT ( 'NONE',  ( -2.167161191928854258, -27.87656208324061069, -12.44306432472098756 ) ) ;
#49136 = VERTEX_POINT ( 'NONE', #52438 ) ;
#49137 = CYLINDRICAL_SURFACE ( 'NONE', #23836, 7.499999999999988454 ) ;
#49138 = CARTESIAN_POINT ( 'NONE',  ( 0.2648978790185593790, -12.03635331166810651, -2.256510822326266652 ) ) ;
#49139 = CARTESIAN_POINT ( 'NONE',  ( 16.87411952752378852, -11.83808284204321204, 6.535263924872153574 ) ) ;
#49140 = LINE ( 'NONE', #9506, #54080 ) ;
#49141 = DIRECTION ( 'NONE',  ( 1.000000000000000000, 0.000000000000000000, 0.000000000000000000 ) ) ;
#49142 = EDGE_CURVE ( 'NONE', #11247, #21985, #216, .T. ) ;
#49143 = AXIS2_PLACEMENT_3D ( 'NONE', #62586, #53635, #32337 ) ;
#49144 = DIRECTION ( 'NONE',  ( -1.000000000000000000, 0.000000000000000000, 0.000000000000000000 ) ) ;
#49145 = ORIENTED_EDGE ( 'NONE', *, *, #52298, .T. ) ;
#49146 = DIRECTION ( 'NONE',  ( -1.000000000000000000, 0.000000000000000000, 0.000000000000000000 ) ) ;
#49147 = CARTESIAN_POINT ( 'NONE',  ( 0.3665391374699467075, -2.392238720110539951, 12.04754782681756886 ) ) ;
#49149 = CARTESIAN_POINT ( 'NONE',  ( 0.3223008802179254118, -9.550960164375549510, -7.695050880595591281 ) ) ;
#49148 =( BOUNDED_SURFACE ( )  B_SPLINE_SURFACE ( 3, 1, ( 
 ( #22905, #7598 ),
 ( #43158, #33832 ),
 ( #8571, #28858 ),
 ( #49169, #3626 ) ),
 .UNSPECIFIED., .F., .F., .F. ) 
 B_SPLINE_SURFACE_WITH_KNOTS ( ( 4, 4 ),
 ( 2, 2 ),
 ( 0.000000000000000000, 1.000000000000000000 ),
 ( 0.000000000000000000, 1.000000000000000000 ),
 .UNSPECIFIED. ) 
 GEOMETRIC_REPRESENTATION_ITEM ( )  RATIONAL_B_SPLINE_SURFACE ( (
 ( 1.000000000000000000, 1.000000000000000000),
 ( 0.6933888150995267674, 0.9895912004443193632),
 ( 0.6933888150995267674, 0.9895912004443193632),
 ( 1.000000000000000000, 1.000000000000000000) ) ) 
 REPRESENTATION_ITEM ( '' )  SURFACE ( )  );
#49150 = CARTESIAN_POINT ( 'NONE',  ( 2.000000000000001776, -6.812627895098285258, 0.04423456934719675882 ) ) ;
#49151 = CARTESIAN_POINT ( 'NONE',  ( 2.245754705088394587, 7.538396044169889620, -1.216173395688163295 ) ) ;
#49152 = DIRECTION ( 'NONE',  ( 0.000000000000000000, 0.01356324068817992175, -0.9999080150203990547 ) ) ;
#49153 = CARTESIAN_POINT ( 'NONE',  ( -28.85619398320021745, 3.750539801530000439, -11.39883551934754280 ) ) ;
#49154 = LINE ( 'NONE', #65701, #20177 ) ;
#49155 = ORIENTED_EDGE ( 'NONE', *, *, #27254, .T. ) ;
#49156 = VERTEX_POINT ( 'NONE', #60267 ) ;
#49157 = CIRCLE ( 'NONE', #28969, 12.75000000000000178 ) ;
#49158 = ORIENTED_EDGE ( 'NONE', *, *, #52394, .F. ) ;
#49159 = FILL_AREA_STYLE ('',( #45130 ) ) ;
#49160 = LINE ( 'NONE', #38500, #10023 ) ;
#49161 = EDGE_CURVE ( 'NONE', #40614, #17964, #51009, .T. ) ;
#49162 = CIRCLE ( 'NONE', #37455, 12.74999999999999822 ) ;
#49163 = CARTESIAN_POINT ( 'NONE',  ( 2.034671305879991010, -11.19279775165753854, 3.325478336154509940 ) ) ;
#49165 = CARTESIAN_POINT ( 'NONE',  ( -22.30078715814471835, -1.645949880549408162, 3.372109767220908605 ) ) ;
#49164 = B_SPLINE_CURVE_WITH_KNOTS ( 'NONE', 3,
 ( #58306, #53323, #21759, #26395, #6787, #57001, #63273, #27062, #47355, #41691, #61980, #1796, #16436, #31696 ),
 .UNSPECIFIED., .F., .F.,
 ( 4, 2, 2, 2, 2, 2, 4 ),
 ( 3.035766082959412415E-18, 0.001898234031154803509, 0.002847351046732204179, 0.003796468062309605717, 0.004745585077887007688, 0.005694702093464407491, 0.007592936124619207097 ),
 .UNSPECIFIED. ) ;
#49166 = ORIENTED_EDGE ( 'NONE', *, *, #37438, .T. ) ;
#49167 = DIRECTION ( 'NONE',  ( 0.000000000000000000, 0.000000000000000000, 1.000000000000000000 ) ) ;
#49168 = VECTOR ( 'NONE', #63508, 1000.000000000000000 ) ;
#49169 = CARTESIAN_POINT ( 'NONE',  ( 5.516018279890452902, 0.001397286410094419331, 0.006629829924290476899 ) ) ;
#49170 = CARTESIAN_POINT ( 'NONE',  ( 2.241317068080773023, -4.977030124433802882, -5.789053609344378515 ) ) ;
#49171 = EDGE_LOOP ( 'NONE', ( #40809, #31551, #44653, #60386, #49280, #12541 ) ) ;
#49172 = CIRCLE ( 'NONE', #7762, 7.499999999999988454 ) ;
#49173 = ORIENTED_EDGE ( 'NONE', *, *, #11874, .F. ) ;
#49174 = PLANE ( 'NONE',  #54429 ) ;
#49175 = CARTESIAN_POINT ( 'NONE',  ( 1.452237505248552996, 9.303501428256026884, 8.579708443906778115 ) ) ;
#49176 = ORIENTED_EDGE ( 'NONE', *, *, #7260, .F. ) ;
#49177 = ORIENTED_EDGE ( 'NONE', *, *, #1276, .F. ) ;
#49178 = CARTESIAN_POINT ( 'NONE',  ( 0.2655924914740778187, -6.084990060696436665, -10.62761259256423330 ) ) ;
#49179 = DIRECTION ( 'NONE',  ( -1.000000000000000000, 0.000000000000000000, 0.000000000000000000 ) ) ;
#49180 = CARTESIAN_POINT ( 'NONE',  ( -36.00000000000000711, -1.908798535168293897, -12.60630747491665282 ) ) ;
#49181 = DIRECTION ( 'NONE',  ( 1.000000000000000000, 0.000000000000000000, 0.000000000000000000 ) ) ;
#49182 = DIRECTION ( 'NONE',  ( 0.000000000000000000, -0.01356324068817991828, 0.9999080150203990547 ) ) ;
#49183 = CARTESIAN_POINT ( 'NONE',  ( 0.000000000000000000, 5.217815162096836268, 5.387430271863580700 ) ) ;
#49184 = EDGE_CURVE ( 'NONE', #48271, #64858, #4773, .T. ) ;
#49185 = ORIENTED_EDGE ( 'NONE', *, *, #42048, .T. ) ;
#49186 = DIRECTION ( 'NONE',  ( -1.000000000000000000, 0.000000000000000000, 0.000000000000000000 ) ) ;
#49187 = CARTESIAN_POINT ( 'NONE',  ( 0.2650492594609233366, 7.955687020697175704, -9.309909082761068433 ) ) ;
#49188 = EDGE_CURVE ( 'NONE', #64815, #57020, #7458, .T. ) ;
#49189 = LINE ( 'NONE', #29842, #14073 ) ;
#49190 = CARTESIAN_POINT ( 'NONE',  ( -35.04683013664716640, 0.002177781393214479368, -0.01216443238274463913 ) ) ;
#49192 = FACE_OUTER_BOUND ( 'NONE', #5200, .T. ) ;
#49191 = AXIS2_PLACEMENT_3D ( 'NONE', #20245, #11578, #10932 ) ;
#49193 = CARTESIAN_POINT ( 'NONE',  ( 0.3675815128205894289, 0.2638082659430137644, -12.27743992903065973 ) ) ;
#49194 = CARTESIAN_POINT ( 'NONE',  ( 2.000000000000001776, -4.570217215903394248, 5.218059682435592705 ) ) ;
#49195 = CARTESIAN_POINT ( 'NONE',  ( -37.00000000000000711, -8.624332853796127907, 9.390600770287960586 ) ) ;
#49196 = VECTOR ( 'NONE', #60097, 1000.000000000000000 ) ;
#49197 = CARTESIAN_POINT ( 'NONE',  ( 26.08439714455133185, 25.00000000000000000, 3.743551691817327942 ) ) ;
#49198 = VECTOR ( 'NONE', #11159, 1000.000000000000000 ) ;
#49199 = VECTOR ( 'NONE', #5640, 1000.000000000000000 ) ;
#49200 = VERTEX_POINT ( 'NONE', #5082 ) ;
#49201 = ADVANCED_FACE ( 'NONE', ( #72 ), #20694, .T. ) ;
#49202 = DIRECTION ( 'NONE',  ( 0.000000000000000000, 0.01356324068817998940, -0.9999080150203990547 ) ) ;
#49203 = ORIENTED_EDGE ( 'NONE', *, *, #10824, .F. ) ;
#49204 = CARTESIAN_POINT ( 'NONE',  ( 1.719304012338199517, 0.000000000000000000, 0.000000000000000000 ) ) ;
#49205 = FACE_OUTER_BOUND ( 'NONE', #58217, .T. ) ;
#49206 = DIRECTION ( 'NONE',  ( 1.000000000000000000, 0.000000000000000000, 0.000000000000000000 ) ) ;
#49207 = AXIS2_PLACEMENT_3D ( 'NONE', #64599, #19412, #40318 ) ;
#49208 = CARTESIAN_POINT ( 'NONE',  ( -25.54417658651491863, -7.498517398407823720, 11.22596262356930197 ) ) ;
#49209 = CARTESIAN_POINT ( 'NONE',  ( 2.430348790457652619, 5.095533593440028319, 5.769383131055089819 ) ) ;
#49210 = ORIENTED_EDGE ( 'NONE', *, *, #24219, .T. ) ;
#49211 = AXIS2_PLACEMENT_3D ( 'NONE', #15139, #20471, #56363 ) ;
#49212 = CARTESIAN_POINT ( 'NONE',  ( 0.3040950598368152291, 7.687624643091557353, -9.552450779732032160 ) ) ;
#49213 = DIRECTION ( 'NONE',  ( 0.000000000000000000, -0.01356324068817998940, 0.9999080150203990547 ) ) ;
#49214 = CARTESIAN_POINT ( 'NONE',  ( 9.772191328647716446, 2.017934697571601710, 11.83060272079844388 ) ) ;
#49215 = CARTESIAN_POINT ( 'NONE',  ( 13.92922077006575599, -33.59874296436084506, -9.921733781854390699 ) ) ;
#49216 = AXIS2_PLACEMENT_3D ( 'NONE', #44132, #27519, #7236 ) ;
#49217 = ADVANCED_FACE ( 'NONE', ( #28780 ), #33395, .F. ) ;
#49218 = DIRECTION ( 'NONE',  ( -1.000000000000000000, 0.000000000000000000, 0.000000000000000000 ) ) ;
#49219 = VERTEX_POINT ( 'NONE', #15677 ) ;
#49220 = AXIS2_PLACEMENT_3D ( 'NONE', #63142, #31256, #54150 ) ;
#49221 = DIRECTION ( 'NONE',  ( -1.000000000000000000, 0.000000000000000000, 0.000000000000000000 ) ) ;
#49222 = VERTEX_POINT ( 'NONE', #10369 ) ;
#49223 = DIRECTION ( 'NONE',  ( 0.000000000000000000, -0.4935949184179321825, 0.8696919319575150409 ) ) ;
#49224 = CARTESIAN_POINT ( 'NONE',  ( -7.187257474332334972, -31.45475789300513370, 14.12255545930775469 ) ) ;
#49225 = DIRECTION ( 'NONE',  ( -1.000000000000000000, 0.000000000000000000, 0.000000000000000000 ) ) ;
#49226 = DIRECTION ( 'NONE',  ( 0.000000000000000000, 0.000000000000000000, -1.000000000000000000 ) ) ;
#49227 = ORIENTED_EDGE ( 'NONE', *, *, #16886, .T. ) ;
#49228 = ORIENTED_EDGE ( 'NONE', *, *, #50213, .F. ) ;
#49229 = CARTESIAN_POINT ( 'NONE',  ( -27.10307689719060420, 2.250862122746726701, -0.6678239540327265411 ) ) ;
#49230 = CARTESIAN_POINT ( 'NONE',  ( 2.273267844204674315, 5.029122824445567908, 5.758000272829374211 ) ) ;
#49231 = LINE ( 'NONE', #64173, #13061 ) ;
#49232 = DIRECTION ( 'NONE',  ( -0.3865475372811021382, 0.4778122177792039071, 0.7888450329201760480 ) ) ;
#49233 = DIRECTION ( 'NONE',  ( 1.000000000000000000, 0.000000000000000000, 0.000000000000000000 ) ) ;
#49234 = CARTESIAN_POINT ( 'NONE',  ( -22.31099767395440736, -2.106713667647941435, -3.142100240805198563 ) ) ;
#49235 = ORIENTED_EDGE ( 'NONE', *, *, #31161, .F. ) ;
#49236 = AXIS2_PLACEMENT_3D ( 'NONE', #8554, #13534, #19534 ) ;
#49237 = CIRCLE ( 'NONE', #61984, 7.499999999999988454 ) ;
#49238 = VERTEX_POINT ( 'NONE', #55625 ) ;
#49239 = ORIENTED_EDGE ( 'NONE', *, *, #6994, .T. ) ;
#49240 = CARTESIAN_POINT ( 'NONE',  ( 0.3665391374699472626, 11.44911061034392574, -4.447929964102733003 ) ) ;
#49241 = CIRCLE ( 'NONE', #58784, 4.999999999999999112 ) ;
#49242 = ADVANCED_FACE ( 'NONE', ( #35313 ), #35643, .F. ) ;
#49244 = VECTOR ( 'NONE', #64721, 1000.000000000000114 ) ;
#49243 = DIRECTION ( 'NONE',  ( 1.000000000000000000, 0.000000000000000000, 0.000000000000000000 ) ) ;
#49245 = ORIENTED_EDGE ( 'NONE', *, *, #65327, .T. ) ;
#49246 = CARTESIAN_POINT ( 'NONE',  ( 2.000000000000001776, -6.441884263200848615, 2.217201541069723891 ) ) ;
#49247 = CARTESIAN_POINT ( 'NONE',  ( -35.04834644901396956, -0.01358669851862852156, -0.002604658385686434759 ) ) ;
#49248 = ORIENTED_EDGE ( 'NONE', *, *, #1761, .T. ) ;
#49249 = DIRECTION ( 'NONE',  ( 0.3939253465568944290, 0.4511294145502710018, 0.8008152550167613182 ) ) ;
#49250 = CARTESIAN_POINT ( 'NONE',  ( 2.273267844204864829, -2.756477528575253633, -7.130811676080301531 ) ) ;
#49251 = CARTESIAN_POINT ( 'NONE',  ( 0.000000000000000000, 0.000000000000000000, 0.000000000000000000 ) ) ;
#49252 = VERTEX_POINT ( 'NONE', #65565 ) ;
#49253 = CIRCLE ( 'NONE', #7842, 5.000000000000000000 ) ;
#49254 = EDGE_LOOP ( 'NONE', ( #10373, #22150, #16568, #28275 ) ) ;
#49255 = DIRECTION ( 'NONE',  ( -1.000000000000000000, -0.000000000000000000, -0.000000000000000000 ) ) ;
#49256 = VERTEX_POINT ( 'NONE', #45622 ) ;
#49257 = PRESENTATION_STYLE_ASSIGNMENT (( #53898 ) ) ;
#49258 = ORIENTED_EDGE ( 'NONE', *, *, #18526, .F. ) ;
#49259 = ORIENTED_EDGE ( 'NONE', *, *, #28615, .T. ) ;
#49260 = ORIENTED_EDGE ( 'NONE', *, *, #45577, .F. ) ;
#49261 = CARTESIAN_POINT ( 'NONE',  ( -35.00000000000000000, 0.000000000000000000, 0.000000000000000000 ) ) ;
#49262 = VECTOR ( 'NONE', #60994, 1000.000000000000000 ) ;
#49263 = CARTESIAN_POINT ( 'NONE',  ( -22.28506771379528573, 1.050362426369367164, 3.575989816848450076 ) ) ;
#49264 = CARTESIAN_POINT ( 'NONE',  ( 2.000000000000001776, 6.883677378339481123, -0.8544109087185395301 ) ) ;
#49265 = EDGE_CURVE ( 'NONE', #61654, #26437, #31906, .T. ) ;
#49266 = CARTESIAN_POINT ( 'NONE',  ( 2.000000000000001776, 0.000000000000000000, 0.000000000000000000 ) ) ;
#49267 = CARTESIAN_POINT ( 'NONE',  ( -22.71097035706202405, 0.4203397252017515573, -4.965150228107761521 ) ) ;
#49268 = VERTEX_POINT ( 'NONE', #40639 ) ;
#49269 = CARTESIAN_POINT ( 'NONE',  ( 2.251139882113958990, -7.133642337268841338, -2.728563091335224122 ) ) ;
#49270 = ORIENTED_EDGE ( 'NONE', *, *, #55042, .F. ) ;
#49271 = CARTESIAN_POINT ( 'NONE',  ( 2.000000000000001776, 3.795144977083636739, 6.468916029978800886 ) ) ;
#49272 = EDGE_CURVE ( 'NONE', #44677, #35395, #8511, .T. ) ;
#49273 = VECTOR ( 'NONE', #23483, 1000.000000000000000 ) ;
#49274 = CARTESIAN_POINT ( 'NONE',  ( -19.18766336847270182, -4.482615930790736058, -12.73550487531713493 ) ) ;
#49275 = EDGE_CURVE ( 'NONE', #9298, #17535, #45677, .T. ) ;
#49276 = ORIENTED_EDGE ( 'NONE', *, *, #41608, .T. ) ;
#49277 = CARTESIAN_POINT ( 'NONE',  ( 22.88594695219327235, -4.822122601967141264, 10.98850006195556261 ) ) ;
#49278 = CARTESIAN_POINT ( 'NONE',  ( 0.3160775863651097417, 3.967735865794352002, 11.60348481172936808 ) ) ;
#49279 = CARTESIAN_POINT ( 'NONE',  ( 0.2650492433740082587, -9.451472485870498375, -7.786978278830065214 ) ) ;
#49280 = ORIENTED_EDGE ( 'NONE', *, *, #279, .T. ) ;
#49281 = AXIS2_PLACEMENT_3D ( 'NONE', #29574, #45875, #50219 ) ;
#49282 = ORIENTED_EDGE ( 'NONE', *, *, #15204, .F. ) ;
#49283 = EDGE_CURVE ( 'NONE', #61894, #16455, #54155, .T. ) ;
#49284 = CARTESIAN_POINT ( 'NONE',  ( 0.6473888112830208375, 6.470260187014720721, 10.54705164520780691 ) ) ;
#49285 = ORIENTED_EDGE ( 'NONE', *, *, #2249, .F. ) ;
#49286 = EDGE_CURVE ( 'NONE', #54019, #18418, #46949, .T. ) ;
#49287 = FACE_OUTER_BOUND ( 'NONE', #341, .T. ) ;
#49288 = CARTESIAN_POINT ( 'NONE',  ( 0.4613984246114898879, 9.610550265395851000, 7.694922453052171818 ) ) ;
#49289 = CARTESIAN_POINT ( 'NONE',  ( 0.2655924914740778187, -9.352877839710547647, -7.905499957109333842 ) ) ;
#49290 = CARTESIAN_POINT ( 'NONE',  ( 3.152665057735260845, 4.377619405893435456, 6.622010822086191517 ) ) ;
#49291 = CARTESIAN_POINT ( 'NONE',  ( 11.87488961725744296, 11.87513487482758556, -1.734258419331586198 ) ) ;
#49292 = ORIENTED_EDGE ( 'NONE', *, *, #4518, .F. ) ;
#49293 = VECTOR ( 'NONE', #6029, 1000.000000000000000 ) ;
#49294 = CIRCLE ( 'NONE', #5762, 12.75000000000000178 ) ;
#49295 = CARTESIAN_POINT ( 'NONE',  ( -37.00000000000000711, 0.000000000000000000, 0.000000000000000000 ) ) ;
#49296 = CARTESIAN_POINT ( 'NONE',  ( 1.375507693218337213, 1.606074886185604678, 12.51366828189644664 ) ) ;
#49297 = AXIS2_PLACEMENT_3D ( 'NONE', #42369, #27114, #11798 ) ;
#49298 = EDGE_CURVE ( 'NONE', #45722, #8028, #61615, .T. ) ;
#49299 = CARTESIAN_POINT ( 'NONE',  ( -35.00000000000000000, -11.80185301892984384, 4.824807283154076920 ) ) ;
#49300 = AXIS2_PLACEMENT_3D ( 'NONE', #56053, #29468, #50106 ) ;
#49301 = AXIS2_PLACEMENT_3D ( 'NONE', #14473, #64050, #44740 ) ;
#49302 = EDGE_CURVE ( 'NONE', #3960, #41521, #6217, .T. ) ;
#49303 = CARTESIAN_POINT ( 'NONE',  ( -17.19821944094000088, -8.152051224790197281, 8.812769963160908659 ) ) ;
#49304 = CARTESIAN_POINT ( 'NONE',  ( -22.71097035706203116, 4.965150228107710006, 0.4203397252017151420 ) ) ;
#49305 = PRODUCT ( 'Inner cradle housing', 'Inner cradle housing', '', ( #17497 ) ) ;
#49306 = CARTESIAN_POINT ( 'NONE',  ( 0.2653519991613838003, 7.854838327448966595, 9.395283368383198663 ) ) ;
#49307 = DIRECTION ( 'NONE',  ( 0.000000000000000000, 0.01356324068817998940, -0.9999080150203990547 ) ) ;
#49308 = CARTESIAN_POINT ( 'NONE',  ( -35.00000000000000000, -1.738225594539906771, -12.63095688309030962 ) ) ;
#49309 = CIRCLE ( 'NONE', #397, 5.000000000000000000 ) ;
#49310 = AXIS2_PLACEMENT_3D ( 'NONE', #33183, #28851, #32834 ) ;
#49311 = ORIENTED_EDGE ( 'NONE', *, *, #55147, .T. ) ;
#49312 = CARTESIAN_POINT ( 'NONE',  ( -27.08456565417852602, -1.328664661355672516, -1.867985369022553188 ) ) ;
#49313 = VERTEX_POINT ( 'NONE', #11358 ) ;
#49314 = CARTESIAN_POINT ( 'NONE',  ( 0.3006302518451998140, 1.905681544119403270, -12.10891847026071488 ) ) ;
#49315 = CARTESIAN_POINT ( 'NONE',  ( -22.27722022243423794, -3.619868281251738207, 0.6721023714405491845 ) ) ;
#49316 = LINE ( 'NONE', #63911, #61886 ) ;
#49317 = AXIS2_PLACEMENT_3D ( 'NONE', #31171, #37459, #37120 ) ;
#49318 = DIRECTION ( 'NONE',  ( 1.000000000000000000, 0.000000000000000000, 0.000000000000000000 ) ) ;
#49319 = EDGE_LOOP ( 'NONE', ( #54664, #28666, #57198, #3227 ) ) ;
#49320 = ORIENTED_EDGE ( 'NONE', *, *, #46396, .T. ) ;
#49321 = VERTEX_POINT ( 'NONE', #739 ) ;
#49322 = B_SPLINE_CURVE_WITH_KNOTS ( 'NONE', 3,
 ( #44917, #39925, #61199, #15627, #60209, #34910, #5022, #60873, #15314, #55220, #29946, #50253, #24976, #52220, #42871, #37887, #6331, #58179, #36901, #61846, #2330, #62179 ),
 .UNSPECIFIED., .F., .F.,
 ( 4, 3, 3, 3, 3, 3, 3, 4 ),
 ( 5.421010862427522170E-20, 4.449119708436901857E-05, 6.626296329540710202E-05, 8.803456484962969336E-05, 0.0001098060367612836182, 0.0001315774408628541618, 0.0001760698110411196781, 0.0001829697163287832395 ),
 .UNSPECIFIED. ) ;
#49323 = CARTESIAN_POINT ( 'NONE',  ( 2.000000000000001776, 0.000000000000000000, 0.000000000000000000 ) ) ;
#49324 = EDGE_CURVE ( 'NONE', #10957, #6586, #49963, .T. ) ;
#49325 = EDGE_CURVE ( 'NONE', #30454, #36193, #58468, .T. ) ;
#49326 = AXIS2_PLACEMENT_3D ( 'NONE', #4444, #35326, #49983 ) ;
#49327 = ORIENTED_EDGE ( 'NONE', *, *, #34452, .F. ) ;
#49328 = CARTESIAN_POINT ( 'NONE',  ( -22.27720412283625961, -2.444672752438193708, -2.752887114864236651 ) ) ;
#49329 = DIRECTION ( 'NONE',  ( 0.000000000000000000, -0.01356324068817991828, 0.9999080150203990547 ) ) ;
#49330 = CARTESIAN_POINT ( 'NONE',  ( 0.3160775863651095752, 10.49803827792122668, 6.338373607799229426 ) ) ;
#49331 = CARTESIAN_POINT ( 'NONE',  ( 2.000000000000001776, -6.767909380267597363, -0.7805499053121327524 ) ) ;
#49332 = VERTEX_POINT ( 'NONE', #41281 ) ;
#49333 = DIRECTION ( 'NONE',  ( 1.000000000000000000, -0.000000000000000000, -0.000000000000000000 ) ) ;
#49334 = CARTESIAN_POINT ( 'NONE',  ( 19.43600575278776788, -28.99999999999999289, 5.424900065531946147 ) ) ;
#49335 = CARTESIAN_POINT ( 'NONE',  ( 2.263328370261531663, -1.466596409249111055, -7.499672967744989371 ) ) ;
#49337 = ORIENTED_EDGE ( 'NONE', *, *, #48952, .T. ) ;
#49336 = CARTESIAN_POINT ( 'NONE',  ( -37.00000000000000711, 2.696588552979058750, 12.46157735505190267 ) ) ;
#49338 = CARTESIAN_POINT ( 'NONE',  ( 2.000000000000001776, -3.155844197800145690, 6.177028383390419819 ) ) ;
#49339 = ORIENTED_EDGE ( 'NONE', *, *, #26149, .T. ) ;
#49340 = CIRCLE ( 'NONE', #37633, 2.899999999999994582 ) ;
#49341 = DIRECTION ( 'NONE',  ( -1.000000000000000000, 0.000000000000000000, 0.000000000000000000 ) ) ;
#49342 = EDGE_CURVE ( 'NONE', #39489, #42516, #46974, .T. ) ;
#49343 = VECTOR ( 'NONE', #50437, 1000.000000000000000 ) ;
#49344 = ORIENTED_EDGE ( 'NONE', *, *, #32074, .T. ) ;
#49345 = CARTESIAN_POINT ( 'NONE',  ( -37.00000000000000711, 0.000000000000000000, 0.000000000000000000 ) ) ;
#49346 = CARTESIAN_POINT ( 'NONE',  ( -47.00000000000000711, 0.000000000000000000, 0.000000000000000000 ) ) ;
#49347 = CARTESIAN_POINT ( 'NONE',  ( 2.241352910868908754, 2.532612177304442991, 7.202080440908749992 ) ) ;
#49348 = CARTESIAN_POINT ( 'NONE',  ( 35.00000000000000000, -11.05394794832825767, 5.130401251914841865 ) ) ;
#49349 = CARTESIAN_POINT ( 'NONE',  ( 0.3632410797595283514, 9.572936598843634570, 7.689504457927688996 ) ) ;
#49350 = EDGE_CURVE ( 'NONE', #51910, #55845, #36300, .T. ) ;
#49351 = DIRECTION ( 'NONE',  ( -1.000000000000000000, 0.000000000000000000, 0.000000000000000000 ) ) ;
#49353 = ORIENTED_EDGE ( 'NONE', *, *, #14335, .F. ) ;
#49352 = DIRECTION ( 'NONE',  ( 0.000000000000000000, 0.000000000000000000, 1.000000000000000000 ) ) ;
#49354 = ORIENTED_EDGE ( 'NONE', *, *, #41045, .F. ) ;
#49355 = DIRECTION ( 'NONE',  ( 1.000000000000000000, 0.000000000000000000, 0.000000000000000000 ) ) ;
#49356 = VERTEX_POINT ( 'NONE', #17345 ) ;
#49357 = EDGE_CURVE ( 'NONE', #21596, #2479, #9584, .T. ) ;
#49358 = ORIENTED_EDGE ( 'NONE', *, *, #21915, .F. ) ;
#49359 = AXIS2_PLACEMENT_3D ( 'NONE', #21445, #52696, #26111 ) ;
#49360 = CARTESIAN_POINT ( 'NONE',  ( 0.2655924914740778742, 6.084990060696657821, -10.62761259256410540 ) ) ;
#49361 = DIRECTION ( 'NONE',  ( 1.000000000000000000, 0.000000000000000000, -0.000000000000000000 ) ) ;
#49362 = CARTESIAN_POINT ( 'NONE',  ( 5.520433897694421610, -0.01432141647227066876, 0.004666464468077991673 ) ) ;
#49363 = CARTESIAN_POINT ( 'NONE',  ( -22.28169757117798966, 0.9841724999440121247, 3.561623073126532812 ) ) ;
#49364 = DIRECTION ( 'NONE',  ( 1.000000000000000000, 0.000000000000000000, 0.000000000000000000 ) ) ;
#49365 = CARTESIAN_POINT ( 'NONE',  ( 2.241537034860907163, -7.517665055735995416, -1.330359961362363119 ) ) ;
#49366 = LINE ( 'NONE', #39343, #23849 ) ;
#49367 =( BOUNDED_CURVE ( )  B_SPLINE_CURVE ( 3, ( #36054, #16464, #62634, #11146 ),
 .UNSPECIFIED., .F., .F. ) 
 B_SPLINE_CURVE_WITH_KNOTS ( ( 4, 4 ),
 ( 4.423281819347653965, 4.457400363100178176 ),
 .UNSPECIFIED. ) 
 CURVE ( )  GEOMETRIC_REPRESENTATION_ITEM ( )  RATIONAL_B_SPLINE_CURVE ( ( 1.000000000000000000, 0.9999029961002143807, 0.9999029961002143807, 1.000000000000000000 ) ) 
 REPRESENTATION_ITEM ( '' )  );
#49368 = VERTEX_POINT ( 'NONE', #6071 ) ;
#49369 = CIRCLE ( 'NONE', #47223, 5.000000000000000888 ) ;
#49370 = EDGE_CURVE ( 'NONE', #1207, #26844, #46775, .T. ) ;
#49371 = CARTESIAN_POINT ( 'NONE',  ( 37.00000000000000711, -1.171570255487531131, -11.68758509253248157 ) ) ;
#49372 = CARTESIAN_POINT ( 'NONE',  ( -27.08419642509983305, -1.538761233743673795, -1.697757994346420940 ) ) ;
#49373 = DIRECTION ( 'NONE',  ( 0.000000000000000000, 0.01356324068817998940, -0.9999080150203990547 ) ) ;
#49374 = ADVANCED_FACE ( 'NONE', ( #52608 ), #11677, .T. ) ;
#49375 = ORIENTED_EDGE ( 'NONE', *, *, #47031, .T. ) ;
#49376 = EDGE_CURVE ( 'NONE', #61981, #57557, #6384, .T. ) ;
#49377 = AXIS2_PLACEMENT_3D ( 'NONE', #37559, #12938, #32870 ) ;
#49378 = B_SPLINE_CURVE_WITH_KNOTS ( 'NONE', 3,
 ( #3953, #50158, #35497, #55795, #29217, #34518, #40143, #60121, #4614, #9236 ),
 .UNSPECIFIED., .F., .F.,
 ( 4, 3, 3, 4 ),
 ( 8.673617379884035472E-19, 6.607638129004469909E-05, 9.911389841680505995E-05, 0.0001667630577588622841 ),
 .UNSPECIFIED. ) ;
#49379 = EDGE_CURVE ( 'NONE', #60603, #20926, #43586, .T. ) ;
#49380 = CARTESIAN_POINT ( 'NONE',  ( -11.40165637462999904, -7.508992741355383416, 11.21895841913464409 ) ) ;
#49381 = B_SPLINE_CURVE_WITH_KNOTS ( 'NONE', 3,
 ( #44945, #33975, #24668, #49620, #59269, #60235, #54919, #59927, #53949, #48976, #3764, #3433, #23701 ),
 .UNSPECIFIED., .F., .F.,
 ( 4, 3, 3, 3, 4 ),
 ( 1.734723475976807094E-18, 6.607593386745509354E-05, 0.0001321518677373535993, 0.0001982171734706209411, 0.0002642860854759494760 ),
 .UNSPECIFIED. ) ;
#49382 = EDGE_CURVE ( 'NONE', #62542, #36458, #52099, .T. ) ;
#49383 = DIRECTION ( 'NONE',  ( 0.000000000000000000, -0.7617968321374946061, -0.6478160128811869534 ) ) ;
#49384 = ORIENTED_EDGE ( 'NONE', *, *, #55928, .T. ) ;
#49385 = DIRECTION ( 'NONE',  ( 0.000000000000000000, -0.01356324068818000848, 0.9999080150203990547 ) ) ;
#49386 = CARTESIAN_POINT ( 'NONE',  ( -37.00000000000000711, 0.000000000000000000, 0.000000000000000000 ) ) ;
#49387 = CYLINDRICAL_SURFACE ( 'NONE', #8827, 5.000000000000000888 ) ;
#49388 = DIRECTION ( 'NONE',  ( 0.000000000000000000, -1.000000000000000000, 0.000000000000000000 ) ) ;
#49389 = CARTESIAN_POINT ( 'NONE',  ( 0.3675815128205894289, 0.2638082659430137644, -12.27743992903065973 ) ) ;
#49390 = CIRCLE ( 'NONE', #52567, 5.000000000000000888 ) ;
#49391 = ORIENTED_EDGE ( 'NONE', *, *, #21634, .F. ) ;
#49392 = CARTESIAN_POINT ( 'NONE',  ( -22.27384469013076185, 3.548341908721028837, 0.9835229356381977039 ) ) ;
#49393 = CARTESIAN_POINT ( 'NONE',  ( 0.2759803524722203583, -12.09509972435083114, 1.940323823244621160 ) ) ;
#49394 = CARTESIAN_POINT ( 'NONE',  ( -17.29244623348158783, 2.525873743887551814, -11.73115347397429176 ) ) ;
#49395 = EDGE_LOOP ( 'NONE', ( #3354, #3110, #1190, #19475 ) ) ;
#49396 = LINE ( 'NONE', #29714, #40373 ) ;
#49397 = CYLINDRICAL_SURFACE ( 'NONE', #10707, 12.18649999999999878 ) ;
#49398 = ORIENTED_EDGE ( 'NONE', *, *, #24653, .T. ) ;
#49399 = VECTOR ( 'NONE', #59225, 1000.000000000000000 ) ;
#49400 = VERTEX_POINT ( 'NONE', #18983 ) ;
#49401 = CYLINDRICAL_SURFACE ( 'NONE', #38483, 5.000000000000000888 ) ;
#49402 = AXIS2_PLACEMENT_3D ( 'NONE', #25093, #51020, #20757 ) ;
#49403 = ADVANCED_FACE ( 'NONE', ( #27628 ), #63527, .T. ) ;
#49404 = EDGE_LOOP ( 'NONE', ( #61632, #38515, #27573, #6353 ) ) ;
#49405 = CYLINDRICAL_SURFACE ( 'NONE', #10052, 2.899999999999994582 ) ;
#49406 = FACE_OUTER_BOUND ( 'NONE', #63747, .T. ) ;
#49407 = CARTESIAN_POINT ( 'NONE',  ( -22.27706485742869091, 3.563814065926677710, -0.9221835209182235316 ) ) ;
#49408 = CARTESIAN_POINT ( 'NONE',  ( 2.241317068080775687, -7.533758201955906841, -1.235499051333850185 ) ) ;
#49409 = DIRECTION ( 'NONE',  ( 1.000000000000000000, 0.000000000000000000, 0.000000000000000000 ) ) ;
#49411 = ORIENTED_EDGE ( 'NONE', *, *, #45355, .T. ) ;
#49410 = DIRECTION ( 'NONE',  ( 0.000000000000000000, 0.000000000000000000, 1.000000000000000000 ) ) ;
#49412 = DIRECTION ( 'NONE',  ( -1.000000000000000000, -0.000000000000000000, -0.000000000000000000 ) ) ;
#49413 = VERTEX_POINT ( 'NONE', #37940 ) ;
#49414 = DIRECTION ( 'NONE',  ( 0.000000000000000000, -0.01356324068817998940, 0.9999080150203990547 ) ) ;
#49415 = ORIENTED_EDGE ( 'NONE', *, *, #14302, .T. ) ;
#49416 = EDGE_CURVE ( 'NONE', #44602, #28911, #41486, .T. ) ;
#49417 = VERTEX_POINT ( 'NONE', #13646 ) ;
#49418 = CARTESIAN_POINT ( 'NONE',  ( -24.81333898230430535, 10.23818681080158655, 8.801029818708748564 ) ) ;
#49419 = CARTESIAN_POINT ( 'NONE',  ( 0.9185403246812403610, -30.53691730605505228, 15.30924831176142042 ) ) ;
#49420 = CARTESIAN_POINT ( 'NONE',  ( 37.00000000000000711, 9.908974237959730758, 6.307491713048920090 ) ) ;
#49421 = AXIS2_PLACEMENT_3D ( 'NONE', #42268, #26349, #21023 ) ;
#49422 = DIRECTION ( 'NONE',  ( 1.000000000000000000, -0.000000000000000000, 0.000000000000000000 ) ) ;
#49423 = DIRECTION ( 'NONE',  ( 0.000000000000000000, -0.6269146997507876184, -0.7790879021242596014 ) ) ;
#49424 = CARTESIAN_POINT ( 'NONE',  ( 35.00000000000000000, 8.573591947375318156, -8.029056188533719052 ) ) ;
#49425 = EDGE_LOOP ( 'NONE', ( #63580, #5810, #536, #41220 ) ) ;
#49426 = ORIENTED_EDGE ( 'NONE', *, *, #29862, .F. ) ;
#49427 = CARTESIAN_POINT ( 'NONE',  ( 5.516018279890452902, -0.006286471671802459221, -0.002527316374434270853 ) ) ;
#49428 = EDGE_CURVE ( 'NONE', #36377, #56447, #53592, .T. ) ;
#49429 = ORIENTED_EDGE ( 'NONE', *, *, #19701, .T. ) ;
#49430 = CARTESIAN_POINT ( 'NONE',  ( 2.241352910868908310, -7.503490710578242684, 1.407733736974842165 ) ) ;
#49431 = CARTESIAN_POINT ( 'NONE',  ( 0.2956976708475464455, 0.2200030809427307998, -12.25433786972504890 ) ) ;
#49432 = CYLINDRICAL_SURFACE ( 'NONE', #2373, 2.899999999999994582 ) ;
#49433 = ADVANCED_FACE ( 'NONE', ( #17679 ), #8034, .T. ) ;
#49434 = DIRECTION ( 'NONE',  ( -1.000000000000000000, 0.000000000000000000, 0.000000000000000000 ) ) ;
#49435 = DIRECTION ( 'NONE',  ( -1.000000000000000000, 0.000000000000000000, 0.000000000000000000 ) ) ;
#49436 = CYLINDRICAL_SURFACE ( 'NONE', #48230, 12.74999999999999822 ) ;
#49437 = VERTEX_POINT ( 'NONE', #38257 ) ;
#49438 = AXIS2_PLACEMENT_3D ( 'NONE', #36592, #16637, #56893 ) ;
#49439 = ORIENTED_EDGE ( 'NONE', *, *, #16076, .T. ) ;
#49440 = DIRECTION ( 'NONE',  ( -1.000000000000000000, -0.000000000000000000, 0.000000000000000000 ) ) ;
#49441 = CARTESIAN_POINT ( 'NONE',  ( 37.00000000000000711, -9.390600770288051180, -8.624332853796024878 ) ) ;
#49442 = DIRECTION ( 'NONE',  ( -1.000000000000000000, 0.000000000000000000, 0.000000000000000000 ) ) ;
#49443 = ADVANCED_FACE ( 'NONE', ( #42933 ), #27980, .T. ) ;
#49444 = AXIS2_PLACEMENT_3D ( 'NONE', #43400, #63677, #58742 ) ;
#49445 = CARTESIAN_POINT ( 'NONE',  ( 1.719304012341272836, -1.452142814148833949, -12.64775761152634281 ) ) ;
#49446 = CARTESIAN_POINT ( 'NONE',  ( 2.305787727787084407, 2.461236246751170142, -7.249469779319884566 ) ) ;
#49447 = EDGE_CURVE ( 'NONE', #11603, #30420, #1172, .T. ) ;
#49448 = CARTESIAN_POINT ( 'NONE',  ( 7.290274017563119990, -6.630274286016201835, -11.76160339896002149 ) ) ;
#49449 = FACE_OUTER_BOUND ( 'NONE', #40361, .T. ) ;
#49450 = EDGE_CURVE ( 'NONE', #2058, #40710, #58233, .T. ) ;
#49451 = CARTESIAN_POINT ( 'NONE',  ( -27.09150307427447757, -2.085162835057302821, -1.001311209617661291 ) ) ;
#49452 = CARTESIAN_POINT ( 'NONE',  ( -35.00000000000000000, -11.60979404548637461, 3.704519465651263221 ) ) ;
#49453 = ORIENTED_EDGE ( 'NONE', *, *, #35330, .T. ) ;
#49454 = CARTESIAN_POINT ( 'NONE',  ( 0.000000000000000000, -4.915517050588371184, -4.717154614762162801 ) ) ;
#49455 = CARTESIAN_POINT ( 'NONE',  ( 22.21053567399755124, 13.47268488964861000, -0.8606552803710473265 ) ) ;
#49456 = B_SPLINE_CURVE_WITH_KNOTS ( 'NONE', 3,
 ( #19453, #61305, #40357, #9438, #14751, #55340, #64978, #55681, #5478, #30708, #60656, #49705, #9129 ),
 .UNSPECIFIED., .F., .F.,
 ( 4, 3, 3, 3, 4 ),
 ( 1.734723475976807094E-18, 6.607593386745476828E-05, 0.0001321518677373514309, 0.0001982171734706212663, 0.0002642860854759490966 ),
 .UNSPECIFIED. ) ;
#49457 = EDGE_CURVE ( 'NONE', #16833, #55363, #35118, .T. ) ;
#49458 = CARTESIAN_POINT ( 'NONE',  ( 2.491965175173986413, -3.673871285745626825, 6.787433375639312594 ) ) ;
#49459 = CARTESIAN_POINT ( 'NONE',  ( 2.262775599886256206, -5.943524836196959704, 4.802882839669045723 ) ) ;
#49460 = ORIENTED_EDGE ( 'NONE', *, *, #40818, .T. ) ;
#49461 = CARTESIAN_POINT ( 'NONE',  ( 2.242418902651940105, -2.517330194228340812, 7.207816731001393862 ) ) ;
#49462 = CARTESIAN_POINT ( 'NONE',  ( 5.530133899448235191, 0.008946569461392158557, -0.01324661008606532915 ) ) ;
#49463 = CARTESIAN_POINT ( 'NONE',  ( -7.278994278378053018, -26.30414574191657096, -14.75709246356266036 ) ) ;
#49464 = ORIENTED_EDGE ( 'NONE', *, *, #32416, .F. ) ;
#49465 = CARTESIAN_POINT ( 'NONE',  ( -8.333177752689428175, -1.918561656600153098, -13.36554899929619289 ) ) ;
#49466 = CYLINDRICAL_SURFACE ( 'NONE', #18301, 12.74999999999999822 ) ;
#49467 = DIRECTION ( 'NONE',  ( -1.000000000000000000, 0.000000000000000000, 0.000000000000000000 ) ) ;
#49468 = CARTESIAN_POINT ( 'NONE',  ( 0.6511581176954489569, 12.37037447926092781, 0.3309006379874227521 ) ) ;
#49469 = CARTESIAN_POINT ( 'NONE',  ( -9.614904064140660012, -12.77521411685881425, -4.380909147133119852 ) ) ;
#49470 = CARTESIAN_POINT ( 'NONE',  ( 0.6473888112830230579, 12.12394591856681991, -2.472751636945246467 ) ) ;
#49471 = ORIENTED_EDGE ( 'NONE', *, *, #45102, .F. ) ;
#49472 = CARTESIAN_POINT ( 'NONE',  ( 2.284126774967658147, -7.240052432235668967, 2.466502196988942242 ) ) ;
#49473 = EDGE_CURVE ( 'NONE', #41912, #42091, #37226, .T. ) ;
#49474 = CARTESIAN_POINT ( 'NONE',  ( -37.00000000000000711, 0.000000000000000000, 0.000000000000000000 ) ) ;
#49475 = CARTESIAN_POINT ( 'NONE',  ( -37.00000000000000711, 3.093009498344089003, -11.78745411414836752 ) ) ;
#49476 = CARTESIAN_POINT ( 'NONE',  ( -28.67667724226168602, -1.695959153103724582, -0.8389685652162183205 ) ) ;
#49477 = DIRECTION ( 'NONE',  ( 0.000000000000000000, -0.01356324068817998940, 0.9999080150203990547 ) ) ;
#49478 = DIRECTION ( 'NONE',  ( -1.000000000000000000, 0.000000000000000000, 0.000000000000000000 ) ) ;
#49479 = CARTESIAN_POINT ( 'NONE',  ( -23.18047892478189098, 3.933989833240163048, 2.738168160732657341 ) ) ;
#49480 = CARTESIAN_POINT ( 'NONE',  ( 47.00000000000000711, 4.705694406421931860E-17, -3.469127814946512892E-15 ) ) ;
#49481 = VERTEX_POINT ( 'NONE', #13973 ) ;
#49482 = ORIENTED_EDGE ( 'NONE', *, *, #5097, .F. ) ;
#49483 = ORIENTED_EDGE ( 'NONE', *, *, #38765, .T. ) ;
#49484 = SURFACE_STYLE_FILL_AREA ( #49159 ) ;
#49485 = VECTOR ( 'NONE', #22395, 1000.000000000000114 ) ;
#49486 = DIRECTION ( 'NONE',  ( 1.000000000000000000, 0.000000000000000000, -0.000000000000000000 ) ) ;
#49487 = B_SPLINE_CURVE_WITH_KNOTS ( 'NONE', 3,
 ( #4090, #7776, #24359, #8104, #17754, #53979, #64581, #59626, #8423, #58316, #3795, #28062, #2809, #23070, #18424, #43327, #29041, #63604, #18078, #49349, #19055, #58992 ),
 .UNSPECIFIED., .F., .F.,
 ( 4, 3, 3, 3, 3, 3, 3, 4 ),
 ( 1.951563910473907981E-18, 4.449119708436932350E-05, 6.626296329540588229E-05, 8.803456484962986954E-05, 0.0001098060367612875891, 0.0001315774408628584986, 0.0001760698110411265628, 0.0001829697163287840526 ),
 .UNSPECIFIED. ) ;
#49488 = DIRECTION ( 'NONE',  ( 1.000000000000000000, -0.000000000000000000, -0.000000000000000000 ) ) ;
#49489 = VERTEX_POINT ( 'NONE', #22993 ) ;
#49490 = CARTESIAN_POINT ( 'NONE',  ( 35.00000000000000000, 4.705694406421931860E-17, -3.469127814946512892E-15 ) ) ;
#49491 = DIRECTION ( 'NONE',  ( 0.000000000000000000, 0.6876994588534246500, -0.7259954919231293990 ) ) ;
#49492 = CARTESIAN_POINT ( 'NONE',  ( -35.00000000000000000, -11.02904044024211849, 4.041347439435823752 ) ) ;
#49493 = ORIENTED_EDGE ( 'NONE', *, *, #59345, .T. ) ;
#49494 = ORIENTED_EDGE ( 'NONE', *, *, #31128, .T. ) ;
#49495 = CARTESIAN_POINT ( 'NONE',  ( 2.288423627607476085, -7.242304196986135700, -2.464337058688830684 ) ) ;
#49496 = EDGE_CURVE ( 'NONE', #35321, #36878, #48287, .T. ) ;
#49497 = FACE_OUTER_BOUND ( 'NONE', #65164, .T. ) ;
#49498 = ORIENTED_EDGE ( 'NONE', *, *, #40382, .F. ) ;
#49499 = CARTESIAN_POINT ( 'NONE',  ( 4.040225803495397727, -10.40460620550539161, -5.985298750905354126 ) ) ;
#49500 = VERTEX_POINT ( 'NONE', #38606 ) ;
#49501 = CARTESIAN_POINT ( 'NONE',  ( 37.00000000000000711, -9.217970097227780713, -7.971186206369443639 ) ) ;
#49502 = EDGE_CURVE ( 'NONE', #7744, #10208, #1751, .T. ) ;
#49503 = DIRECTION ( 'NONE',  ( 0.000000000000000000, 0.01356324068817998940, -0.9999080150203989437 ) ) ;
#49504 = DIRECTION ( 'NONE',  ( -1.000000000000000000, 0.000000000000000000, 0.000000000000000000 ) ) ;
#49505 = CARTESIAN_POINT ( 'NONE',  ( 5.516018279890452902, 0.006771744149385265123, -0.0002248006052448750405 ) ) ;
#49506 = CARTESIAN_POINT ( 'NONE',  ( 0.2671309869109469437, 11.56263543972758967, 4.036029264453025789 ) ) ;
#49507 = VERTEX_POINT ( 'NONE', #28959 ) ;
#49508 = CARTESIAN_POINT ( 'NONE',  ( 3.152665057734126197, -1.848755561852092333, 7.719888720907804647 ) ) ;
#49509 = CARTESIAN_POINT ( 'NONE',  ( -16.60799812198239778, 7.628243526059563351, 9.263658496022879163 ) ) ;
#49510 = CARTESIAN_POINT ( 'NONE',  ( -19.31247144139280181, -13.48787587759413142, -0.6540986653347018454 ) ) ;
#49511 = CARTESIAN_POINT ( 'NONE',  ( 35.00000000000000000, 8.496612874013157679, -9.506317355798403312 ) ) ;
#49512 = CARTESIAN_POINT ( 'NONE',  ( 35.00000000000000000, -3.704519465651390675, -11.60979404548633731 ) ) ;
#49513 = CARTESIAN_POINT ( 'NONE',  ( -22.59983133926799326, -4.058100437359466461, 2.272383229042392205 ) ) ;
#49514 = CARTESIAN_POINT ( 'NONE',  ( -37.00000000000000711, 0.000000000000000000, 0.000000000000000000 ) ) ;
#49515 = DIRECTION ( 'NONE',  ( 0.000000000000000000, -0.01356324068817998940, 0.9999080150203990547 ) ) ;
#49516 = DIRECTION ( 'NONE',  ( 0.3939253465568944290, -0.4511294145502765529, -0.8008152550167580985 ) ) ;
#49517 = EDGE_CURVE ( 'NONE', #34961, #50103, #43925, .T. ) ;
#49518 = ORIENTED_EDGE ( 'NONE', *, *, #64493, .T. ) ;
#49519 = CARTESIAN_POINT ( 'NONE',  ( 0.2958664285830424068, 0.2205161970874386923, 12.25438626999990177 ) ) ;
#49520 = CIRCLE ( 'NONE', #45232, 12.74999999999999822 ) ;
#49521 = AXIS2_PLACEMENT_3D ( 'NONE', #10738, #31027, #6754 ) ;
#49522 = ORIENTED_EDGE ( 'NONE', *, *, #39924, .T. ) ;
#49523 = CARTESIAN_POINT ( 'NONE',  ( 1.452237505248555660, 8.579708443906746140, 9.303501428256057082 ) ) ;
#49524 = CARTESIAN_POINT ( 'NONE',  ( 2.247206125382828379, -7.499376972323885227, -1.439877054338178475 ) ) ;
#49525 = CARTESIAN_POINT ( 'NONE',  ( 2.241352910868908754, -4.843133558968167662, 5.901537464758438212 ) ) ;
#49526 = CARTESIAN_POINT ( 'NONE',  ( -35.00000000000000000, 10.14408668126213442, 5.921969905510389154 ) ) ;
#49527 = FACE_OUTER_BOUND ( 'NONE', #7985, .T. ) ;
#49528 = ORIENTED_EDGE ( 'NONE', *, *, #12955, .F. ) ;
#49529 = CARTESIAN_POINT ( 'NONE',  ( 2.034671305879538039, 0.7032348381694819572, -11.65517003034116605 ) ) ;
#49530 = CARTESIAN_POINT ( 'NONE',  ( 0.2648978790185602672, 1.996248716311790128, -12.08224454301446826 ) ) ;
#49531 = DIRECTION ( 'NONE',  ( -1.000000000000000000, 0.000000000000000000, 0.000000000000000000 ) ) ;
#49532 = CARTESIAN_POINT ( 'NONE',  ( 13.29259107886408131, -33.36832009551300615, -10.54479676546161926 ) ) ;
#49533 = EDGE_CURVE ( 'NONE', #11516, #41856, #42530, .T. ) ;
#49534 = DIRECTION ( 'NONE',  ( 0.000000000000000000, 0.9635499925192236859, -0.2675283385292183680 ) ) ;
#49535 =( BOUNDED_SURFACE ( )  B_SPLINE_SURFACE ( 3, 1, ( 
 ( #1643, #17583 ),
 ( #57828, #31859 ),
 ( #52515, #32191 ),
 ( #42159, #6627 ) ),
 .UNSPECIFIED., .F., .F., .F. ) 
 B_SPLINE_SURFACE_WITH_KNOTS ( ( 4, 4 ),
 ( 2, 2 ),
 ( 0.000000000000000000, 1.000000000000000000 ),
 ( 0.000000000000000000, 1.000000000000000000 ),
 .UNSPECIFIED. ) 
 GEOMETRIC_REPRESENTATION_ITEM ( )  RATIONAL_B_SPLINE_SURFACE ( (
 ( 1.000000000000000000, 1.000000000000000000),
 ( 0.6933888150995267674, 0.9895912004443193632),
 ( 0.6933888150995267674, 0.9895912004443193632),
 ( 1.000000000000000000, 1.000000000000000000) ) ) 
 REPRESENTATION_ITEM ( '' )  SURFACE ( )  );
#49536 = VERTEX_POINT ( 'NONE', #60188 ) ;
#49537 = DIRECTION ( 'NONE',  ( 1.000000000000000000, 0.000000000000000000, 0.000000000000000000 ) ) ;
#49538 = ORIENTED_EDGE ( 'NONE', *, *, #25581, .F. ) ;
#49539 = CYLINDRICAL_SURFACE ( 'NONE', #37864, 12.18650000000000055 ) ;
#49540 = DIRECTION ( 'NONE',  ( 0.000000000000000000, -0.6478160128812003871, 0.7617968321374830598 ) ) ;
#49541 = DIRECTION ( 'NONE',  ( 1.000000000000000000, -0.000000000000000000, -0.000000000000000000 ) ) ;
#49542 = CARTESIAN_POINT ( 'NONE',  ( -29.68541646480307250, -2.175302793937436974, -13.34544795947793716 ) ) ;
#49543 = ORIENTED_EDGE ( 'NONE', *, *, #3419, .F. ) ;
#49544 = ORIENTED_EDGE ( 'NONE', *, *, #26051, .F. ) ;
#49545 = CARTESIAN_POINT ( 'NONE',  ( -27.08702828306176258, 2.216258174335476561, -0.6138566972905349362 ) ) ;
#49546 = EDGE_CURVE ( 'NONE', #6221, #61765, #16003, .T. ) ;
#49547 = CARTESIAN_POINT ( 'NONE',  ( 2.241352910868908310, 4.970878533273761946, 5.794346703933863196 ) ) ;
#49548 = CARTESIAN_POINT ( 'NONE',  ( 2.241449424704146320, -5.887589908049611687, -4.860179885671861655 ) ) ;
#49549 = DIRECTION ( 'NONE',  ( 0.000000000000000000, -0.2149704402110318713, 0.9766205557100849921 ) ) ;
#49550 = DIRECTION ( 'NONE',  ( 0.000000000000000000, -0.5472293298355156432, 0.8369827122275419473 ) ) ;
#49551 = DIRECTION ( 'NONE',  ( 0.000000000000000000, 0.000000000000000000, 1.000000000000000000 ) ) ;
#49552 = CARTESIAN_POINT ( 'NONE',  ( 1.462291587749891209, -12.62932306616585798, -0.6330131614654728178 ) ) ;
#49553 = EDGE_CURVE ( 'NONE', #51541, #22230, #26350, .T. ) ;
#49554 = ORIENTED_EDGE ( 'NONE', *, *, #15098, .T. ) ;
#49555 = ORIENTED_EDGE ( 'NONE', *, *, #55172, .F. ) ;
#49556 = ORIENTED_EDGE ( 'NONE', *, *, #64607, .F. ) ;
#49557 = AXIS2_PLACEMENT_3D ( 'NONE', #48667, #53662, #8100 ) ;
#49558 = DIRECTION ( 'NONE',  ( 0.000000000000000000, -0.01356324068817998073, 0.9999080150203990547 ) ) ;
#49559 = CARTESIAN_POINT ( 'NONE',  ( 2.406456491627778860, 10.41426194694948038, -0.6290357040717751147 ) ) ;
#49560 = EDGE_CURVE ( 'NONE', #52831, #36393, #48980, .T. ) ;
#49561 = ORIENTED_EDGE ( 'NONE', *, *, #35566, .T. ) ;
#49562 = CIRCLE ( 'NONE', #46372, 5.000000000000000888 ) ;
#49563 = CARTESIAN_POINT ( 'NONE',  ( 3.347841273039249721, -10.61118957148187825, 25.00000000000000000 ) ) ;
#49564 = CARTESIAN_POINT ( 'NONE',  ( 0.000000000000000000, 5.814643797626986910, -3.550179297009520063 ) ) ;
#49565 = ORIENTED_EDGE ( 'NONE', *, *, #63115, .T. ) ;
#49566 = CARTESIAN_POINT ( 'NONE',  ( -22.71097035706202760, 2.846599994298365743, -4.089776368546553798 ) ) ;
#49567 = DIRECTION ( 'NONE',  ( 0.000000000000000000, -0.01356324068817992175, 0.9999080150203990547 ) ) ;
#49568 = CARTESIAN_POINT ( 'NONE',  ( 1.000000000000000888, -5.662015959325215952, 4.918493191653933394 ) ) ;
#49569 = ORIENTED_EDGE ( 'NONE', *, *, #57575, .T. ) ;
#49570 = ORIENTED_EDGE ( 'NONE', *, *, #51423, .T. ) ;
#49571 = CARTESIAN_POINT ( 'NONE',  ( -35.00000000000000000, 0.000000000000000000, 0.000000000000000000 ) ) ;
#49572 = VERTEX_POINT ( 'NONE', #54880 ) ;
#49573 = EDGE_CURVE ( 'NONE', #49489, #21740, #13859, .T. ) ;
#49574 = DIRECTION ( 'NONE',  ( -1.000000000000000000, 0.000000000000000000, 0.000000000000000000 ) ) ;
#49575 = ORIENTED_EDGE ( 'NONE', *, *, #6039, .T. ) ;
#49576 = EDGE_LOOP ( 'NONE', ( #28453, #56591, #62532, #43806 ) ) ;
#49577 = VERTEX_POINT ( 'NONE', #59882 ) ;
#49578 = CARTESIAN_POINT ( 'NONE',  ( -2.952869152607111136, 25.00000000000000000, 11.17020052527586138 ) ) ;
#49579 = CARTESIAN_POINT ( 'NONE',  ( 35.00000000000000000, -10.42955799785315563, 6.303578524887051948 ) ) ;
#49580 = CARTESIAN_POINT ( 'NONE',  ( 37.00000000000000711, 4.705694406421931860E-17, -3.469127814946512892E-15 ) ) ;
#49581 = CARTESIAN_POINT ( 'NONE',  ( 1.549075743845464759, -0.6747257554049737038, 12.65619669351041487 ) ) ;
#49582 = ORIENTED_EDGE ( 'NONE', *, *, #7253, .T. ) ;
#49583 = CARTESIAN_POINT ( 'NONE',  ( 39.82770826892757299, -25.90431001312668968, 4.499999999999997335 ) ) ;
#49584 = ORIENTED_EDGE ( 'NONE', *, *, #15174, .T. ) ;
#49585 = CARTESIAN_POINT ( 'NONE',  ( 2.000000000000001776, 0.000000000000000000, 0.000000000000000000 ) ) ;
#49586 = CARTESIAN_POINT ( 'NONE',  ( -17.76813863392193582, -8.408734016395053246, -10.56536593579148153 ) ) ;
#49587 = VERTEX_POINT ( 'NONE', #14304 ) ;
#49588 = LINE ( 'NONE', #24295, #61506 ) ;
#49589 = CARTESIAN_POINT ( 'NONE',  ( 0.3002738374340838678, 3.979745968261205302, 11.59380198135583484 ) ) ;
#49590 = CARTESIAN_POINT ( 'NONE',  ( 0.000000000000000000, -0.4804830611970390408, 6.919838746524553663 ) ) ;
#49591 = ORIENTED_EDGE ( 'NONE', *, *, #3897, .F. ) ;
#49592 = ORIENTED_EDGE ( 'NONE', *, *, #21396, .T. ) ;
#49593 = CARTESIAN_POINT ( 'NONE',  ( -22.27218376572352554, 1.571356284315160501, -3.330959526935376225 ) ) ;
#49594 = ORIENTED_EDGE ( 'NONE', *, *, #23288, .F. ) ;
#49595 = DIRECTION ( 'NONE',  ( 1.000000000000000000, 0.000000000000000000, 0.000000000000000000 ) ) ;
#49596 = FACE_OUTER_BOUND ( 'NONE', #12543, .T. ) ;
#49597 = CARTESIAN_POINT ( 'NONE',  ( 2.994568964204211259, 7.020079750321941425, -3.591541975631893369 ) ) ;
#49598 = CARTESIAN_POINT ( 'NONE',  ( 0.3053067050349172473, -9.241336250185305801, -8.055646999028104105 ) ) ;
#49599 = CARTESIAN_POINT ( 'NONE',  ( -35.00000000000000000, 9.621072037177116343, -8.366449238204259231 ) ) ;
#49600 = ORIENTED_EDGE ( 'NONE', *, *, #53045, .T. ) ;
#49601 = EDGE_CURVE ( 'NONE', #43917, #36445, #40223, .T. ) ;
#49602 = CARTESIAN_POINT ( 'NONE',  ( -27.10719052120871098, -1.622102031466687189, 1.714424047991066846 ) ) ;
#49603 = AXIS2_PLACEMENT_3D ( 'NONE', #6382, #60931, #10694 ) ;
#49604 = CARTESIAN_POINT ( 'NONE',  ( 0.8375941296797054791, 1.780036797758661526, 12.30893872205235340 ) ) ;
#49605 = ADVANCED_FACE ( 'NONE', ( #4018 ), #4695, .T. ) ;
#49606 = AXIS2_PLACEMENT_3D ( 'NONE', #54929, #55604, #25325 ) ;
#49607 = DIRECTION ( 'NONE',  ( 0.000000000000000000, 0.000000000000000000, 1.000000000000000000 ) ) ;
#49608 = FACE_OUTER_BOUND ( 'NONE', #46862, .T. ) ;
#49609 = CARTESIAN_POINT ( 'NONE',  ( 1.937114397841935398, 11.72279974487470788, -5.226660192101475033 ) ) ;
#49610 = DIRECTION ( 'NONE',  ( -1.000000000000000000, 0.000000000000000000, 0.000000000000000000 ) ) ;
#49611 = CARTESIAN_POINT ( 'NONE',  ( -35.00000000000000000, 0.000000000000000000, 0.000000000000000000 ) ) ;
#49612 = ADVANCED_FACE ( 'NONE', ( #40561, #4347 ), #24956, .F. ) ;
#49613 = VERTEX_POINT ( 'NONE', #65488 ) ;
#49614 = DIRECTION ( 'NONE',  ( 0.000000000000000000, 0.9903235168508544017, 0.1387779952735853917 ) ) ;
#49616 = VERTEX_POINT ( 'NONE', #9986 ) ;
#49615 = ADVANCED_FACE ( 'NONE', ( #44551 ), #60513, .T. ) ;
#49617 = CARTESIAN_POINT ( 'NONE',  ( 0.3632410797595244656, 1.872837903657359027, -12.13515851238021703 ) ) ;
#49618 = EDGE_CURVE ( 'NONE', #3042, #11376, #19311, .T. ) ;
#49619 = CARTESIAN_POINT ( 'NONE',  ( -22.27218376572352554, 3.026314224080938864, -2.099017427146244952 ) ) ;
#49620 = CARTESIAN_POINT ( 'NONE',  ( 0.2652384770603652409, 6.065775245581168207, 10.63836422907226975 ) ) ;
#49621 = DIRECTION ( 'NONE',  ( -1.000000000000000000, 0.000000000000000000, 0.000000000000000000 ) ) ;
#49622 = EDGE_CURVE ( 'NONE', #22141, #12853, #25553, .T. ) ;
#49623 = ORIENTED_EDGE ( 'NONE', *, *, #55311, .T. ) ;
#49624 = EDGE_LOOP ( 'NONE', ( #34901, #17399, #17952, #25577 ) ) ;
#49625 = ORIENTED_EDGE ( 'NONE', *, *, #37664, .F. ) ;
#49626 = LINE ( 'NONE', #64251, #51447 ) ;
#49627 = CARTESIAN_POINT ( 'NONE',  ( 2.000000000000001776, 6.441884263200815752, 2.217201541069855786 ) ) ;
#49628 = EDGE_CURVE ( 'NONE', #58596, #22365, #61668, .T. ) ;
#49629 = VERTEX_POINT ( 'NONE', #40910 ) ;
#49630 = CARTESIAN_POINT ( 'NONE',  ( -22.27720387087365239, -2.302200479844928260, -2.873095842208896578 ) ) ;
#49631 = DIRECTION ( 'NONE',  ( 0.000000000000000000, 0.000000000000000000, -1.000000000000000000 ) ) ;
#49632 = CARTESIAN_POINT ( 'NONE',  ( 0.3223008802179253007, -9.236652594547187789, 8.069628056118085979 ) ) ;
#49633 = DIRECTION ( 'NONE',  ( -1.000000000000000000, 0.000000000000000000, 0.000000000000000000 ) ) ;
#49634 = ORIENTED_EDGE ( 'NONE', *, *, #23022, .T. ) ;
#49635 = CARTESIAN_POINT ( 'NONE',  ( 36.00000000000000711, -7.745827850123079727, -10.12742074351894317 ) ) ;
#49636 = EDGE_CURVE ( 'NONE', #65189, #61311, #36168, .T. ) ;
#49637 = CARTESIAN_POINT ( 'NONE',  ( -8.269707202464296358, -27.33416996378218755, -14.97774446421700922 ) ) ;
#49638 = CARTESIAN_POINT ( 'NONE',  ( 2.257661810676422132, -1.459225434025932300, -7.499185766072603343 ) ) ;
#49640 = EDGE_LOOP ( 'NONE', ( #19203, #34880, #58042, #42114 ) ) ;
#49639 = CARTESIAN_POINT ( 'NONE',  ( 37.00000000000000711, 4.705694406421931860E-17, -3.469127814946512892E-15 ) ) ;
#49641 = CARTESIAN_POINT ( 'NONE',  ( 0.3040950598368152291, 5.912066680610761793, -10.74226959800785153 ) ) ;
#49642 = ORIENTED_EDGE ( 'NONE', *, *, #15462, .T. ) ;
#49643 = CARTESIAN_POINT ( 'NONE',  ( 1.287602823386838402, -9.987902848013685997, 7.659913635101823104 ) ) ;
#49644 = ORIENTED_EDGE ( 'NONE', *, *, #55475, .F. ) ;
#49645 = AXIS2_PLACEMENT_3D ( 'NONE', #37195, #37542, #51862 ) ;
#49646 = DIRECTION ( 'NONE',  ( 1.000000000000000000, -0.000000000000000000, -0.000000000000000000 ) ) ;
#49647 = DIRECTION ( 'NONE',  ( -1.000000000000000000, 0.000000000000000000, 0.000000000000000000 ) ) ;
#49648 = DIRECTION ( 'NONE',  ( 1.000000000000000000, -0.000000000000000000, 0.000000000000000000 ) ) ;
#49649 = CARTESIAN_POINT ( 'NONE',  ( 35.00000000000000000, 4.705694406421931860E-17, -3.469127814946512892E-15 ) ) ;
#49650 = FACE_OUTER_BOUND ( 'NONE', #10940, .T. ) ;
#49651 = AXIS2_PLACEMENT_3D ( 'NONE', #30721, #20438, #4835 ) ;
#49652 = CARTESIAN_POINT ( 'NONE',  ( -27.09861164373156228, -0.1603819633258334043, -2.328930759213686752 ) ) ;
#49653 = CARTESIAN_POINT ( 'NONE',  ( -36.00000000000000711, -10.02106554660702997, -7.882940143791884680 ) ) ;
#49655 = ORIENTED_EDGE ( 'NONE', *, *, #15462, .F. ) ;
#49654 = CARTESIAN_POINT ( 'NONE',  ( -36.00000000000000711, 8.830544224262947495, 9.196955404009329982 ) ) ;
#49656 = EDGE_CURVE ( 'NONE', #50600, #7923, #23476, .T. ) ;
#49657 = ORIENTED_EDGE ( 'NONE', *, *, #49265, .T. ) ;
#49658 = CARTESIAN_POINT ( 'NONE',  ( 5.516018279890452902, 0.002527316374434291236, -0.006286471671802449680 ) ) ;
#49659 = EDGE_LOOP ( 'NONE', ( #26084, #18635, #62248, #40587 ) ) ;
#49660 = ORIENTED_EDGE ( 'NONE', *, *, #52214, .F. ) ;
#49661 = DIRECTION ( 'NONE',  ( 0.000000000000000000, 0.01356324068817998940, -0.9999080150203990547 ) ) ;
#49662 = DIRECTION ( 'NONE',  ( 0.000000000000000000, 0.9635499925192217985, 0.2675283385292246963 ) ) ;
#49663 = CARTESIAN_POINT ( 'NONE',  ( -27.28573687977896256, -1.043905432732877392, -2.702109387930243578 ) ) ;
#49664 = CARTESIAN_POINT ( 'NONE',  ( 0.2638984909335720941, -8.023974293733116880, -9.252728947331158693 ) ) ;
#49665 = CARTESIAN_POINT ( 'NONE',  ( -22.30527770659433529, 1.656864125491268824, -3.381761229713376338 ) ) ;
#49666 = CARTESIAN_POINT ( 'NONE',  ( -35.00000000000000000, 0.000000000000000000, 0.000000000000000000 ) ) ;
#49667 = DIRECTION ( 'NONE',  ( 0.000000000000000000, 0.000000000000000000, 1.000000000000000000 ) ) ;
#49668 = ORIENTED_EDGE ( 'NONE', *, *, #10804, .F. ) ;
#49669 = CARTESIAN_POINT ( 'NONE',  ( -37.00000000000000711, 0.000000000000000000, 0.000000000000000000 ) ) ;
#49670 = FACE_OUTER_BOUND ( 'NONE', #32853, .T. ) ;
#49671 = CARTESIAN_POINT ( 'NONE',  ( 0.2653141334712564303, -7.905403790036909406, -9.352759824582582482 ) ) ;
#49672 = ORIENTED_EDGE ( 'NONE', *, *, #25939, .T. ) ;
#49673 = AXIS2_PLACEMENT_3D ( 'NONE', #8993, #30567, #13964 ) ;
#49674 = ADVANCED_FACE ( 'NONE', ( #347 ), #20625, .T. ) ;
#49675 = CIRCLE ( 'NONE', #39075, 5.000000000000002665 ) ;
#49676 = CARTESIAN_POINT ( 'NONE',  ( -11.27062903137229810, -6.186534743127487523, 12.00099709470298315 ) ) ;
#49677 = B_SPLINE_CURVE_WITH_KNOTS ( 'NONE', 3,
 ( #48564, #8006, #54537, #48889, #64172, #49230, #23616, #3686, #33251, #44518, #29553, #38223, #58544, #38570, #28924, #59194, #8969, #29251, #49547 ),
 .UNSPECIFIED., .F., .F.,
 ( 4, 3, 3, 3, 3, 3, 4 ),
 ( 6.992893892674702526E-18, 2.825908398850998936E-05, 4.208813692510701612E-05, 5.591713746977713896E-05, 6.279584083269157033E-05, 9.105792820349262943E-05, 0.0001153131102488628534 ),
 .UNSPECIFIED. ) ;
#49678 = CARTESIAN_POINT ( 'NONE',  ( 2.000000000000001776, 5.457833520448658327, 4.281014542496528463 ) ) ;
#49679 = ORIENTED_EDGE ( 'NONE', *, *, #52551, .F. ) ;
#49680 = CARTESIAN_POINT ( 'NONE',  ( 2.941278708680199916, 3.185832147968520545, -5.248410529370191924 ) ) ;
#49681 = DIRECTION ( 'NONE',  ( -1.000000000000000000, -0.000000000000000000, 0.000000000000000000 ) ) ;
#49682 = CARTESIAN_POINT ( 'NONE',  ( 1.658631356726815387, 0.7601067232070346513, 11.97997174763777650 ) ) ;
#49683 = AXIS2_PLACEMENT_3D ( 'NONE', #42673, #10798, #46703 ) ;
#49684 = EDGE_CURVE ( 'NONE', #37589, #22708, #15223, .T. ) ;
#49685 = CIRCLE ( 'NONE', #25228, 12.18650000000000233 ) ;
#49686 = LINE ( 'NONE', #40684, #10811 ) ;
#49687 = CARTESIAN_POINT ( 'NONE',  ( 35.00000000000000000, 11.56998259273182583, 3.827046518384956020 ) ) ;
#49688 = ORIENTED_EDGE ( 'NONE', *, *, #53695, .T. ) ;
#49689 = EDGE_CURVE ( 'NONE', #55692, #53292, #32990, .T. ) ;
#49690 = CARTESIAN_POINT ( 'NONE',  ( 22.36482863261543486, 13.46837713145128923, -0.9234811557364158707 ) ) ;
#49691 = CARTESIAN_POINT ( 'NONE',  ( 0.000000000000000000, 0.000000000000000000, 0.000000000000000000 ) ) ;
#49692 = CARTESIAN_POINT ( 'NONE',  ( -35.04582288351658548, 0.01092946910272441126, -0.006479247284622759000 ) ) ;
#49693 = ORIENTED_EDGE ( 'NONE', *, *, #11145, .T. ) ;
#49694 = CARTESIAN_POINT ( 'NONE',  ( 35.00000000000000000, -7.718225330433870823, -9.430788938294027091 ) ) ;
#49695 = FACE_OUTER_BOUND ( 'NONE', #61081, .T. ) ;
#49696 = EDGE_CURVE ( 'NONE', #63445, #37474, #47736, .T. ) ;
#49697 = ORIENTED_EDGE ( 'NONE', *, *, #26032, .F. ) ;
#49698 = ORIENTED_EDGE ( 'NONE', *, *, #4260, .F. ) ;
#49699 = ORIENTED_EDGE ( 'NONE', *, *, #41962, .T. ) ;
#49700 = DIRECTION ( 'NONE',  ( 1.000000000000000000, 0.000000000000000000, -0.000000000000000000 ) ) ;
#49701 = VERTEX_POINT ( 'NONE', #6314 ) ;
#49702 = CARTESIAN_POINT ( 'NONE',  ( 18.84867683979355846, 5.944105725974518251, 12.12095735156415088 ) ) ;
#49703 = DIRECTION ( 'NONE',  ( -0.000000000000000000, -0.000000000000000000, -1.000000000000000000 ) ) ;
#49704 = DIRECTION ( 'NONE',  ( 0.000000000000000000, 1.000000000000000000, 0.000000000000000000 ) ) ;
#49705 = CARTESIAN_POINT ( 'NONE',  ( 0.2650492433740053722, 4.084772052580754043, -11.54478237753287573 ) ) ;
#49706 = ADVANCED_FACE ( 'NONE', ( #62467 ), #40171, .F. ) ;
#49707 = CARTESIAN_POINT ( 'NONE',  ( -12.19463663866909187, -29.31670792731426545, 5.824636309908064469 ) ) ;
#49708 = CARTESIAN_POINT ( 'NONE',  ( -35.04660725145885891, 0.01191704700717466717, -0.003039313842370838965 ) ) ;
#49710 = ORIENTED_EDGE ( 'NONE', *, *, #21009, .F. ) ;
#49709 = CARTESIAN_POINT ( 'NONE',  ( 1.198791140417495571, 7.669598593075251713, 9.943044756147862984 ) ) ;
#49711 = CARTESIAN_POINT ( 'NONE',  ( -22.27721688985630522, 2.338410344701265409, 2.843753050855849285 ) ) ;
#49712 = EDGE_CURVE ( 'NONE', #18784, #40821, #55922, .T. ) ;
#49713 = ORIENTED_EDGE ( 'NONE', *, *, #30624, .F. ) ;
#49714 = CARTESIAN_POINT ( 'NONE',  ( 0.2653519890518161728, 10.60551359205158661, -6.123106317427046363 ) ) ;
#49715 = VERTEX_POINT ( 'NONE', #1331 ) ;
#49716 = ORIENTED_EDGE ( 'NONE', *, *, #64705, .F. ) ;
#49717 = CARTESIAN_POINT ( 'NONE',  ( -22.30861784526116054, -0.8834205920623459107, 3.671054459752214338 ) ) ;
#49718 = ADVANCED_FACE ( 'NONE', ( #26260 ), #29815, .T. ) ;
#49719 = CARTESIAN_POINT ( 'NONE',  ( -11.87635721006996192, -32.86858074101603222, 11.71246211286135619 ) ) ;
#49720 = DIRECTION ( 'NONE',  ( 0.3628680629012471792, -0.9318405276259971171, 0.000000000000000000 ) ) ;
#49721 = CARTESIAN_POINT ( 'NONE',  ( 24.31148382840972033, -1.623357687012453088, 11.89098708344122812 ) ) ;
#49722 = CARTESIAN_POINT ( 'NONE',  ( 1.937114397841932290, -12.45230409340479660, -3.111612666690204421 ) ) ;
#49723 = CARTESIAN_POINT ( 'NONE',  ( 6.812204945636112896, -4.138731716409435712, 25.00000000000000000 ) ) ;
#49725 = ORIENTED_EDGE ( 'NONE', *, *, #64237, .F. ) ;
#49724 = EDGE_CURVE ( 'NONE', #59781, #16732, #21260, .T. ) ;
#49726 = AXIS2_PLACEMENT_3D ( 'NONE', #47134, #16847, #37123 ) ;
#49727 =( BOUNDED_SURFACE ( )  B_SPLINE_SURFACE ( 3, 1, ( 
 ( #9730, #5094 ),
 ( #60279, #9087 ),
 ( #25358, #54668 ),
 ( #34985, #55951 ) ),
 .UNSPECIFIED., .F., .F., .F. ) 
 B_SPLINE_SURFACE_WITH_KNOTS ( ( 4, 4 ),
 ( 2, 2 ),
 ( 0.000000000000000000, 1.000000000000000000 ),
 ( 0.000000000000000000, 1.000000000000000000 ),
 .UNSPECIFIED. ) 
 GEOMETRIC_REPRESENTATION_ITEM ( )  RATIONAL_B_SPLINE_SURFACE ( (
 ( 1.000000000000000000, 1.000000000000000000),
 ( 0.9942764183789327692, 0.8450855930916580938),
 ( 0.9942764183789327692, 0.8450855930916580938),
 ( 1.000000000000000000, 1.000000000000000000) ) ) 
 REPRESENTATION_ITEM ( '' )  SURFACE ( )  );
#49728 = VERTEX_POINT ( 'NONE', #57182 ) ;
#49729 = CARTESIAN_POINT ( 'NONE',  ( -35.00000000000000000, 0.000000000000000000, 0.000000000000000000 ) ) ;
#49730 = EDGE_CURVE ( 'NONE', #30664, #26254, #11610, .T. ) ;
#49731 = CIRCLE ( 'NONE', #30581, 12.18649999999999878 ) ;
#49732 = EDGE_LOOP ( 'NONE', ( #23861, #4641 ) ) ;
#49733 = CYLINDRICAL_SURFACE ( 'NONE', #57214, 7.499999999999988454 ) ;
#49734 = AXIS2_PLACEMENT_3D ( 'NONE', #26668, #46963, #1421 ) ;
#49735 = CARTESIAN_POINT ( 'NONE',  ( 0.3160775863651064110, -10.49803827792118405, -6.338373607799300480 ) ) ;
#49736 = FACE_OUTER_BOUND ( 'NONE', #38579, .T. ) ;
#49737 = CARTESIAN_POINT ( 'NONE',  ( 2.262775599886257538, 7.640237753423675393, 0.1412024122916144542 ) ) ;
#49738 = CARTESIAN_POINT ( 'NONE',  ( -35.00000000000000000, -9.430788938294105250, 7.718225330433773124 ) ) ;
#49739 = CARTESIAN_POINT ( 'NONE',  ( 1.948354844646296158, 1.364409644999653226, -11.88693049004315583 ) ) ;
#49740 = ORIENTED_EDGE ( 'NONE', *, *, #33399, .T. ) ;
#49741 = ORIENTED_EDGE ( 'NONE', *, *, #6747, .T. ) ;
#49742 = CARTESIAN_POINT ( 'NONE',  ( 0.4626703367443965598, 3.943760108616825022, 11.66326339726735561 ) ) ;
#49743 = SURFACE_STYLE_FILL_AREA ( #23160 ) ;
#49744 = CARTESIAN_POINT ( 'NONE',  ( 6.812204945636112896, -4.138731716409435712, -12.84993773446340803 ) ) ;
#49745 = EDGE_CURVE ( 'NONE', #53403, #18319, #63806, .T. ) ;
#49746 = CARTESIAN_POINT ( 'NONE',  ( 3.347841273039249721, -10.61118957148187825, 25.00000000000000000 ) ) ;
#49747 = FACE_OUTER_BOUND ( 'NONE', #30896, .T. ) ;
#49748 = VECTOR ( 'NONE', #53248, 1000.000000000000000 ) ;
#49749 = CARTESIAN_POINT ( 'NONE',  ( 7.219696859909502606, -7.180886164847118280, -11.43374296297836779 ) ) ;
#49750 = CARTESIAN_POINT ( 'NONE',  ( 0.000000000000000000, 6.643843315911821534, -1.507714007300717585 ) ) ;
#49751 = CARTESIAN_POINT ( 'NONE',  ( 2.907497136250300596, 6.243048412628660060, 4.769582063554193674 ) ) ;
#49752 = CARTESIAN_POINT ( 'NONE',  ( 2.844750968616321263, -5.286885609674953024, -5.783165144077072384 ) ) ;
#49753 = VERTEX_POINT ( 'NONE', #11934 ) ;
#49754 = FACE_OUTER_BOUND ( 'NONE', #35574, .T. ) ;
#49755 = CYLINDRICAL_SURFACE ( 'NONE', #64019, 4.999999999999999112 ) ;
#49756 = EDGE_CURVE ( 'NONE', #63312, #8204, #58524, .T. ) ;
#49757 = CARTESIAN_POINT ( 'NONE',  ( 35.00000000000000000, -12.09831040184922912, 1.463443770872898453 ) ) ;
#49758 = AXIS2_PLACEMENT_3D ( 'NONE', #1244, #57419, #6230 ) ;
#49759 = CARTESIAN_POINT ( 'NONE',  ( -16.21117406328131949, -35.00000000000000000, -4.142385751841763053 ) ) ;
#49760 = CARTESIAN_POINT ( 'NONE',  ( 1.283627346226862809, -4.817767733507260175, -11.62704807385642169 ) ) ;
#49761 = AXIS2_PLACEMENT_3D ( 'NONE', #28988, #34920, #9661 ) ;
#49762 = AXIS2_PLACEMENT_3D ( 'NONE', #3531, #13461, #34071 ) ;
#49763 = ORIENTED_EDGE ( 'NONE', *, *, #14413, .F. ) ;
#49764 = CARTESIAN_POINT ( 'NONE',  ( -37.00000000000000711, 12.09831040184926287, -1.463443770872647542 ) ) ;
#49765 = CARTESIAN_POINT ( 'NONE',  ( 47.00000000000000711, 4.705694406421931860E-17, -3.469127814946512892E-15 ) ) ;
#49766 = CARTESIAN_POINT ( 'NONE',  ( -4.291397156012838110, -28.05769852054764968, -12.02237517917411047 ) ) ;
#49767 = VERTEX_POINT ( 'NONE', #27556 ) ;
#49768 = DIRECTION ( 'NONE',  ( 0.000000000000000000, -0.01356324068817998940, 0.9999080150203990547 ) ) ;
#49769 = CARTESIAN_POINT ( 'NONE',  ( -27.94693092740403273, -13.15284231573790130, -3.100845697411033441 ) ) ;
#49770 = CARTESIAN_POINT ( 'NONE',  ( 0.2646305136544072623, -12.24595685781654453, -0.1321451301299099712 ) ) ;
#49771 = EDGE_CURVE ( 'NONE', #3400, #58711, #58161, .T. ) ;
#49772 = CIRCLE ( 'NONE', #38081, 5.000000000000001776 ) ;
#49773 = CARTESIAN_POINT ( 'NONE',  ( 0.9296196016816532515, 12.46069139398388081, 0.4155906739593158705 ) ) ;
#49774 = B_SPLINE_CURVE_WITH_KNOTS ( 'NONE', 3,
 ( #4900, #61072, #61377, #15819, #35769, #31138, #25162, #20171, #56068, #21146 ),
 .UNSPECIFIED., .F., .F.,
 ( 4, 2, 2, 2, 4 ),
 ( 0.006778809408328222152, 0.007562956181792331208, 0.008347102955256440263, 0.009131249728720550185, 0.009915396502184661842 ),
 .UNSPECIFIED. ) ;
#49775 = CARTESIAN_POINT ( 'NONE',  ( -27.08430792439081003, 2.211452765398042697, 0.6005833784282403887 ) ) ;
#49776 = FACE_OUTER_BOUND ( 'NONE', #49018, .T. ) ;
#49777 = VERTEX_POINT ( 'NONE', #27898 ) ;
#49778 = CARTESIAN_POINT ( 'NONE',  ( 0.000000000000000000, 3.230174184210159893, -5.998318953995314118 ) ) ;
#49779 = CARTESIAN_POINT ( 'NONE',  ( -2.952869152607111136, -4.384817011589735358, 11.17020052527586138 ) ) ;
#49780 = CYLINDRICAL_SURFACE ( 'NONE', #35353, 12.75000000000000178 ) ;
#49781 = DIRECTION ( 'NONE',  ( -1.000000000000000000, 0.000000000000000000, 0.000000000000000000 ) ) ;
#49782 = LINE ( 'NONE', #4231, #65149 ) ;
#49783 = CARTESIAN_POINT ( 'NONE',  ( 37.00000000000000711, -11.59605747147790211, -5.300372733891605570 ) ) ;
#49784 = DIRECTION ( 'NONE',  ( -1.000000000000000000, 0.000000000000000000, -0.000000000000000000 ) ) ;
#49785 = DIRECTION ( 'NONE',  ( 0.000000000000000000, 1.000000000000000000, 0.000000000000000000 ) ) ;
#49786 = EDGE_LOOP ( 'NONE', ( #30473, #471, #47181, #37540 ) ) ;
#49787 = VERTEX_POINT ( 'NONE', #42851 ) ;
#49788 = CARTESIAN_POINT ( 'NONE',  ( 3.152665057736252940, 7.609997527622067715, 2.258875078500286016 ) ) ;
#49789 = ORIENTED_EDGE ( 'NONE', *, *, #57452, .T. ) ;
#49790 = PRESENTATION_STYLE_ASSIGNMENT (( #24184 ) ) ;
#49791 = ADVANCED_FACE ( 'NONE', ( #37869 ), #17604, .T. ) ;
#49792 = DIRECTION ( 'NONE',  ( -0.9582930651793755139, 0.2742293873734353293, -0.08045274594386130074 ) ) ;
#49793 = VECTOR ( 'NONE', #22607, 1000.000000000000000 ) ;
#49794 = ADVANCED_FACE ( 'NONE', ( #33542 ), #52152, .T. ) ;
#49795 = DIRECTION ( 'NONE',  ( -1.000000000000000000, 0.000000000000000000, 0.000000000000000000 ) ) ;
#49796 = ORIENTED_EDGE ( 'NONE', *, *, #13653, .T. ) ;
#49797 = CYLINDRICAL_SURFACE ( 'NONE', #3621, 4.999999999999999112 ) ;
#49798 = DIRECTION ( 'NONE',  ( -1.000000000000000000, 0.000000000000000000, 0.000000000000000000 ) ) ;
#49799 = VECTOR ( 'NONE', #6811, 1000.000000000000000 ) ;
#49800 = CARTESIAN_POINT ( 'NONE',  ( 0.000000000000000000, 0.000000000000000000, 0.000000000000000000 ) ) ;
#49801 = ORIENTED_EDGE ( 'NONE', *, *, #49826, .T. ) ;
#49802 = EDGE_LOOP ( 'NONE', ( #4147, #58152, #13022, #52294 ) ) ;
#49803 = EDGE_CURVE ( 'NONE', #5331, #24263, #14957, .T. ) ;
#49804 = CARTESIAN_POINT ( 'NONE',  ( 2.963017218115625351, 0.3847317984106394251, -7.865565884553431530 ) ) ;
#49805 = CARTESIAN_POINT ( 'NONE',  ( 35.00000000000000000, 4.705694406421931860E-17, -3.469127814946512892E-15 ) ) ;
#49806 = ORIENTED_EDGE ( 'NONE', *, *, #28150, .F. ) ;
#49807 = CARTESIAN_POINT ( 'NONE',  ( 2.941278708680199916, 5.814102272488588241, 1.972702289976022483 ) ) ;
#49808 = ORIENTED_EDGE ( 'NONE', *, *, #36983, .T. ) ;
#49809 = DIRECTION ( 'NONE',  ( -1.000000000000000000, 0.000000000000000000, 0.000000000000000000 ) ) ;
#49811 = VECTOR ( 'NONE', #51477, 1000.000000000000114 ) ;
#49810 = CARTESIAN_POINT ( 'NONE',  ( 2.000000000000001776, 1.754183803416544452, 6.711026108862249373 ) ) ;
#49812 = CARTESIAN_POINT ( 'NONE',  ( 0.000000000000000000, 0.000000000000000000, 0.000000000000000000 ) ) ;
#49813 = DIRECTION ( 'NONE',  ( 0.000000000000000000, 0.5472293298355273006, -0.8369827122275342868 ) ) ;
#49814 = FACE_OUTER_BOUND ( 'NONE', #5467, .T. ) ;
#49815 = VECTOR ( 'NONE', #61943, 1000.000000000000000 ) ;
#49816 = ORIENTED_EDGE ( 'NONE', *, *, #12212, .T. ) ;
#49817 = CARTESIAN_POINT ( 'NONE',  ( 2.298277635560276533, -1.491234112749247220, 7.506689984432345142 ) ) ;
#49818 = CARTESIAN_POINT ( 'NONE',  ( 2.827825597296804272, 2.100863646776170768, -8.776379025186153982 ) ) ;
#49819 = DIRECTION ( 'NONE',  ( 0.000000000000000000, -0.8827602140260265573, 0.4698238015817460256 ) ) ;
#49820 = DIRECTION ( 'NONE',  ( 0.000000000000000000, -0.4380125133593848474, 0.8989688749565218906 ) ) ;
#49821 = CARTESIAN_POINT ( 'NONE',  ( 12.64843508166302399, 11.70598649689469717, -6.727170912064254438 ) ) ;
#49822 = LINE ( 'NONE', #28552, #6365 ) ;
#49823 = CARTESIAN_POINT ( 'NONE',  ( 35.00000000000000000, 10.54834585426228877, 6.102719229070555862 ) ) ;
#49824 = CARTESIAN_POINT ( 'NONE',  ( -35.00000000000000000, 0.000000000000000000, 0.000000000000000000 ) ) ;
#49825 = CARTESIAN_POINT ( 'NONE',  ( 0.3675815128205912052, 9.235491948680007113, 8.093875121226108860 ) ) ;
#49826 = EDGE_CURVE ( 'NONE', #38510, #38095, #30307, .T. ) ;
#49827 = ORIENTED_EDGE ( 'NONE', *, *, #56234, .F. ) ;
#49828 = CARTESIAN_POINT ( 'NONE',  ( 0.3474126878361805670, 0.2587235634078023927, 12.27082419038177541 ) ) ;
#49829 = EDGE_CURVE ( 'NONE', #64891, #16581, #58493, .T. ) ;
#49830 = EDGE_LOOP ( 'NONE', ( #57239, #6433, #10605, #4989 ) ) ;
#49831 = DIRECTION ( 'NONE',  ( 0.000000000000000000, 0.01356324068817998940, -0.9999080150203990547 ) ) ;
#49832 = CARTESIAN_POINT ( 'NONE',  ( 2.268878695253351285, -7.500319319173561539, -1.472930498387347242 ) ) ;
#49833 = DIRECTION ( 'NONE',  ( 1.000000000000000000, -0.000000000000000000, -0.000000000000000000 ) ) ;
#49834 = DIRECTION ( 'NONE',  ( 0.000000000000000000, 0.000000000000000000, 1.000000000000000000 ) ) ;
#49835 = CARTESIAN_POINT ( 'NONE',  ( 2.653899356900503825, 5.192946150929651061, 5.782420802795840586 ) ) ;
#49836 = ORIENTED_EDGE ( 'NONE', *, *, #56369, .T. ) ;
#49837 = CARTESIAN_POINT ( 'NONE',  ( -27.01437459610461644, 8.723448335974111956, -8.240233560378637634 ) ) ;
#49838 = LINE ( 'NONE', #4288, #44844 ) ;
#49839 = ADVANCED_FACE ( 'NONE', ( #57851 ), #7959, .T. ) ;
#49840 = CARTESIAN_POINT ( 'NONE',  ( -27.09602251845159060, 2.092130925171141520, 1.018053071731282344 ) ) ;
#49841 = CARTESIAN_POINT ( 'NONE',  ( 35.00000000000000000, 12.49688848680883879, -2.527899948230684313 ) ) ;
#49842 = AXIS2_PLACEMENT_3D ( 'NONE', #55889, #61512, #25623 ) ;
#49843 = CYLINDRICAL_SURFACE ( 'NONE', #2138, 2.899999999999994582 ) ;
#49844 = ORIENTED_EDGE ( 'NONE', *, *, #45821, .F. ) ;
#49845 = CIRCLE ( 'NONE', #11626, 4.999999999999999112 ) ;
#49846 = CARTESIAN_POINT ( 'NONE',  ( 37.00000000000000711, 4.705694406421931860E-17, -3.469127814946512892E-15 ) ) ;
#49847 = ORIENTED_EDGE ( 'NONE', *, *, #55303, .F. ) ;
#49848 = CARTESIAN_POINT ( 'NONE',  ( 0.2653141617321011503, 12.24612535104216526, 0.04404194803635243238 ) ) ;
#49850 = EDGE_CURVE ( 'NONE', #60788, #32449, #57413, .T. ) ;
#49849 = DIRECTION ( 'NONE',  ( 0.000000000000000000, 0.01356324068817998940, -0.9999080150203989437 ) ) ;
#49851 = ADVANCED_FACE ( 'NONE', ( #7270 ), #22587, .T. ) ;
#49852 = CARTESIAN_POINT ( 'NONE',  ( -2.532614230583026593, -7.965877694534051479, 10.89930238848911337 ) ) ;
#49853 = EDGE_CURVE ( 'NONE', #40181, #51873, #64886, .T. ) ;
#49854 = CARTESIAN_POINT ( 'NONE',  ( 0.000000000000000000, -5.450255447309769963, 4.087611905901399112 ) ) ;
#49855 = AXIS2_PLACEMENT_3D ( 'NONE', #53792, #52492, #13217 ) ;
#49856 = ORIENTED_EDGE ( 'NONE', *, *, #59253, .T. ) ;
#49857 = ORIENTED_EDGE ( 'NONE', *, *, #59741, .F. ) ;
#49858 = CARTESIAN_POINT ( 'NONE',  ( 0.000000000000000000, 0.000000000000000000, 0.000000000000000000 ) ) ;
#49859 = ORIENTED_EDGE ( 'NONE', *, *, #9535, .T. ) ;
#49860 = CIRCLE ( 'NONE', #51962, 12.75000000000000178 ) ;
#49861 = CARTESIAN_POINT ( 'NONE',  ( 35.00000000000000000, -4.603882218679472338, 10.80631716521671493 ) ) ;
#49862 = LINE ( 'NONE', #45195, #18357 ) ;
#49863 = CARTESIAN_POINT ( 'NONE',  ( 0.000000000000000000, 6.250523986464036064, -3.007653927006531447 ) ) ;
#49864 = CARTESIAN_POINT ( 'NONE',  ( 0.2657645697724693723, 12.24540328300722081, 0.1513403555225990293 ) ) ;
#49865 = CARTESIAN_POINT ( 'NONE',  ( 2.589278595513858860, 6.588350318048553866, -4.081908913132052064 ) ) ;
#49866 = CARTESIAN_POINT ( 'NONE',  ( -28.67667724226168602, -1.888227992976682756, 0.1214114860980369109 ) ) ;
#49867 = DIRECTION ( 'NONE',  ( -1.000000000000000000, 0.000000000000000000, 0.000000000000000000 ) ) ;
#49868 = VERTEX_POINT ( 'NONE', #3293 ) ;
#49869 = ORIENTED_EDGE ( 'NONE', *, *, #48425, .T. ) ;
#49870 = VECTOR ( 'NONE', #32515, 1000.000000000000000 ) ;
#49871 = ORIENTED_EDGE ( 'NONE', *, *, #18530, .F. ) ;
#49872 = B_SPLINE_CURVE_WITH_KNOTS ( 'NONE', 3,
 ( #56640, #6099, #17034, #15706, #41973, #36665, #57284, #21718, #56964, #10732, #29770, #37312, #41647, #11387, #768, #11706 ),
 .UNSPECIFIED., .F., .F.,
 ( 4, 2, 2, 2, 2, 2, 2, 4 ),
 ( 3.878959614448864246E-18, 0.002501164792002928683, 0.003751747188004390856, 0.005002329584005853029, 0.006252911980007317370, 0.007503494376008781712, 0.008754076772010246921, 0.01000465916801171126 ),
 .UNSPECIFIED. ) ;
#49873 = CARTESIAN_POINT ( 'NONE',  ( 1.372161826076855995, -2.769012792636821541, -12.30755118281459914 ) ) ;
#49874 = EDGE_CURVE ( 'NONE', #15604, #45790, #19257, .T. ) ;
#49875 = DIRECTION ( 'NONE',  ( 1.000000000000000000, 0.000000000000000000, 0.000000000000000000 ) ) ;
#49876 = ORIENTED_EDGE ( 'NONE', *, *, #5488, .F. ) ;
#49877 = EDGE_CURVE ( 'NONE', #2479, #12997, #8616, .T. ) ;
#49878 = FACE_BOUND ( 'NONE', #19024, .T. ) ;
#49879 = EDGE_LOOP ( 'NONE', ( #11687, #64827, #318, #32607 ) ) ;
#49880 = CARTESIAN_POINT ( 'NONE',  ( -36.00000000000000711, 7.745827850123011338, 10.12742074351899468 ) ) ;
#49881 = B_SPLINE_CURVE_WITH_KNOTS ( 'NONE', 3,
 ( #20136, #10158, #10812, #5861, #31099, #36415, #51412, #35422 ),
 .UNSPECIFIED., .F., .F.,
 ( 4, 2, 2, 4 ),
 ( 0.000000000000000000, 0.0003639104015150018603, 0.0007278208030300037205, 0.001455641606060010260 ),
 .UNSPECIFIED. ) ;
#49882 = CARTESIAN_POINT ( 'NONE',  ( 5.514624014163232779, 0.0001700579043838694037, 0.004137701579365772944 ) ) ;
#49883 = CARTESIAN_POINT ( 'NONE',  ( -27.09030469827879983, -2.239626370111428955, -0.5638997280370279253 ) ) ;
#49884 = ORIENTED_EDGE ( 'NONE', *, *, #40260, .T. ) ;
#49885 = ORIENTED_EDGE ( 'NONE', *, *, #55336, .F. ) ;
#49886 = CARTESIAN_POINT ( 'NONE',  ( 2.305787727787083519, -6.711944854845849129, 3.682701754025489826 ) ) ;
#49887 = ORIENTED_EDGE ( 'NONE', *, *, #49473, .T. ) ;
#49888 = PLANE ( 'NONE',  #54976 ) ;
#49889 = ORIENTED_EDGE ( 'NONE', *, *, #42882, .F. ) ;
#49890 = VERTEX_POINT ( 'NONE', #19563 ) ;
#49891 = ORIENTED_EDGE ( 'NONE', *, *, #65582, .T. ) ;
#49892 = LINE ( 'NONE', #33615, #19204 ) ;
#49893 = CARTESIAN_POINT ( 'NONE',  ( -13.30196514322741841, -33.37310655729432085, -10.51054543287389542 ) ) ;
#49894 = CIRCLE ( 'NONE', #50934, 22.50555349946515449 ) ;
#49895 = CIRCLE ( 'NONE', #2139, 12.75000000000000178 ) ;
#49896 = DIRECTION ( 'NONE',  ( -1.000000000000000000, 0.000000000000000000, 0.000000000000000000 ) ) ;
#49897 = CARTESIAN_POINT ( 'NONE',  ( 37.00000000000000711, 3.340853584269691368, 11.26103545359851665 ) ) ;
#49898 = ORIENTED_EDGE ( 'NONE', *, *, #53163, .F. ) ;
#49899 = CARTESIAN_POINT ( 'NONE',  ( 2.000000000000001776, -5.107597897712365054, 4.693343793638375061 ) ) ;
#49900 = ORIENTED_EDGE ( 'NONE', *, *, #29459, .F. ) ;
#49901 = AXIS2_PLACEMENT_3D ( 'NONE', #56100, #24213, #19233 ) ;
#49902 = FACE_OUTER_BOUND ( 'NONE', #11826, .T. ) ;
#49903 = DIRECTION ( 'NONE',  ( 1.000000000000000000, 0.000000000000000000, 0.000000000000000000 ) ) ;
#49904 = ORIENTED_EDGE ( 'NONE', *, *, #20332, .T. ) ;
#49905 = CARTESIAN_POINT ( 'NONE',  ( 1.020182472824526121, 9.854645283131009847, -7.686484208904769133 ) ) ;
#49906 = DIRECTION ( 'NONE',  ( 0.000000000000000000, 0.000000000000000000, 1.000000000000000000 ) ) ;
#49907 = DIRECTION ( 'NONE',  ( 0.000000000000000000, 0.000000000000000000, 1.000000000000000000 ) ) ;
#49908 = CIRCLE ( 'NONE', #21215, 2.899999999999995470 ) ;
#49909 = ORIENTED_EDGE ( 'NONE', *, *, #64449, .F. ) ;
#49910 = VERTEX_POINT ( 'NONE', #40470 ) ;
#49911 = CARTESIAN_POINT ( 'NONE',  ( 1.194176325881331380, 6.717888447700822496, 10.60746084433557535 ) ) ;
#49912 = VECTOR ( 'NONE', #45345, 1000.000000000000000 ) ;
#49913 = EDGE_CURVE ( 'NONE', #59829, #37286, #9687, .T. ) ;
#49914 =( BOUNDED_CURVE ( )  B_SPLINE_CURVE ( 3, ( #18975, #39571, #59874, #29582 ),
 .UNSPECIFIED., .F., .F. ) 
 B_SPLINE_CURVE_WITH_KNOTS ( ( 4, 4 ),
 ( 5.331207651931955560, 5.369882018696277015 ),
 .UNSPECIFIED. ) 
 CURVE ( )  GEOMETRIC_REPRESENTATION_ITEM ( )  RATIONAL_B_SPLINE_CURVE ( ( 1.000000000000000000, 0.9998753616634872277, 0.9998753616634872277, 1.000000000000000000 ) ) 
 REPRESENTATION_ITEM ( '' )  );
#49915 = ORIENTED_EDGE ( 'NONE', *, *, #25509, .F. ) ;
#49916 = CARTESIAN_POINT ( 'NONE',  ( 0.000000000000000000, -3.795144977083660720, 6.468916029978762694 ) ) ;
#49917 = DIRECTION ( 'NONE',  ( -1.000000000000000000, -0.000000000000000000, -0.000000000000000000 ) ) ;
#49918 = CARTESIAN_POINT ( 'NONE',  ( -15.75855542457932046, -29.13485235466247403, 10.82860303369087873 ) ) ;
#49919 = CARTESIAN_POINT ( 'NONE',  ( -3.358052903796875377, 10.43609928815077126, 5.926952491707684345 ) ) ;
#49920 = DIRECTION ( 'NONE',  ( 1.000000000000000000, 0.000000000000000000, 0.000000000000000000 ) ) ;
#49921 = ORIENTED_EDGE ( 'NONE', *, *, #26381, .F. ) ;
#49922 = AXIS2_PLACEMENT_3D ( 'NONE', #2296, #38167, #23220 ) ;
#49923 = DIRECTION ( 'NONE',  ( 0.000000000000000000, -0.2355298848897378339, -0.9718671068226493182 ) ) ;
#49924 = DIRECTION ( 'NONE',  ( -1.000000000000000000, -0.000000000000000000, -0.000000000000000000 ) ) ;
#49925 = EDGE_CURVE ( 'NONE', #28265, #7169, #37320, .T. ) ;
#49926 = CARTESIAN_POINT ( 'NONE',  ( 0.2958664285830446272, -12.10650684287252687, -1.910785783655700509 ) ) ;
#49927 = DIRECTION ( 'NONE',  ( 1.000000000000000000, 0.000000000000000000, 0.000000000000000000 ) ) ;
#49929 = EDGE_CURVE ( 'NONE', #56844, #58552, #36228, .T. ) ;
#49928 = CARTESIAN_POINT ( 'NONE',  ( 5.530133899448235191, -0.004396748047611123179, -0.01536822665454899879 ) ) ;
#49930 = CARTESIAN_POINT ( 'NONE',  ( -36.00000000000000711, -8.830544224262881770, -9.196955404009390378 ) ) ;
#49931 = DIRECTION ( 'NONE',  ( 0.000000000000000000, -0.01356324068817991828, 0.9999080150203990547 ) ) ;
#49932 = AXIS2_PLACEMENT_3D ( 'NONE', #47627, #48957, #37966 ) ;
#49933 = CIRCLE ( 'NONE', #21259, 5.000000000000000000 ) ;
#49934 = EDGE_LOOP ( 'NONE', ( #61896, #29918, #55365, #52518 ) ) ;
#49935 = CARTESIAN_POINT ( 'NONE',  ( 35.00000000000000000, 4.705694406421931860E-17, -3.469127814946512892E-15 ) ) ;
#49936 = ORIENTED_EDGE ( 'NONE', *, *, #34613, .F. ) ;
#49937 = CARTESIAN_POINT ( 'NONE',  ( 5.515188684475870851, -0.002983184900675359651, -0.004442604682416606034 ) ) ;
#49938 = PLANE ( 'NONE',  #9901 ) ;
#49939 = CARTESIAN_POINT ( 'NONE',  ( -37.00000000000000711, 0.000000000000000000, 0.000000000000000000 ) ) ;
#49940 = CARTESIAN_POINT ( 'NONE',  ( -36.00000000000000711, 12.71517666308949579, -0.9416912585473031783 ) ) ;
#49941 = ORIENTED_EDGE ( 'NONE', *, *, #52766, .F. ) ;
#49942 = EDGE_LOOP ( 'NONE', ( #25169, #37730, #57201, #18944 ) ) ;
#49943 = ORIENTED_EDGE ( 'NONE', *, *, #63381, .F. ) ;
#49944 = CARTESIAN_POINT ( 'NONE',  ( 3.152665057734129750, 3.161213418913565221, -7.281573230474259972 ) ) ;
#49945 = AXIS2_PLACEMENT_3D ( 'NONE', #58134, #3267, #53804 ) ;
#49946 = EDGE_CURVE ( 'NONE', #24268, #7657, #46996, .T. ) ;
#49947 = CARTESIAN_POINT ( 'NONE',  ( -35.00000000000000000, 11.26103545359856106, -3.340853584269573684 ) ) ;
#49948 = EDGE_LOOP ( 'NONE', ( #61297, #43720, #64738, #39478 ) ) ;
#49949 = DIRECTION ( 'NONE',  ( 0.000000000000000000, 0.000000000000000000, 1.000000000000000000 ) ) ;
#49950 = CARTESIAN_POINT ( 'NONE',  ( -36.00000000000000711, 12.38385022362082033, 3.033604067594622755 ) ) ;
#49951 = CIRCLE ( 'NONE', #58456, 4.999999999999998224 ) ;
#49952 = DIRECTION ( 'NONE',  ( -1.000000000000000000, -0.000000000000000000, 0.000000000000000000 ) ) ;
#49953 = CARTESIAN_POINT ( 'NONE',  ( 2.907497136250675407, -2.346692756478266251, 7.497839665536838893 ) ) ;
#49954 = ORIENTED_EDGE ( 'NONE', *, *, #52505, .F. ) ;
#49955 = PLANE ( 'NONE',  #55377 ) ;
#49956 = CARTESIAN_POINT ( 'NONE',  ( 4.532733354134117931, -28.39821948934984874, -13.34103783736786042 ) ) ;
#49957 = DIRECTION ( 'NONE',  ( -1.000000000000000000, 0.000000000000000000, 0.000000000000000000 ) ) ;
#49959 = ORIENTED_EDGE ( 'NONE', *, *, #2492, .F. ) ;
#49958 = CARTESIAN_POINT ( 'NONE',  ( 37.00000000000000711, 4.705694406421931860E-17, -3.469127814946512892E-15 ) ) ;
#49960 = CARTESIAN_POINT ( 'NONE',  ( -36.00000000000000711, 8.954052073409602741, 9.076753354954030684 ) ) ;
#49961 = VERTEX_POINT ( 'NONE', #24204 ) ;
#49962 = CARTESIAN_POINT ( 'NONE',  ( 0.7446945582519360896, -9.728576129010020779, 7.698291984229315155 ) ) ;
#49963 = CIRCLE ( 'NONE', #21286, 12.74999999999999822 ) ;
#49964 = EDGE_LOOP ( 'NONE', ( #56707, #4173, #60648, #64941 ) ) ;
#49965 = DIRECTION ( 'NONE',  ( 0.000000000000000000, 0.000000000000000000, 1.000000000000000000 ) ) ;
#49966 = CARTESIAN_POINT ( 'NONE',  ( -22.51237073810381517, 3.933875531624977828, 2.023441661740695618 ) ) ;
#49967 = CYLINDRICAL_SURFACE ( 'NONE', #37231, 5.000000000000000888 ) ;
#49968 = CARTESIAN_POINT ( 'NONE',  ( 1.104777566491150997, -6.672212870706140109, -10.60111489796741857 ) ) ;
#49969 = EDGE_CURVE ( 'NONE', #14515, #6027, #54292, .T. ) ;
#49970 = CARTESIAN_POINT ( 'NONE',  ( 35.00000000000000000, 4.705694406421931860E-17, -3.469127814946512892E-15 ) ) ;
#49971 = CARTESIAN_POINT ( 'NONE',  ( -10.74958689447668014, -6.108794307151256042, -12.04558683403140940 ) ) ;
#49972 = DIRECTION ( 'NONE',  ( 1.000000000000000000, 0.000000000000000000, -0.000000000000000000 ) ) ;
#49974 = ORIENTED_EDGE ( 'NONE', *, *, #64560, .F. ) ;
#49973 = DIRECTION ( 'NONE',  ( -1.000000000000000000, 0.000000000000000000, 0.000000000000000000 ) ) ;
#49975 = AXIS2_PLACEMENT_3D ( 'NONE', #56776, #46767, #1228 ) ;
#49976 = VERTEX_POINT ( 'NONE', #19220 ) ;
#49977 = CARTESIAN_POINT ( 'NONE',  ( 13.35499959353619914, -12.72359730182141568, -4.517647836983113230 ) ) ;
#49978 = ORIENTED_EDGE ( 'NONE', *, *, #28629, .T. ) ;
#49979 = AXIS2_PLACEMENT_3D ( 'NONE', #49150, #39133, #59123 ) ;
#49980 = VERTEX_POINT ( 'NONE', #50480 ) ;
#49981 = CARTESIAN_POINT ( 'NONE',  ( 0.2671309869109481094, 7.995521393275818234, 9.276621593297539548 ) ) ;
#49982 = CARTESIAN_POINT ( 'NONE',  ( -27.08417568107324058, 0.3682236895270734611, 2.261355310631410820 ) ) ;
#49983 = DIRECTION ( 'NONE',  ( 0.000000000000000000, 0.000000000000000000, -1.000000000000000000 ) ) ;
#49984 = CARTESIAN_POINT ( 'NONE',  ( -35.00000000000000000, -9.060822531526103063, 7.474872387600973944 ) ) ;
#49985 = DIRECTION ( 'NONE',  ( 0.000000000000000000, -0.9987865678893281807, 0.04924826701373505311 ) ) ;
#49986 = CARTESIAN_POINT ( 'NONE',  ( -37.00000000000000711, -0.4871980014162358152, 12.74068829017553739 ) ) ;
#49987 = VECTOR ( 'NONE', #4294, 1000.000000000000000 ) ;
#49988 = AXIS2_PLACEMENT_3D ( 'NONE', #34528, #64769, #43862 ) ;
#49989 = AXIS2_PLACEMENT_3D ( 'NONE', #3837, #10106, #25394 ) ;
#49990 = FACE_OUTER_BOUND ( 'NONE', #24506, .T. ) ;
#49991 = ADVANCED_FACE ( 'NONE', ( #4261 ), #60688, .F. ) ;
#49992 = EDGE_CURVE ( 'NONE', #1800, #12565, #54486, .T. ) ;
#49993 = VERTEX_POINT ( 'NONE', #29207 ) ;
#49994 = DIRECTION ( 'NONE',  ( -1.000000000000000000, -0.000000000000000000, 0.000000000000000000 ) ) ;
#49995 = CARTESIAN_POINT ( 'NONE',  ( 0.000000000000000000, 1.225832621831856484, 6.827324998361554265 ) ) ;
#49996 = ADVANCED_FACE ( 'NONE', ( #60111 ), #44165, .T. ) ;
#49997 = CARTESIAN_POINT ( 'NONE',  ( -35.00000000000000000, 7.717887834988368390, -8.854740511458771834 ) ) ;
#49998 = EDGE_LOOP ( 'NONE', ( #4995, #35729, #15522, #33715 ) ) ;
#49999 = AXIS2_PLACEMENT_3D ( 'NONE', #8408, #64902, #24041 ) ;
#50000 = VECTOR ( 'NONE', #23094, 1000.000000000000000 ) ;
#50001 = EDGE_CURVE ( 'NONE', #44289, #26844, #54854, .T. ) ;
#50002 = AXIS2_PLACEMENT_3D ( 'NONE', #56827, #36521, #37829 ) ;
#50003 = CARTESIAN_POINT ( 'NONE',  ( -7.154245469367370269, -1.341795249608957130, 13.43334531127548281 ) ) ;
#50004 = VECTOR ( 'NONE', #54160, 1000.000000000000000 ) ;
#50005 = CYLINDRICAL_SURFACE ( 'NONE', #60718, 4.999999999999999112 ) ;
#50006 = CARTESIAN_POINT ( 'NONE',  ( -47.77550903397568760, -0.4437794964969083433, -10.34167951973068611 ) ) ;
#50007 = EDGE_LOOP ( 'NONE', ( #19195, #521, #65466, #14937 ) ) ;
#50008 = CARTESIAN_POINT ( 'NONE',  ( 2.284126774967662588, 6.701756155761997569, -3.686252397487058019 ) ) ;
#50009 = CARTESIAN_POINT ( 'NONE',  ( 3.202861212859688056, -30.72210164159773882, 15.08749394223661788 ) ) ;
#50010 = CARTESIAN_POINT ( 'NONE',  ( 3.899688111913728772, 7.685012310942984648, 9.227363078734208912 ) ) ;
#50011 = AXIS2_PLACEMENT_3D ( 'NONE', #21610, #46535, #992 ) ;
#50012 = EDGE_CURVE ( 'NONE', #24413, #12853, #9888, .T. ) ;
#50013 = DIRECTION ( 'NONE',  ( -0.000000000000000000, -1.000000000000000000, -0.000000000000000000 ) ) ;
#50014 = CARTESIAN_POINT ( 'NONE',  ( 36.00000000000000711, -8.017674001891711200, 9.913596905230193101 ) ) ;
#50015 = AXIS2_PLACEMENT_3D ( 'NONE', #9072, #49648, #65257 ) ;
#50016 = ORIENTED_EDGE ( 'NONE', *, *, #22350, .T. ) ;
#50017 = DIRECTION ( 'NONE',  ( -1.000000000000000000, 0.000000000000000000, -0.000000000000000000 ) ) ;
#50018 = CARTESIAN_POINT ( 'NONE',  ( -9.257124744190798893, -8.325323762313093567, -8.651777918013287660 ) ) ;
#50019 = CARTESIAN_POINT ( 'NONE',  ( -22.30398854582848145, 3.608860109585136922, -1.062335901716034758 ) ) ;
#50020 = VERTEX_POINT ( 'NONE', #65725 ) ;
#50021 = DIRECTION ( 'NONE',  ( 1.000000000000000000, 0.000000000000000000, 0.000000000000000000 ) ) ;
#50022 = AXIS2_PLACEMENT_3D ( 'NONE', #19443, #10107, #14102 ) ;
#50023 = CARTESIAN_POINT ( 'NONE',  ( 36.00000000000000711, -12.31350058095520339, 3.307597835713371737 ) ) ;
#50024 = ORIENTED_EDGE ( 'NONE', *, *, #31666, .F. ) ;
#50025 = ORIENTED_EDGE ( 'NONE', *, *, #3424, .F. ) ;
#50026 = VERTEX_POINT ( 'NONE', #20196 ) ;
#50027 = VECTOR ( 'NONE', #25803, 1000.000000000000000 ) ;
#50028 = VECTOR ( 'NONE', #28165, 1000.000000000000000 ) ;
#50029 = AXIS2_PLACEMENT_3D ( 'NONE', #48484, #8887, #64716 ) ;
#50030 = ORIENTED_EDGE ( 'NONE', *, *, #57949, .T. ) ;
#50031 = DIRECTION ( 'NONE',  ( -1.000000000000000000, -0.000000000000000000, 0.000000000000000000 ) ) ;
#50032 = CARTESIAN_POINT ( 'NONE',  ( 2.000000000000001776, 6.662861565602083758, -1.421313227905602883 ) ) ;
#50033 = CARTESIAN_POINT ( 'NONE',  ( 37.00000000000000711, 4.705694406421931860E-17, -3.469127814946512892E-15 ) ) ;
#50034 = AXIS2_PLACEMENT_3D ( 'NONE', #19070, #2483, #64593 ) ;
#50035 = CARTESIAN_POINT ( 'NONE',  ( -18.19295774167957447, -28.79006254106626272, 7.843687167517533254 ) ) ;
#50036 = CARTESIAN_POINT ( 'NONE',  ( 35.00000000000000000, 4.705694406421931860E-17, -3.469127814946512892E-15 ) ) ;
#50038 = VERTEX_POINT ( 'NONE', #60770 ) ;
#50037 = DIRECTION ( 'NONE',  ( 0.2180658516479614395, -0.9759340573753174652, 0.000000000000000000 ) ) ;
#50039 = DIRECTION ( 'NONE',  ( -1.000000000000000000, 0.000000000000000000, -0.000000000000000000 ) ) ;
#50040 = ORIENTED_EDGE ( 'NONE', *, *, #61940, .T. ) ;
#50041 = CARTESIAN_POINT ( 'NONE',  ( 0.000000000000000000, -5.860254403322033845, 3.474373880649773039 ) ) ;
#50042 = VERTEX_POINT ( 'NONE', #35488 ) ;
#50043 = ORIENTED_EDGE ( 'NONE', *, *, #2408, .F. ) ;
#50044 = LINE ( 'NONE', #14443, #36866 ) ;
#50045 = CIRCLE ( 'NONE', #4390, 3.000000000000000444 ) ;
#50046 = CARTESIAN_POINT ( 'NONE',  ( 13.85759530760384628, -30.12605952702068279, 5.992721990255546416 ) ) ;
#50047 = DIRECTION ( 'NONE',  ( 0.000000000000000000, -0.9970832820307030664, -0.07632122047557565736 ) ) ;
#50048 = EDGE_CURVE ( 'NONE', #34961, #56217, #44720, .T. ) ;
#50049 = AXIS2_PLACEMENT_3D ( 'NONE', #25302, #30, #54909 ) ;
#50050 = CARTESIAN_POINT ( 'NONE',  ( 2.835339799623983303, 7.763739326985127143, -1.035140033449970520 ) ) ;
#50051 = CARTESIAN_POINT ( 'NONE',  ( 35.00000000000000000, 4.705694406421931860E-17, -3.469127814946512892E-15 ) ) ;
#50052 = CARTESIAN_POINT ( 'NONE',  ( 35.00000000000000000, -11.90598845858536770, -4.561791185930372805 ) ) ;
#50054 = ORIENTED_EDGE ( 'NONE', *, *, #44712, .T. ) ;
#50053 = CIRCLE ( 'NONE', #13902, 4.999999999999999112 ) ;
#50055 = AXIS2_PLACEMENT_3D ( 'NONE', #24048, #33366, #7772 ) ;
#50056 = ORIENTED_EDGE ( 'NONE', *, *, #9814, .F. ) ;
#50057 = CARTESIAN_POINT ( 'NONE',  ( 1.000000000000000888, 6.997684042076903310, 2.698595569414223849 ) ) ;
#50058 = ORIENTED_EDGE ( 'NONE', *, *, #40785, .T. ) ;
#50059 = AXIS2_PLACEMENT_3D ( 'NONE', #58979, #2796, #39307 ) ;
#50060 = VERTEX_POINT ( 'NONE', #5241 ) ;
#50061 = AXIS2_PLACEMENT_3D ( 'NONE', #48115, #6887, #38779 ) ;
#50062 = CARTESIAN_POINT ( 'NONE',  ( 35.00000000000000000, 11.37311665002363270, 2.936739658819908616 ) ) ;
#50063 = CARTESIAN_POINT ( 'NONE',  ( 2.241352910868908310, 1.407733736974867034, 7.503490710578237355 ) ) ;
#50064 = CARTESIAN_POINT ( 'NONE',  ( 16.92262867437927198, -9.930101274560646729, 6.758629725180155035 ) ) ;
#50065 = CARTESIAN_POINT ( 'NONE',  ( -22.27713295444592845, 1.050517974989026104, -3.528329525272667411 ) ) ;
#50066 = CARTESIAN_POINT ( 'NONE',  ( -11.40165637463000436, -7.508992741355388745, -9.360289953322599388 ) ) ;
#50067 = EDGE_CURVE ( 'NONE', #30237, #18262, #31996, .T. ) ;
#50068 = CARTESIAN_POINT ( 'NONE',  ( 2.655192694323565750, 1.093661162900110284, -9.539062147543583947 ) ) ;
#50069 = ORIENTED_EDGE ( 'NONE', *, *, #32600, .T. ) ;
#50070 = ADVANCED_FACE ( 'NONE', ( #16842 ), #62700, .F. ) ;
#50071 = EDGE_LOOP ( 'NONE', ( #45205, #8124, #9427, #37963 ) ) ;
#50072 = AXIS2_PLACEMENT_3D ( 'NONE', #12721, #2795, #38325 ) ;
#50073 = AXIS2_PLACEMENT_3D ( 'NONE', #14580, #54851, #29555 ) ;
#50074 = ADVANCED_FACE ( 'NONE', ( #16196 ), #5924, .T. ) ;
#50075 = LINE ( 'NONE', #30745, #10496 ) ;
#50076 = CARTESIAN_POINT ( 'NONE',  ( 2.000000000000001776, 6.606214214351110670, -2.114938770769863030 ) ) ;
#50077 = CARTESIAN_POINT ( 'NONE',  ( 37.00000000000000711, 8.352657516904789858, 8.258652103341336925 ) ) ;
#50078 = CIRCLE ( 'NONE', #9716, 12.75000000000000178 ) ;
#50079 = AXIS2_PLACEMENT_3D ( 'NONE', #5863, #4866, #26119 ) ;
#50080 = DIRECTION ( 'NONE',  ( 0.000000000000000000, 0.9985334138511239299, -0.05413890858541457046 ) ) ;
#50081 = DIRECTION ( 'NONE',  ( -1.000000000000000000, 0.000000000000000000, 0.000000000000000000 ) ) ;
#50082 = EDGE_CURVE ( 'NONE', #29886, #48262, #3375, .T. ) ;
#50083 = CARTESIAN_POINT ( 'NONE',  ( 7.118931388086720879, -4.897740429628226089, -12.58727760722467259 ) ) ;
#50084 = ADVANCED_FACE ( 'NONE', ( #46451 ), #51130, .T. ) ;
#50085 = CARTESIAN_POINT ( 'NONE',  ( -37.00000000000000711, 5.644643009979071202, 10.30098186818251982 ) ) ;
#50086 = DIRECTION ( 'NONE',  ( 1.000000000000000000, 0.000000000000000000, 0.000000000000000000 ) ) ;
#50087 = DIRECTION ( 'NONE',  ( -1.000000000000000000, -0.000000000000000000, 0.000000000000000000 ) ) ;
#50088 = VERTEX_POINT ( 'NONE', #45803 ) ;
#50089 = CARTESIAN_POINT ( 'NONE',  ( 2.491965175173335378, -6.046355957630531464, -4.796682362486714979 ) ) ;
#50090 = CARTESIAN_POINT ( 'NONE',  ( 17.27839441901508977, 12.20388373500084711, 5.771933972472493402 ) ) ;
#50091 = LINE ( 'NONE', #49757, #20617 ) ;
#50092 = EDGE_CURVE ( 'NONE', #42734, #52455, #33049, .T. ) ;
#50093 = VECTOR ( 'NONE', #14766, 1000.000000000000000 ) ;
#50094 = AXIS2_PLACEMENT_3D ( 'NONE', #40513, #60808, #15246 ) ;
#50095 = EDGE_CURVE ( 'NONE', #22010, #65658, #62756, .T. ) ;
#50096 = CARTESIAN_POINT ( 'NONE',  ( -15.99047871552766331, -35.00000000000001421, -5.006074194136237665 ) ) ;
#50097 = CARTESIAN_POINT ( 'NONE',  ( -28.12637923985837674, -10.04112151140785691, -6.578508732650774071 ) ) ;
#50098 =( BOUNDED_SURFACE ( )  B_SPLINE_SURFACE ( 3, 1, ( 
 ( #18780, #59028 ),
 ( #53031, #3507 ),
 ( #8462, #53376 ),
 ( #59334, #7466 ) ),
 .UNSPECIFIED., .F., .F., .F. ) 
 B_SPLINE_SURFACE_WITH_KNOTS ( ( 4, 4 ),
 ( 2, 2 ),
 ( 0.000000000000000000, 1.000000000000000000 ),
 ( 0.000000000000000000, 1.000000000000000000 ),
 .UNSPECIFIED. ) 
 GEOMETRIC_REPRESENTATION_ITEM ( )  RATIONAL_B_SPLINE_SURFACE ( (
 ( 1.000000000000000000, 1.000000000000000000),
 ( 0.9942764183789327692, 0.8450855930916580938),
 ( 0.9942764183789327692, 0.8450855930916580938),
 ( 1.000000000000000000, 1.000000000000000000) ) ) 
 REPRESENTATION_ITEM ( '' )  SURFACE ( )  );
#50099 = ORIENTED_EDGE ( 'NONE', *, *, #38027, .T. ) ;
#50100 = DIRECTION ( 'NONE',  ( 1.000000000000000000, 0.000000000000000000, 0.000000000000000000 ) ) ;
#50102 = EDGE_CURVE ( 'NONE', #53254, #45502, #1243, .T. ) ;
#50101 = CARTESIAN_POINT ( 'NONE',  ( 3.413903065650966351, -31.27385512440588400, -14.18194743136197289 ) ) ;
#50103 = VERTEX_POINT ( 'NONE', #31168 ) ;
#50104 = CARTESIAN_POINT ( 'NONE',  ( 1.462291587748817623, -6.862867011841285780, 10.62080802716765682 ) ) ;
#50105 = CARTESIAN_POINT ( 'NONE',  ( -22.59983133926797549, 4.650609684383191222, 0.06110861519532605202 ) ) ;
#50106 = DIRECTION ( 'NONE',  ( 0.000000000000000000, 0.000000000000000000, 1.000000000000000000 ) ) ;
#50107 = AXIS2_PLACEMENT_3D ( 'NONE', #20460, #55715, #51053 ) ;
#50108 = DIRECTION ( 'NONE',  ( -0.000000000000000000, -0.000000000000000000, -1.000000000000000000 ) ) ;
#50109 = CARTESIAN_POINT ( 'NONE',  ( -9.824684730204651828, -11.82156200828225145, -6.531049348231868557 ) ) ;
#50110 = CARTESIAN_POINT ( 'NONE',  ( 35.00000000000000000, 1.488153103996963100, -11.65150730582935523 ) ) ;
#50111 = EDGE_LOOP ( 'NONE', ( #4606, #64169, #12671, #13995, #6359, #9752 ) ) ;
#50112 = CARTESIAN_POINT ( 'NONE',  ( -22.59969328935897437, 0.7214993884004556879, -4.594269189967459255 ) ) ;
#50113 = AXIS2_PLACEMENT_3D ( 'NONE', #41713, #11141, #37714 ) ;
#50114 = CARTESIAN_POINT ( 'NONE',  ( 1.719304012338199517, 0.000000000000000000, 0.000000000000000000 ) ) ;
#50115 = CARTESIAN_POINT ( 'NONE',  ( -17.47051625687515397, 7.643161633986498948, -11.12960797627961007 ) ) ;
#50116 = CARTESIAN_POINT ( 'NONE',  ( 9.382205902475009296, 7.259643443602203483, -11.38652836844183369 ) ) ;
#50117 =( BOUNDED_SURFACE ( )  B_SPLINE_SURFACE ( 3, 1, ( 
 ( #25046, #14066 ),
 ( #65578, #15385 ),
 ( #41955, #6082 ),
 ( #60947, #31001 ) ),
 .UNSPECIFIED., .F., .F., .F. ) 
 B_SPLINE_SURFACE_WITH_KNOTS ( ( 4, 4 ),
 ( 2, 2 ),
 ( 0.000000000000000000, 1.000000000000000000 ),
 ( 0.000000000000000000, 1.000000000000000000 ),
 .UNSPECIFIED. ) 
 GEOMETRIC_REPRESENTATION_ITEM ( )  RATIONAL_B_SPLINE_SURFACE ( (
 ( 1.000000000000000000, 1.000000000000000000),
 ( 0.9942764183789327692, 0.8450855930916585379),
 ( 0.9942764183789327692, 0.8450855930916585379),
 ( 1.000000000000000000, 1.000000000000000000) ) ) 
 REPRESENTATION_ITEM ( '' )  SURFACE ( )  );
#50118 = CARTESIAN_POINT ( 'NONE',  ( 35.00000000000000000, -11.70009620280412399, -1.039216533672868481 ) ) ;
#50119 = FACE_OUTER_BOUND ( 'NONE', #2630, .T. ) ;
#50120 = CARTESIAN_POINT ( 'NONE',  ( 19.56743653832047514, -28.99999999999999645, 4.999999999999997335 ) ) ;
#50121 = EDGE_LOOP ( 'NONE', ( #3011, #48351, #46654, #57843 ) ) ;
#50122 = EDGE_LOOP ( 'NONE', ( #39009, #2059, #25431, #58136 ) ) ;
#50123 = CARTESIAN_POINT ( 'NONE',  ( 2.241311220309554653, -4.978033760028411692, 5.788190037953256706 ) ) ;
#50124 = VERTEX_POINT ( 'NONE', #36478 ) ;
#50125 =( LENGTH_UNIT ( ) NAMED_UNIT ( * ) SI_UNIT ( .MILLI., .METRE. ) );
#50127 = DIRECTION ( 'NONE',  ( -0.000000000000000000, 1.000000000000000000, 0.000000000000000000 ) ) ;
#50126 = CIRCLE ( 'NONE', #10808, 4.000000000000000000 ) ;
#50128 = EDGE_CURVE ( 'NONE', #54202, #16892, #20535, .T. ) ;
#50129 = AXIS2_PLACEMENT_3D ( 'NONE', #56870, #35234, #30573 ) ;
#50130 = EDGE_CURVE ( 'NONE', #59008, #39168, #57526, .T. ) ;
#50131 = AXIS2_PLACEMENT_3D ( 'NONE', #4473, #50673, #29705 ) ;
#50132 = ORIENTED_EDGE ( 'NONE', *, *, #49850, .F. ) ;
#50133 = CARTESIAN_POINT ( 'NONE',  ( -35.00000000000000000, 12.01765980939845058, -2.021542716731266065 ) ) ;
#50134 = CARTESIAN_POINT ( 'NONE',  ( 10.35219383903665857, 11.93001091997956919, -1.309405142360217544 ) ) ;
#50135 = DIRECTION ( 'NONE',  ( 0.000000000000000000, 0.01356324068817998940, -0.9999080150203990547 ) ) ;
#50136 = ORIENTED_EDGE ( 'NONE', *, *, #54006, .F. ) ;
#50137 = ORIENTED_EDGE ( 'NONE', *, *, #9979, .T. ) ;
#50138 = DIRECTION ( 'NONE',  ( 1.000000000000000000, 0.000000000000000000, 0.000000000000000000 ) ) ;
#50139 = ADVANCED_FACE ( 'NONE', ( #11212 ), #31487, .T. ) ;
#50140 = VERTEX_POINT ( 'NONE', #46780 ) ;
#50141 = CARTESIAN_POINT ( 'NONE',  ( 2.000000000000001776, -5.585096664091960150, 4.113602740025890547 ) ) ;
#50142 = VERTEX_POINT ( 'NONE', #21523 ) ;
#50143 = AXIS2_PLACEMENT_3D ( 'NONE', #44983, #34008, #4093 ) ;
#50144 = DIRECTION ( 'NONE',  ( -1.000000000000000000, -0.000000000000000000, 0.000000000000000000 ) ) ;
#50145 = CARTESIAN_POINT ( 'NONE',  ( -27.10422407540546885, 1.039355862229912164, -2.109093808474372889 ) ) ;
#50146 = AXIS2_PLACEMENT_3D ( 'NONE', #63567, #8072, #18386 ) ;
#50147 = CARTESIAN_POINT ( 'NONE',  ( 2.899286259009678179, -4.231523595108526159, 6.616268644969679258 ) ) ;
#50148 = FACE_BOUND ( 'NONE', #64635, .T. ) ;
#50149 = EDGE_CURVE ( 'NONE', #26657, #64905, #53798, .T. ) ;
#50150 = CARTESIAN_POINT ( 'NONE',  ( 1.719304012338199517, 0.000000000000000000, 0.000000000000000000 ) ) ;
#50151 = ORIENTED_EDGE ( 'NONE', *, *, #50217, .F. ) ;
#50152 = CARTESIAN_POINT ( 'NONE',  ( 2.000000000000001776, 6.164400007374793766, -2.900694413976553143 ) ) ;
#50153 = CARTESIAN_POINT ( 'NONE',  ( -17.96188634106787063, 6.007102645581881895, 10.39092871488517389 ) ) ;
#50154 = CIRCLE ( 'NONE', #24656, 1.500000000000000444 ) ;
#50155 = CARTESIAN_POINT ( 'NONE',  ( 0.2648978790185593790, -0.1321385342563263510, 12.24533305150758089 ) ) ;
#50156 = EDGE_CURVE ( 'NONE', #4686, #23899, #42572, .T. ) ;
#50157 = CARTESIAN_POINT ( 'NONE',  ( 35.00000000000000000, 8.258652103341434625, -8.352657516904704593 ) ) ;
#50158 = CARTESIAN_POINT ( 'NONE',  ( 2.241449424704146320, -7.507583637787357489, 1.386092121067182159 ) ) ;
#50159 = CARTESIAN_POINT ( 'NONE',  ( 23.75066733795811658, -3.115628287466211344, 13.13955084818059404 ) ) ;
#50160 = CARTESIAN_POINT ( 'NONE',  ( -35.00000000000000000, 12.16632754454237819, -0.7008968033237440443 ) ) ;
#50161 = CYLINDRICAL_SURFACE ( 'NONE', #33393, 12.18649999999999878 ) ;
#50162 = CARTESIAN_POINT ( 'NONE',  ( 0.000000000000000000, 0.000000000000000000, 0.000000000000000000 ) ) ;
#50163 = ORIENTED_EDGE ( 'NONE', *, *, #9030, .T. ) ;
#50164 = CARTESIAN_POINT ( 'NONE',  ( -17.08774245407508019, 7.933722547746723919, -9.005484594861211889 ) ) ;
#50165 = CIRCLE ( 'NONE', #21489, 12.75000000000000178 ) ;
#50166 = VERTEX_POINT ( 'NONE', #57099 ) ;
#50167 = DIRECTION ( 'NONE',  ( 1.000000000000000000, 0.000000000000000000, 0.000000000000000000 ) ) ;
#50168 = CARTESIAN_POINT ( 'NONE',  ( -22.27786964138239867, -3.667590411552013929, 0.3434379038477752277 ) ) ;
#50169 = ADVANCED_FACE ( 'NONE', ( #21855 ), #31795, .T. ) ;
#50170 = DIRECTION ( 'NONE',  ( -1.000000000000000000, 0.000000000000000000, 0.000000000000000000 ) ) ;
#50171 = DIRECTION ( 'NONE',  ( 0.000000000000000000, -0.01356324068817991828, 0.9999080150203990547 ) ) ;
#50172 = CARTESIAN_POINT ( 'NONE',  ( 35.00000000000000000, 8.235637554476779698, 9.733281772932071974 ) ) ;
#50173 = EDGE_CURVE ( 'NONE', #43014, #36640, #51109, .T. ) ;
#50174 = ORIENTED_EDGE ( 'NONE', *, *, #57846, .F. ) ;
#50175 = CARTESIAN_POINT ( 'NONE',  ( 2.665405856346786173, 0.5773576323839043622, -9.549966053095394258 ) ) ;
#50176 = CARTESIAN_POINT ( 'NONE',  ( 2.241317068080780128, -3.737686401540277537, 6.656851426547345518 ) ) ;
#50177 = CARTESIAN_POINT ( 'NONE',  ( 10.28253184321369140, 1.474010143406270679, 11.91011122907010922 ) ) ;
#50178 = CARTESIAN_POINT ( 'NONE',  ( -22.28073302975501235, 2.626377654649359794, 2.595086548179975416 ) ) ;
#50179 = EDGE_CURVE ( 'NONE', #44827, #55595, #22418, .T. ) ;
#50180 = AXIS2_PLACEMENT_3D ( 'NONE', #19107, #28750, #23787 ) ;
#50181 = CIRCLE ( 'NONE', #62880, 5.000000000000000000 ) ;
#50182 = ADVANCED_FACE ( 'NONE', ( #17519 ), #1569, .F. ) ;
#50183 = DIRECTION ( 'NONE',  ( -1.000000000000000000, -0.000000000000000000, -0.000000000000000000 ) ) ;
#50184 = ORIENTED_EDGE ( 'NONE', *, *, #33585, .F. ) ;
#50186 = EDGE_CURVE ( 'NONE', #31213, #9689, #30918, .T. ) ;
#50185 = CARTESIAN_POINT ( 'NONE',  ( 0.000000000000000000, 7.248432822490259220, 1.926193556693033271 ) ) ;
#50187 = ORIENTED_EDGE ( 'NONE', *, *, #20161, .F. ) ;
#50188 = DIRECTION ( 'NONE',  ( -1.000000000000000000, -0.000000000000000000, 0.000000000000000000 ) ) ;
#50189 = CARTESIAN_POINT ( 'NONE',  ( 0.000000000000000000, -4.570217215903314312, -5.218059682435693958 ) ) ;
#50190 = DIRECTION ( 'NONE',  ( 0.000000000000000000, -0.8835120444460272671, 0.4684084406997819916 ) ) ;
#50191 = VECTOR ( 'NONE', #41099, 1000.000000000000000 ) ;
#50192 = CYLINDRICAL_SURFACE ( 'NONE', #53263, 5.000000000000002665 ) ;
#50193 = AXIS2_PLACEMENT_3D ( 'NONE', #13611, #2704, #63492 ) ;
#50194 = VERTEX_POINT ( 'NONE', #63056 ) ;
#50195 = ORIENTED_EDGE ( 'NONE', *, *, #12585, .T. ) ;
#50196 = CARTESIAN_POINT ( 'NONE',  ( -27.08850691366480490, 2.218359546717756370, -0.6228349286848119393 ) ) ;
#50197 = ORIENTED_EDGE ( 'NONE', *, *, #387, .F. ) ;
#50198 = CYLINDRICAL_SURFACE ( 'NONE', #24532, 5.000000000000000888 ) ;
#50200 = AXIS2_PLACEMENT_3D ( 'NONE', #65472, #60492, #19935 ) ;
#50199 = CARTESIAN_POINT ( 'NONE',  ( 37.00000000000000711, 4.705694406421931860E-17, -3.469127814946512892E-15 ) ) ;
#50201 = CARTESIAN_POINT ( 'NONE',  ( 35.00000000000000000, -9.926225166346981155, 6.280308599560240346 ) ) ;
#50202 = LINE ( 'NONE', #19923, #36437 ) ;
#50203 = CARTESIAN_POINT ( 'NONE',  ( 35.00000000000000000, 4.705694406421931860E-17, -3.469127814946512892E-15 ) ) ;
#50204 = AXIS2_PLACEMENT_3D ( 'NONE', #53155, #3630, #43484 ) ;
#50205 = LINE ( 'NONE', #28033, #32786 ) ;
#50206 = CARTESIAN_POINT ( 'NONE',  ( 2.000000000000001776, -6.936109781200651803, -2.853135311045104316 ) ) ;
#50207 = ORIENTED_EDGE ( 'NONE', *, *, #61651, .T. ) ;
#50209 = ORIENTED_EDGE ( 'NONE', *, *, #6500, .F. ) ;
#50208 = CARTESIAN_POINT ( 'NONE',  ( 0.3053067050349180800, -12.03105545708855395, -2.355726819985549891 ) ) ;
#50210 = EDGE_LOOP ( 'NONE', ( #3368, #48886, #37612, #35857 ) ) ;
#50211 = CARTESIAN_POINT ( 'NONE',  ( 0.4613984246114871679, -2.415907815801322300, -12.07219521825822817 ) ) ;
#50212 = CARTESIAN_POINT ( 'NONE',  ( -27.08871896697694837, 1.896680818244936617, -1.309412067288129311 ) ) ;
#50213 = EDGE_CURVE ( 'NONE', #25571, #20337, #4402, .T. ) ;
#50214 = ORIENTED_EDGE ( 'NONE', *, *, #59765, .T. ) ;
#50215 = AXIS2_PLACEMENT_3D ( 'NONE', #17189, #37465, #62090 ) ;
#50216 = DIRECTION ( 'NONE',  ( -0.6334066780386838902, 0.000000000000000000, -0.7738190875236917732 ) ) ;
#50217 = EDGE_CURVE ( 'NONE', #28860, #65138, #37789, .T. ) ;
#50218 = ORIENTED_EDGE ( 'NONE', *, *, #54229, .T. ) ;
#50219 = DIRECTION ( 'NONE',  ( 0.000000000000000000, -0.01356324068817998767, 0.9999080150203990547 ) ) ;
#50220 = CARTESIAN_POINT ( 'NONE',  ( 37.00000000000000711, 4.705694406421931860E-17, -3.469127814946512892E-15 ) ) ;
#50221 = FACE_OUTER_BOUND ( 'NONE', #484, .T. ) ;
#50222 = CARTESIAN_POINT ( 'NONE',  ( 6.320217901527452220, -9.250799897007995654, 7.654551209031711601 ) ) ;
#50223 = EDGE_LOOP ( 'NONE', ( #29031, #23488, #38630, #10455 ) ) ;
#50224 = ORIENTED_EDGE ( 'NONE', *, *, #21930, .F. ) ;
#50225 = CARTESIAN_POINT ( 'NONE',  ( -36.00000000000000711, 12.46157735505193109, -2.696588552978925524 ) ) ;
#50226 = ORIENTED_EDGE ( 'NONE', *, *, #57277, .T. ) ;
#50227 = CARTESIAN_POINT ( 'NONE',  ( 0.3401186441510247183, 11.61600526280576595, -3.955862996551386512 ) ) ;
#50228 = EDGE_LOOP ( 'NONE', ( #3595, #50471, #26965, #54543 ) ) ;
#50229 = AXIS2_PLACEMENT_3D ( 'NONE', #57714, #26448, #12136 ) ;
#50230 = EDGE_CURVE ( 'NONE', #45140, #62469, #1891, .T. ) ;
#50231 = VECTOR ( 'NONE', #19200, 1000.000000000000114 ) ;
#50232 = ORIENTED_EDGE ( 'NONE', *, *, #64302, .T. ) ;
#50233 = VERTEX_POINT ( 'NONE', #7189 ) ;
#50234 = CARTESIAN_POINT ( 'NONE',  ( -36.00000000000000711, 0.4871980014163243000, -12.74068829017553561 ) ) ;
#50235 = CARTESIAN_POINT ( 'NONE',  ( -9.737135312703241397, -26.73636926326595642, 14.00099174170044058 ) ) ;
#50236 = CARTESIAN_POINT ( 'NONE',  ( 35.00000000000000000, -10.80631716521670427, -4.603882218679513194 ) ) ;
#50237 = CARTESIAN_POINT ( 'NONE',  ( -37.00000000000000711, 5.927257550915472351, -10.64792938439748937 ) ) ;
#50238 = VERTEX_POINT ( 'NONE', #53082 ) ;
#50239 = CARTESIAN_POINT ( 'NONE',  ( -35.00000000000000000, -1.791059740004510070, 12.05416472667165273 ) ) ;
#50240 = ORIENTED_EDGE ( 'NONE', *, *, #48689, .T. ) ;
#50241 = CYLINDRICAL_SURFACE ( 'NONE', #64606, 12.18649999999999878 ) ;
#50242 = DIRECTION ( 'NONE',  ( 0.000000000000000000, -6.879075853011489629E-15, 1.000000000000000000 ) ) ;
#50243 = EDGE_CURVE ( 'NONE', #57170, #5815, #28832, .T. ) ;
#50244 = ORIENTED_EDGE ( 'NONE', *, *, #39001, .F. ) ;
#50245 = CARTESIAN_POINT ( 'NONE',  ( 5.530133899448235191, 0.01437126147332072092, 0.006998616117864119544 ) ) ;
#50246 = AXIS2_PLACEMENT_3D ( 'NONE', #5524, #21107, #41384 ) ;
#50247 = CARTESIAN_POINT ( 'NONE',  ( 0.3218525148189836371, 3.964374483810649163, 11.60666749448225232 ) ) ;
#50248 = CARTESIAN_POINT ( 'NONE',  ( 2.263328370261521894, -6.687792802426766769, -3.697218830764027686 ) ) ;
#50249 = EDGE_CURVE ( 'NONE', #3889, #43541, #12868, .T. ) ;
#50250 = ORIENTED_EDGE ( 'NONE', *, *, #53441, .T. ) ;
#50251 = CARTESIAN_POINT ( 'NONE',  ( 1.547277799337855475, 6.911346840319977147, 10.62321481610070784 ) ) ;
#50252 = ORIENTED_EDGE ( 'NONE', *, *, #17449, .T. ) ;
#50253 = CARTESIAN_POINT ( 'NONE',  ( 0.3006302518452059758, 10.72687985734942373, 5.932248915294198177 ) ) ;
#50254 = CARTESIAN_POINT ( 'NONE',  ( -37.00000000000000711, -11.86701198550358427, 2.772148766916072926 ) ) ;
#50255 = VECTOR ( 'NONE', #37283, 1000.000000000000000 ) ;
#50256 = FACE_OUTER_BOUND ( 'NONE', #40808, .T. ) ;
#50257 = DIRECTION ( 'NONE',  ( 1.000000000000000000, 0.000000000000000000, 0.000000000000000000 ) ) ;
#50258 = CARTESIAN_POINT ( 'NONE',  ( -37.00000000000000711, 0.000000000000000000, 0.000000000000000000 ) ) ;
#50259 = EDGE_LOOP ( 'NONE', ( #35689, #57863, #23818, #16424 ) ) ;
#50260 = CARTESIAN_POINT ( 'NONE',  ( 2.257661810676424796, -4.806737555285489627, 5.938215228162603054 ) ) ;
#50261 = DIRECTION ( 'NONE',  ( 0.000000000000000000, 0.3807014730195152907, -0.9246979985058750851 ) ) ;
#50262 = CARTESIAN_POINT ( 'NONE',  ( -27.35552965826137140, -1.773915698030568366, 2.548625910254532112 ) ) ;
#50263 = CARTESIAN_POINT ( 'NONE',  ( 0.4626703367444975346, 1.858541096401209902, 12.17089897506927620 ) ) ;
#50264 = EDGE_CURVE ( 'NONE', #37599, #45626, #22159, .T. ) ;
#50265 = CIRCLE ( 'NONE', #44928, 7.938172270156617749 ) ;
#50266 = EDGE_CURVE ( 'NONE', #34038, #10268, #38100, .T. ) ;
#50267 = CARTESIAN_POINT ( 'NONE',  ( -19.27703245284566691, -30.00000000000001066, -5.988254523999591683 ) ) ;
#50269 = EDGE_CURVE ( 'NONE', #59063, #43191, #62712, .T. ) ;
#50268 = CARTESIAN_POINT ( 'NONE',  ( -22.27218376572352554, 2.577901515391834764, -2.630375585211903733 ) ) ;
#50270 = CARTESIAN_POINT ( 'NONE',  ( 2.257661810676416803, -5.938215228162571968, -4.806737555285515384 ) ) ;
#50271 = LINE ( 'NONE', #49930, #52736 ) ;
#50272 = CARTESIAN_POINT ( 'NONE',  ( 2.000000000000001776, 0.000000000000000000, 0.000000000000000000 ) ) ;
#50273 = CIRCLE ( 'NONE', #37481, 5.000000000000000000 ) ;
#50274 = CIRCLE ( 'NONE', #13096, 12.74999999999999822 ) ;
#50275 = VECTOR ( 'NONE', #14411, 1000.000000000000227 ) ;
#50276 = B_SPLINE_CURVE_WITH_KNOTS ( 'NONE', 3,
 ( #41094, #20169, #25825, #35112, #4573, #25482, #56066, #36095, #14504, #24841, #9861, #15500, #30781, #10847, #5893, #30151 ),
 .UNSPECIFIED., .F., .F.,
 ( 4, 3, 3, 3, 3, 4 ),
 ( 0.000000000000000000, 0.0002999043160757426532, 0.0005998071753051172636, 0.0008997092107374794973, 0.001204458948196454778, 0.001510329163478115952 ),
 .UNSPECIFIED. ) ;
#50277 = EDGE_CURVE ( 'NONE', #21283, #3374, #40502, .T. ) ;
#50278 = ORIENTED_EDGE ( 'NONE', *, *, #7305, .F. ) ;
#50279 = LINE ( 'NONE', #34619, #39527 ) ;
#50280 = EDGE_LOOP ( 'NONE', ( #17055, #36617, #48429, #29786 ) ) ;
#50281 = DIRECTION ( 'NONE',  ( 0.000000000000000000, 0.4198891015602657650, -0.9075754196709565624 ) ) ;
#50282 = CARTESIAN_POINT ( 'NONE',  ( 5.516018279890452902, -0.0009545156522404840260, 0.006707902355168859562 ) ) ;
#50283 = CARTESIAN_POINT ( 'NONE',  ( 2.994568964204212147, -7.537093683963806967, 2.317954327151198868 ) ) ;
#50284 = AXIS2_PLACEMENT_3D ( 'NONE', #47232, #15945, #56544 ) ;
#50285 = B_SPLINE_CURVE_WITH_KNOTS ( 'NONE', 3,
 ( #47201, #27222, #1956, #21593, #26562, #47516, #46851, #41858 ),
 .UNSPECIFIED., .F., .F.,
 ( 4, 2, 2, 4 ),
 ( 0.000000000000000000, 0.0003639104015150009929, 0.0007278208030300019858, 0.001455641606060005273 ),
 .UNSPECIFIED. ) ;
#50286 = FACE_OUTER_BOUND ( 'NONE', #36206, .T. ) ;
#50287 = EDGE_LOOP ( 'NONE', ( #10894, #3137, #24864, #60832 ) ) ;
#50288 = AXIS2_PLACEMENT_3D ( 'NONE', #1358, #41901, #50907 ) ;
#50289 = VERTEX_POINT ( 'NONE', #43760 ) ;
#50290 = ORIENTED_EDGE ( 'NONE', *, *, #25982, .F. ) ;
#50291 = CARTESIAN_POINT ( 'NONE',  ( -10.90165637462999904, -7.508992741355383416, -9.360289953322597611 ) ) ;
#50292 = CONICAL_SURFACE ( 'NONE', #1405, 7.938172270156617749, 1.280189991382167047 ) ;
#50293 = CARTESIAN_POINT ( 'NONE',  ( 2.524535260912702306, 3.671333852642910678, -6.801151891677163164 ) ) ;
#50294 = VERTEX_POINT ( 'NONE', #57765 ) ;
#50295 = DIRECTION ( 'NONE',  ( 1.000000000000000000, 0.000000000000000000, 0.000000000000000000 ) ) ;
#50296 = CARTESIAN_POINT ( 'NONE',  ( 35.00000000000000000, 4.705694406421931860E-17, -3.469127814946512892E-15 ) ) ;
#50297 = CARTESIAN_POINT ( 'NONE',  ( 3.092491956585575963, -2.283527081234287603, 7.581757403488253111 ) ) ;
#50298 = EDGE_CURVE ( 'NONE', #15913, #45235, #64942, .T. ) ;
#50299 = EDGE_LOOP ( 'NONE', ( #23806, #19372, #44535, #16597 ) ) ;
#50300 = CARTESIAN_POINT ( 'NONE',  ( 35.00000000000000000, -9.060822531525994705, 7.474872387601095625 ) ) ;
#50301 = AXIS2_PLACEMENT_3D ( 'NONE', #19651, #39909, #60191 ) ;
#50302 = CARTESIAN_POINT ( 'NONE',  ( -5.261125060310215318, -26.86576352283318059, -15.75274798952653832 ) ) ;
#50303 = CYLINDRICAL_SURFACE ( 'NONE', #10111, 6.595312090839647645 ) ;
#50305 = ORIENTED_EDGE ( 'NONE', *, *, #31860, .T. ) ;
#50304 = CARTESIAN_POINT ( 'NONE',  ( 35.00000000000000000, 11.39945968423471356, -5.710938531231753323 ) ) ;
#50306 = CARTESIAN_POINT ( 'NONE',  ( -36.00000000000000711, 11.01837265713082203, -6.415447294506590126 ) ) ;
#50307 = ORIENTED_EDGE ( 'NONE', *, *, #18013, .T. ) ;
#50308 = CYLINDRICAL_SURFACE ( 'NONE', #33710, 4.999999999999999112 ) ;
#50309 = ORIENTED_EDGE ( 'NONE', *, *, #37159, .F. ) ;
#50310 = CARTESIAN_POINT ( 'NONE',  ( -29.14105348823734687, 1.985002961251433051, -11.86469874868790519 ) ) ;
#50311 = CARTESIAN_POINT ( 'NONE',  ( -35.05012975565874456, -0.004360246756757623493, 0.01323209221895336324 ) ) ;
#50312 = DIRECTION ( 'NONE',  ( 1.000000000000000000, -0.000000000000000000, 0.000000000000000000 ) ) ;
#50313 = DIRECTION ( 'NONE',  ( -1.000000000000000000, 0.000000000000000000, 0.000000000000000000 ) ) ;
#50314 = CARTESIAN_POINT ( 'NONE',  ( -22.27722019117889829, 0.6493872998088092707, 3.623937139367928939 ) ) ;
#50315 = CIRCLE ( 'NONE', #2571, 4.999999999999999112 ) ;
#50316 = DIRECTION ( 'NONE',  ( -1.000000000000000000, -0.000000000000000000, -0.000000000000000000 ) ) ;
#50317 = CARTESIAN_POINT ( 'NONE',  ( 2.247112776671469359, 5.774169979601987635, -4.997244136394421332 ) ) ;
#50318 = CARTESIAN_POINT ( 'NONE',  ( -14.47334165536099881, 5.400000000000000355, 1.000000000000000000 ) ) ;
#50319 = LINE ( 'NONE', #25346, #10943 ) ;
#50321 = ORIENTED_EDGE ( 'NONE', *, *, #53318, .T. ) ;
#50320 = CARTESIAN_POINT ( 'NONE',  ( 2.000000000000001776, 0.000000000000000000, 0.000000000000000000 ) ) ;
#50322 = CARTESIAN_POINT ( 'NONE',  ( 2.406456491627198879, 10.00134798414537229, 2.970787154400166941 ) ) ;
#50323 =( BOUNDED_CURVE ( )  B_SPLINE_CURVE ( 3, ( #49208, #3664, #63471, #17942 ),
 .UNSPECIFIED., .F., .F. ) 
 B_SPLINE_CURVE_WITH_KNOTS ( ( 4, 4 ),
 ( 3.730491548985638506, 3.779698989410085197 ),
 .UNSPECIFIED. ) 
 CURVE ( )  GEOMETRIC_REPRESENTATION_ITEM ( )  RATIONAL_B_SPLINE_CURVE ( ( 1.000000000000000000, 0.9997982291625954199, 0.9997982291625954199, 1.000000000000000000 ) ) 
 REPRESENTATION_ITEM ( '' )  );
#50324 = ORIENTED_EDGE ( 'NONE', *, *, #40148, .T. ) ;
#50325 = CARTESIAN_POINT ( 'NONE',  ( 12.10998784662220729, -10.46621227226782835, -8.526922110106905706 ) ) ;
#50326 = ORIENTED_EDGE ( 'NONE', *, *, #47180, .T. ) ;
#50327 = ADVANCED_FACE ( 'NONE', ( #28458 ), #48760, .T. ) ;
#50328 = VECTOR ( 'NONE', #25293, 1000.000000000000000 ) ;
#50329 = ORIENTED_EDGE ( 'NONE', *, *, #40282, .F. ) ;
#50331 = AXIS2_PLACEMENT_3D ( 'NONE', #21423, #36384, #6141 ) ;
#50330 = CARTESIAN_POINT ( 'NONE',  ( 0.3109076770649021881, 8.060731492642796425, 9.239379580302124140 ) ) ;
#50332 = DIRECTION ( 'NONE',  ( 0.000000000000000000, 0.5243256840888561587, 0.8515178078024868702 ) ) ;
#50333 = CARTESIAN_POINT ( 'NONE',  ( -35.00000000000000000, 10.80478261802190154, -5.636262487437199376 ) ) ;
#50334 = B_SPLINE_CURVE_WITH_KNOTS ( 'NONE', 3,
 ( #59096, #59400, #33788, #54089, #53774, #19162, #55059, #64376, #45096, #9489, #9175, #44748, #54755 ),
 .UNSPECIFIED., .F., .F.,
 ( 4, 3, 3, 3, 4 ),
 ( 2.168404344971008868E-18, 6.607593386745438881E-05, 0.0001321518677373501841, 0.0001982171734706190437, 0.0002642860854759493676 ),
 .UNSPECIFIED. ) ;
#50335 = LINE ( 'NONE', #4785, #63522 ) ;
#50336 = EDGE_CURVE ( 'NONE', #17474, #17695, #24134, .T. ) ;
#50337 = CIRCLE ( 'NONE', #29097, 12.18650000000000055 ) ;
#50338 = CYLINDRICAL_SURFACE ( 'NONE', #19192, 12.75000000000000178 ) ;
#50339 = DIRECTION ( 'NONE',  ( -1.000000000000000000, -0.000000000000000000, 0.000000000000000000 ) ) ;
#50340 = ORIENTED_EDGE ( 'NONE', *, *, #50456, .T. ) ;
#50341 = CARTESIAN_POINT ( 'NONE',  ( 2.000000000000001776, 0.000000000000000000, 0.000000000000000000 ) ) ;
#50342 = AXIS2_PLACEMENT_3D ( 'NONE', #17936, #27571, #23248 ) ;
#50343 = DIRECTION ( 'NONE',  ( 0.4622435816439414147, -0.000000000000000000, 0.8867529933577789070 ) ) ;
#50344 = CARTESIAN_POINT ( 'NONE',  ( 1.109979610369347114, 12.24510427445464522, 2.646302643131894783 ) ) ;
#50345 = ORIENTED_EDGE ( 'NONE', *, *, #55307, .T. ) ;
#50346 = VECTOR ( 'NONE', #55735, 1000.000000000000000 ) ;
#50347 = ADVANCED_FACE ( 'NONE', ( #19484 ), #39414, .T. ) ;
#50348 = CIRCLE ( 'NONE', #29069, 12.75000000000000178 ) ;
#50349 = CARTESIAN_POINT ( 'NONE',  ( 36.06592381555555704, -2.436921198044744497, 22.43244911821615162 ) ) ;
#50350 = CIRCLE ( 'NONE', #3662, 12.73084802173761787 ) ;
#50351 = DIRECTION ( 'NONE',  ( 0.000000000000000000, -0.1740410799127686259, -0.9847383929261604996 ) ) ;
#50352 = CARTESIAN_POINT ( 'NONE',  ( -49.78928762170311018, -0.04292493490549997154, -3.265281182697543638 ) ) ;
#50353 = ORIENTED_EDGE ( 'NONE', *, *, #20045, .F. ) ;
#50354 = CARTESIAN_POINT ( 'NONE',  ( 2.242819959140646358, 6.662619100654793236, -3.728423299584912254 ) ) ;
#50355 = FACE_OUTER_BOUND ( 'NONE', #56225, .T. ) ;
#50356 = CARTESIAN_POINT ( 'NONE',  ( 3.780834652287974773, 8.352030633203074927, 8.616471685210687070 ) ) ;
#50357 = EDGE_CURVE ( 'NONE', #40350, #54896, #45887, .T. ) ;
#50358 = CIRCLE ( 'NONE', #34434, 5.000000000000000888 ) ;
#50359 = DIRECTION ( 'NONE',  ( 0.000000000000000000, 0.01356324068817992175, -0.9999080150203990547 ) ) ;
#50360 = CARTESIAN_POINT ( 'NONE',  ( 5.516018279890452902, 0.0002248006052448508899, 0.006771744149385265123 ) ) ;
#50361 = ORIENTED_EDGE ( 'NONE', *, *, #12758, .F. ) ;
#50362 = CARTESIAN_POINT ( 'NONE',  ( 2.288423627607478306, 0.1612945702821758642, 7.648392725410191773 ) ) ;
#50363 = CARTESIAN_POINT ( 'NONE',  ( 0.3537226245948360548, -12.13174752084887587, 1.874138792912971807 ) ) ;
#50364 = CARTESIAN_POINT ( 'NONE',  ( 37.00000000000000711, -4.074242145636093326, -12.08151691381188719 ) ) ;
#50365 = VERTEX_POINT ( 'NONE', #49103 ) ;
#50366 = CARTESIAN_POINT ( 'NONE',  ( 21.63471773768895190, 12.68614566336015947, -4.633447873545391893 ) ) ;
#50367 = DIRECTION ( 'NONE',  ( -1.000000000000000000, 0.000000000000000000, -0.000000000000000000 ) ) ;
#50368 = ORIENTED_EDGE ( 'NONE', *, *, #45260, .F. ) ;
#50369 = CIRCLE ( 'NONE', #41848, 2.899999999999993694 ) ;
#50370 = ORIENTED_EDGE ( 'NONE', *, *, #1434, .T. ) ;
#50371 = ORIENTED_EDGE ( 'NONE', *, *, #32404, .T. ) ;
#50372 = ORIENTED_EDGE ( 'NONE', *, *, #10327, .F. ) ;
#50373 = DIRECTION ( 'NONE',  ( 1.000000000000000000, -0.000000000000000000, 0.000000000000000000 ) ) ;
#50374 = CARTESIAN_POINT ( 'NONE',  ( -22.70624764888619751, -2.702761586319157860, 4.501516772829871726 ) ) ;
#50375 = CARTESIAN_POINT ( 'NONE',  ( -35.00000000000000000, 0.000000000000000000, 0.000000000000000000 ) ) ;
#50376 = CARTESIAN_POINT ( 'NONE',  ( -22.38932658256920405, -2.201197575855953659, -3.361598243548662879 ) ) ;
#50377 = EDGE_CURVE ( 'NONE', #36681, #53717, #58621, .T. ) ;
#50378 = CARTESIAN_POINT ( 'NONE',  ( -14.91771861688918399, -27.95837112815216230, 11.21176701200369763 ) ) ;
#50379 = DIRECTION ( 'NONE',  ( 1.000000000000000000, 0.000000000000000000, 0.000000000000000000 ) ) ;
#50381 = ORIENTED_EDGE ( 'NONE', *, *, #18479, .F. ) ;
#50380 = CARTESIAN_POINT ( 'NONE',  ( -37.00000000000000711, -6.753013023069787124, 10.14433819232432477 ) ) ;
#50382 = EDGE_CURVE ( 'NONE', #57089, #19062, #8669, .T. ) ;
#50383 = FACE_OUTER_BOUND ( 'NONE', #25488, .T. ) ;
#50384 = ORIENTED_EDGE ( 'NONE', *, *, #62965, .F. ) ;
#50385 = CARTESIAN_POINT ( 'NONE',  ( 0.2646305136544065406, -11.55263159009955842, -4.064188116014664232 ) ) ;
#50386 = VECTOR ( 'NONE', #20052, 1000.000000000000000 ) ;
#50387 = ORIENTED_EDGE ( 'NONE', *, *, #24873, .T. ) ;
#50388 = EDGE_LOOP ( 'NONE', ( #17989, #40774, #6049, #37108 ) ) ;
#50389 = CARTESIAN_POINT ( 'NONE',  ( -22.28546858134833286, -0.9133285433746629600, 3.592117891549486242 ) ) ;
#50390 = CARTESIAN_POINT ( 'NONE',  ( 12.84304429912246981, -30.00680403999870194, 7.859709520792756088 ) ) ;
#50391 = VECTOR ( 'NONE', #11274, 1000.000000000000000 ) ;
#50392 = CARTESIAN_POINT ( 'NONE',  ( 1.719304012338249921, 10.22720798541395837, 7.581471372740089976 ) ) ;
#50393 = EDGE_CURVE ( 'NONE', #22233, #17330, #18446, .T. ) ;
#50394 = CARTESIAN_POINT ( 'NONE',  ( 2.899286259009685285, 7.788326766693364434, -1.011320371384261341 ) ) ;
#50395 = CARTESIAN_POINT ( 'NONE',  ( -19.02967556479663713, 11.99999999999999645, 1.585036030062028271E-15 ) ) ;
#50396 = CARTESIAN_POINT ( 'NONE',  ( 2.266490820341525048, 5.947069344278602898, 4.800466063946337236 ) ) ;
#50397 = VERTEX_POINT ( 'NONE', #20124 ) ;
#50398 = ORIENTED_EDGE ( 'NONE', *, *, #3739, .F. ) ;
#50399 = DIRECTION ( 'NONE',  ( 0.000000000000000000, 0.01356324068817998940, -0.9999080150203990547 ) ) ;
#50400 = ORIENTED_EDGE ( 'NONE', *, *, #48586, .F. ) ;
#50401 = ADVANCED_FACE ( 'NONE', ( #4526 ), #3558, .T. ) ;
#50402 = ORIENTED_EDGE ( 'NONE', *, *, #31797, .T. ) ;
#50403 = FACE_OUTER_BOUND ( 'NONE', #42949, .T. ) ;
#50404 = CARTESIAN_POINT ( 'NONE',  ( 0.3164563675027661227, 10.49799587805939183, -6.338687639235927485 ) ) ;
#50405 = CARTESIAN_POINT ( 'NONE',  ( -22.28073302975500880, 0.9342220484184898810, -3.572053042948128088 ) ) ;
#50406 = CARTESIAN_POINT ( 'NONE',  ( 18.68377751299183132, 2.160179296860150977, 11.81608574661026978 ) ) ;
#50407 = CARTESIAN_POINT ( 'NONE',  ( -22.27711653538342773, 1.465933162149084978, -3.377206745424994327 ) ) ;
#50408 = CARTESIAN_POINT ( 'NONE',  ( -11.08198513529404394, -5.470473237785703269, -10.68265194728579282 ) ) ;
#50409 = AXIS2_PLACEMENT_3D ( 'NONE', #61838, #36579, #56881 ) ;
#50410 = DIRECTION ( 'NONE',  ( 0.000000000000000000, 0.000000000000000000, 1.000000000000000000 ) ) ;
#50411 = EDGE_LOOP ( 'NONE', ( #61822, #41327, #45865, #42251 ) ) ;
#50412 = VERTEX_POINT ( 'NONE', #40391 ) ;
#50413 = LINE ( 'NONE', #522, #38126 ) ;
#50414 = CIRCLE ( 'NONE', #59953, 12.74999999999999822 ) ;
#50415 = CARTESIAN_POINT ( 'NONE',  ( 2.244591118396555451, 7.500068934084588967, -1.431619869711765469 ) ) ;
#50416 = CARTESIAN_POINT ( 'NONE',  ( 0.000000000000000000, 6.664893814313781029, -3.439359016433444438 ) ) ;
#50417 = CARTESIAN_POINT ( 'NONE',  ( -27.32343372485686572, -3.007804754713678808, -0.1402256980610577797 ) ) ;
#50418 = LINE ( 'NONE', #60708, #10920 ) ;
#50419 = AXIS2_PLACEMENT_3D ( 'NONE', #55384, #25790, #15137 ) ;
#50420 = LINE ( 'NONE', #56365, #63818 ) ;
#50421 = DIRECTION ( 'NONE',  ( 0.000000000000000000, 0.000000000000000000, 1.000000000000000000 ) ) ;
#50422 = CARTESIAN_POINT ( 'NONE',  ( 0.3665391374699465965, -12.13918562134717760, -1.872534962004925196 ) ) ;
#50423 = VERTEX_POINT ( 'NONE', #29437 ) ;
#50424 = VECTOR ( 'NONE', #20283, 1000.000000000000000 ) ;
#50425 = CARTESIAN_POINT ( 'NONE',  ( 35.00000000000000000, 7.499679039484058229, -9.040300684349723781 ) ) ;
#50426 = CARTESIAN_POINT ( 'NONE',  ( 17.70433014606954103, 10.91857155134370494, 7.947521937489286259 ) ) ;
#50427 = CARTESIAN_POINT ( 'NONE',  ( 35.00000000000000000, 10.92721691015455754, -4.309077947445693724 ) ) ;
#50428 = CIRCLE ( 'NONE', #30243, 12.18650000000000055 ) ;
#50429 = EDGE_CURVE ( 'NONE', #62374, #17087, #11230, .T. ) ;
#50430 = DIRECTION ( 'NONE',  ( -1.000000000000000000, 0.000000000000000000, 0.000000000000000000 ) ) ;
#50431 = CYLINDRICAL_SURFACE ( 'NONE', #8582, 4.999999999999999112 ) ;
#50432 = VERTEX_POINT ( 'NONE', #49738 ) ;
#50433 = CARTESIAN_POINT ( 'NONE',  ( 2.241506898688419458, 7.634383346098567280, -0.03933068055393580675 ) ) ;
#50434 = FACE_OUTER_BOUND ( 'NONE', #15764, .T. ) ;
#50435 = CARTESIAN_POINT ( 'NONE',  ( 17.33919137821584044, -28.58640580301184286, -8.960163943132222641 ) ) ;
#50436 = ORIENTED_EDGE ( 'NONE', *, *, #49, .F. ) ;
#50437 = DIRECTION ( 'NONE',  ( -1.000000000000000000, 0.000000000000000000, 0.000000000000000000 ) ) ;
#50439 = DIRECTION ( 'NONE',  ( -1.000000000000000000, 0.000000000000000000, 0.000000000000000000 ) ) ;
#50438 = B_SPLINE_CURVE_WITH_KNOTS ( 'NONE', 3,
 ( #21856, #52105, #12185, #7190, #52764, #62084, #594, #46452, #21175, #16537, #11524, #15844, #6561, #22160, #62713, #26829 ),
 .UNSPECIFIED., .F., .F.,
 ( 4, 3, 3, 3, 3, 4 ),
 ( 0.000000000000000000, 0.0002176109881720253523, 0.0004352086762394627266, 0.0006528017811446922784, 0.0007615147961451759632, 0.0009453342004947127772 ),
 .UNSPECIFIED. ) ;
#50440 = CARTESIAN_POINT ( 'NONE',  ( -35.00000000000000000, 3.827046518385245122, -11.56998259273173701 ) ) ;
#50442 = ORIENTED_EDGE ( 'NONE', *, *, #6322, .T. ) ;
#50441 = CARTESIAN_POINT ( 'NONE',  ( 0.3675815128205894289, 12.27743992903066150, 0.2638082659428850896 ) ) ;
#50443 = CARTESIAN_POINT ( 'NONE',  ( 37.00000000000000711, 10.91536515067648239, 4.339012074899986970 ) ) ;
#50444 = CIRCLE ( 'NONE', #9037, 12.18650000000000233 ) ;
#50445 = ADVANCED_FACE ( 'NONE', ( #3874 ), #4181, .T. ) ;
#50446 = CARTESIAN_POINT ( 'NONE',  ( 5.514624014163232779, -0.003668383633201386610, 0.001921576324372439642 ) ) ;
#50447 = ORIENTED_EDGE ( 'NONE', *, *, #53812, .F. ) ;
#50448 = DIRECTION ( 'NONE',  ( -1.000000000000000000, 0.000000000000000000, -0.000000000000000000 ) ) ;
#50449 = CARTESIAN_POINT ( 'NONE',  ( -27.10422407540546885, 1.306850885988335209, 1.954655484500537277 ) ) ;
#50450 = LINE ( 'NONE', #25481, #59825 ) ;
#50451 = CARTESIAN_POINT ( 'NONE',  ( 9.169146324975033124, 6.964048800780563653, -11.57111712795824587 ) ) ;
#50452 = CARTESIAN_POINT ( 'NONE',  ( -37.00000000000000711, -1.262958560998674429, -12.12087942037211086 ) ) ;
#50453 = EDGE_CURVE ( 'NONE', #18319, #14466, #39086, .T. ) ;
#50454 = DIRECTION ( 'NONE',  ( -1.000000000000000000, 0.000000000000000000, 0.000000000000000000 ) ) ;
#50455 = CARTESIAN_POINT ( 'NONE',  ( 2.257661810674664871, 1.193649218122989852, -7.546014018370192034 ) ) ;
#50456 = EDGE_CURVE ( 'NONE', #63705, #38749, #60044, .T. ) ;
#50457 =( GEOMETRIC_REPRESENTATION_CONTEXT ( 3 ) GLOBAL_UNCERTAINTY_ASSIGNED_CONTEXT ( ( #23639 ) ) GLOBAL_UNIT_ASSIGNED_CONTEXT ( ( #53809, #42157, #62445 ) ) REPRESENTATION_CONTEXT ( 'NONE', 'WORKASPACE' ) );
#50458 = ORIENTED_EDGE ( 'NONE', *, *, #9664, .F. ) ;
#50459 = CARTESIAN_POINT ( 'NONE',  ( -35.00000000000000000, -11.74614673114904129, -0.01609748574457297438 ) ) ;
#50460 = VERTEX_POINT ( 'NONE', #29754 ) ;
#50461 =( LENGTH_UNIT ( ) NAMED_UNIT ( * ) SI_UNIT ( .MILLI., .METRE. ) );
#50462 = CARTESIAN_POINT ( 'NONE',  ( 0.2706063244538003398, 11.44820198696415936, 4.353289770698253847 ) ) ;
#50463 = EDGE_CURVE ( 'NONE', #15694, #61226, #65155, .T. ) ;
#50464 = DIRECTION ( 'NONE',  ( 0.000000000000000000, 0.000000000000000000, 1.000000000000000000 ) ) ;
#50465 = VERTEX_POINT ( 'NONE', #10149 ) ;
#50466 = FACE_OUTER_BOUND ( 'NONE', #41683, .T. ) ;
#50467 = CIRCLE ( 'NONE', #3778, 4.999999999999999112 ) ;
#50468 = DIRECTION ( 'NONE',  ( -1.000000000000000000, 0.000000000000000000, 0.000000000000000000 ) ) ;
#50470 = ADVANCED_FACE ( 'NONE', ( #52032 ), #5511, .T. ) ;
#50469 = CARTESIAN_POINT ( 'NONE',  ( 24.19770493339638406, 1.945095382686029550, 13.36407410745160540 ) ) ;
#50471 = ORIENTED_EDGE ( 'NONE', *, *, #46318, .T. ) ;
#50472 = VERTEX_POINT ( 'NONE', #56351 ) ;
#50473 = CARTESIAN_POINT ( 'NONE',  ( 2.931247277082682068, 0.3703309885897901887, -7.855653518374113631 ) ) ;
#50474 = VERTEX_POINT ( 'NONE', #831 ) ;
#50475 = CARTESIAN_POINT ( 'NONE',  ( 5.514970785353741078, 0.001897634820904481583, -0.004324946436530190987 ) ) ;
#50476 = DIRECTION ( 'NONE',  ( -1.000000000000000000, 0.000000000000000000, 0.000000000000000000 ) ) ;
#50477 = CARTESIAN_POINT ( 'NONE',  ( -27.10128162969864363, 2.337214317750537340, -0.1566844438592116806 ) ) ;
#50478 = CIRCLE ( 'NONE', #38788, 5.000000000000000000 ) ;
#50479 = CARTESIAN_POINT ( 'NONE',  ( 2.259025283528087513, 7.131631878998428320, -2.741148848567693808 ) ) ;
#50480 = CARTESIAN_POINT ( 'NONE',  ( 2.000000000000001776, 5.457833520448724940, -4.281014542496488495 ) ) ;
#50481 = CARTESIAN_POINT ( 'NONE',  ( -35.00000000000000000, 0.000000000000000000, 0.000000000000000000 ) ) ;
#50482 = ADVANCED_FACE ( 'NONE', ( #10799 ), #31089, .T. ) ;
#50483 = CARTESIAN_POINT ( 'NONE',  ( 22.00000000000000711, -20.00000000000000000, 1.500000000000002887 ) ) ;
#50484 = ORIENTED_EDGE ( 'NONE', *, *, #57734, .F. ) ;
#50485 = CARTESIAN_POINT ( 'NONE',  ( 2.827825597296801607, -2.100863646776117033, 8.776379025186180627 ) ) ;
#50486 = EDGE_CURVE ( 'NONE', #2113, #38173, #5173, .T. ) ;
#50487 = CARTESIAN_POINT ( 'NONE',  ( 2.899286259009691502, 4.231523595108580338, -6.616268644969650836 ) ) ;
#50488 = CARTESIAN_POINT ( 'NONE',  ( -37.00000000000000711, -2.936739658819952581, 11.37311665002362560 ) ) ;
#50489 = LINE ( 'NONE', #19884, #25388 ) ;
#50490 = DIRECTION ( 'NONE',  ( 0.3628680629012471792, -0.9318405276259971171, 0.000000000000000000 ) ) ;
#50491 = CARTESIAN_POINT ( 'NONE',  ( 35.00000000000000000, 4.705694406421931860E-17, -3.469127814946512892E-15 ) ) ;
#50492 = FACE_OUTER_BOUND ( 'NONE', #28316, .T. ) ;
#50493 = CARTESIAN_POINT ( 'NONE',  ( -37.00000000000000711, 2.021542716731397071, 12.01765980939842748 ) ) ;
#50494 = CIRCLE ( 'NONE', #34563, 12.18649999999999878 ) ;
#50495 = ORIENTED_EDGE ( 'NONE', *, *, #49730, .T. ) ;
#50496 = DIRECTION ( 'NONE',  ( 1.000000000000000000, 0.000000000000000000, -0.000000000000000000 ) ) ;
#50497 =( BOUNDED_SURFACE ( )  B_SPLINE_SURFACE ( 3, 1, ( 
 ( #61764, #35814 ),
 ( #65748, #46802 ),
 ( #51157, #25881 ),
 ( #46474, #930 ) ),
 .UNSPECIFIED., .F., .F., .F. ) 
 B_SPLINE_SURFACE_WITH_KNOTS ( ( 4, 4 ),
 ( 2, 2 ),
 ( 0.000000000000000000, 1.000000000000000000 ),
 ( 0.000000000000000000, 1.000000000000000000 ),
 .UNSPECIFIED. ) 
 GEOMETRIC_REPRESENTATION_ITEM ( )  RATIONAL_B_SPLINE_SURFACE ( (
 ( 1.000000000000000000, 1.000000000000000000),
 ( 0.6933888150995267674, 0.9895912004443193632),
 ( 0.6933888150995267674, 0.9895912004443193632),
 ( 1.000000000000000000, 1.000000000000000000) ) ) 
 REPRESENTATION_ITEM ( '' )  SURFACE ( )  );
#50498 = ORIENTED_EDGE ( 'NONE', *, *, #23444, .F. ) ;
#50499 = CYLINDRICAL_SURFACE ( 'NONE', #22201, 12.74999999999999822 ) ;
#50500 = DIRECTION ( 'NONE',  ( 0.000000000000000000, 0.01356324068817992175, -0.9999080150203990547 ) ) ;
#50501 = CARTESIAN_POINT ( 'NONE',  ( -17.88545287150297014, 6.217808922599323829, -11.98485482592045237 ) ) ;
#50502 = CARTESIAN_POINT ( 'NONE',  ( 0.2650492433740064824, -12.04046084639674596, 2.234874822562856966 ) ) ;
#50503 = CARTESIAN_POINT ( 'NONE',  ( -37.00000000000000711, -9.321877890560388735, -7.146664589318012517 ) ) ;
#50504 = ORIENTED_EDGE ( 'NONE', *, *, #24947, .T. ) ;
#50505 = CARTESIAN_POINT ( 'NONE',  ( -35.04643116707788408, -0.01193867652720878580, 0.002453861112621663620 ) ) ;
#50506 = CARTESIAN_POINT ( 'NONE',  ( 2.259025283528085737, -3.701170455111014501, 6.683966451873017967 ) ) ;
#50507 = CARTESIAN_POINT ( 'NONE',  ( -37.00000000000000711, -5.273331777780412288, 10.49591321039678959 ) ) ;
#50508 = CARTESIAN_POINT ( 'NONE',  ( 36.00000000000000711, 12.02534193257720574, -4.237174932027271801 ) ) ;
#50509 = EDGE_CURVE ( 'NONE', #13166, #38215, #37371, .T. ) ;
#50510 = CARTESIAN_POINT ( 'NONE',  ( -17.56786360922926349, -5.609040142167114773, 10.61363638985786473 ) ) ;
#50511 = DIRECTION ( 'NONE',  ( 1.000000000000000000, 0.000000000000000000, 0.000000000000000000 ) ) ;
#50512 = AXIS2_PLACEMENT_3D ( 'NONE', #14479, #23506, #34757 ) ;
#50513 = ORIENTED_EDGE ( 'NONE', *, *, #3231, .T. ) ;
#50514 = CARTESIAN_POINT ( 'NONE',  ( -27.08429572838383947, -0.6096735944848084010, 2.208905845566022208 ) ) ;
#50515 = ORIENTED_EDGE ( 'NONE', *, *, #64602, .T. ) ;
#50516 = CARTESIAN_POINT ( 'NONE',  ( 35.00000000000000000, 4.705694406421931860E-17, -3.469127814946512892E-15 ) ) ;
#50517 = LINE ( 'NONE', #302, #54375 ) ;
#50518 = ADVANCED_FACE ( 'NONE', ( #15774 ), #36730, .T. ) ;
#50519 = CARTESIAN_POINT ( 'NONE',  ( 0.2648978790185619880, 11.46165506714233828, -4.312320170909121231 ) ) ;
#50520 = CARTESIAN_POINT ( 'NONE',  ( 0.3675815128205894289, 6.367184624550164429, 10.50067073900654080 ) ) ;
#50521 = AXIS2_PLACEMENT_3D ( 'NONE', #23299, #33273, #38592 ) ;
#50522 = EDGE_CURVE ( 'NONE', #37286, #5947, #9745, .T. ) ;
#50523 = ORIENTED_EDGE ( 'NONE', *, *, #40239, .F. ) ;
#50524 = VERTEX_POINT ( 'NONE', #31722 ) ;
#50525 = DIRECTION ( 'NONE',  ( -1.000000000000000000, 0.000000000000000000, 0.000000000000000000 ) ) ;
#50526 = ORIENTED_EDGE ( 'NONE', *, *, #2765, .F. ) ;
#50527 = CARTESIAN_POINT ( 'NONE',  ( 2.242819959140643693, -6.560218843829757951, -3.905785747113998063 ) ) ;
#50528 = CARTESIAN_POINT ( 'NONE',  ( 5.516018279890452902, -0.005752102158673865970, 0.003580555109620777322 ) ) ;
#50529 = CARTESIAN_POINT ( 'NONE',  ( 0.000000000000000000, 3.805198749487521681, -5.799611601383208637 ) ) ;
#50530 = CARTESIAN_POINT ( 'NONE',  ( -27.31123137524929234, 10.57279367158373162, -8.394978051634899074 ) ) ;
#50531 = FACE_OUTER_BOUND ( 'NONE', #54956, .T. ) ;
#50532 = CARTESIAN_POINT ( 'NONE',  ( -11.35685066047967062, -8.377133794443500037, 10.59944628267702527 ) ) ;
#50534 = CARTESIAN_POINT ( 'NONE',  ( 1.719304012339893051, -12.70777170743897422, -0.7661785589590540679 ) ) ;
#50533 = B_SPLINE_CURVE_WITH_KNOTS ( 'NONE', 3,
 ( #21384, #57295, #37663, #31999, #32334, #11399, #41661, #52322, #2434, #42621, #21733, #36675, #52953, #36991, #57961, #11717, #6762, #42971, #31672 ),
 .UNSPECIFIED., .F., .F.,
 ( 4, 3, 3, 3, 3, 3, 4 ),
 ( 7.884170296961029399E-18, 4.457896483014795814E-05, 6.639290541542046452E-05, 8.820687556478797845E-05, 0.0001100173248778924787, 0.0001545671401658121294, 0.0001830328308068605012 ),
 .UNSPECIFIED. ) ;
#50535 = VERTEX_POINT ( 'NONE', #61663 ) ;
#50536 = EDGE_CURVE ( 'NONE', #65336, #648, #57564, .T. ) ;
#50537 = CARTESIAN_POINT ( 'NONE',  ( -9.144366736240645110, -11.10870866445312544, -4.554380859875097443 ) ) ;
#50538 = ORIENTED_EDGE ( 'NONE', *, *, #26123, .F. ) ;
#50539 = CARTESIAN_POINT ( 'NONE',  ( 1.459561108994059442, -2.815016945601032106, -12.32692860927485334 ) ) ;
#50540 = DIRECTION ( 'NONE',  ( -1.000000000000000000, 0.000000000000000000, 0.000000000000000000 ) ) ;
#50541 = VERTEX_POINT ( 'NONE', #51400 ) ;
#50542 = DIRECTION ( 'NONE',  ( -1.000000000000000000, 0.000000000000000000, 0.000000000000000000 ) ) ;
#50543 = ORIENTED_EDGE ( 'NONE', *, *, #31216, .F. ) ;
#50544 = CARTESIAN_POINT ( 'NONE',  ( 37.00000000000000711, 5.391785509271111110, 10.43555801961468887 ) ) ;
#50545 = DIRECTION ( 'NONE',  ( -1.000000000000000000, 0.000000000000000000, 0.000000000000000000 ) ) ;
#50547 = EDGE_CURVE ( 'NONE', #42222, #19077, #39450, .T. ) ;
#50546 = DIRECTION ( 'NONE',  ( -1.000000000000000000, 0.000000000000000000, 0.000000000000000000 ) ) ;
#50548 = CARTESIAN_POINT ( 'NONE',  ( 2.969415267404470260, 7.260393470501825597, -3.055358878717542748 ) ) ;
#50549 = EDGE_LOOP ( 'NONE', ( #13443, #3094, #34715, #7770 ) ) ;
#50550 = ORIENTED_EDGE ( 'NONE', *, *, #62667, .F. ) ;
#50551 = CARTESIAN_POINT ( 'NONE',  ( 2.903928887688318916, 2.496183838365873431, -8.407112942776702624 ) ) ;
#50553 = ORIENTED_EDGE ( 'NONE', *, *, #59896, .F. ) ;
#50552 = EDGE_CURVE ( 'NONE', #65779, #61418, #21437, .T. ) ;
#50554 = DIRECTION ( 'NONE',  ( 0.000000000000000000, -0.01356324068817998940, 0.9999080150203990547 ) ) ;
#50555 = ORIENTED_EDGE ( 'NONE', *, *, #34446, .F. ) ;
#50556 = ORIENTED_EDGE ( 'NONE', *, *, #25110, .F. ) ;
#50558 = EDGE_CURVE ( 'NONE', #40917, #30330, #62814, .T. ) ;
#50557 = ORIENTED_EDGE ( 'NONE', *, *, #23742, .F. ) ;
#50559 = CARTESIAN_POINT ( 'NONE',  ( 2.717984159219029472, -5.783767685176845141, 5.223388265379668383 ) ) ;
#50560 = CARTESIAN_POINT ( 'NONE',  ( -7.856485614137364237, -26.39148214816155757, 14.61473980079826518 ) ) ;
#50561 = DIRECTION ( 'NONE',  ( -1.000000000000000000, 0.000000000000000000, 0.000000000000000000 ) ) ;
#50562 = DIRECTION ( 'NONE',  ( 0.000000000000000000, -0.01356324068817998940, 0.9999080150203990547 ) ) ;
#50563 = DIRECTION ( 'NONE',  ( -1.000000000000000000, 0.000000000000000000, 0.000000000000000000 ) ) ;
#50564 = ORIENTED_EDGE ( 'NONE', *, *, #33348, .F. ) ;
#50565 = CIRCLE ( 'NONE', #3862, 4.999999999999999112 ) ;
#50566 = EDGE_CURVE ( 'NONE', #38541, #25992, #5849, .T. ) ;
#50567 = ADVANCED_FACE ( 'NONE', ( #31417 ), #51717, .T. ) ;
#50568 = CARTESIAN_POINT ( 'NONE',  ( 2.247206125382658293, -2.502718378779159814, -7.214589497757414094 ) ) ;
#50569 = AXIS2_PLACEMENT_3D ( 'NONE', #19758, #21036, #5116 ) ;
#50570 = ORIENTED_EDGE ( 'NONE', *, *, #17127, .F. ) ;
#50571 = CARTESIAN_POINT ( 'NONE',  ( -17.19065538327509657, 2.658487034042159802, 13.23633903133955414 ) ) ;
#50572 = CARTESIAN_POINT ( 'NONE',  ( -27.08485414902838784, 0.5952588087544679052, 2.214586389210142059 ) ) ;
#50573 = EDGE_CURVE ( 'NONE', #19083, #11411, #7627, .T. ) ;
#50574 = ORIENTED_EDGE ( 'NONE', *, *, #24260, .F. ) ;
#50575 = CARTESIAN_POINT ( 'NONE',  ( 35.00000000000000000, 8.366449238204499039, 9.621072037176897851 ) ) ;
#50576 = CARTESIAN_POINT ( 'NONE',  ( 28.91776584869966626, 9.508282570375039100, 7.334618107890905847 ) ) ;
#50577 = FACE_OUTER_BOUND ( 'NONE', #40507, .T. ) ;
#50578 = CIRCLE ( 'NONE', #6993, 4.999999999999999112 ) ;
#50579 = ORIENTED_EDGE ( 'NONE', *, *, #4540, .F. ) ;
#50580 = CARTESIAN_POINT ( 'NONE',  ( 1.633930747250945670, 6.963441708413322218, 10.62371422070954274 ) ) ;
#50581 = EDGE_LOOP ( 'NONE', ( #3100, #45369, #11094, #55632, #19656, #2946 ) ) ;
#50582 = DIRECTION ( 'NONE',  ( -1.000000000000000000, 0.000000000000000000, 0.000000000000000000 ) ) ;
#50583 = CARTESIAN_POINT ( 'NONE',  ( -37.00000000000000711, 9.677500615117999416, -6.657191900728212985 ) ) ;
#50584 = DIRECTION ( 'NONE',  ( 0.000000000000000000, -0.01356324068817998940, 0.9999080150203990547 ) ) ;
#50585 = DIRECTION ( 'NONE',  ( -1.000000000000000000, 0.000000000000000000, 0.000000000000000000 ) ) ;
#50586 = CARTESIAN_POINT ( 'NONE',  ( 2.241451721903216399, 7.507681056655377105, 1.385577012535781138 ) ) ;
#50587 = ORIENTED_EDGE ( 'NONE', *, *, #28819, .F. ) ;
#50588 = CARTESIAN_POINT ( 'NONE',  ( 35.00000000000000000, 4.705694406421931860E-17, -3.469127814946512892E-15 ) ) ;
#50589 = CARTESIAN_POINT ( 'NONE',  ( 0.9232167919969084258, 5.871274944231854143, -10.99620217063209893 ) ) ;
#50590 = DIRECTION ( 'NONE',  ( 0.000000000000000000, 0.3554799084908970563, 0.9346839223284539866 ) ) ;
#50591 = CARTESIAN_POINT ( 'NONE',  ( 2.994568964204204153, 3.591541975631971528, 7.020079750321906786 ) ) ;
#50592 = ADVANCED_FACE ( 'NONE', ( #42343 ), #42674, .T. ) ;
#50593 = CARTESIAN_POINT ( 'NONE',  ( -2.534465382079153173, -26.62629929685681063, -16.11622222973024421 ) ) ;
#50594 = LINE ( 'NONE', #54908, #2010 ) ;
#50595 = CARTESIAN_POINT ( 'NONE',  ( -36.00000000000000711, -6.265926637539413591, -11.10408318471066380 ) ) ;
#50596 = CARTESIAN_POINT ( 'NONE',  ( 35.00000000000000000, 4.705694406421931860E-17, -3.469127814946512892E-15 ) ) ;
#50597 = CARTESIAN_POINT ( 'NONE',  ( 2.258463476536644698, 0.1358786215989210844, -7.638896687393369689 ) ) ;
#50598 = EDGE_CURVE ( 'NONE', #52926, #38497, #27397, .T. ) ;
#50599 = CIRCLE ( 'NONE', #28280, 2.899999999999995026 ) ;
#50600 = VERTEX_POINT ( 'NONE', #43675 ) ;
#50601 = AXIS2_PLACEMENT_3D ( 'NONE', #28019, #33963, #54615 ) ;
#50602 = VERTEX_POINT ( 'NONE', #17443 ) ;
#50603 = DIRECTION ( 'NONE',  ( 0.000000000000000000, 0.01356324068818000848, -0.9999080150203990547 ) ) ;
#50604 = CARTESIAN_POINT ( 'NONE',  ( 35.00000000000000000, 11.16627499335655216, 3.645068577060061266 ) ) ;
#50605 = DIRECTION ( 'NONE',  ( 1.000000000000000000, -0.000000000000000000, -0.000000000000000000 ) ) ;
#50606 = CARTESIAN_POINT ( 'NONE',  ( 2.241352910868909643, 5.794346703933845433, 4.970878533273779709 ) ) ;
#50607 = VERTEX_POINT ( 'NONE', #32055 ) ;
#50608 = EDGE_CURVE ( 'NONE', #23216, #29886, #53287, .T. ) ;
#50609 = ORIENTED_EDGE ( 'NONE', *, *, #17032, .F. ) ;
#50610 = VERTEX_POINT ( 'NONE', #62979 ) ;
#50611 = B_SPLINE_CURVE_WITH_KNOTS ( 'NONE', 3,
 ( #24764, #19783, #40039, #45361, #15099, #40706, #35376, #25409, #25749, #14753, #45689, #492, #35030, #55345, #31057, #9783, #5820, #55684, #10121, #21065, #30399, #60998 ),
 .UNSPECIFIED., .F., .F.,
 ( 4, 2, 2, 2, 2, 2, 2, 2, 2, 2, 4 ),
 ( 0.000000000000000000, 0.001195189350898897109, 0.002390378701797794218, 0.003585568052696691543, 0.004780757403595588435, 0.005378352079045037315, 0.005975946754494486195, 0.006573541429943933340, 0.007171136105393381352, 0.008366325456292272172, 0.009561514807191164728 ),
 .UNSPECIFIED. ) ;
#50612 = CARTESIAN_POINT ( 'NONE',  ( 29.45729197154192747, -9.438926003476494131, 7.413919495756846167 ) ) ;
#50613 = CYLINDRICAL_SURFACE ( 'NONE', #55479, 12.75000000000000178 ) ;
#50614 = ORIENTED_EDGE ( 'NONE', *, *, #6621, .F. ) ;
#50615 = CARTESIAN_POINT ( 'NONE',  ( -37.00000000000000711, 12.46157735505193109, -2.696588552978925524 ) ) ;
#50616 = DIRECTION ( 'NONE',  ( -1.000000000000000000, -0.000000000000000000, 0.000000000000000000 ) ) ;
#50617 = DIRECTION ( 'NONE',  ( 0.000000000000000000, 0.3193015301359742875, 0.9476531711828043436 ) ) ;
#50618 = ORIENTED_EDGE ( 'NONE', *, *, #41903, .F. ) ;
#50619 = CARTESIAN_POINT ( 'NONE',  ( -22.28350523959500862, 0.3047406164877414225, 3.687952016964565871 ) ) ;
#50620 = CARTESIAN_POINT ( 'NONE',  ( 5.268658153348980910, -26.87458176590483916, -15.73590792199858868 ) ) ;
#50621 = CARTESIAN_POINT ( 'NONE',  ( 37.00000000000000711, 4.705694406421931860E-17, -3.469127814946512892E-15 ) ) ;
#50623 = ORIENTED_EDGE ( 'NONE', *, *, #64261, .F. ) ;
#50622 = CARTESIAN_POINT ( 'NONE',  ( -27.08935880048797529, 1.653090150968474781, 1.608762129669635721 ) ) ;
#50624 = CARTESIAN_POINT ( 'NONE',  ( 0.000000000000000000, -1.865193240757054394, -6.552473556515217012 ) ) ;
#50625 = ORIENTED_EDGE ( 'NONE', *, *, #39669, .T. ) ;
#50626 = DIRECTION ( 'NONE',  ( 0.000000000000000000, 0.01356324068817998940, -0.9999080150203990547 ) ) ;
#50627 = ORIENTED_EDGE ( 'NONE', *, *, #55231, .F. ) ;
#50628 = CARTESIAN_POINT ( 'NONE',  ( 35.00000000000000000, -10.99909370905160699, -5.246972444133983338 ) ) ;
#50629 = ADVANCED_FACE ( 'NONE', ( #37044 ), #7793, .T. ) ;
#50630 = CYLINDRICAL_SURFACE ( 'NONE', #3313, 12.18650000000000055 ) ;
#50631 = EDGE_CURVE ( 'NONE', #18668, #39229, #12936, .T. ) ;
#50632 = DIRECTION ( 'NONE',  ( 0.000000000000000000, 0.000000000000000000, 1.000000000000000000 ) ) ;
#50633 = DIRECTION ( 'NONE',  ( -1.000000000000000000, 0.000000000000000000, 0.000000000000000000 ) ) ;
#50634 = FACE_OUTER_BOUND ( 'NONE', #30168, .T. ) ;
#50635 = DIRECTION ( 'NONE',  ( 1.000000000000000000, 0.000000000000000000, -0.000000000000000000 ) ) ;
#50636 = CARTESIAN_POINT ( 'NONE',  ( 11.38817443037663679, 0.2421923074375172957, 11.99781792006712955 ) ) ;
#50637 = CARTESIAN_POINT ( 'NONE',  ( -27.08419797710328325, 2.268561579780429494, -0.3221715127607987506 ) ) ;
#50638 = CARTESIAN_POINT ( 'NONE',  ( 0.2956976708475448357, -3.984495122852500959, -11.59055635407405482 ) ) ;
#50640 = ORIENTED_EDGE ( 'NONE', *, *, #62040, .T. ) ;
#50639 = CARTESIAN_POINT ( 'NONE',  ( 5.736444914132059480, -9.902886448537387309, 9.181108836895850445 ) ) ;
#50641 = EDGE_CURVE ( 'NONE', #50142, #22284, #18272, .T. ) ;
#50642 = DIRECTION ( 'NONE',  ( 0.000000000000000000, -0.07632122047557186872, 0.9970832820307033995 ) ) ;
#50643 = ORIENTED_EDGE ( 'NONE', *, *, #45001, .T. ) ;
#50644 = LINE ( 'NONE', #55633, #63558 ) ;
#50645 = ORIENTED_EDGE ( 'NONE', *, *, #25800, .F. ) ;
#50646 = B_SPLINE_CURVE_WITH_KNOTS ( 'NONE', 3,
 ( #11195, #17500, #16178, #16827, #51770, #26812, #41427, #61720, #6212, #1225 ),
 .UNSPECIFIED., .F., .F.,
 ( 4, 2, 2, 2, 4 ),
 ( 4.336808689942017736E-19, 0.0006730921559986501133, 0.001346184311997299793, 0.002019276467995947087, 0.002692368623994594382 ),
 .UNSPECIFIED. ) ;
#50647 = EDGE_CURVE ( 'NONE', #33925, #16732, #26750, .T. ) ;
#50648 = ORIENTED_EDGE ( 'NONE', *, *, #61380, .F. ) ;
#50649 = CARTESIAN_POINT ( 'NONE',  ( 0.2958664285830411300, 8.045892866065361915, 9.245659426743914722 ) ) ;
#50650 = CARTESIAN_POINT ( 'NONE',  ( -27.08418322526031119, 0.3452258100746978253, 2.265123059255399696 ) ) ;
#50651 = CARTESIAN_POINT ( 'NONE',  ( 37.00000000000000711, 4.705694406421931860E-17, -3.469127814946512892E-15 ) ) ;
#50652 = CIRCLE ( 'NONE', #21962, 5.000000000000000000 ) ;
#50653 = DIRECTION ( 'NONE',  ( 1.000000000000000000, -0.000000000000000000, -0.000000000000000000 ) ) ;
#50654 = FACE_OUTER_BOUND ( 'NONE', #25221, .T. ) ;
#50655 = CIRCLE ( 'NONE', #14533, 7.938172270156617749 ) ;
#50656 = CARTESIAN_POINT ( 'NONE',  ( 2.000000000000001776, 0.3246585432986198727, 6.805031400696091914 ) ) ;
#50657 = ORIENTED_EDGE ( 'NONE', *, *, #12887, .F. ) ;
#50658 = CARTESIAN_POINT ( 'NONE',  ( 2.844750968615211484, 0.3326424433129591685, 7.828506085988378160 ) ) ;
#50659 = DIRECTION ( 'NONE',  ( 0.8867529933577789070, 0.000000000000000000, -0.4622435816439414147 ) ) ;
#50660 = CARTESIAN_POINT ( 'NONE',  ( 1.719304012338239485, 12.38166659046522788, 2.961219984258211202 ) ) ;
#50661 = ORIENTED_EDGE ( 'NONE', *, *, #46263, .F. ) ;
#50662 = CARTESIAN_POINT ( 'NONE',  ( 0.3057689695767506488, -4.409323295154131905, -11.43929056598610217 ) ) ;
#50663 = ADVANCED_FACE ( 'NONE', ( #53006 ), #3726, .F. ) ;
#50664 = EDGE_CURVE ( 'NONE', #21253, #37151, #1822, .T. ) ;
#50665 = CARTESIAN_POINT ( 'NONE',  ( 28.29050403390680302, -3.446535021889316930, 24.79622249374515519 ) ) ;
#50666 = CARTESIAN_POINT ( 'NONE',  ( -22.51237073810381517, 2.395115314842884757, 3.719289647955732914 ) ) ;
#50667 = CARTESIAN_POINT ( 'NONE',  ( -40.23304019309010471, -1.796181362175412133, -19.88949158386754235 ) ) ;
#50668 = ORIENTED_EDGE ( 'NONE', *, *, #12029, .F. ) ;
#50669 = DIRECTION ( 'NONE',  ( -1.000000000000000000, 0.000000000000000000, 0.000000000000000000 ) ) ;
#50670 = CARTESIAN_POINT ( 'NONE',  ( 1.836544102203957696, -30.58412608844328417, 15.25442441212345557 ) ) ;
#50671 = DIRECTION ( 'NONE',  ( -1.000000000000000000, 0.000000000000000000, 0.000000000000000000 ) ) ;
#50672 = EDGE_CURVE ( 'NONE', #52930, #40729, #6589, .T. ) ;
#50673 = DIRECTION ( 'NONE',  ( -1.000000000000000000, 0.000000000000000000, 0.000000000000000000 ) ) ;
#50674 = DIRECTION ( 'NONE',  ( -0.3939253465568944290, -0.9190910618577645685, 0.009718094113430031031 ) ) ;
#50675 = ORIENTED_EDGE ( 'NONE', *, *, #55953, .F. ) ;
#50676 = AXIS2_PLACEMENT_3D ( 'NONE', #54667, #35325, #10074 ) ;
#50677 = CARTESIAN_POINT ( 'NONE',  ( -35.00000000000000000, 12.18359334611896472, 0.2661492558803780772 ) ) ;
#50678 = CARTESIAN_POINT ( 'NONE',  ( 3.441679217059768980, 6.045329562784094612, -10.36821124058885424 ) ) ;
#50679 = ORIENTED_EDGE ( 'NONE', *, *, #16143, .T. ) ;
#50680 = CARTESIAN_POINT ( 'NONE',  ( 11.92331831525852159, 0.08325394350958797984, 13.49997450358961792 ) ) ;
#50681 = DIRECTION ( 'NONE',  ( 0.000000000000000000, 1.000000000000000000, 0.000000000000000000 ) ) ;
#50682 = ORIENTED_EDGE ( 'NONE', *, *, #12080, .T. ) ;
#50683 = EDGE_CURVE ( 'NONE', #22894, #4994, #48373, .T. ) ;
#50684 = EDGE_CURVE ( 'NONE', #48941, #53899, #52252, .T. ) ;
#50685 = ORIENTED_EDGE ( 'NONE', *, *, #42349, .T. ) ;
#50686 = AXIS2_PLACEMENT_3D ( 'NONE', #32855, #12922, #58839 ) ;
#50687 = ORIENTED_EDGE ( 'NONE', *, *, #31911, .F. ) ;
#50688 = EDGE_CURVE ( 'NONE', #37930, #10044, #60730, .T. ) ;
#50689 = CIRCLE ( 'NONE', #10328, 2.899999999999995026 ) ;
#50690 = ORIENTED_EDGE ( 'NONE', *, *, #60475, .F. ) ;
#50691 = CARTESIAN_POINT ( 'NONE',  ( 37.00000000000000711, 12.16893194857555116, 3.805206332242343059 ) ) ;
#50692 = FACE_OUTER_BOUND ( 'NONE', #37690, .T. ) ;
#50693 = DIRECTION ( 'NONE',  ( -1.000000000000000000, -0.000000000000000000, -0.000000000000000000 ) ) ;
#50694 = CARTESIAN_POINT ( 'NONE',  ( 2.000000000000001776, 0.000000000000000000, 0.000000000000000000 ) ) ;
#50695 =( BOUNDED_SURFACE ( )  B_SPLINE_SURFACE ( 3, 1, ( 
 ( #32433, #52744 ),
 ( #28124, #19119 ),
 ( #24112, #23455 ),
 ( #49080, #17813 ) ),
 .UNSPECIFIED., .F., .F., .F. ) 
 B_SPLINE_SURFACE_WITH_KNOTS ( ( 4, 4 ),
 ( 2, 2 ),
 ( 0.000000000000000000, 1.000000000000000000 ),
 ( 0.000000000000000000, 1.000000000000000000 ),
 .UNSPECIFIED. ) 
 GEOMETRIC_REPRESENTATION_ITEM ( )  RATIONAL_B_SPLINE_SURFACE ( (
 ( 1.000000000000000000, 1.000000000000000000),
 ( 0.8716676215708681896, 0.8964445200148164483),
 ( 0.8716676215708681896, 0.8964445200148164483),
 ( 1.000000000000000000, 1.000000000000000000) ) ) 
 REPRESENTATION_ITEM ( '' )  SURFACE ( )  );
#50696 = CARTESIAN_POINT ( 'NONE',  ( -12.58062741647496274, -29.25281707778071549, 4.759732266940784662 ) ) ;
#50697 = CARTESIAN_POINT ( 'NONE',  ( 35.00000000000000000, 4.705694406421931860E-17, -3.469127814946512892E-15 ) ) ;
#50699 = VERTEX_POINT ( 'NONE', #22765 ) ;
#50698 = CARTESIAN_POINT ( 'NONE',  ( 0.2652384770603659070, -12.04846497255941173, -2.191555293694098516 ) ) ;
#50700 = CARTESIAN_POINT ( 'NONE',  ( 35.00000000000000000, 4.705694406421931860E-17, -3.469127814946512892E-15 ) ) ;
#50701 = ORIENTED_EDGE ( 'NONE', *, *, #37692, .T. ) ;
#50702 = CARTESIAN_POINT ( 'NONE',  ( -10.00000000000000178, 0.000000000000000000, 0.000000000000000000 ) ) ;
#50703 = ORIENTED_EDGE ( 'NONE', *, *, #50664, .F. ) ;
#50704 = ORIENTED_EDGE ( 'NONE', *, *, #6976, .T. ) ;
#50705 = CARTESIAN_POINT ( 'NONE',  ( 0.2833330754217478487, 9.514385791198202824, -7.719627479384551627 ) ) ;
#50706 = CARTESIAN_POINT ( 'NONE',  ( 6.272189122741911760, -31.23296902231887273, 14.43357722546982380 ) ) ;
#50707 = EDGE_CURVE ( 'NONE', #28767, #28152, #40554, .T. ) ;
#50708 = CARTESIAN_POINT ( 'NONE',  ( 47.00000000000000711, 4.705694406421931860E-17, -3.469127814946512892E-15 ) ) ;
#50709 = DIRECTION ( 'NONE',  ( 0.000000000000000000, 0.000000000000000000, -1.000000000000000000 ) ) ;
#50710 = DIRECTION ( 'NONE',  ( 0.000000000000000000, 0.000000000000000000, 1.000000000000000000 ) ) ;
#50711 = CARTESIAN_POINT ( 'NONE',  ( 5.516018279890452902, 0.001397286410094317416, -0.006629829924290979969 ) ) ;
#50712 = ORIENTED_EDGE ( 'NONE', *, *, #2939, .F. ) ;
#50713 = EDGE_CURVE ( 'NONE', #38649, #26297, #17609, .T. ) ;
#50714 = VERTEX_POINT ( 'NONE', #23750 ) ;
#50715 = DIRECTION ( 'NONE',  ( -1.000000000000000000, 0.000000000000000000, 0.000000000000000000 ) ) ;
#50716 = ORIENTED_EDGE ( 'NONE', *, *, #44767, .T. ) ;
#50717 = VERTEX_POINT ( 'NONE', #30022 ) ;
#50718 = DIRECTION ( 'NONE',  ( -1.000000000000000000, -1.836970198721029688E-16, 0.000000000000000000 ) ) ;
#50719 = CYLINDRICAL_SURFACE ( 'NONE', #41615, 12.18649999999999878 ) ;
#50720 = DIRECTION ( 'NONE',  ( -1.000000000000000000, 0.000000000000000000, 0.000000000000000000 ) ) ;
#50721 = CARTESIAN_POINT ( 'NONE',  ( 0.5547464869798217624, -12.09851097165511291, 2.442933571354931388 ) ) ;
#50722 = CARTESIAN_POINT ( 'NONE',  ( -22.27718150314433387, 1.117371044661096713, -3.507884203786629129 ) ) ;
#50723 = CIRCLE ( 'NONE', #40064, 12.75000000000000178 ) ;
#50724 = CARTESIAN_POINT ( 'NONE',  ( 35.00000000000000000, 8.551552972817191289, 8.052525312709789773 ) ) ;
#50725 = CARTESIAN_POINT ( 'NONE',  ( -35.00000000000000000, 12.01765980939845058, -2.021542716731266065 ) ) ;
#50727 = ORIENTED_EDGE ( 'NONE', *, *, #2098, .F. ) ;
#50726 = VECTOR ( 'NONE', #13266, 1000.000000000000000 ) ;
#50728 = VERTEX_POINT ( 'NONE', #64933 ) ;
#50729 = DIRECTION ( 'NONE',  ( -1.000000000000000000, -0.000000000000000000, -0.000000000000000000 ) ) ;
#50730 = CARTESIAN_POINT ( 'NONE',  ( 2.269879328256729778, 7.500604381673476873, -1.473193649116055992 ) ) ;
#50731 = AXIS2_PLACEMENT_3D ( 'NONE', #42759, #6228, #26490 ) ;
#50732 = DIRECTION ( 'NONE',  ( 0.3865475372811021937, -0.3335716741247308215, 0.8598319252293086246 ) ) ;
#50733 = CARTESIAN_POINT ( 'NONE',  ( 6.433569295279546907, -8.070817871543312094, 8.888545806055137888 ) ) ;
#50734 = DIRECTION ( 'NONE',  ( 1.000000000000000000, 0.000000000000000000, 0.000000000000000000 ) ) ;
#50735 = CIRCLE ( 'NONE', #1893, 4.999999999999999112 ) ;
#50736 = EDGE_CURVE ( 'NONE', #50472, #11758, #62856, .T. ) ;
#50737 = CARTESIAN_POINT ( 'NONE',  ( 0.2646305136544065406, -9.296005949277169833, -7.972778379581646924 ) ) ;
#50738 = CARTESIAN_POINT ( 'NONE',  ( 1.287602823388301010, 2.727479899221430859, -12.28793447239746506 ) ) ;
#50739 = DIRECTION ( 'NONE',  ( -1.000000000000000000, 0.000000000000000000, 0.000000000000000000 ) ) ;
#50740 = ORIENTED_EDGE ( 'NONE', *, *, #47652, .T. ) ;
#50741 = CARTESIAN_POINT ( 'NONE',  ( 3.152665057734121756, -0.4801242025592447060, 7.923639299008720549 ) ) ;
#50742 = CARTESIAN_POINT ( 'NONE',  ( 17.48655162378398131, 11.52771039025705591, 7.062232779588992315 ) ) ;
#50743 = CARTESIAN_POINT ( 'NONE',  ( 0.000000000000000000, 6.796153407501467569, -1.388283512725773772 ) ) ;
#50744 = EDGE_CURVE ( 'NONE', #59777, #39315, #19411, .T. ) ;
#50745 = CARTESIAN_POINT ( 'NONE',  ( 5.514624014163232779, 0.003830004412313247914, 0.001574979445068904913 ) ) ;
#50746 = CARTESIAN_POINT ( 'NONE',  ( 3.152665057736111720, -7.281573230473792790, 3.161213418915395312 ) ) ;
#50747 = EDGE_LOOP ( 'NONE', ( #42558, #41919, #63375, #37884 ) ) ;
#50748 = CARTESIAN_POINT ( 'NONE',  ( 2.241536586108912488, -3.822683724643419545, -6.608496983003830927 ) ) ;
#50749 = CARTESIAN_POINT ( 'NONE',  ( 26.34661844826604593, 13.08594712317291986, 3.317828791472332117 ) ) ;
#50750 = CARTESIAN_POINT ( 'NONE',  ( 12.59130566666910944, -33.86016745060436506, -10.02644098062840960 ) ) ;
#50751 = EDGE_LOOP ( 'NONE', ( #53606, #21922, #3772, #32117 ) ) ;
#50752 = CARTESIAN_POINT ( 'NONE',  ( 0.000000000000000000, -6.201547234536999298, -2.820401998297984214 ) ) ;
#50753 = CARTESIAN_POINT ( 'NONE',  ( 0.2646305136544065406, -12.24595685781654275, -0.1321451301299126913 ) ) ;
#50754 = CARTESIAN_POINT ( 'NONE',  ( -22.28284753389937123, -0.9912969289936532924, -3.563226652211067602 ) ) ;
#50756 = VERTEX_POINT ( 'NONE', #24720 ) ;
#50755 = CARTESIAN_POINT ( 'NONE',  ( -37.00000000000000711, 11.60979404548639948, -3.704519465651187282 ) ) ;
#50757 = CARTESIAN_POINT ( 'NONE',  ( -27.09569413923794556, 2.259195818742697703, 0.5521997980586177412 ) ) ;
#50758 = AXIS2_PLACEMENT_3D ( 'NONE', #15922, #36557, #46860 ) ;
#50759 = CARTESIAN_POINT ( 'NONE',  ( 37.00000000000000711, 3.805206332242470957, -12.16893194857551563 ) ) ;
#50760 = ORIENTED_EDGE ( 'NONE', *, *, #35602, .T. ) ;
#50761 = DIRECTION ( 'NONE',  ( -1.000000000000000000, 0.000000000000000000, 0.000000000000000000 ) ) ;
#50762 = CARTESIAN_POINT ( 'NONE',  ( -27.09483304420744787, 1.303111346475875010, 1.923212037694846055 ) ) ;
#50763 = CIRCLE ( 'NONE', #8286, 12.18649999999999878 ) ;
#50764 = CARTESIAN_POINT ( 'NONE',  ( -18.58686583997247155, 5.151216734910867068, -12.47858029384659417 ) ) ;
#50765 = DIRECTION ( 'NONE',  ( 0.000000000000000000, 0.01356324068817998940, -0.9999080150203990547 ) ) ;
#50766 = DIRECTION ( 'NONE',  ( -1.000000000000000000, 0.000000000000000000, -0.000000000000000000 ) ) ;
#50767 = DIRECTION ( 'NONE',  ( 0.000000000000000000, 0.01356324068817998940, -0.9999080150203990547 ) ) ;
#50768 = CARTESIAN_POINT ( 'NONE',  ( 37.00000000000000711, 4.705694406421931860E-17, -3.469127814946512892E-15 ) ) ;
#50769 = AXIS2_PLACEMENT_3D ( 'NONE', #13091, #33372, #53672 ) ;
#50770 = ORIENTED_EDGE ( 'NONE', *, *, #5097, .T. ) ;
#50771 = CARTESIAN_POINT ( 'NONE',  ( 2.242819959140645913, -4.985618132689713988, 5.782321801516522086 ) ) ;
#50772 = VERTEX_POINT ( 'NONE', #49986 ) ;
#50773 = AXIS2_PLACEMENT_3D ( 'NONE', #30357, #50653, #90 ) ;
#50774 = DIRECTION ( 'NONE',  ( 0.000000000000000000, 0.000000000000000000, 1.000000000000000000 ) ) ;
#50775 = DIRECTION ( 'NONE',  ( -1.000000000000000000, 0.000000000000000000, 0.000000000000000000 ) ) ;
#50776 = DIRECTION ( 'NONE',  ( 0.000000000000000000, 0.000000000000000000, -1.000000000000000000 ) ) ;
#50777 = CARTESIAN_POINT ( 'NONE',  ( 5.536195898058073439, -0.006344799443923986905, 0.005656495196971059354 ) ) ;
#50778 = ORIENTED_EDGE ( 'NONE', *, *, #19410, .T. ) ;
#50779 = DIRECTION ( 'NONE',  ( 0.000000000000000000, -0.9467777615094536969, -0.3218879778916073908 ) ) ;
#50780 = CARTESIAN_POINT ( 'NONE',  ( 12.83590194764781778, 10.34016517225328080, -6.102282133837778844 ) ) ;
#50781 = FACE_BOUND ( 'NONE', #10719, .T. ) ;
#50782 = ORIENTED_EDGE ( 'NONE', *, *, #58004, .T. ) ;
#50783 = EDGE_LOOP ( 'NONE', ( #39208, #26086, #5176, #4634 ) ) ;
#50784 = DIRECTION ( 'NONE',  ( 0.000000000000000000, -0.8515178078024813191, 0.5243256840888652626 ) ) ;
#50785 = ORIENTED_EDGE ( 'NONE', *, *, #59116, .F. ) ;
#50786 = CARTESIAN_POINT ( 'NONE',  ( 0.2646305136544065406, 2.256625640822316647, 12.03696649559615217 ) ) ;
#50787 = CARTESIAN_POINT ( 'NONE',  ( -27.10113028276028402, 0.5479825692853955710, -2.276991616286355935 ) ) ;
#50788 = CARTESIAN_POINT ( 'NONE',  ( -37.00000000000000711, -10.12742074351902311, 7.745827850122975811 ) ) ;
#50789 = CARTESIAN_POINT ( 'NONE',  ( -35.00000000000000000, -11.38112321385052716, 2.905556151562584954 ) ) ;
#50790 = ADVANCED_FACE ( 'NONE', ( #28712 ), #50338, .T. ) ;
#50791 = DIRECTION ( 'NONE',  ( 0.000000000000000000, 0.9985334138511240409, -0.05413890858541454271 ) ) ;
#50792 = CARTESIAN_POINT ( 'NONE',  ( 6.361445718264521432, -4.355102044641763648, -12.77822703589027320 ) ) ;
#50793 = LINE ( 'NONE', #39828, #43971 ) ;
#50794 = ORIENTED_EDGE ( 'NONE', *, *, #30635, .T. ) ;
#50795 = CARTESIAN_POINT ( 'NONE',  ( 2.258463476536646031, -1.460294809170993968, 7.499249607179734767 ) ) ;
#50796 = VECTOR ( 'NONE', #60040, 1000.000000000000000 ) ;
#50797 = CARTESIAN_POINT ( 'NONE',  ( 2.000000000000001776, -3.224464355699868889, 6.771471746881965181 ) ) ;
#50798 = CARTESIAN_POINT ( 'NONE',  ( 35.00000000000000000, 11.54110654723649176, -2.185196060783925809 ) ) ;
#50799 = CARTESIAN_POINT ( 'NONE',  ( 12.84739494846498786, 12.07655647595275994, -6.046275926700755754 ) ) ;
#50800 = FACE_OUTER_BOUND ( 'NONE', #5889, .T. ) ;
#50801 = DIRECTION ( 'NONE',  ( 0.000000000000000000, -0.4198891015602715382, 0.9075754196709537869 ) ) ;
#50802 = DIRECTION ( 'NONE',  ( 1.000000000000000000, -0.000000000000000000, 0.000000000000000000 ) ) ;
#50803 = DIRECTION ( 'NONE',  ( 0.000000000000000000, 0.5767582926624970074, 0.8169148498130275327 ) ) ;
#50804 = CIRCLE ( 'NONE', #39111, 5.000000000000001776 ) ;
#50805 = ADVANCED_FACE ( 'NONE', ( #33702 ), #59004, .T. ) ;
#50806 = ORIENTED_EDGE ( 'NONE', *, *, #21254, .F. ) ;
#50807 = CARTESIAN_POINT ( 'NONE',  ( 35.00000000000000000, -11.47561260193572963, 5.556331110570524423 ) ) ;
#50808 = CIRCLE ( 'NONE', #33794, 12.18650000000000055 ) ;
#50809 = VECTOR ( 'NONE', #4502, 1000.000000000000000 ) ;
#50810 = EDGE_CURVE ( 'NONE', #43258, #30430, #3482, .T. ) ;
#50811 = ORIENTED_EDGE ( 'NONE', *, *, #38722, .T. ) ;
#50812 = EDGE_CURVE ( 'NONE', #59321, #35137, #46915, .T. ) ;
#50813 = CARTESIAN_POINT ( 'NONE',  ( 37.00000000000000711, -1.738225594540086405, -12.63095688309028652 ) ) ;
#50814 = DIRECTION ( 'NONE',  ( -1.000000000000000000, 0.000000000000000000, 0.000000000000000000 ) ) ;
#50815 = CARTESIAN_POINT ( 'NONE',  ( 5.515188684475870851, -0.004893136156457983908, 0.002166413411657847846 ) ) ;
#50816 = AXIS2_PLACEMENT_3D ( 'NONE', #41625, #26336, #22315 ) ;
#50817 = CARTESIAN_POINT ( 'NONE',  ( 2.430348790457138364, -7.611893186157356439, -1.144258029164478385 ) ) ;
#50818 = ADVANCED_FACE ( 'NONE', ( #9090 ), #29372, .T. ) ;
#50819 = CARTESIAN_POINT ( 'NONE',  ( 2.266490820343019408, 2.476945027124536125, -7.230273269342557541 ) ) ;
#50820 = EDGE_LOOP ( 'NONE', ( #51349, #43765, #14565, #42943 ) ) ;
#50821 = CARTESIAN_POINT ( 'NONE',  ( 47.00000000000000711, 4.705694406421931860E-17, -3.469127814946512892E-15 ) ) ;
#50822 = CARTESIAN_POINT ( 'NONE',  ( -30.01168020819624616, -3.375037589979597463, -11.52238638448564600 ) ) ;
#50823 = CARTESIAN_POINT ( 'NONE',  ( 0.9296196016833884190, -12.34355205587689319, 1.754499435240041150 ) ) ;
#50824 = CIRCLE ( 'NONE', #3043, 5.000000000000000888 ) ;
#50825 = DIRECTION ( 'NONE',  ( 1.000000000000000000, -0.000000000000000000, 0.000000000000000000 ) ) ;
#50826 = B_SPLINE_CURVE_WITH_KNOTS ( 'NONE', 3,
 ( #5611, #40161, #31194, #20562, #35168, #35513, #30515, #50819, #51499, #60453, #14877, #56116, #9919, #614, #41144, #61426, #30206, #20220, #5946 ),
 .UNSPECIFIED., .F., .F.,
 ( 4, 3, 3, 3, 3, 3, 4 ),
 ( 6.829613154537258970E-18, 2.825908398850651652E-05, 4.208813692510337049E-05, 5.591713746977225327E-05, 6.279584083268735550E-05, 9.105792820348497226E-05, 0.0001153131102488632871 ),
 .UNSPECIFIED. ) ;
#50827 = EDGE_CURVE ( 'NONE', #42070, #49910, #31812, .T. ) ;
#50828 = CARTESIAN_POINT ( 'NONE',  ( -18.01507738101584621, -4.918977875164763702, 10.94647906529714732 ) ) ;
#50829 = CARTESIAN_POINT ( 'NONE',  ( 2.305787727787084407, 2.774453000917148415, 7.135468203929992370 ) ) ;
#50830 = ORIENTED_EDGE ( 'NONE', *, *, #34589, .F. ) ;
#50831 = EDGE_CURVE ( 'NONE', #5805, #17595, #54243, .T. ) ;
#50832 = CARTESIAN_POINT ( 'NONE',  ( -37.00000000000000711, -4.732539170486343316, 11.23004253107762906 ) ) ;
#50833 = ORIENTED_EDGE ( 'NONE', *, *, #60208, .T. ) ;
#50834 = CARTESIAN_POINT ( 'NONE',  ( 0.3654063281920733042, -0.2633658439602484802, -12.27672420655578911 ) ) ;
#50835 = CARTESIAN_POINT ( 'NONE',  ( -15.60798173054863014, -34.17470894020248551, 7.727686298002682364 ) ) ;
#50836 = CARTESIAN_POINT ( 'NONE',  ( -22.27384469013076185, -0.9224151068931498720, -3.564715702084492399 ) ) ;
#50837 = CARTESIAN_POINT ( 'NONE',  ( 0.3160775863651118511, -11.60348481172938406, 3.967735865794311145 ) ) ;
#50838 = AXIS2_PLACEMENT_3D ( 'NONE', #47546, #1682, #42197 ) ;
#50839 = VERTEX_POINT ( 'NONE', #61581 ) ;
#50840 = ORIENTED_EDGE ( 'NONE', *, *, #34750, .T. ) ;
#50842 = EDGE_CURVE ( 'NONE', #44156, #34336, #10466, .T. ) ;
#50841 = CARTESIAN_POINT ( 'NONE',  ( -25.00000000000000355, -28.99999999999999645, -5.000000000000000000 ) ) ;
#50843 = VERTEX_POINT ( 'NONE', #36318 ) ;
#50844 = DIRECTION ( 'NONE',  ( -1.000000000000000000, 0.000000000000000000, -0.000000000000000000 ) ) ;
#50845 = CARTESIAN_POINT ( 'NONE',  ( -18.49080574448724690, 11.99999999999999645, 2.510045011421233839E-15 ) ) ;
#50846 = CARTESIAN_POINT ( 'NONE',  ( -22.27716857039623477, -3.514919882996453637, -1.095155339732105881 ) ) ;
#50847 = CARTESIAN_POINT ( 'NONE',  ( 0.8375941296786644230, 9.275620596396400686, 8.285008510334364473 ) ) ;
#50849 = CARTESIAN_POINT ( 'NONE',  ( 3.152665057734127974, -4.377619405892426485, 6.622010822086644488 ) ) ;
#50848 = AXIS2_PLACEMENT_3D ( 'NONE', #32050, #47045, #17094 ) ;
#50850 = CARTESIAN_POINT ( 'NONE',  ( 0.3040950598368144520, -7.687624643091368171, -9.552450779732186703 ) ) ;
#50851 = DIRECTION ( 'NONE',  ( -0.02770351589312032917, 0.9996161839461982224, 0.000000000000000000 ) ) ;
#50852 = ORIENTED_EDGE ( 'NONE', *, *, #14547, .F. ) ;
#50853 = CARTESIAN_POINT ( 'NONE',  ( 1.375507693218758432, -11.20969178069603700, 5.789143338282145557 ) ) ;
#50854 = ORIENTED_EDGE ( 'NONE', *, *, #6400, .T. ) ;
#50855 = CARTESIAN_POINT ( 'NONE',  ( 35.00000000000000000, -4.426194442447322075, -11.35427606708804937 ) ) ;
#50856 = CIRCLE ( 'NONE', #4146, 2.899999999999993694 ) ;
#50857 = CARTESIAN_POINT ( 'NONE',  ( -27.09483304420744787, 1.923212037694859822, -1.303111346475867904 ) ) ;
#50858 = ORIENTED_EDGE ( 'NONE', *, *, #47715, .F. ) ;
#50859 = FACE_OUTER_BOUND ( 'NONE', #40409, .T. ) ;
#50860 = ORIENTED_EDGE ( 'NONE', *, *, #20659, .F. ) ;
#50861 = CIRCLE ( 'NONE', #1873, 4.999999999999999112 ) ;
#50862 = PLANE ( 'NONE',  #31211 ) ;
#50863 = CARTESIAN_POINT ( 'NONE',  ( 6.788880239637845371, -6.730272244910862511, -11.70889290456736909 ) ) ;
#50864 = CARTESIAN_POINT ( 'NONE',  ( 0.000000000000000000, 0.000000000000000000, 0.000000000000000000 ) ) ;
#50865 = DIRECTION ( 'NONE',  ( 1.000000000000000000, -0.000000000000000000, -0.000000000000000000 ) ) ;
#50866 = ORIENTED_EDGE ( 'NONE', *, *, #26156, .F. ) ;
#50867 = VERTEX_POINT ( 'NONE', #443 ) ;
#50868 = VECTOR ( 'NONE', #15532, 1000.000000000000000 ) ;
#50869 = CARTESIAN_POINT ( 'NONE',  ( 1.000000000000000888, 7.493043167941614513, -0.3229614270519962638 ) ) ;
#50870 = ORIENTED_EDGE ( 'NONE', *, *, #55425, .F. ) ;
#50871 = CARTESIAN_POINT ( 'NONE',  ( -35.00000000000000000, -3.645068577060105230, 11.16627499335654150 ) ) ;
#50872 = ORIENTED_EDGE ( 'NONE', *, *, #63432, .F. ) ;
#50873 = VERTEX_POINT ( 'NONE', #15049 ) ;
#50874 = AXIS2_PLACEMENT_3D ( 'NONE', #51407, #55047, #14468 ) ;
#50875 = ORIENTED_EDGE ( 'NONE', *, *, #59857, .T. ) ;
#50876 = CARTESIAN_POINT ( 'NONE',  ( 3.031336079628848879, -5.773872239512904514, 5.388626255826518552 ) ) ;
#50877 = CARTESIAN_POINT ( 'NONE',  ( -0.9955874700083148232, -25.73414319850213161, 15.65071058219114342 ) ) ;
#50878 = ADVANCED_FACE ( 'NONE', ( #21354 ), #40657, .T. ) ;
#50879 = CARTESIAN_POINT ( 'NONE',  ( 1.719304012338439325, 7.017415949612858306, 10.62216384465677521 ) ) ;
#50880 = DIRECTION ( 'NONE',  ( 0.000000000000000000, -1.000000000000000000, 0.000000000000000000 ) ) ;
#50881 = CARTESIAN_POINT ( 'NONE',  ( -35.04683013664716640, -0.004196202180954865246, -0.01162359816266951562 ) ) ;
#50882 = ORIENTED_EDGE ( 'NONE', *, *, #18439, .T. ) ;
#50883 = CARTESIAN_POINT ( 'NONE',  ( -21.17861794710831091, 25.00000000000000000, -3.604945070120774808 ) ) ;
#50884 =( BOUNDED_SURFACE ( )  B_SPLINE_SURFACE ( 3, 1, ( 
 ( #9064, #34643 ),
 ( #64904, #18414 ),
 ( #23726, #29344 ),
 ( #18738, #7767 ) ),
 .UNSPECIFIED., .F., .F., .F. ) 
 B_SPLINE_SURFACE_WITH_KNOTS ( ( 4, 4 ),
 ( 2, 2 ),
 ( 0.000000000000000000, 1.000000000000000000 ),
 ( 0.000000000000000000, 1.000000000000000000 ),
 .UNSPECIFIED. ) 
 GEOMETRIC_REPRESENTATION_ITEM ( )  RATIONAL_B_SPLINE_SURFACE ( (
 ( 1.000000000000000000, 1.000000000000000000),
 ( 0.9932032654565553509, 0.8386279382598740284),
 ( 0.9932032654565553509, 0.8386279382598740284),
 ( 1.000000000000000000, 1.000000000000000000) ) ) 
 REPRESENTATION_ITEM ( '' )  SURFACE ( )  );
#50885 = ORIENTED_EDGE ( 'NONE', *, *, #3872, .F. ) ;
#50886 = CARTESIAN_POINT ( 'NONE',  ( -27.09342121492585420, 0.6436068655225422042, 2.227768580955189925 ) ) ;
#50887 = ORIENTED_EDGE ( 'NONE', *, *, #49803, .T. ) ;
#50888 = CARTESIAN_POINT ( 'NONE',  ( 36.00000000000000711, 5.865551165831078606, -11.32068061209297483 ) ) ;
#50889 = CARTESIAN_POINT ( 'NONE',  ( 35.00000000000000000, 4.705694406421931860E-17, -3.469127814946512892E-15 ) ) ;
#50890 = FACE_OUTER_BOUND ( 'NONE', #58105, .T. ) ;
#50891 = CIRCLE ( 'NONE', #37050, 12.18649999999999878 ) ;
#50892 = EDGE_CURVE ( 'NONE', #40209, #26482, #10386, .T. ) ;
#50893 = VERTEX_POINT ( 'NONE', #61267 ) ;
#50894 = CARTESIAN_POINT ( 'NONE',  ( 35.00000000000000000, -3.340853584269612764, -11.26103545359855040 ) ) ;
#50895 = AXIS2_PLACEMENT_3D ( 'NONE', #8594, #53841, #17929 ) ;
#50896 = EDGE_LOOP ( 'NONE', ( #64416, #52182, #44229, #65427 ) ) ;
#50897 = ADVANCED_FACE ( 'NONE', ( #30359 ), #44438, .F. ) ;
#50898 = DIRECTION ( 'NONE',  ( 0.000000000000000000, 0.2960891610144441022, 0.9551603052523500725 ) ) ;
#50899 = CARTESIAN_POINT ( 'NONE',  ( 16.71517827323052785, -28.42750353049531853, -9.642361815241612177 ) ) ;
#50900 = CARTESIAN_POINT ( 'NONE',  ( -13.38666790241063964, -28.49056413965659473, 12.64716857254873617 ) ) ;
#50901 = CARTESIAN_POINT ( 'NONE',  ( 2.305787727787084407, 3.971363876083963351, 6.545285700970541853 ) ) ;
#50902 = ADVANCED_FACE ( 'NONE', ( #60609 ), #30662, .T. ) ;
#50903 = CARTESIAN_POINT ( 'NONE',  ( 35.00000000000000000, 2.544412758415841580, -11.91791701451267471 ) ) ;
#50904 = ORIENTED_EDGE ( 'NONE', *, *, #20882, .F. ) ;
#50905 = CARTESIAN_POINT ( 'NONE',  ( -35.00000000000000000, -8.052525312709946093, 8.551552972817052733 ) ) ;
#50906 = CARTESIAN_POINT ( 'NONE',  ( 1.014383007554943594, 5.859361736620487981, -11.03701226956410508 ) ) ;
#50907 = DIRECTION ( 'NONE',  ( 0.000000000000000000, -0.07632122047557189648, 0.9970832820307033995 ) ) ;
#50908 = LINE ( 'NONE', #30937, #26356 ) ;
#50909 = AXIS2_PLACEMENT_3D ( 'NONE', #33158, #58797, #13215 ) ;
#50910 = AXIS2_PLACEMENT_3D ( 'NONE', #48803, #37499, #3254 ) ;
#50911 = EDGE_CURVE ( 'NONE', #47922, #63874, #58519, .T. ) ;
#50912 = VECTOR ( 'NONE', #42060, 1000.000000000000000 ) ;
#50913 = CARTESIAN_POINT ( 'NONE',  ( 0.3610902822527198297, 12.27530799859938959, -0.2623004149195046208 ) ) ;
#50914 = EDGE_CURVE ( 'NONE', #9977, #22363, #31006, .T. ) ;
#50915 = FACE_OUTER_BOUND ( 'NONE', #46872, .T. ) ;
#50916 = EDGE_CURVE ( 'NONE', #33895, #23378, #34188, .T. ) ;
#50917 = CARTESIAN_POINT ( 'NONE',  ( 0.2651627923886311078, -2.213220384814353903, 12.04449855907067501 ) ) ;
#50918 = DIRECTION ( 'NONE',  ( -1.000000000000000000, 0.000000000000000000, 0.000000000000000000 ) ) ;
#50919 = CARTESIAN_POINT ( 'NONE',  ( 1.937114397841935398, 7.538912286488483439, -10.38782037574609163 ) ) ;
#50920 = AXIS2_PLACEMENT_3D ( 'NONE', #8023, #48581, #42919 ) ;
#50921 = EDGE_CURVE ( 'NONE', #40113, #60906, #25547, .T. ) ;
#50922 = VERTEX_POINT ( 'NONE', #41298 ) ;
#50923 = EDGE_CURVE ( 'NONE', #35283, #10110, #11261, .T. ) ;
#50924 = VERTEX_POINT ( 'NONE', #11063 ) ;
#50925 = DIRECTION ( 'NONE',  ( -1.000000000000000000, 0.000000000000000000, 0.000000000000000000 ) ) ;
#50926 = CARTESIAN_POINT ( 'NONE',  ( 48.22764741571069891, -0.3553121838687465228, 6.242084797467406965 ) ) ;
#50927 = CARTESIAN_POINT ( 'NONE',  ( 2.000000000000001776, -1.225832621831887792, 6.827324998361543607 ) ) ;
#50928 = ADVANCED_FACE ( 'NONE', ( #50654 ), #13895, .T. ) ;
#50929 = CARTESIAN_POINT ( 'NONE',  ( 2.241537034860904942, 3.813147095850985213, 6.614004440763060266 ) ) ;
#50930 = VERTEX_POINT ( 'NONE', #38192 ) ;
#50931 = ORIENTED_EDGE ( 'NONE', *, *, #48735, .F. ) ;
#50932 = ORIENTED_EDGE ( 'NONE', *, *, #64705, .T. ) ;
#50933 = CARTESIAN_POINT ( 'NONE',  ( 1.000000000000000888, -3.073484823194281290, -6.841322316745092280 ) ) ;
#50935 = CARTESIAN_POINT ( 'NONE',  ( 2.941278708680199916, -5.721889327162137384, -2.226055275041848525 ) ) ;
#50934 = AXIS2_PLACEMENT_3D ( 'NONE', #38549, #13909, #8294 ) ;
#50936 = ORIENTED_EDGE ( 'NONE', *, *, #3021, .T. ) ;
#50937 = DIRECTION ( 'NONE',  ( 0.000000000000000000, -0.01356324068817992175, 0.9999080150203990547 ) ) ;
#50938 = LINE ( 'NONE', #31936, #6088 ) ;
#50939 = CARTESIAN_POINT ( 'NONE',  ( 3.152665057735716037, -2.258875078500806044, 7.609997527621833235 ) ) ;
#50940 = VERTEX_POINT ( 'NONE', #53529 ) ;
#50941 = CARTESIAN_POINT ( 'NONE',  ( 2.241352910868908754, 4.843133558968205854, -5.901537464758406237 ) ) ;
#50942 = AXIS2_PLACEMENT_3D ( 'NONE', #18097, #6239, #61747 ) ;
#50943 = CARTESIAN_POINT ( 'NONE',  ( -1.046707184715599759, -26.56309036555548886, -16.21005351936483052 ) ) ;
#50944 = DIRECTION ( 'NONE',  ( 1.000000000000000000, 0.000000000000000000, 0.000000000000000000 ) ) ;
#50945 = VERTEX_POINT ( 'NONE', #8277 ) ;
#50946 = CARTESIAN_POINT ( 'NONE',  ( -19.47984447937493613, -1.416020129149132334, 25.00000000000000000 ) ) ;
#50947 = EDGE_LOOP ( 'NONE', ( #36139, #45377, #21365, #24283 ) ) ;
#50948 = CARTESIAN_POINT ( 'NONE',  ( -37.00000000000000711, 1.286231064351496922, -12.68495603654570481 ) ) ;
#50949 = ORIENTED_EDGE ( 'NONE', *, *, #57931, .T. ) ;
#50950 = CARTESIAN_POINT ( 'NONE',  ( 12.10998784662220729, -8.443435280036764468, -8.526922110106905706 ) ) ;
#50951 = AXIS2_PLACEMENT_3D ( 'NONE', #57228, #11655, #21970 ) ;
#50952 = CARTESIAN_POINT ( 'NONE',  ( -14.83484859610010886, -34.67578963453992458, 7.338086519103280025 ) ) ;
#50953 = CARTESIAN_POINT ( 'NONE',  ( 2.000000000000001776, -4.915517050588371184, -4.717154614762162801 ) ) ;
#50954 = DIRECTION ( 'NONE',  ( 1.000000000000000000, 0.000000000000000000, 0.000000000000000000 ) ) ;
#50955 = EDGE_CURVE ( 'NONE', #21432, #31007, #53279, .T. ) ;
#50956 = CARTESIAN_POINT ( 'NONE',  ( 36.00000000000000711, 12.74921544981111055, -0.1414404973752615424 ) ) ;
#50957 = CARTESIAN_POINT ( 'NONE',  ( 2.257661810676422576, 5.764872664104583322, -5.013319178751116212 ) ) ;
#50958 = CARTESIAN_POINT ( 'NONE',  ( -27.08426504710140392, 2.223709847896212732, -0.5533780324190695765 ) ) ;
#50959 = CARTESIAN_POINT ( 'NONE',  ( -35.00000000000000000, -8.017674001891851532, 9.913596905230086520 ) ) ;
#50961 = ORIENTED_EDGE ( 'NONE', *, *, #65228, .T. ) ;
#50960 = LINE ( 'NONE', #61251, #26775 ) ;
#50962 = CIRCLE ( 'NONE', #56259, 6.936499999999993449 ) ;
#50963 = CYLINDRICAL_SURFACE ( 'NONE', #22622, 5.000000000000000888 ) ;
#50964 = ORIENTED_EDGE ( 'NONE', *, *, #37336, .T. ) ;
#50965 = CARTESIAN_POINT ( 'NONE',  ( 11.83609954913792883, -13.39357575799777145, -1.699053554970645363 ) ) ;
#50966 = ORIENTED_EDGE ( 'NONE', *, *, #22895, .F. ) ;
#50967 = CARTESIAN_POINT ( 'NONE',  ( 3.152665057734040488, 0.000000000000000000, 0.000000000000000000 ) ) ;
#50968 = ORIENTED_EDGE ( 'NONE', *, *, #41754, .F. ) ;
#50969 = EDGE_CURVE ( 'NONE', #65490, #24851, #38868, .T. ) ;
#50970 = CARTESIAN_POINT ( 'NONE',  ( 0.3610902822527199407, 8.091349661862622611, 9.234828023175118972 ) ) ;
#50971 = CARTESIAN_POINT ( 'NONE',  ( -37.25000000000000711, -45.00200000000000244, 4.499999999999997335 ) ) ;
#50972 = VECTOR ( 'NONE', #5991, 1000.000000000000000 ) ;
#50973 = DIRECTION ( 'NONE',  ( -1.000000000000000000, 0.000000000000000000, 0.000000000000000000 ) ) ;
#50974 = CARTESIAN_POINT ( 'NONE',  ( -22.27945548916780183, 1.551028078364857343, -3.346394890313965753 ) ) ;
#50975 = CARTESIAN_POINT ( 'NONE',  ( 2.257661810674664871, 7.224098098129182688, 2.485866587323505961 ) ) ;
#50976 = ADVANCED_FACE ( 'NONE', ( #58169 ), #12590, .T. ) ;
#50977 = ORIENTED_EDGE ( 'NONE', *, *, #53310, .T. ) ;
#50978 = CARTESIAN_POINT ( 'NONE',  ( -17.15262702242703341, -7.064764427389573775, -9.706288918837138624 ) ) ;
#50979 = VERTEX_POINT ( 'NONE', #7970 ) ;
#50980 = CARTESIAN_POINT ( 'NONE',  ( 2.507146904658095643, -6.052884339496452881, 4.796593924427959621 ) ) ;
#50981 = DIRECTION ( 'NONE',  ( -1.000000000000000000, 0.000000000000000000, 0.000000000000000000 ) ) ;
#50982 = ADVANCED_FACE ( 'NONE', ( #2670 ), #48530, .T. ) ;
#50983 = ORIENTED_EDGE ( 'NONE', *, *, #59989, .F. ) ;
#50984 = CARTESIAN_POINT ( 'NONE',  ( 0.3632410797595253538, -4.445654054452453430, -11.44577450250091566 ) ) ;
#50985 = CIRCLE ( 'NONE', #44587, 12.18649999999999878 ) ;
#50986 = CARTESIAN_POINT ( 'NONE',  ( 50.00070814568294963, 0.0001445496031041041481, 0.7971761463862205854 ) ) ;
#50987 = DIRECTION ( 'NONE',  ( -1.000000000000000000, -0.000000000000000000, -0.000000000000000000 ) ) ;
#50988 = CARTESIAN_POINT ( 'NONE',  ( 0.000000000000000000, -1.018311147294196806, 6.861346417234461370 ) ) ;
#50989 = VERTEX_POINT ( 'NONE', #64442 ) ;
#50990 = CARTESIAN_POINT ( 'NONE',  ( 2.241352910868908310, 6.652881166698564108, -3.744764251556923274 ) ) ;
#50991 = CARTESIAN_POINT ( 'NONE',  ( 8.434373009633013396, -31.78234095107969281, 13.63772037844789864 ) ) ;
#50992 = CARTESIAN_POINT ( 'NONE',  ( 0.000000000000000000, 0.000000000000000000, 0.000000000000000000 ) ) ;
#50993 = EDGE_CURVE ( 'NONE', #37253, #27036, #61160, .T. ) ;
#50994 = AXIS2_PLACEMENT_3D ( 'NONE', #44138, #9203, #19537 ) ;
#50995 = B_SPLINE_CURVE_WITH_KNOTS ( 'NONE', 3,
 ( #45982, #41292, #49981, #30354, #15688, #35967, #9389, #14699, #20371, #40311, #50649, #55286, #55949, #50330, #5092, #44991, #5761, #30658, #50970, #5420, #65577, #25356 ),
 .UNSPECIFIED., .F., .F.,
 ( 4, 3, 3, 3, 3, 3, 3, 4 ),
 ( 1.626303258728256651E-19, 4.449119708436531195E-05, 6.626296329540292784E-05, 8.803456484962480090E-05, 0.0001098060367612777635, 0.0001315774408628478192, 0.0001760698110411119260, 0.0001829697163287825890 ),
 .UNSPECIFIED. ) ;
#50996 = EDGE_CURVE ( 'NONE', #7257, #62589, #38309, .T. ) ;
#50997 = DIRECTION ( 'NONE',  ( 1.000000000000000000, -0.000000000000000000, 0.000000000000000000 ) ) ;
#50998 = CYLINDRICAL_SURFACE ( 'NONE', #40413, 13.50000000000000178 ) ;
#50999 = AXIS2_PLACEMENT_3D ( 'NONE', #64084, #29175, #23869 ) ;
#51000 = ORIENTED_EDGE ( 'NONE', *, *, #44789, .T. ) ;
#51001 = DIRECTION ( 'NONE',  ( 1.000000000000000000, 0.000000000000000000, 0.000000000000000000 ) ) ;
#51002 = LINE ( 'NONE', #5461, #22603 ) ;
#51003 = CARTESIAN_POINT ( 'NONE',  ( -22.28546858134833641, 3.567529619157801868, -1.005093225210833330 ) ) ;
#51004 = ORIENTED_EDGE ( 'NONE', *, *, #46490, .F. ) ;
#51005 = EDGE_CURVE ( 'NONE', #13375, #62432, #29808, .T. ) ;
#51006 = CARTESIAN_POINT ( 'NONE',  ( 5.515188684475870851, -0.005194992164431762316, 0.001283816547385177240 ) ) ;
#51007 = CARTESIAN_POINT ( 'NONE',  ( 35.00000000000000000, 4.705694406421931860E-17, -3.469127814946512892E-15 ) ) ;
#51008 = ORIENTED_EDGE ( 'NONE', *, *, #52660, .F. ) ;
#51009 = CIRCLE ( 'NONE', #24, 12.18649999999999878 ) ;
#51010 = ORIENTED_EDGE ( 'NONE', *, *, #50186, .F. ) ;
#51011 = ORIENTED_EDGE ( 'NONE', *, *, #50911, .T. ) ;
#51012 = EDGE_LOOP ( 'NONE', ( #13047, #2963, #62946, #11027 ) ) ;
#51013 = DIRECTION ( 'NONE',  ( 0.000000000000000000, 0.01356324068817998940, -0.9999080150203990547 ) ) ;
#51014 = DIRECTION ( 'NONE',  ( 0.000000000000000000, 0.01356324068817991828, -0.9999080150203990547 ) ) ;
#51015 = CARTESIAN_POINT ( 'NONE',  ( 2.889800649504073782, -3.118861721612529170, -5.267262008933701445 ) ) ;
#51016 = AXIS2_PLACEMENT_3D ( 'NONE', #20029, #53976, #29661 ) ;
#51017 = CARTESIAN_POINT ( 'NONE',  ( 8.982479512971032420, 5.162787350578708967, 10.83868146673709276 ) ) ;
#51018 = DIRECTION ( 'NONE',  ( 0.000000000000000000, 0.000000000000000000, -1.000000000000000000 ) ) ;
#51019 = CARTESIAN_POINT ( 'NONE',  ( -6.714735010819111949, -31.93429545817926751, 13.37736225704815141 ) ) ;
#51020 = DIRECTION ( 'NONE',  ( 1.000000000000000000, 0.000000000000000000, 0.000000000000000000 ) ) ;
#51022 = ORIENTED_EDGE ( 'NONE', *, *, #59830, .F. ) ;
#51021 = CARTESIAN_POINT ( 'NONE',  ( 5.515188684475870851, 0.0003622115669623291682, -0.005339000964281804575 ) ) ;
#51024 = CIRCLE ( 'NONE', #2170, 12.74999999999999822 ) ;
#51023 = CARTESIAN_POINT ( 'NONE',  ( -36.00000000000000711, 12.21925492305362226, 3.640372113593595138 ) ) ;
#51025 = ORIENTED_EDGE ( 'NONE', *, *, #2124, .F. ) ;
#51026 = CARTESIAN_POINT ( 'NONE',  ( 5.514970785353741078, 0.002796696073589870733, 0.003805873180274323229 ) ) ;
#51027 = EDGE_LOOP ( 'NONE', ( #3020, #13231, #55599, #3387 ) ) ;
#51028 = ORIENTED_EDGE ( 'NONE', *, *, #61367, .F. ) ;
#51029 = CARTESIAN_POINT ( 'NONE',  ( 0.3537226245948408843, 9.569332148897569112, -7.688925565304919552 ) ) ;
#51030 = CARTESIAN_POINT ( 'NONE',  ( 14.48396081724360229, -30.02861890643185916, 3.972401191364298700 ) ) ;
#51031 = CARTESIAN_POINT ( 'NONE',  ( -35.00000000000000000, 5.672855678558835102, -10.28547182238001767 ) ) ;
#51032 = VECTOR ( 'NONE', #49218, 1000.000000000000000 ) ;
#51033 = EDGE_CURVE ( 'NONE', #6128, #43782, #59162, .T. ) ;
#51034 = AXIS2_PLACEMENT_3D ( 'NONE', #59563, #64531, #44258 ) ;
#51035 = AXIS2_PLACEMENT_3D ( 'NONE', #19323, #44250, #59234 ) ;
#51037 = CIRCLE ( 'NONE', #22339, 12.75000000000000178 ) ;
#51036 = CARTESIAN_POINT ( 'NONE',  ( 1.719304012340749033, -5.066286238787660601, -11.67935079956571087 ) ) ;
#51038 = DIRECTION ( 'NONE',  ( -1.000000000000000000, 0.000000000000000000, 0.000000000000000000 ) ) ;
#51039 = DIRECTION ( 'NONE',  ( -1.000000000000000000, 0.000000000000000000, 0.000000000000000000 ) ) ;
#51040 = VERTEX_POINT ( 'NONE', #18913 ) ;
#51041 = EDGE_CURVE ( 'NONE', #16656, #16455, #29520, .T. ) ;
#51042 = EDGE_LOOP ( 'NONE', ( #51242, #55160, #58830, #45354 ) ) ;
#51043 = FACE_OUTER_BOUND ( 'NONE', #8026, .T. ) ;
#51044 = ORIENTED_EDGE ( 'NONE', *, *, #9899, .F. ) ;
#51045 = ORIENTED_EDGE ( 'NONE', *, *, #4620, .T. ) ;
#51046 = EDGE_CURVE ( 'NONE', #18668, #24851, #13853, .T. ) ;
#51047 = CARTESIAN_POINT ( 'NONE',  ( -17.29244623348158783, 2.525873743887551814, 25.00000000000000000 ) ) ;
#51048 = DIRECTION ( 'NONE',  ( 1.000000000000000000, 0.000000000000000000, -0.000000000000000000 ) ) ;
#51049 = DIRECTION ( 'NONE',  ( -1.000000000000000000, -1.836970198721029688E-16, -0.000000000000000000 ) ) ;
#51050 = CARTESIAN_POINT ( 'NONE',  ( 1.194176325881333600, -12.26540585042610410, 2.684784923266246626 ) ) ;
#51052 = AXIS2_PLACEMENT_3D ( 'NONE', #12469, #33091, #12803 ) ;
#51051 = DIRECTION ( 'NONE',  ( 0.000000000000000000, 0.000000000000000000, 1.000000000000000000 ) ) ;
#51053 = DIRECTION ( 'NONE',  ( 0.000000000000000000, -0.01356324068817998940, 0.9999080150203990547 ) ) ;
#51054 = AXIS2_PLACEMENT_3D ( 'NONE', #31181, #57113, #47143 ) ;
#51055 = AXIS2_PLACEMENT_3D ( 'NONE', #32165, #27509, #16573 ) ;
#51056 = ORIENTED_EDGE ( 'NONE', *, *, #40656, .T. ) ;
#51057 = ORIENTED_EDGE ( 'NONE', *, *, #65440, .T. ) ;
#51058 = VECTOR ( 'NONE', #40828, 1000.000000000000000 ) ;
#51059 = CARTESIAN_POINT ( 'NONE',  ( 35.00000000000000000, 4.705694406421931860E-17, -3.469127814946512892E-15 ) ) ;
#51060 = EDGE_CURVE ( 'NONE', #57376, #17810, #19573, .T. ) ;
#51061 = CARTESIAN_POINT ( 'NONE',  ( 2.280717697723836146, 7.502592193582066749, -1.481796453660239044 ) ) ;
#51062 = AXIS2_PLACEMENT_3D ( 'NONE', #13005, #7344, #59224 ) ;
#51063 = CARTESIAN_POINT ( 'NONE',  ( -2.665275975174092871, -8.247467911538802099, 10.69349901239360001 ) ) ;
#51064 = EDGE_CURVE ( 'NONE', #23892, #40032, #30504, .T. ) ;
#51065 = CARTESIAN_POINT ( 'NONE',  ( 6.774697637567625996, -5.779741746118725487, 10.51838463467937856 ) ) ;
#51066 = CYLINDRICAL_SURFACE ( 'NONE', #49211, 5.000000000000000888 ) ;
#51067 = CARTESIAN_POINT ( 'NONE',  ( -35.00000000000000000, 0.000000000000000000, 0.000000000000000000 ) ) ;
#51068 = CARTESIAN_POINT ( 'NONE',  ( 3.158320548757213686, 2.992226752387131761, -11.62285000527830192 ) ) ;
#51069 = CARTESIAN_POINT ( 'NONE',  ( 3.092491956585259327, 6.343509225034840604, 4.738927301402335424 ) ) ;
#51070 = AXIS2_PLACEMENT_3D ( 'NONE', #3848, #59046, #13455 ) ;
#51071 = VERTEX_POINT ( 'NONE', #60779 ) ;
#51072 = CARTESIAN_POINT ( 'NONE',  ( 0.2652384770603641306, 10.57229757085623056, 6.180206054297643803 ) ) ;
#51073 = DIRECTION ( 'NONE',  ( 0.000000000000000000, 0.01356324068817998940, -0.9999080150203990547 ) ) ;
#51074 = DIRECTION ( 'NONE',  ( 0.000000000000000000, -0.01356324068817998940, 0.9999080150203990547 ) ) ;
#51075 = ADVANCED_FACE ( 'NONE', ( #60123 ), #65101, .T. ) ;
#51076 = AXIS2_PLACEMENT_3D ( 'NONE', #59026, #8138, #44667 ) ;
#51077 = AXIS2_PLACEMENT_3D ( 'NONE', #7890, #37805, #32471 ) ;
#51078 = CIRCLE ( 'NONE', #7535, 12.75000000000000178 ) ;
#51079 = ADVANCED_FACE ( 'NONE', ( #24883 ), #29846, .T. ) ;
#51080 = CARTESIAN_POINT ( 'NONE',  ( -15.66937148611491359, -34.93011823067270427, -5.816432770871436730 ) ) ;
#51081 = CARTESIAN_POINT ( 'NONE',  ( -37.00000000000000711, 1.903127969211188653, 11.59095880812009227 ) ) ;
#51082 =( BOUNDED_SURFACE ( )  B_SPLINE_SURFACE ( 3, 1, ( 
 ( #45230, #65489 ),
 ( #50881, #5328 ),
 ( #40225, #55542 ),
 ( #25267, #45894 ) ),
 .UNSPECIFIED., .F., .F., .F. ) 
 B_SPLINE_SURFACE_WITH_KNOTS ( ( 4, 4 ),
 ( 2, 2 ),
 ( 0.000000000000000000, 1.000000000000000000 ),
 ( 0.000000000000000000, 1.000000000000000000 ),
 .UNSPECIFIED. ) 
 GEOMETRIC_REPRESENTATION_ITEM ( )  RATIONAL_B_SPLINE_SURFACE ( (
 ( 1.000000000000000000, 1.000000000000000000),
 ( 0.9932032654565553509, 0.8386279382598736953),
 ( 0.9932032654565553509, 0.8386279382598736953),
 ( 1.000000000000000000, 1.000000000000000000) ) ) 
 REPRESENTATION_ITEM ( '' )  SURFACE ( )  );
#51083 = ORIENTED_EDGE ( 'NONE', *, *, #46689, .F. ) ;
#51084 = CARTESIAN_POINT ( 'NONE',  ( 2.241506898688418126, -3.851253041557060719, -6.591904579673272480 ) ) ;
#51085 = CARTESIAN_POINT ( 'NONE',  ( 28.03536240197431439, 12.64334364039261693, 4.746761413380614414 ) ) ;
#51086 = CARTESIAN_POINT ( 'NONE',  ( 2.253265082352434501, 1.199885753716626091, 7.543541742286975271 ) ) ;
#51087 = ORIENTED_EDGE ( 'NONE', *, *, #16997, .T. ) ;
#51088 = CARTESIAN_POINT ( 'NONE',  ( 2.406456491625667660, -7.573451137023450741, 7.176027849161565442 ) ) ;
#51089 = DIRECTION ( 'NONE',  ( 0.000000000000000000, -0.01356324068817992175, 0.9999080150203990547 ) ) ;
#51090 = DIRECTION ( 'NONE',  ( 1.000000000000000000, 0.000000000000000000, -0.000000000000000000 ) ) ;
#51092 = ORIENTED_EDGE ( 'NONE', *, *, #5579, .F. ) ;
#51091 = DIRECTION ( 'NONE',  ( -1.000000000000000000, 0.000000000000000000, 0.000000000000000000 ) ) ;
#51093 = CYLINDRICAL_SURFACE ( 'NONE', #42634, 6.000000000000000888 ) ;
#51094 = AXIS2_PLACEMENT_3D ( 'NONE', #18887, #24189, #29818 ) ;
#51095 = CARTESIAN_POINT ( 'NONE',  ( -22.94572469358971034, -4.870584850960110401, -0.4123340087948408894 ) ) ;
#51096 = VERTEX_POINT ( 'NONE', #29219 ) ;
#51097 = CIRCLE ( 'NONE', #53230, 12.18650000000000233 ) ;
#51098 = FACE_OUTER_BOUND ( 'NONE', #31977, .T. ) ;
#51099 = CIRCLE ( 'NONE', #19245, 7.938172270156617749 ) ;
#51100 = DIRECTION ( 'NONE',  ( 0.000000000000000000, 1.000000000000000000, 0.000000000000000000 ) ) ;
#51101 = CARTESIAN_POINT ( 'NONE',  ( 0.2650492594609232255, -7.955687020697113532, 9.309909082761121724 ) ) ;
#51102 = CARTESIAN_POINT ( 'NONE',  ( 2.000000000000001776, -3.341639490130703827, -6.078525953551491057 ) ) ;
#51103 = DIRECTION ( 'NONE',  ( 0.000000000000000000, 0.01356324068817998940, -0.9999080150203990547 ) ) ;
#51104 = AXIS2_PLACEMENT_3D ( 'NONE', #48899, #32909, #53223 ) ;
#51105 = CARTESIAN_POINT ( 'NONE',  ( -37.00000000000000711, 0.000000000000000000, 0.000000000000000000 ) ) ;
#51106 = CARTESIAN_POINT ( 'NONE',  ( -35.00000000000000000, 4.339012074900111315, -10.91536515067643620 ) ) ;
#51107 = VERTEX_POINT ( 'NONE', #39508 ) ;
#51108 = DIRECTION ( 'NONE',  ( 0.000000000000000000, 0.8515178078024849828, -0.5243256840888593784 ) ) ;
#51109 = CIRCLE ( 'NONE', #59594, 12.75000000000000178 ) ;
#51110 = ORIENTED_EDGE ( 'NONE', *, *, #29081, .T. ) ;
#51111 = CARTESIAN_POINT ( 'NONE',  ( 0.000000000000000000, 0.000000000000000000, 0.000000000000000000 ) ) ;
#51112 = CARTESIAN_POINT ( 'NONE',  ( 3.291290029914074378, 8.250315036047103590, -10.68561190601526079 ) ) ;
#51113 = CARTESIAN_POINT ( 'NONE',  ( -37.00000000000000711, 4.561791185930588632, -11.90598845858528776 ) ) ;
#51114 = DIRECTION ( 'NONE',  ( -1.000000000000000000, 0.000000000000000000, 0.000000000000000000 ) ) ;
#51115 = ORIENTED_EDGE ( 'NONE', *, *, #57795, .F. ) ;
#51116 = CARTESIAN_POINT ( 'NONE',  ( 5.515188684475870851, 0.005194992164431771857, -0.001283816547385141027 ) ) ;
#51117 = EDGE_CURVE ( 'NONE', #49961, #8080, #9904, .T. ) ;
#51118 = CARTESIAN_POINT ( 'NONE',  ( 37.00000000000000711, -11.72397916322011824, 0.7214809346829776926 ) ) ;
#51119 = VERTEX_POINT ( 'NONE', #35805 ) ;
#51120 = ORIENTED_EDGE ( 'NONE', *, *, #35659, .F. ) ;
#51121 = CARTESIAN_POINT ( 'NONE',  ( 29.22851443451641984, -10.03996910372599238, 9.034550257766868597 ) ) ;
#51122 = CIRCLE ( 'NONE', #37290, 12.18649999999999878 ) ;
#51123 = ORIENTED_EDGE ( 'NONE', *, *, #55385, .T. ) ;
#51124 = CARTESIAN_POINT ( 'NONE',  ( 22.02159064219758022, -11.31093606971245791, -4.012113827732382454 ) ) ;
#51125 = CYLINDRICAL_SURFACE ( 'NONE', #15072, 12.75000000000000178 ) ;
#51126 = DIRECTION ( 'NONE',  ( -1.000000000000000000, 0.000000000000000000, -0.000000000000000000 ) ) ;
#51127 = DIRECTION ( 'NONE',  ( 0.3939253465568943180, 0.4679616473074897920, -0.7910971609033186080 ) ) ;
#51128 = AXIS2_PLACEMENT_3D ( 'NONE', #57637, #61954, #62265 ) ;
#51129 = AXIS2_PLACEMENT_3D ( 'NONE', #3572, #29449, #13816 ) ;
#51131 = EDGE_CURVE ( 'NONE', #18651, #8885, #56515, .T. ) ;
#51130 = CYLINDRICAL_SURFACE ( 'NONE', #10740, 5.000000000000000888 ) ;
#51132 = CARTESIAN_POINT ( 'NONE',  ( 37.00000000000000711, 4.705694406421931860E-17, -3.469127814946512892E-15 ) ) ;
#51133 = CIRCLE ( 'NONE', #4430, 2.899999999999994582 ) ;
#51134 = CARTESIAN_POINT ( 'NONE',  ( -22.65999102136916576, -1.886119913916072255, -4.450325798697174484 ) ) ;
#51135 = ORIENTED_EDGE ( 'NONE', *, *, #16035, .F. ) ;
#51136 = CARTESIAN_POINT ( 'NONE',  ( 0.4613984246114877785, 12.30830943644279962, -0.2828900474740810300 ) ) ;
#51137 = CARTESIAN_POINT ( 'NONE',  ( 24.73935261814495590, 8.970571808567301630, -7.973448879465720118 ) ) ;
#51138 = EDGE_CURVE ( 'NONE', #39393, #40131, #15214, .T. ) ;
#51139 = CARTESIAN_POINT ( 'NONE',  ( 5.520433897694421610, 0.009283255140285620599, -0.01186170453199863681 ) ) ;
#51140 = CARTESIAN_POINT ( 'NONE',  ( 5.515539859299206427, 0.004037661319611307587, 0.004509673239148500115 ) ) ;
#51141 = DIRECTION ( 'NONE',  ( 0.000000000000000000, 0.01356324068817992175, -0.9999080150203990547 ) ) ;
#51142 = CARTESIAN_POINT ( 'NONE',  ( 0.9232058338315048962, 7.723624854284715902, 9.791640253608173694 ) ) ;
#51143 = DIRECTION ( 'NONE',  ( 0.000000000000000000, 0.4935949184179200810, -0.8696919319575219243 ) ) ;
#51144 = B_SPLINE_CURVE_WITH_KNOTS ( 'NONE', 3,
 ( #62988, #17450, #37725, #12430, #48038, #2500, #22774, #19980, #28398, #23089, #65206, #50260, #30291, #7801, #43352, #3150, #13426, #4723, #63626 ),
 .UNSPECIFIED., .F., .F.,
 ( 4, 3, 3, 3, 3, 3, 4 ),
 ( 6.269651592512720910E-18, 2.825908398830553593E-05, 4.208813692483162199E-05, 5.591713746942991644E-05, 6.279584083230896894E-05, 9.105792820295216820E-05, 0.0001153131102488888472 ),
 .UNSPECIFIED. ) ;
#51145 = CARTESIAN_POINT ( 'NONE',  ( -35.00000000000000000, 11.61976888909158490, 3.827969819614505997 ) ) ;
#51146 = CIRCLE ( 'NONE', #61801, 12.75000000000000178 ) ;
#51147 = EDGE_CURVE ( 'NONE', #19224, #37445, #51217, .T. ) ;
#51148 = AXIS2_PLACEMENT_3D ( 'NONE', #30374, #50669, #35675 ) ;
#51149 = EDGE_LOOP ( 'NONE', ( #31203, #56851, #37739, #30744 ) ) ;
#51150 = CARTESIAN_POINT ( 'NONE',  ( 35.00000000000000000, 4.705694406421931860E-17, -3.469127814946512892E-15 ) ) ;
#51151 = CIRCLE ( 'NONE', #23513, 12.75000000000000178 ) ;
#51152 = VERTEX_POINT ( 'NONE', #19235 ) ;
#51153 = CARTESIAN_POINT ( 'NONE',  ( 0.2638984909335716500, 12.24571285024409129, 0.1991813963114414388 ) ) ;
#51154 = FACE_OUTER_BOUND ( 'NONE', #63188, .T. ) ;
#51155 = AXIS2_PLACEMENT_3D ( 'NONE', #23802, #55013, #19117 ) ;
#51156 = DIRECTION ( 'NONE',  ( 0.000000000000000000, 0.000000000000000000, 1.000000000000000000 ) ) ;
#51157 = CARTESIAN_POINT ( 'NONE',  ( 5.530133899448235191, 0.01324661008606589467, -0.008946569461392295600 ) ) ;
#51158 = ORIENTED_EDGE ( 'NONE', *, *, #42596, .T. ) ;
#51159 = DIRECTION ( 'NONE',  ( 1.000000000000000000, 0.000000000000000000, 0.000000000000000000 ) ) ;
#51161 = AXIS2_PLACEMENT_3D ( 'NONE', #26757, #47052, #12109 ) ;
#51160 = CARTESIAN_POINT ( 'NONE',  ( 35.00000000000000000, 2.021542716731571154, 12.01765980939839196 ) ) ;
#51162 = CARTESIAN_POINT ( 'NONE',  ( 3.152665057736256493, -0.9030954876717440793, 7.886634106564762270 ) ) ;
#51163 = DIRECTION ( 'NONE',  ( 1.000000000000000000, 0.000000000000000000, 0.000000000000000000 ) ) ;
#51164 = EDGE_CURVE ( 'NONE', #36886, #24124, #65736, .T. ) ;
#51165 = CARTESIAN_POINT ( 'NONE',  ( 10.47324744292499510, 7.645705331602621335, -11.12856369570244830 ) ) ;
#51166 = VECTOR ( 'NONE', #1888, 1000.000000000000000 ) ;
#51167 = CARTESIAN_POINT ( 'NONE',  ( -35.00000000000000000, -12.71517666308948513, 0.9416912585473978803 ) ) ;
#51168 = ORIENTED_EDGE ( 'NONE', *, *, #45580, .T. ) ;
#51169 = LINE ( 'NONE', #30851, #15846 ) ;
#51170 = AXIS2_PLACEMENT_3D ( 'NONE', #43499, #62476, #53174 ) ;
#51171 = ORIENTED_EDGE ( 'NONE', *, *, #59038, .F. ) ;
#51172 = AXIS2_PLACEMENT_3D ( 'NONE', #32648, #39876, #63571 ) ;
#51173 = CARTESIAN_POINT ( 'NONE',  ( 0.2650492433740075926, 12.24562113162318688, -0.1101179680249403520 ) ) ;
#51174 = LINE ( 'NONE', #37155, #22515 ) ;
#51175 = CARTESIAN_POINT ( 'NONE',  ( 35.00000000000000000, 11.72195762423409704, 0.7536123767498881243 ) ) ;
#51176 = CARTESIAN_POINT ( 'NONE',  ( 35.00000000000000000, 11.78745411414844035, 3.093009498343795460 ) ) ;
#51177 = EDGE_CURVE ( 'NONE', #3171, #3708, #42894, .T. ) ;
#51178 = VECTOR ( 'NONE', #57724, 1000.000000000000000 ) ;
#51179 = CIRCLE ( 'NONE', #36297, 12.75000000000000178 ) ;
#51180 = CIRCLE ( 'NONE', #56478, 4.000000000000000000 ) ;
#51181 = EDGE_LOOP ( 'NONE', ( #18017, #30612, #33878, #42592 ) ) ;
#51182 = VERTEX_POINT ( 'NONE', #9238 ) ;
#51183 = CARTESIAN_POINT ( 'NONE',  ( -29.72940237447408762, 1.708107138515393864, 11.88595848903394092 ) ) ;
#51184 = ORIENTED_EDGE ( 'NONE', *, *, #48222, .F. ) ;
#51185 = CARTESIAN_POINT ( 'NONE',  ( 2.241352910868909643, -6.569501556381414531, -3.889181972941518683 ) ) ;
#51186 = DIRECTION ( 'NONE',  ( -1.000000000000000000, 0.000000000000000000, 0.000000000000000000 ) ) ;
#51187 = DIRECTION ( 'NONE',  ( 0.000000000000000000, 0.000000000000000000, -1.000000000000000000 ) ) ;
#51188 = CARTESIAN_POINT ( 'NONE',  ( 1.948354844647008477, -10.97658859989599378, 4.761851831283274272 ) ) ;
#51189 = CARTESIAN_POINT ( 'NONE',  ( -35.00000000000000000, 8.839356091080043498, 8.389074212634319849 ) ) ;
#51190 = CARTESIAN_POINT ( 'NONE',  ( -35.00000000000000000, -8.029056188533626681, -8.573591947375405198 ) ) ;
#51191 = EDGE_LOOP ( 'NONE', ( #28913, #11761, #34915, #30874 ) ) ;
#51192 = CARTESIAN_POINT ( 'NONE',  ( 2.305787727787084407, -2.461236246751023593, -7.249469779319933416 ) ) ;
#51193 = EDGE_LOOP ( 'NONE', ( #60150, #50340, #7782, #16028 ) ) ;
#51194 = CARTESIAN_POINT ( 'NONE',  ( 8.937200413559436285, 4.816788486362209021, 12.61660635838017797 ) ) ;
#51195 = CIRCLE ( 'NONE', #2352, 12.74999999999999822 ) ;
#51196 = CARTESIAN_POINT ( 'NONE',  ( 0.3278977287071219715, 10.49733767381182759, 6.347150352417348707 ) ) ;
#51197 = CIRCLE ( 'NONE', #15048, 12.75000000000000178 ) ;
#51198 = CARTESIAN_POINT ( 'NONE',  ( -27.09150307427401927, 1.909742362149659867, -1.305148381378450351 ) ) ;
#51199 = ORIENTED_EDGE ( 'NONE', *, *, #49850, .T. ) ;
#51200 = B_SPLINE_CURVE_WITH_KNOTS ( 'NONE', 3,
 ( #52748, #5652, #22479, #27453, #5307, #25578, #45873 ),
 .UNSPECIFIED., .F., .F.,
 ( 4, 3, 4 ),
 ( 0.000000000000000000, 0.001700533616330527362, 0.005002426799371310386 ),
 .UNSPECIFIED. ) ;
#51201 = AXIS2_PLACEMENT_3D ( 'NONE', #19426, #34375, #49383 ) ;
#51202 = CARTESIAN_POINT ( 'NONE',  ( -22.27713295444592845, 3.580881989303326129, -0.8543895091636388717 ) ) ;
#51203 = EDGE_LOOP ( 'NONE', ( #9015, #10862, #31600, #37775 ) ) ;
#51204 = CARTESIAN_POINT ( 'NONE',  ( 37.00000000000000711, -4.400442035670863561, 11.96656215839372983 ) ) ;
#51205 = EDGE_CURVE ( 'NONE', #44528, #55692, #44659, .T. ) ;
#51206 = DIRECTION ( 'NONE',  ( -1.000000000000000000, -0.000000000000000000, -0.000000000000000000 ) ) ;
#51207 = CARTESIAN_POINT ( 'NONE',  ( 2.556980015513900639, 2.862731173723978451, 7.190718924764532005 ) ) ;
#51208 = CARTESIAN_POINT ( 'NONE',  ( 7.301893923874954062, -6.385938209748294625, 10.16239020806034432 ) ) ;
#51209 = ORIENTED_EDGE ( 'NONE', *, *, #42029, .F. ) ;
#51210 = AXIS2_PLACEMENT_3D ( 'NONE', #65248, #4419, #19717 ) ;
#51211 = VERTEX_POINT ( 'NONE', #14864 ) ;
#51212 = CARTESIAN_POINT ( 'NONE',  ( 2.573738926104374158, -6.822065037112458263, 3.667129335223178632 ) ) ;
#51213 = ADVANCED_FACE ( 'NONE', ( #274 ), #35152, .T. ) ;
#51214 = ORIENTED_EDGE ( 'NONE', *, *, #30666, .T. ) ;
#51215 = CARTESIAN_POINT ( 'NONE',  ( 1.372161826076674362, -12.04315837901297925, -3.755740169579745658 ) ) ;
#51216 = ORIENTED_EDGE ( 'NONE', *, *, #5099, .F. ) ;
#51217 = CIRCLE ( 'NONE', #55308, 12.18650000000000055 ) ;
#51218 = ORIENTED_EDGE ( 'NONE', *, *, #48249, .F. ) ;
#51219 = VERTEX_POINT ( 'NONE', #40482 ) ;
#51220 = CARTESIAN_POINT ( 'NONE',  ( 3.092491956585110113, -5.768471164323004885, 5.424230976134056803 ) ) ;
#51221 = LINE ( 'NONE', #21256, #6084 ) ;
#51222 = CYLINDRICAL_SURFACE ( 'NONE', #50129, 12.74999999999999822 ) ;
#51224 = EDGE_CURVE ( 'NONE', #30158, #17686, #35500, .T. ) ;
#51223 = CARTESIAN_POINT ( 'NONE',  ( 2.241352910868908754, 2.689314586382447914, -7.145045428366549878 ) ) ;
#51225 = CARTESIAN_POINT ( 'NONE',  ( -22.71097035706202405, -2.846599994298329328, 4.089776368546542251 ) ) ;
#51226 = ORIENTED_EDGE ( 'NONE', *, *, #37285, .T. ) ;
#51227 = DIRECTION ( 'NONE',  ( -0.6334066780386838902, 0.000000000000000000, -0.7738190875236917732 ) ) ;
#51228 = AXIS2_PLACEMENT_3D ( 'NONE', #52761, #22494, #42758 ) ;
#51229 = ORIENTED_EDGE ( 'NONE', *, *, #46880, .F. ) ;
#51230 = CARTESIAN_POINT ( 'NONE',  ( 37.00000000000000711, 4.705694406421931860E-17, -3.469127814946512892E-15 ) ) ;
#51231 = CARTESIAN_POINT ( 'NONE',  ( 0.000000000000000000, 5.769711778877384845, -4.791703871138491166 ) ) ;
#51232 = DIRECTION ( 'NONE',  ( 1.000000000000000000, 0.000000000000000000, -0.000000000000000000 ) ) ;
#51233 = CARTESIAN_POINT ( 'NONE',  ( -27.46772105850581980, 13.11490794829154005, -3.249960617400303509 ) ) ;
#51234 = CARTESIAN_POINT ( 'NONE',  ( 29.12484106848172161, 5.686051718212023154, 10.57743981609822903 ) ) ;
#51235 = CARTESIAN_POINT ( 'NONE',  ( 2.963017218115624019, -7.865565884553436860, -0.3847317984106120581 ) ) ;
#51236 = CIRCLE ( 'NONE', #36340, 12.75000000000000178 ) ;
#51237 = AXIS2_PLACEMENT_3D ( 'NONE', #2416, #32315, #12037 ) ;
#51238 = VECTOR ( 'NONE', #34822, 1000.000000000000000 ) ;
#51239 = ORIENTED_EDGE ( 'NONE', *, *, #42084, .T. ) ;
#51240 = CARTESIAN_POINT ( 'NONE',  ( -37.00000000000000711, 12.14284015767850100, 1.030638227056609679 ) ) ;
#51241 = ADVANCED_FACE ( 'NONE', ( #5254 ), #25520, .T. ) ;
#51242 = ORIENTED_EDGE ( 'NONE', *, *, #33124, .F. ) ;
#51243 = DIRECTION ( 'NONE',  ( -1.000000000000000000, 0.000000000000000000, 0.000000000000000000 ) ) ;
#51244 = CARTESIAN_POINT ( 'NONE',  ( 2.963017218115621354, 6.272673870919160954, -4.761166637500448218 ) ) ;
#51245 = CARTESIAN_POINT ( 'NONE',  ( 2.717984159219280826, 4.139692542159186139, 6.602931111513647089 ) ) ;
#51246 = CARTESIAN_POINT ( 'NONE',  ( -35.00000000000000000, -9.896810808925444292, 7.110831038798244741 ) ) ;
#51247 = EDGE_LOOP ( 'NONE', ( #10320, #60019, #41379, #53056, #61712, #34932 ) ) ;
#51248 = DIRECTION ( 'NONE',  ( 1.000000000000000000, 0.000000000000000000, 0.000000000000000000 ) ) ;
#51249 = LINE ( 'NONE', #10322, #50328 ) ;
#51250 = CARTESIAN_POINT ( 'NONE',  ( 21.76150723431516454, 10.89040160248869960, -5.054754920142551455 ) ) ;
#51251 = CARTESIAN_POINT ( 'NONE',  ( 2.373367633546869637, 3.681545031436654458, 6.738274194514227489 ) ) ;
#51252 = CIRCLE ( 'NONE', #59723, 5.000000000000001776 ) ;
#51253 = AXIS2_PLACEMENT_3D ( 'NONE', #31118, #17719, #15805 ) ;
#51254 = CARTESIAN_POINT ( 'NONE',  ( 0.2671309869109501078, 12.24572650704445032, -0.1620273132356114532 ) ) ;
#51255 = VECTOR ( 'NONE', #48195, 1000.000000000000000 ) ;
#51256 = CYLINDRICAL_SURFACE ( 'NONE', #44517, 5.000000000000000888 ) ;
#51257 = CARTESIAN_POINT ( 'NONE',  ( 0.3665391374699465965, -11.44911061034389732, 4.447929964102806721 ) ) ;
#51258 = CARTESIAN_POINT ( 'NONE',  ( 1.719304012338836563, -1.452142814150213734, 12.64775761152536759 ) ) ;
#51259 = DIRECTION ( 'NONE',  ( -1.000000000000000000, 0.000000000000000000, 0.000000000000000000 ) ) ;
#51260 = ADVANCED_FACE ( 'NONE', ( #15853 ), #18661, .F. ) ;
#51261 = ORIENTED_EDGE ( 'NONE', *, *, #55003, .F. ) ;
#51262 = ORIENTED_EDGE ( 'NONE', *, *, #12088, .F. ) ;
#51263 = CYLINDRICAL_SURFACE ( 'NONE', #40592, 15.00000000000000000 ) ;
#51264 = CARTESIAN_POINT ( 'NONE',  ( 38.94999461337799573, -1.999059167504507739, -19.54503265464387241 ) ) ;
#51265 = CYLINDRICAL_SURFACE ( 'NONE', #55539, 2.899999999999994582 ) ;
#51266 = CARTESIAN_POINT ( 'NONE',  ( -2.952869152607111136, 7.581333670610111319, 11.17020052527586138 ) ) ;
#51267 = ORIENTED_EDGE ( 'NONE', *, *, #3921, .F. ) ;
#51268 = B_SPLINE_CURVE_WITH_KNOTS ( 'NONE', 3,
 ( #58029, #12441, #47402, #47072, #2513, #17123, #26774, #37397, #1530, #32712, #57707, #47713, #21805, #22434, #53025, #42361 ),
 .UNSPECIFIED., .F., .F.,
 ( 4, 3, 3, 3, 3, 4 ),
 ( 2.788974592819220452E-15, 0.0002126834539179592873, 0.0004253519300366052653, 0.0006380165497223855980, 0.0007442707582427891952, 0.0009453531351420179241 ),
 .UNSPECIFIED. ) ;
#51269 = AXIS2_PLACEMENT_3D ( 'NONE', #50604, #14655, #19999 ) ;
#51270 = CIRCLE ( 'NONE', #45942, 5.000000000000000888 ) ;
#51271 = ORIENTED_EDGE ( 'NONE', *, *, #58759, .T. ) ;
#51272 = ORIENTED_EDGE ( 'NONE', *, *, #32366, .T. ) ;
#51273 = LINE ( 'NONE', #50933, #20632 ) ;
#51274 = VECTOR ( 'NONE', #57449, 1000.000000000000000 ) ;
#51276 = AXIS2_PLACEMENT_3D ( 'NONE', #49691, #55324, #39703 ) ;
#51275 = CARTESIAN_POINT ( 'NONE',  ( -22.27711351828769892, 0.8770428151440663456, 3.575417021793764416 ) ) ;
#51277 = EDGE_CURVE ( 'NONE', #23800, #36879, #10088, .T. ) ;
#51278 = ORIENTED_EDGE ( 'NONE', *, *, #39165, .T. ) ;
#51279 = FACE_OUTER_BOUND ( 'NONE', #28217, .T. ) ;
#51280 = CYLINDRICAL_SURFACE ( 'NONE', #13024, 12.18649999999999878 ) ;
#51281 = ORIENTED_EDGE ( 'NONE', *, *, #4760, .F. ) ;
#51282 =( BOUNDED_CURVE ( )  B_SPLINE_CURVE ( 3, ( #32948, #3059, #23321, #3733 ),
 .UNSPECIFIED., .F., .F. ) 
 B_SPLINE_CURVE_WITH_KNOTS ( ( 4, 4 ),
 ( 5.358943115472171392, 5.400987736605186385 ),
 .UNSPECIFIED. ) 
 CURVE ( )  GEOMETRIC_REPRESENTATION_ITEM ( )  RATIONAL_B_SPLINE_CURVE ( ( 1.000000000000000000, 0.9998526929113126238, 0.9998526929113126238, 1.000000000000000000 ) ) 
 REPRESENTATION_ITEM ( '' )  );
#51283 = CARTESIAN_POINT ( 'NONE',  ( 2.251152103364163271, 4.812779263774475957, -5.930529991878751517 ) ) ;
#51284 = EDGE_CURVE ( 'NONE', #36860, #32235, #15998, .T. ) ;
#51285 = CARTESIAN_POINT ( 'NONE',  ( 14.27815883903287464, -30.09651741059179031, -4.806648824294282640 ) ) ;
#51286 = CARTESIAN_POINT ( 'NONE',  ( 0.2638984909335720941, -10.50550771760524249, 6.295352574288949121 ) ) ;
#51287 = ORIENTED_EDGE ( 'NONE', *, *, #2086, .F. ) ;
#51288 = CARTESIAN_POINT ( 'NONE',  ( 2.000000000000001776, -6.777474576704058506, 0.6925993764990423518 ) ) ;
#51289 = EDGE_CURVE ( 'NONE', #60763, #64737, #53190, .T. ) ;
#51290 = VERTEX_POINT ( 'NONE', #26504 ) ;
#51291 = FACE_OUTER_BOUND ( 'NONE', #38487, .T. ) ;
#51292 = ORIENTED_EDGE ( 'NONE', *, *, #49553, .F. ) ;
#51293 = DIRECTION ( 'NONE',  ( -1.000000000000000000, 0.000000000000000000, 0.000000000000000000 ) ) ;
#51294 = CARTESIAN_POINT ( 'NONE',  ( -1.754394376698012570, -31.09667363889180791, 14.37851519254956756 ) ) ;
#51295 = CARTESIAN_POINT ( 'NONE',  ( -37.00000000000000711, 0.000000000000000000, 0.000000000000000000 ) ) ;
#51296 = VECTOR ( 'NONE', #20591, 1000.000000000000000 ) ;
#51297 = DIRECTION ( 'NONE',  ( -1.000000000000000000, -0.000000000000000000, -0.000000000000000000 ) ) ;
#51298 = DIRECTION ( 'NONE',  ( 0.000000000000000000, 0.000000000000000000, 1.000000000000000000 ) ) ;
#51300 = EDGE_CURVE ( 'NONE', #21470, #22647, #2258, .T. ) ;
#51299 = DIRECTION ( 'NONE',  ( 1.000000000000000000, -0.000000000000000000, 0.000000000000000000 ) ) ;
#51301 = DIRECTION ( 'NONE',  ( 1.000000000000000000, 0.000000000000000000, -0.000000000000000000 ) ) ;
#51302 = CARTESIAN_POINT ( 'NONE',  ( 9.088549504245943211, 6.815555982525443923, -9.878547223985661319 ) ) ;
#51304 = EDGE_LOOP ( 'NONE', ( #11741, #13769, #15491, #64226 ) ) ;
#51303 = DIRECTION ( 'NONE',  ( 0.000000000000000000, -0.9937233664769749009, 0.1118654143051720229 ) ) ;
#51305 = CARTESIAN_POINT ( 'NONE',  ( -37.00000000000000711, 10.14433819232434253, 6.753013023069750709 ) ) ;
#51306 = ORIENTED_EDGE ( 'NONE', *, *, #56208, .F. ) ;
#51307 = CARTESIAN_POINT ( 'NONE',  ( 0.3278977287071205282, -4.427879319182963513, 11.44003061923229225 ) ) ;
#51308 = EDGE_CURVE ( 'NONE', #8903, #332, #48977, .T. ) ;
#51309 = CIRCLE ( 'NONE', #4593, 4.999999999999999112 ) ;
#51310 = DIRECTION ( 'NONE',  ( -1.000000000000000000, 0.000000000000000000, 0.000000000000000000 ) ) ;
#51311 = ORIENTED_EDGE ( 'NONE', *, *, #7691, .F. ) ;
#51312 = CARTESIAN_POINT ( 'NONE',  ( 0.4613984246114876120, -12.30830943644279962, 0.2828900474739950432 ) ) ;
#51313 = CARTESIAN_POINT ( 'NONE',  ( 1.198791140420743639, 11.96656299555157688, -3.806343609710548304 ) ) ;
#51314 = CARTESIAN_POINT ( 'NONE',  ( 35.00000000000000000, -6.036400161834636791, -10.07641281632175634 ) ) ;
#51315 = FACE_OUTER_BOUND ( 'NONE', #13616, .T. ) ;
#51316 = CARTESIAN_POINT ( 'NONE',  ( 35.00000000000000000, -5.814360711498364864, -10.70999494708490829 ) ) ;
#51317 = ORIENTED_EDGE ( 'NONE', *, *, #11714, .T. ) ;
#51318 = DIRECTION ( 'NONE',  ( 1.000000000000000000, -0.000000000000000000, 0.000000000000000000 ) ) ;
#51319 = ADVANCED_FACE ( 'NONE', ( #10890 ), #51487, .T. ) ;
#51320 = ORIENTED_EDGE ( 'NONE', *, *, #36603, .T. ) ;
#51321 = CARTESIAN_POINT ( 'NONE',  ( 2.907497136249980407, 0.3592423305251248866, 7.848280798452631046 ) ) ;
#51322 = EDGE_CURVE ( 'NONE', #17416, #9772, #21186, .T. ) ;
#51323 = FACE_OUTER_BOUND ( 'NONE', #62839, .T. ) ;
#51324 = CARTESIAN_POINT ( 'NONE',  ( -37.00000000000000711, 0.000000000000000000, 0.000000000000000000 ) ) ;
#51325 = EDGE_LOOP ( 'NONE', ( #53597, #36794, #29719, #60560 ) ) ;
#51326 = AXIS2_PLACEMENT_3D ( 'NONE', #58547, #17967, #53561 ) ;
#51327 = AXIS2_PLACEMENT_3D ( 'NONE', #23812, #22820, #54395 ) ;
#51328 = CARTESIAN_POINT ( 'NONE',  ( -35.00000000000000000, -11.65150730582933392, -1.488153103997089888 ) ) ;
#51329 = AXIS2_PLACEMENT_3D ( 'NONE', #3018, #23279, #49550 ) ;
#51330 = DIRECTION ( 'NONE',  ( -1.000000000000000000, 0.000000000000000000, 0.000000000000000000 ) ) ;
#51331 = LINE ( 'NONE', #40998, #52178 ) ;
#51332 = CARTESIAN_POINT ( 'NONE',  ( 2.000000000000001776, -6.812627895098285258, -0.04423456934733380197 ) ) ;
#51333 = CARTESIAN_POINT ( 'NONE',  ( 9.883521448361594963, 7.802028015148476214, 11.02197474982682124 ) ) ;
#51334 = CARTESIAN_POINT ( 'NONE',  ( 0.2653141617321005952, 2.169890202573355520, -12.05243138604823905 ) ) ;
#51335 = CARTESIAN_POINT ( 'NONE',  ( 13.29259107886818647, -33.36832009551446987, 10.54479676545775035 ) ) ;
#51336 = DIRECTION ( 'NONE',  ( -1.000000000000000000, 0.000000000000000000, 0.000000000000000000 ) ) ;
#51337 = AXIS2_PLACEMENT_3D ( 'NONE', #17632, #12607, #62832 ) ;
#51338 = EDGE_CURVE ( 'NONE', #24646, #54088, #32511, .T. ) ;
#51339 = ORIENTED_EDGE ( 'NONE', *, *, #4391, .F. ) ;
#51340 = CARTESIAN_POINT ( 'NONE',  ( -16.78077304548816429, 7.535057906616318135, 11.20259948750489976 ) ) ;
#51341 = CARTESIAN_POINT ( 'NONE',  ( 17.36552780755588543, -11.88930279851165928, 6.437067910676037563 ) ) ;
#51342 = AXIS2_PLACEMENT_3D ( 'NONE', #59280, #23372, #12390 ) ;
#51343 = ORIENTED_EDGE ( 'NONE', *, *, #30588, .F. ) ;
#51344 = ADVANCED_FACE ( 'NONE', ( #30398 ), #32981, .T. ) ;
#51345 = CARTESIAN_POINT ( 'NONE',  ( 1.719304012338210619, 10.62216384465585328, 7.017415949611872428 ) ) ;
#51346 = CYLINDRICAL_SURFACE ( 'NONE', #14083, 12.18650000000000055 ) ;
#51347 = AXIS2_PLACEMENT_3D ( 'NONE', #25946, #60859, #36219 ) ;
#51348 = CARTESIAN_POINT ( 'NONE',  ( -22.27706485742869091, 3.563814065926677710, -0.9221835209182235316 ) ) ;
#51349 = ORIENTED_EDGE ( 'NONE', *, *, #42329, .F. ) ;
#51350 = CARTESIAN_POINT ( 'NONE',  ( -17.68824251889582655, 2.869235522687681339, 11.65378641629914647 ) ) ;
#51351 = LINE ( 'NONE', #31677, #187 ) ;
#51352 = VERTEX_POINT ( 'NONE', #29026 ) ;
#51353 = ADVANCED_FACE ( 'NONE', ( #48995 ), #3452, .T. ) ;
#51354 = ORIENTED_EDGE ( 'NONE', *, *, #65168, .T. ) ;
#51355 = ORIENTED_EDGE ( 'NONE', *, *, #31828, .F. ) ;
#51356 = CARTESIAN_POINT ( 'NONE',  ( 145.1370849898475797, 3.309064568108273190E-14, 0.000000000000000000 ) ) ;
#51357 = VECTOR ( 'NONE', #54952, 1000.000000000000000 ) ;
#51358 = EDGE_CURVE ( 'NONE', #37217, #50194, #42567, .T. ) ;
#51359 = ORIENTED_EDGE ( 'NONE', *, *, #31378, .T. ) ;
#51360 = LINE ( 'NONE', #15426, #55723 ) ;
#51361 = CARTESIAN_POINT ( 'NONE',  ( 0.5572780756287500914, -11.49107179558554748, -4.507550621618535480 ) ) ;
#51362 = CARTESIAN_POINT ( 'NONE',  ( -35.00000000000000000, -8.235637554476575417, -9.733281772932249609 ) ) ;
#51363 = DIRECTION ( 'NONE',  ( 1.000000000000000000, -0.000000000000000000, 0.000000000000000000 ) ) ;
#51364 = VERTEX_POINT ( 'NONE', #23722 ) ;
#51365 = LINE ( 'NONE', #16431, #21540 ) ;
#51366 = CARTESIAN_POINT ( 'NONE',  ( 0.8805962972398279076, -27.81433265277922828, 12.58259205803954828 ) ) ;
#51367 = CARTESIAN_POINT ( 'NONE',  ( 3.152665057736217413, -7.923639299008909731, 0.4801242025612903475 ) ) ;
#51368 = ORIENTED_EDGE ( 'NONE', *, *, #49573, .F. ) ;
#51369 = B_SPLINE_CURVE_WITH_KNOTS ( 'NONE', 3,
 ( #34221, #65134, #49542, #55157 ),
 .UNSPECIFIED., .F., .F.,
 ( 4, 4 ),
 ( 0.000000000000000000, 0.002277974501771297573 ),
 .UNSPECIFIED. ) ;
#51370 = CARTESIAN_POINT ( 'NONE',  ( -22.31328051695926007, -3.685074213229319717, -0.8849444482788241251 ) ) ;
#51371 = EDGE_CURVE ( 'NONE', #14741, #16694, #38988, .T. ) ;
#51372 = ORIENTED_EDGE ( 'NONE', *, *, #14573, .F. ) ;
#51373 = AXIS2_PLACEMENT_3D ( 'NONE', #65513, #5699, #50261 ) ;
#51374 = CARTESIAN_POINT ( 'NONE',  ( 2.000000000000001776, 3.155844197800189210, -6.177028383390422484 ) ) ;
#51375 = ORIENTED_EDGE ( 'NONE', *, *, #32647, .T. ) ;
#51376 = AXIS2_PLACEMENT_3D ( 'NONE', #18422, #58991, #13402 ) ;
#51377 = EDGE_LOOP ( 'NONE', ( #27386, #52834, #21907, #31929 ) ) ;
#51378 = CARTESIAN_POINT ( 'NONE',  ( 2.000000000000001776, -4.962980376314023445, -4.846014654777856201 ) ) ;
#51379 = CARTESIAN_POINT ( 'NONE',  ( 3.616736114193262353, -30.77385512440581650, 15.02426791487729218 ) ) ;
#51381 = LINE ( 'NONE', #22067, #35384 ) ;
#51380 = CIRCLE ( 'NONE', #36494, 5.000000000000000888 ) ;
#51382 = ORIENTED_EDGE ( 'NONE', *, *, #53609, .F. ) ;
#51383 = DIRECTION ( 'NONE',  ( 1.000000000000000000, -0.000000000000000000, 0.000000000000000000 ) ) ;
#51384 = CARTESIAN_POINT ( 'NONE',  ( 0.3610902822527207734, -12.04327049858141763, 2.389900346488049721 ) ) ;
#51385 = ORIENTED_EDGE ( 'NONE', *, *, #28156, .T. ) ;
#51386 = ORIENTED_EDGE ( 'NONE', *, *, #48523, .F. ) ;
#51387 = CARTESIAN_POINT ( 'NONE',  ( 0.3002738374340830352, 12.03040002643111706, 2.350339881554986743 ) ) ;
#51388 = EDGE_LOOP ( 'NONE', ( #27941, #16382, #7114, #51546 ) ) ;
#51389 = EDGE_CURVE ( 'NONE', #27863, #45739, #55364, .T. ) ;
#51390 = AXIS2_PLACEMENT_3D ( 'NONE', #46553, #25960, #20640 ) ;
#51391 = ADVANCED_FACE ( 'NONE', ( #43988 ), #64262, .T. ) ;
#51392 = ORIENTED_EDGE ( 'NONE', *, *, #38434, .T. ) ;
#51393 = VECTOR ( 'NONE', #6837, 1000.000000000000000 ) ;
#51394 = DIRECTION ( 'NONE',  ( 0.000000000000000000, 0.000000000000000000, -1.000000000000000000 ) ) ;
#51395 = CARTESIAN_POINT ( 'NONE',  ( 1.633930747251797211, -10.62371422070957117, 6.963441708413805387 ) ) ;
#51396 = DIRECTION ( 'NONE',  ( 1.000000000000000000, 0.000000000000000000, 0.000000000000000000 ) ) ;
#51397 = CARTESIAN_POINT ( 'NONE',  ( 17.53254851291653438, -7.812843716768262503, 9.123340610460312305 ) ) ;
#51398 = EDGE_CURVE ( 'NONE', #26437, #22263, #22732, .T. ) ;
#51399 = VECTOR ( 'NONE', #144, 1000.000000000000000 ) ;
#51400 = CARTESIAN_POINT ( 'NONE',  ( 2.000000000000001776, -4.472310526050724100, -6.020667617347421618 ) ) ;
#51401 = EDGE_CURVE ( 'NONE', #60526, #45531, #38366, .T. ) ;
#51402 = DIRECTION ( 'NONE',  ( 1.000000000000000000, 0.000000000000000000, 0.000000000000000000 ) ) ;
#51403 = CIRCLE ( 'NONE', #63042, 12.18649999999999878 ) ;
#51404 = EDGE_LOOP ( 'NONE', ( #12095, #9723, #60826, #5737 ) ) ;
#51405 = VECTOR ( 'NONE', #36124, 1000.000000000000000 ) ;
#51406 = EDGE_CURVE ( 'NONE', #26022, #43321, #19250, .T. ) ;
#51407 = CARTESIAN_POINT ( 'NONE',  ( 0.000000000000000000, 0.000000000000000000, 0.000000000000000000 ) ) ;
#51408 = CARTESIAN_POINT ( 'NONE',  ( 2.241352910868909643, 7.503490710578251566, -1.407733736974789762 ) ) ;
#51409 = CARTESIAN_POINT ( 'NONE',  ( -22.28506771379528573, 3.348518833762387459, 1.636577531579554545 ) ) ;
#51410 = DIRECTION ( 'NONE',  ( 0.000000000000000000, -0.01356324068817998940, 0.9999080150203990547 ) ) ;
#51411 = CIRCLE ( 'NONE', #9942, 7.499999999999988454 ) ;
#51412 = CARTESIAN_POINT ( 'NONE',  ( -22.65996813707689839, 2.220979297960725685, 4.292955455498893791 ) ) ;
#51413 = CARTESIAN_POINT ( 'NONE',  ( 35.00000000000000000, -11.73463472867578083, -3.287724142101374092 ) ) ;
#51414 = CARTESIAN_POINT ( 'NONE',  ( 3.986618437605343512, 6.992948023114762712, -9.794201124374950496 ) ) ;
#51415 = FACE_OUTER_BOUND ( 'NONE', #32145, .T. ) ;
#51416 = ORIENTED_EDGE ( 'NONE', *, *, #41297, .T. ) ;
#51417 = AXIS2_PLACEMENT_3D ( 'NONE', #65695, #9858, #14822 ) ;
#51418 = CARTESIAN_POINT ( 'NONE',  ( -27.35552965826137140, 2.548625910254547655, 1.773915698030531951 ) ) ;
#51419 = CARTESIAN_POINT ( 'NONE',  ( 3.031336079629849412, 0.9593005538805465804, -7.839300734793278380 ) ) ;
#51420 = CIRCLE ( 'NONE', #11058, 5.000000000000000888 ) ;
#51421 = DIRECTION ( 'NONE',  ( -1.000000000000000000, 0.000000000000000000, 0.000000000000000000 ) ) ;
#51422 = AXIS2_PLACEMENT_3D ( 'NONE', #37405, #31114, #6843 ) ;
#51423 = EDGE_CURVE ( 'NONE', #23040, #6900, #54287, .T. ) ;
#51424 = CARTESIAN_POINT ( 'NONE',  ( 5.514970785353741078, 0.004324946436530305478, -0.001897634820904966005 ) ) ;
#51425 = LINE ( 'NONE', #5537, #50027 ) ;
#51426 = CIRCLE ( 'NONE', #1497, 12.75000000000000178 ) ;
#51427 = ORIENTED_EDGE ( 'NONE', *, *, #4328, .F. ) ;
#51428 = CARTESIAN_POINT ( 'NONE',  ( -17.36985044138108947, -8.809625639090254978, -10.23436652272288505 ) ) ;
#51429 = CARTESIAN_POINT ( 'NONE',  ( 0.2648978790185593790, -4.312320170909161199, -11.46165506714232762 ) ) ;
#51430 = CARTESIAN_POINT ( 'NONE',  ( 2.262775599886258426, 1.187656132455270352, 7.548684916004837042 ) ) ;
#51431 = VERTEX_POINT ( 'NONE', #23625 ) ;
#51432 = CARTESIAN_POINT ( 'NONE',  ( -37.00000000000000711, -8.954052073409537016, -9.076753354954096409 ) ) ;
#51433 = CARTESIAN_POINT ( 'NONE',  ( -37.00000000000000711, 7.817492529713987004, -9.348667969174327297 ) ) ;
#51434 = AXIS2_PLACEMENT_3D ( 'NONE', #56716, #41717, #10800 ) ;
#51435 = EDGE_CURVE ( 'NONE', #9266, #14210, #29359, .T. ) ;
#51437 = VERTEX_POINT ( 'NONE', #63501 ) ;
#51436 = DIRECTION ( 'NONE',  ( 1.000000000000000000, -0.000000000000000000, 0.000000000000000000 ) ) ;
#51438 = CARTESIAN_POINT ( 'NONE',  ( 35.00000000000000000, -10.91536515067650903, -4.339012074899918581 ) ) ;
#51439 = VECTOR ( 'NONE', #48341, 1000.000000000000000 ) ;
#51440 = CYLINDRICAL_SURFACE ( 'NONE', #36107, 5.000000000000000888 ) ;
#51441 = ORIENTED_EDGE ( 'NONE', *, *, #8111, .F. ) ;
#51442 = FACE_OUTER_BOUND ( 'NONE', #21542, .T. ) ;
#51443 = FACE_OUTER_BOUND ( 'NONE', #48194, .T. ) ;
#51444 = CARTESIAN_POINT ( 'NONE',  ( -35.00000000000000000, 0.000000000000000000, 0.000000000000000000 ) ) ;
#51445 = DIRECTION ( 'NONE',  ( 1.000000000000000000, -0.000000000000000000, 0.000000000000000000 ) ) ;
#51446 = CARTESIAN_POINT ( 'NONE',  ( -9.721193118338453232, 9.581699509156610617, -7.227512093013982231 ) ) ;
#51447 = VECTOR ( 'NONE', #4067, 1000.000000000000000 ) ;
#51448 = CARTESIAN_POINT ( 'NONE',  ( 2.241352910868908310, 2.532612177304540246, -7.202080440908716241 ) ) ;
#51450 = ORIENTED_EDGE ( 'NONE', *, *, #37587, .T. ) ;
#51449 = CARTESIAN_POINT ( 'NONE',  ( 0.6473888112830248343, 0.3298838684458830772, 12.36914475328377883 ) ) ;
#51451 = ADVANCED_FACE ( 'NONE', ( #13619 ), #64837, .F. ) ;
#51452 = ORIENTED_EDGE ( 'NONE', *, *, #52702, .F. ) ;
#51453 = CARTESIAN_POINT ( 'NONE',  ( -35.00000000000000000, -8.573591947375380329, 8.029056188533655103 ) ) ;
#51454 = EDGE_LOOP ( 'NONE', ( #19120, #46849, #32494, #32308 ) ) ;
#51455 = ADVANCED_FACE ( 'NONE', ( #27954 ), #63190, .T. ) ;
#51456 = CARTESIAN_POINT ( 'NONE',  ( 0.000000000000000000, -6.441884263200848615, 2.217201541069723891 ) ) ;
#51457 = DIRECTION ( 'NONE',  ( 0.000000000000000000, -0.8009703041134103030, -0.5987040770935764256 ) ) ;
#51458 = CIRCLE ( 'NONE', #41835, 5.000000000000000888 ) ;
#51459 = CYLINDRICAL_SURFACE ( 'NONE', #1257, 4.999999999999999112 ) ;
#51460 = EDGE_LOOP ( 'NONE', ( #57116, #52361, #21325, #54559 ) ) ;
#51461 = CYLINDRICAL_SURFACE ( 'NONE', #15960, 4.999999999999999112 ) ;
#51462 = DIRECTION ( 'NONE',  ( 0.000000000000000000, -0.01356324068817992175, 0.9999080150203990547 ) ) ;
#51463 = CYLINDRICAL_SURFACE ( 'NONE', #28689, 4.999999999999998224 ) ;
#51464 = ORIENTED_EDGE ( 'NONE', *, *, #59107, .T. ) ;
#51465 = VERTEX_POINT ( 'NONE', #18315 ) ;
#51466 = CARTESIAN_POINT ( 'NONE',  ( -8.891032880924177206, 25.00000000000000000, -3.860857758255646921 ) ) ;
#51467 = AXIS2_PLACEMENT_3D ( 'NONE', #52661, #32017, #1786 ) ;
#51468 = AXIS2_PLACEMENT_3D ( 'NONE', #36080, #22117, #11170 ) ;
#51469 = VERTEX_POINT ( 'NONE', #43897 ) ;
#51470 = CYLINDRICAL_SURFACE ( 'NONE', #38050, 12.75000000000000178 ) ;
#51471 = B_SPLINE_CURVE_WITH_KNOTS ( 'NONE', 3,
 ( #36706, #6454, #41693, #12083, #7098, #46363, #57003 ),
 .UNSPECIFIED., .F., .F.,
 ( 4, 3, 4 ),
 ( 0.000000000000000000, 0.001700533616330566176, 0.005002426799371234925 ),
 .UNSPECIFIED. ) ;
#51472 = CARTESIAN_POINT ( 'NONE',  ( -35.00000000000000000, 3.614449339633491576, 11.17622378668007777 ) ) ;
#51473 = CARTESIAN_POINT ( 'NONE',  ( 2.000000000000001776, 0.000000000000000000, 0.000000000000000000 ) ) ;
#51474 = EDGE_CURVE ( 'NONE', #49268, #46959, #3320, .T. ) ;
#51475 = DIRECTION ( 'NONE',  ( 1.000000000000000000, 0.000000000000000000, 0.000000000000000000 ) ) ;
#51476 = DIRECTION ( 'NONE',  ( 0.000000000000000000, 0.000000000000000000, -1.000000000000000000 ) ) ;
#51477 = DIRECTION ( 'NONE',  ( 0.3865475372811021382, -0.5778504531711042835, -0.7187975063895702954 ) ) ;
#51478 = EDGE_CURVE ( 'NONE', #3297, #25143, #13944, .T. ) ;
#51479 = CARTESIAN_POINT ( 'NONE',  ( 2.259830038564999644, 7.499347412930722712, 1.462175769136871750 ) ) ;
#51480 = EDGE_LOOP ( 'NONE', ( #21487, #7084, #49698, #26902 ) ) ;
#51481 = CARTESIAN_POINT ( 'NONE',  ( 1.633930747250413207, 12.68212725188695877, -0.7186603069030271795 ) ) ;
#51482 = EDGE_CURVE ( 'NONE', #21758, #47524, #40443, .T. ) ;
#51483 = CARTESIAN_POINT ( 'NONE',  ( 21.94787173280690240, 11.49320247778055837, -3.471189377931829245 ) ) ;
#51484 = CARTESIAN_POINT ( 'NONE',  ( -27.25047371082987624, 12.34411773464382023, 5.468532507261041786 ) ) ;
#51485 = CARTESIAN_POINT ( 'NONE',  ( 35.00000000000000000, 4.705694406421931860E-17, -3.469127814946512892E-15 ) ) ;
#51486 = CARTESIAN_POINT ( 'NONE',  ( -2.816255946208524374, 7.711081843936713476, 11.08213906273406657 ) ) ;
#51487 = CYLINDRICAL_SURFACE ( 'NONE', #63799, 4.999999999999999112 ) ;
#51488 = DIRECTION ( 'NONE',  ( 0.000000000000000000, 0.6269146997507987207, 0.7790879021242504976 ) ) ;
#51489 = CARTESIAN_POINT ( 'NONE',  ( 5.515539859299206427, 0.003193223631738807775, -0.005142293699651648287 ) ) ;
#51490 = CIRCLE ( 'NONE', #46159, 12.75000000000000178 ) ;
#51491 = VERTEX_POINT ( 'NONE', #58211 ) ;
#51492 = ORIENTED_EDGE ( 'NONE', *, *, #59003, .T. ) ;
#51493 = CARTESIAN_POINT ( 'NONE',  ( -36.00000000000000711, -3.307597835713157242, -12.31350058095526911 ) ) ;
#51494 = ADVANCED_FACE ( 'NONE', ( #13310 ), #28595, .T. ) ;
#51495 =( BOUNDED_CURVE ( )  B_SPLINE_CURVE ( 3, ( #65088, #15206, #15528, #30179 ),
 .UNSPECIFIED., .F., .F. ) 
 B_SPLINE_CURVE_WITH_KNOTS ( ( 4, 4 ),
 ( 2.185177278367677278, 2.228289365106483899 ),
 .UNSPECIFIED. ) 
 CURVE ( )  GEOMETRIC_REPRESENTATION_ITEM ( )  RATIONAL_B_SPLINE_CURVE ( ( 1.000000000000000000, 0.9998451183288734612, 0.9998451183288734612, 1.000000000000000000 ) ) 
 REPRESENTATION_ITEM ( '' )  );
#51496 = VERTEX_POINT ( 'NONE', #2711 ) ;
#51497 = CARTESIAN_POINT ( 'NONE',  ( -22.31099767395441091, -3.774495463598469769, 0.2534174342804084712 ) ) ;
#51498 = CARTESIAN_POINT ( 'NONE',  ( 0.3675815128205894289, -9.574637318041910206, -7.689697408877373519 ) ) ;
#51499 = CARTESIAN_POINT ( 'NONE',  ( 2.263328370261319389, 2.479726736363932371, -7.228205514767005901 ) ) ;
#51500 = ORIENTED_EDGE ( 'NONE', *, *, #51586, .F. ) ;
#51501 = CARTESIAN_POINT ( 'NONE',  ( -22.27834755396594346, 2.876353066242391510, -2.305389312780934841 ) ) ;
#51502 = DIRECTION ( 'NONE',  ( 0.000000000000000000, 0.000000000000000000, 1.000000000000000000 ) ) ;
#51503 = CARTESIAN_POINT ( 'NONE',  ( 2.969415267404973413, -0.9841783286029112121, 7.815364626284227789 ) ) ;
#51504 = CARTESIAN_POINT ( 'NONE',  ( -22.65996813707688418, 4.069902221062769776, 2.607318832796647445 ) ) ;
#51505 = CARTESIAN_POINT ( 'NONE',  ( 8.990732662897594096, 5.150069606959243096, -12.48035402102856217 ) ) ;
#51506 = EDGE_CURVE ( 'NONE', #64097, #54202, #20291, .T. ) ;
#51507 = LINE ( 'NONE', #10567, #54207 ) ;
#51508 = VERTEX_POINT ( 'NONE', #64181 ) ;
#51509 = DIRECTION ( 'NONE',  ( -1.000000000000000000, 0.000000000000000000, 0.000000000000000000 ) ) ;
#51510 = ORIENTED_EDGE ( 'NONE', *, *, #53472, .T. ) ;
#51511 = CARTESIAN_POINT ( 'NONE',  ( -37.00000000000000711, 4.400442035671113139, -11.96656215839364457 ) ) ;
#51512 = DIRECTION ( 'NONE',  ( -1.000000000000000000, 0.000000000000000000, 0.000000000000000000 ) ) ;
#51513 = CARTESIAN_POINT ( 'NONE',  ( 1.948354844647012696, -11.63671644762473179, 2.783443994771382712 ) ) ;
#51514 = CIRCLE ( 'NONE', #63166, 5.000000000000000888 ) ;
#51515 = CYLINDRICAL_SURFACE ( 'NONE', #17959, 4.999999999999999112 ) ;
#51516 = DIRECTION ( 'NONE',  ( 1.000000000000000000, 0.000000000000000000, 0.000000000000000000 ) ) ;
#51517 = ORIENTED_EDGE ( 'NONE', *, *, #62290, .F. ) ;
#51518 = ORIENTED_EDGE ( 'NONE', *, *, #30546, .T. ) ;
#51519 = CARTESIAN_POINT ( 'NONE',  ( 5.514970785353741078, 0.003262412238248714284, 0.003415090918276149530 ) ) ;
#51520 = B_SPLINE_CURVE_WITH_KNOTS ( 'NONE', 3,
 ( #31313, #61895, #6061, #27618, #36286, #51615, #37271, #56592, #26319, #21679, #32282, #57914, #22657, #26645, #6376, #1721, #1057, #63202, #1399 ),
 .UNSPECIFIED., .F., .F.,
 ( 4, 3, 3, 3, 3, 3, 4 ),
 ( 8.396094104928349784E-18, 4.457896483014532217E-05, 6.639290541541883822E-05, 8.820687556478810042E-05, 0.0001100173248778926955, 0.0001545671401658162494, 0.0001830328308068598778 ),
 .UNSPECIFIED. ) ;
#51521 = ORIENTED_EDGE ( 'NONE', *, *, #40315, .F. ) ;
#51522 = DIRECTION ( 'NONE',  ( 0.000000000000000000, 0.000000000000000000, 1.000000000000000000 ) ) ;
#51524 = CIRCLE ( 'NONE', #580, 7.499999999999988454 ) ;
#51523 = CARTESIAN_POINT ( 'NONE',  ( -22.27834755396594346, 3.497967921180563877, 1.162947663292818623 ) ) ;
#51525 = LINE ( 'NONE', #40186, #35182 ) ;
#51526 = CARTESIAN_POINT ( 'NONE',  ( -28.66013792860432119, -1.306994062650338684, 1.289369452666812244 ) ) ;
#51527 = CARTESIAN_POINT ( 'NONE',  ( -35.00000000000000000, 0.000000000000000000, 0.000000000000000000 ) ) ;
#51528 = CARTESIAN_POINT ( 'NONE',  ( 1.634816307077890052, 11.34285134320936805, -5.718391684265558439 ) ) ;
#51529 = CARTESIAN_POINT ( 'NONE',  ( -5.883084918421578990, -0.9869286070152175627, 11.95978564732913974 ) ) ;
#51530 = ORIENTED_EDGE ( 'NONE', *, *, #41222, .F. ) ;
#51531 = ADVANCED_FACE ( 'NONE', ( #33908 ), #18653, .T. ) ;
#51532 = EDGE_CURVE ( 'NONE', #27983, #23644, #28933, .T. ) ;
#51533 = DIRECTION ( 'NONE',  ( -1.000000000000000000, 0.000000000000000000, 0.000000000000000000 ) ) ;
#51534 = ORIENTED_EDGE ( 'NONE', *, *, #46840, .T. ) ;
#51535 = EDGE_CURVE ( 'NONE', #23349, #33895, #10259, .T. ) ;
#51537 = CARTESIAN_POINT ( 'NONE',  ( 21.90174657591892071, -13.47998113580522528, -0.7349207973210680755 ) ) ;
#51536 = CIRCLE ( 'NONE', #12196, 2.899999999999994582 ) ;
#51538 = DIRECTION ( 'NONE',  ( -1.000000000000000000, 0.000000000000000000, 0.000000000000000000 ) ) ;
#51539 = ORIENTED_EDGE ( 'NONE', *, *, #11386, .T. ) ;
#51540 = CARTESIAN_POINT ( 'NONE',  ( -14.53304282576173279, -30.00000000000001066, 3.713578627762639250 ) ) ;
#51541 = VERTEX_POINT ( 'NONE', #34237 ) ;
#51542 = FACE_OUTER_BOUND ( 'NONE', #61469, .T. ) ;
#51543 = CARTESIAN_POINT ( 'NONE',  ( 5.516018279890452902, -0.005976902763918694010, -0.003191189039764501679 ) ) ;
#51544 = CARTESIAN_POINT ( 'NONE',  ( 2.907497136250803749, 3.021847490615692688, 7.252103438786950740 ) ) ;
#51545 = CARTESIAN_POINT ( 'NONE',  ( -28.14317553103693825, -3.466682545733132059, 23.84441711261399632 ) ) ;
#51546 = ORIENTED_EDGE ( 'NONE', *, *, #35849, .F. ) ;
#51547 = VERTEX_POINT ( 'NONE', #60829 ) ;
#51548 = CARTESIAN_POINT ( 'NONE',  ( -35.00000000000000000, 0.000000000000000000, 0.000000000000000000 ) ) ;
#51549 = ORIENTED_EDGE ( 'NONE', *, *, #1635, .F. ) ;
#51550 = DIRECTION ( 'NONE',  ( 0.000000000000000000, -0.01356324068817998940, 0.9999080150203990547 ) ) ;
#51551 = ORIENTED_EDGE ( 'NONE', *, *, #4975, .T. ) ;
#51552 = ORIENTED_EDGE ( 'NONE', *, *, #2328, .F. ) ;
#51553 = ORIENTED_EDGE ( 'NONE', *, *, #36841, .F. ) ;
#51554 = CARTESIAN_POINT ( 'NONE',  ( 0.2648978790185602672, 4.312320170909236694, 11.46165506714229565 ) ) ;
#51555 = ADVANCED_FACE ( 'NONE', ( #54860 ), #4669, .T. ) ;
#51556 = CARTESIAN_POINT ( 'NONE',  ( 0.6511581176954477357, 11.51117493088880650, 4.541862140119159008 ) ) ;
#51557 = AXIS2_PLACEMENT_3D ( 'NONE', #17367, #47620, #31650 ) ;
#51558 = CARTESIAN_POINT ( 'NONE',  ( 2.705197763288548440, -1.076142490489816694, -7.714317563576067016 ) ) ;
#51559 = DIRECTION ( 'NONE',  ( -1.000000000000000000, 0.000000000000000000, 0.000000000000000000 ) ) ;
#51560 = ORIENTED_EDGE ( 'NONE', *, *, #32545, .F. ) ;
#51561 = CARTESIAN_POINT ( 'NONE',  ( -22.35190811654612020, -3.498661567523020821, -1.736165297231004434 ) ) ;
#51562 = VERTEX_POINT ( 'NONE', #3996 ) ;
#51563 = DIRECTION ( 'NONE',  ( 0.000000000000000000, 0.7617968321374901652, 0.6478160128811921714 ) ) ;
#51564 = CARTESIAN_POINT ( 'NONE',  ( -27.08430792439081003, 0.5856059198894674189, 2.215465963318176357 ) ) ;
#51565 = CARTESIAN_POINT ( 'NONE',  ( 2.798553295784531159, 25.00000000000000000, 7.462808788758677814 ) ) ;
#51566 = DIRECTION ( 'NONE',  ( -1.000000000000000000, 0.000000000000000000, 0.000000000000000000 ) ) ;
#51567 = CARTESIAN_POINT ( 'NONE',  ( 29.19404894130743600, 6.482428994453312221, 10.10898271525048386 ) ) ;
#51568 = CARTESIAN_POINT ( 'NONE',  ( 3.047904605210430162, -7.891858004695963658, -0.4249306449416186959 ) ) ;
#51569 = EDGE_CURVE ( 'NONE', #40556, #32142, #36224, .T. ) ;
#51570 = ORIENTED_EDGE ( 'NONE', *, *, #57846, .T. ) ;
#51571 = DIRECTION ( 'NONE',  ( -1.000000000000000000, 0.000000000000000000, 0.000000000000000000 ) ) ;
#51572 = VERTEX_POINT ( 'NONE', #39556 ) ;
#51573 = CARTESIAN_POINT ( 'NONE',  ( 5.514970785353741078, -0.001117786416802588273, -0.004588761610585022875 ) ) ;
#51574 = CARTESIAN_POINT ( 'NONE',  ( 17.05919086487388725, -28.51594916623514209, -9.278936603800785221 ) ) ;
#51575 = CARTESIAN_POINT ( 'NONE',  ( 13.39083528062609751, -28.49171679073737451, 12.64377518253357913 ) ) ;
#51576 = CARTESIAN_POINT ( 'NONE',  ( -37.00000000000000711, 0.000000000000000000, 0.000000000000000000 ) ) ;
#51577 = DIRECTION ( 'NONE',  ( 0.000000000000000000, 0.000000000000000000, 1.000000000000000000 ) ) ;
#51578 = ORIENTED_EDGE ( 'NONE', *, *, #46163, .F. ) ;
#51579 = FACE_OUTER_BOUND ( 'NONE', #24611, .T. ) ;
#51580 = CARTESIAN_POINT ( 'NONE',  ( -36.00000000000000711, -7.745827850122939395, -10.12742074351904975 ) ) ;
#51581 = CARTESIAN_POINT ( 'NONE',  ( 1.719304012338834786, 2.961219984257995819, 12.38166659046419227 ) ) ;
#51582 = LINE ( 'NONE', #6992, #41246 ) ;
#51583 = AXIS2_PLACEMENT_3D ( 'NONE', #39232, #28943, #12991 ) ;
#51584 = ADVANCED_FACE ( 'NONE', ( #19931 ), #46233, .F. ) ;
#51585 = CARTESIAN_POINT ( 'NONE',  ( 0.3341166715381295171, 12.26652061402056049, -0.2526177176100498634 ) ) ;
#51586 = EDGE_CURVE ( 'NONE', #19660, #41809, #23010, .T. ) ;
#51587 = CARTESIAN_POINT ( 'NONE',  ( -37.00000000000000711, 4.983891302653582933, 11.73555825188278590 ) ) ;
#51588 = CARTESIAN_POINT ( 'NONE',  ( -18.49080574448680991, -12.00000000000057909, -4.407108900774715188E-13 ) ) ;
#51589 = PLANE ( 'NONE',  #31184 ) ;
#51590 = VECTOR ( 'NONE', #45168, 1000.000000000000000 ) ;
#51591 = EDGE_CURVE ( 'NONE', #52926, #46774, #55546, .T. ) ;
#51592 = ORIENTED_EDGE ( 'NONE', *, *, #31523, .T. ) ;
#51593 = ORIENTED_EDGE ( 'NONE', *, *, #3144, .F. ) ;
#51594 = CARTESIAN_POINT ( 'NONE',  ( 3.152665057736074417, -6.622010822085853121, 4.377619405894153992 ) ) ;
#51595 = CARTESIAN_POINT ( 'NONE',  ( 44.04183182023682974, -1.142706581721708803, -14.69327751537514537 ) ) ;
#51596 = CARTESIAN_POINT ( 'NONE',  ( -29.92777678363736626, -3.750539801530011985, 25.00000000000000000 ) ) ;
#51597 = B_SPLINE_CURVE_WITH_KNOTS ( 'NONE', 3,
 ( #53217, #42219, #16652, #36923, #2362, #32574 ),
 .UNSPECIFIED., .F., .F.,
 ( 4, 2, 4 ),
 ( 0.005162059057943477365, 0.006293711021387341994, 0.007425362984831206624 ),
 .UNSPECIFIED. ) ;
#51598 = CARTESIAN_POINT ( 'NONE',  ( 0.3632410797595259644, -1.872837903657279535, 12.13515851238022947 ) ) ;
#51599 = ORIENTED_EDGE ( 'NONE', *, *, #51308, .T. ) ;
#51600 = EDGE_CURVE ( 'NONE', #43974, #31785, #60166, .T. ) ;
#51601 = ORIENTED_EDGE ( 'NONE', *, *, #11386, .F. ) ;
#51602 = EDGE_LOOP ( 'NONE', ( #35563, #43147, #59984, #59447 ) ) ;
#51603 = B_SPLINE_CURVE_WITH_KNOTS ( 'NONE', 3,
 ( #46701, #42340, #57683, #12418, #11766, #1158, #47377, #41712, #32689, #62006 ),
 .UNSPECIFIED., .F., .F.,
 ( 4, 3, 3, 4 ),
 ( 4.336808689942017736E-19, 6.607638129004468554E-05, 9.911389841680466693E-05, 0.0001667630577588625823 ),
 .UNSPECIFIED. ) ;
#51604 = LINE ( 'NONE', #62521, #30202 ) ;
#51605 = DIRECTION ( 'NONE',  ( 0.000000000000000000, -0.01356324068817992175, 0.9999080150203990547 ) ) ;
#51606 = ORIENTED_EDGE ( 'NONE', *, *, #178, .F. ) ;
#51607 = CARTESIAN_POINT ( 'NONE',  ( -17.32524154617501821, 3.215141440730553413, -11.56265422116751296 ) ) ;
#51608 = CYLINDRICAL_SURFACE ( 'NONE', #7714, 5.000000000000000888 ) ;
#51609 = ORIENTED_EDGE ( 'NONE', *, *, #30872, .F. ) ;
#51610 = CIRCLE ( 'NONE', #60084, 12.18650000000000055 ) ;
#51611 = CARTESIAN_POINT ( 'NONE',  ( -22.28776923226071460, 0.2883912626656737754, 3.702096209084090983 ) ) ;
#51612 = CARTESIAN_POINT ( 'NONE',  ( 13.91355800505865759, -33.59315906254626327, -9.938744394552985639 ) ) ;
#51613 = DIRECTION ( 'NONE',  ( 1.000000000000000000, 0.000000000000000000, 0.000000000000000000 ) ) ;
#51614 = ORIENTED_EDGE ( 'NONE', *, *, #592, .T. ) ;
#51615 = CARTESIAN_POINT ( 'NONE',  ( 0.3160775863651146267, 12.11619190710941396, -1.892533050396041361 ) ) ;
#51616 = VERTEX_POINT ( 'NONE', #14590 ) ;
#51617 = CARTESIAN_POINT ( 'NONE',  ( -35.00000000000000000, 12.42372387097882402, 2.865935305911668785 ) ) ;
#51618 = ORIENTED_EDGE ( 'NONE', *, *, #58654, .F. ) ;
#51619 = CARTESIAN_POINT ( 'NONE',  ( -36.00000000000000711, 11.39945968423479883, -5.710938531231587234 ) ) ;
#51620 = CIRCLE ( 'NONE', #38890, 5.000000000000000888 ) ;
#51621 = CARTESIAN_POINT ( 'NONE',  ( 0.2655924914740778187, -11.49267051747965596, -4.229867354073672203 ) ) ;
#51622 = DIRECTION ( 'NONE',  ( -1.000000000000000000, 0.000000000000000000, 0.000000000000000000 ) ) ;
#51623 = CARTESIAN_POINT ( 'NONE',  ( 35.00000000000000000, -9.493370459201747380, -6.917234959366797220 ) ) ;
#51624 = CARTESIAN_POINT ( 'NONE',  ( 2.241451721903215066, -6.641849090084981810, 3.764430789729956928 ) ) ;
#51625 = DIRECTION ( 'NONE',  ( 0.000000000000000000, -0.9467777615094538080, -0.3218879778916074463 ) ) ;
#51626 = DIRECTION ( 'NONE',  ( 0.000000000000000000, -0.9718671068226484300, 0.2355298848897411923 ) ) ;
#51627 = CARTESIAN_POINT ( 'NONE',  ( 0.2651627923886328841, 4.105544202112549002, 11.53745192040743639 ) ) ;
#51629 = ORIENTED_EDGE ( 'NONE', *, *, #31465, .T. ) ;
#51628 = CARTESIAN_POINT ( 'NONE',  ( 6.916391019076965740, -8.217520853910727396, 10.71822957364710760 ) ) ;
#51630 = CARTESIAN_POINT ( 'NONE',  ( -37.00000000000000711, -11.44858830469742017, 2.627174906296871448 ) ) ;
#51631 = ORIENTED_EDGE ( 'NONE', *, *, #48769, .F. ) ;
#51632 = CARTESIAN_POINT ( 'NONE',  ( -35.00000000000000000, -7.379373053628940582, 10.39746860227888092 ) ) ;
#51633 = CARTESIAN_POINT ( 'NONE',  ( 35.00000000000000000, 4.824807283154291859, 11.80185301892974969 ) ) ;
#51635 = ORIENTED_EDGE ( 'NONE', *, *, #26688, .F. ) ;
#51634 = ADVANCED_FACE ( 'NONE', ( #34867 ), #4982, .T. ) ;
#51636 = CARTESIAN_POINT ( 'NONE',  ( -37.00000000000000711, -7.882940143791846488, 10.02106554660705839 ) ) ;
#51637 = CARTESIAN_POINT ( 'NONE',  ( -27.10719052120871098, -2.355164825213512003, 0.1538293304135223694 ) ) ;
#51638 = CARTESIAN_POINT ( 'NONE',  ( 0.2648978790185584908, -9.295532325666394868, -7.972372351883127095 ) ) ;
#51639 = DIRECTION ( 'NONE',  ( 0.000000000000000000, 0.8369827122275325104, 0.5472293298355301872 ) ) ;
#51640 = EDGE_CURVE ( 'NONE', #28779, #53475, #7560, .T. ) ;
#51641 = CARTESIAN_POINT ( 'NONE',  ( 2.242418902651535539, 7.207816731000297850, 2.517330194231067519 ) ) ;
#51642 = ORIENTED_EDGE ( 'NONE', *, *, #39635, .T. ) ;
#51643 = CARTESIAN_POINT ( 'NONE',  ( 47.00000000000000711, 4.705694406421931860E-17, -3.469127814946512892E-15 ) ) ;
#51644 = ORIENTED_EDGE ( 'NONE', *, *, #32847, .T. ) ;
#51645 = CARTESIAN_POINT ( 'NONE',  ( -35.04643116707788408, -0.009112266603810564858, 0.008094444324481878117 ) ) ;
#51646 = CARTESIAN_POINT ( 'NONE',  ( 0.000000000000000000, -6.777474576704058506, 0.6925993764990423518 ) ) ;
#51647 = DIRECTION ( 'NONE',  ( -1.000000000000000000, 0.000000000000000000, 0.000000000000000000 ) ) ;
#51648 = ORIENTED_EDGE ( 'NONE', *, *, #1015, .F. ) ;
#51649 = CARTESIAN_POINT ( 'NONE',  ( 37.00000000000000711, 11.50504120060948487, 4.018060380616274685 ) ) ;
#51650 = EDGE_CURVE ( 'NONE', #12997, #29569, #32431, .T. ) ;
#51651 = AXIS2_PLACEMENT_3D ( 'NONE', #49970, #51942, #47289 ) ;
#51652 = CIRCLE ( 'NONE', #43121, 12.75000000000000178 ) ;
#51653 = EDGE_CURVE ( 'NONE', #31409, #46540, #37270, .T. ) ;
#51654 = CARTESIAN_POINT ( 'NONE',  ( -22.66110217412718697, -4.366928509133846781, 2.319520136975691482 ) ) ;
#51655 = CARTESIAN_POINT ( 'NONE',  ( 25.82596324657534126, -3.714872568654962848, 25.00000000000000711 ) ) ;
#51656 = EDGE_CURVE ( 'NONE', #37945, #40578, #23473, .T. ) ;
#51657 = CARTESIAN_POINT ( 'NONE',  ( 37.00000000000000711, 3.640372113593552061, -12.21925492305363647 ) ) ;
#51658 = CARTESIAN_POINT ( 'NONE',  ( 8.437200413559441614, 4.476360154859203355, 12.73625532737111143 ) ) ;
#51659 = EDGE_CURVE ( 'NONE', #29418, #65490, #29860, .T. ) ;
#51660 = CARTESIAN_POINT ( 'NONE',  ( -35.00000000000000000, 1.286231064351496034, -12.68495603654570303 ) ) ;
#51661 = CARTESIAN_POINT ( 'NONE',  ( 1.014383007554942484, 4.688516792764612973, 11.58298623339616462 ) ) ;
#51662 = CARTESIAN_POINT ( 'NONE',  ( 1.549075743846074271, -3.694639393663741167, -12.12370443967618172 ) ) ;
#51663 = EDGE_CURVE ( 'NONE', #9187, #36108, #7086, .T. ) ;
#51664 = VERTEX_POINT ( 'NONE', #48415 ) ;
#51665 = CARTESIAN_POINT ( 'NONE',  ( -17.57519261785461850, 6.782244033140607087, 11.67428159032847645 ) ) ;
#51666 = CARTESIAN_POINT ( 'NONE',  ( 6.574848435243071165, -7.682001007202829079, 11.10271414525420575 ) ) ;
#51667 =( BOUNDED_CURVE ( )  B_SPLINE_CURVE ( 3, ( #4992, #45528, #45216, #65476 ),
 .UNSPECIFIED., .F., .F. ) 
 B_SPLINE_CURVE_WITH_KNOTS ( ( 4, 4 ),
 ( 1.062823956857581464, 1.069007632545065700 ),
 .UNSPECIFIED. ) 
 CURVE ( )  GEOMETRIC_REPRESENTATION_ITEM ( )  RATIONAL_B_SPLINE_CURVE ( ( 1.000000000000000000, 0.9999968135154544413, 0.9999968135154544413, 1.000000000000000000 ) ) 
 REPRESENTATION_ITEM ( '' )  );
#51668 = ORIENTED_EDGE ( 'NONE', *, *, #31987, .T. ) ;
#51669 = CARTESIAN_POINT ( 'NONE',  ( -37.00000000000000711, 10.68873102412852560, -6.950793414699682593 ) ) ;
#51670 = EDGE_CURVE ( 'NONE', #38324, #32833, #45975, .T. ) ;
#51671 = CARTESIAN_POINT ( 'NONE',  ( -17.83419946441818027, -9.720786832536937538, 25.00000000000000000 ) ) ;
#51672 = CARTESIAN_POINT ( 'NONE',  ( -9.464296738015105959, 10.76059690970763505, -8.161180804017673651 ) ) ;
#51673 = VERTEX_POINT ( 'NONE', #63345 ) ;
#51674 = DIRECTION ( 'NONE',  ( 0.000000000000000000, -0.8827602140260366603, 0.4698238015817268187 ) ) ;
#51675 = ORIENTED_EDGE ( 'NONE', *, *, #33821, .T. ) ;
#51676 = CARTESIAN_POINT ( 'NONE',  ( 0.2801149460245174749, -5.954809120985783188, 10.70654700624300304 ) ) ;
#51677 = EDGE_LOOP ( 'NONE', ( #10915, #17972, #25764, #337 ) ) ;
#51678 = ORIENTED_EDGE ( 'NONE', *, *, #8809, .T. ) ;
#51679 = CARTESIAN_POINT ( 'NONE',  ( -35.00000000000000000, -12.17626345777664021, 0.4993900848166987760 ) ) ;
#51680 = ORIENTED_EDGE ( 'NONE', *, *, #60786, .F. ) ;
#51681 = ADVANCED_FACE ( 'NONE', ( #7166 ), #27446, .T. ) ;
#51682 = CARTESIAN_POINT ( 'NONE',  ( -25.27109080293329413, -9.776000194394919518, 6.961263260165105216 ) ) ;
#51683 = LINE ( 'NONE', #64256, #18760 ) ;
#51684 = CARTESIAN_POINT ( 'NONE',  ( 37.00000000000000711, -1.908798535168467536, -12.60630747491662618 ) ) ;
#51685 = CARTESIAN_POINT ( 'NONE',  ( -37.00000000000000711, 10.42955799785328708, -6.303578524886837009 ) ) ;
#51686 = VERTEX_POINT ( 'NONE', #15586 ) ;
#51687 = CARTESIAN_POINT ( 'NONE',  ( 37.00000000000000711, 7.608228585767871976, 10.23119532541064203 ) ) ;
#51688 = CARTESIAN_POINT ( 'NONE',  ( -0.5153900578009965594, -25.72562925869133821, 15.66323518044676000 ) ) ;
#51689 = CARTESIAN_POINT ( 'NONE',  ( -35.00000000000000000, 11.74614673114903951, 0.01609748574465447862 ) ) ;
#51691 = ORIENTED_EDGE ( 'NONE', *, *, #39482, .F. ) ;
#51690 = FACE_OUTER_BOUND ( 'NONE', #17974, .T. ) ;
#51692 = CARTESIAN_POINT ( 'NONE',  ( 2.241506898688419458, -2.574154135948738098, 7.187425579579794999 ) ) ;
#51693 = ORIENTED_EDGE ( 'NONE', *, *, #47830, .F. ) ;
#51694 = CARTESIAN_POINT ( 'NONE',  ( 5.514970785353741078, -0.004233694591582967161, -0.002093325033903798652 ) ) ;
#51695 = VERTEX_POINT ( 'NONE', #47432 ) ;
#51696 = ORIENTED_EDGE ( 'NONE', *, *, #11193, .T. ) ;
#51697 = AXIS2_PLACEMENT_3D ( 'NONE', #27978, #11676, #37621 ) ;
#51698 = DIRECTION ( 'NONE',  ( 0.000000000000000000, 0.3807014730195219521, -0.9246979985058723095 ) ) ;
#51699 = CARTESIAN_POINT ( 'NONE',  ( 2.241537034860905386, -4.903726641589485347, -5.851376807350193943 ) ) ;
#51700 = DIRECTION ( 'NONE',  ( -1.000000000000000000, 0.000000000000000000, 0.000000000000000000 ) ) ;
#51701 = ORIENTED_EDGE ( 'NONE', *, *, #358, .T. ) ;
#51702 = FACE_OUTER_BOUND ( 'NONE', #26008, .T. ) ;
#51703 = AXIS2_PLACEMENT_3D ( 'NONE', #3774, #60569, #19706 ) ;
#51704 = CYLINDRICAL_SURFACE ( 'NONE', #57974, 5.000000000000000888 ) ;
#51705 = CARTESIAN_POINT ( 'NONE',  ( 0.3675815128205894289, -12.04510820461660892, 2.391755495700564449 ) ) ;
#51706 = ORIENTED_EDGE ( 'NONE', *, *, #30663, .F. ) ;
#51707 = ORIENTED_EDGE ( 'NONE', *, *, #64842, .F. ) ;
#51708 = DIRECTION ( 'NONE',  ( -1.000000000000000000, 0.000000000000000000, 0.000000000000000000 ) ) ;
#51709 = EDGE_LOOP ( 'NONE', ( #47897, #20268, #54297, #49884 ) ) ;
#51710 = ORIENTED_EDGE ( 'NONE', *, *, #47251, .T. ) ;
#51711 = CARTESIAN_POINT ( 'NONE',  ( -10.00000000000000178, 0.000000000000000000, 0.000000000000000000 ) ) ;
#51712 = LINE ( 'NONE', #41711, #40252 ) ;
#51713 = CARTESIAN_POINT ( 'NONE',  ( 37.00000000000000711, 2.346765782874432382, -11.95840593935202278 ) ) ;
#51714 = CARTESIAN_POINT ( 'NONE',  ( 5.516018279890452902, 0.003191189039764439229, -0.005976902763918727837 ) ) ;
#51715 = FACE_OUTER_BOUND ( 'NONE', #26408, .T. ) ;
#51716 = EDGE_CURVE ( 'NONE', #19597, #2444, #5446, .T. ) ;
#51717 = PLANE ( 'NONE',  #13966 ) ;
#51718 = DIRECTION ( 'NONE',  ( -0.2415534870330798278, 0.000000000000000000, 0.9703875065674330003 ) ) ;
#51719 = ORIENTED_EDGE ( 'NONE', *, *, #60208, .F. ) ;
#51720 = CARTESIAN_POINT ( 'NONE',  ( -22.28350523959500862, -3.041489826385514572, 2.107889123925578367 ) ) ;
#51721 = DIRECTION ( 'NONE',  ( -1.000000000000000000, -0.000000000000000000, 0.000000000000000000 ) ) ;
#51722 = DIRECTION ( 'NONE',  ( -1.000000000000000000, 0.000000000000000000, 0.000000000000000000 ) ) ;
#51723 = EDGE_CURVE ( 'NONE', #9280, #33968, #65022, .T. ) ;
#51724 = CARTESIAN_POINT ( 'NONE',  ( -35.05012975565874456, 0.002073729464855276518, 0.01377677982613004053 ) ) ;
#51725 = CIRCLE ( 'NONE', #10313, 4.999999999999998224 ) ;
#51726 = CARTESIAN_POINT ( 'NONE',  ( 35.00000000000000000, 2.216820770815085773, -11.53507381115584529 ) ) ;
#51727 = ADVANCED_FACE ( 'NONE', ( #64647 ), #11815, .F. ) ;
#51728 = CARTESIAN_POINT ( 'NONE',  ( 3.627734094270521403, 4.214566690872760368, -11.24377562339657999 ) ) ;
#51729 = CARTESIAN_POINT ( 'NONE',  ( 11.38592777356517871, 0.2429536942619314188, -11.99780484965632077 ) ) ;
#51730 = EDGE_CURVE ( 'NONE', #2297, #24257, #8610, .T. ) ;
#51731 = ORIENTED_EDGE ( 'NONE', *, *, #47413, .T. ) ;
#51732 = LINE ( 'NONE', #47399, #19576 ) ;
#51733 = CARTESIAN_POINT ( 'NONE',  ( -47.00000000000000711, 0.000000000000000000, 0.000000000000000000 ) ) ;
#51734 = DIRECTION ( 'NONE',  ( 0.000000000000000000, -0.01356324068817998940, 0.9999080150203990547 ) ) ;
#51735 = CARTESIAN_POINT ( 'NONE',  ( 8.006888830061562601, -32.29065697289883730, 12.88904745433947596 ) ) ;
#51736 = CIRCLE ( 'NONE', #8198, 12.75000000000000178 ) ;
#51737 = CARTESIAN_POINT ( 'NONE',  ( 9.778943843942252911, 2.009314548101766462, -13.35093242851569784 ) ) ;
#51738 = CARTESIAN_POINT ( 'NONE',  ( 2.430348790457476760, -7.164221884688256381, 2.814990071338049571 ) ) ;
#51739 = ORIENTED_EDGE ( 'NONE', *, *, #14222, .T. ) ;
#51740 = CARTESIAN_POINT ( 'NONE',  ( -35.00000000000000000, 10.07641281632186114, -6.036400161834460043 ) ) ;
#51741 = CYLINDRICAL_SURFACE ( 'NONE', #14221, 12.18649999999999878 ) ;
#51742 = EDGE_CURVE ( 'NONE', #16757, #8357, #16044, .T. ) ;
#51743 = CARTESIAN_POINT ( 'NONE',  ( 11.27382677987933057, -33.37417574758200800, -11.09187761368031211 ) ) ;
#51744 = ORIENTED_EDGE ( 'NONE', *, *, #58418, .F. ) ;
#51745 = CARTESIAN_POINT ( 'NONE',  ( 2.177405672431178552, -8.129711416440740024, 7.702458780351658874 ) ) ;
#51746 = CARTESIAN_POINT ( 'NONE',  ( -17.58536674675198341, 6.767421432155036776, -9.911758545779559171 ) ) ;
#51747 = CARTESIAN_POINT ( 'NONE',  ( 37.00000000000000711, 4.705694406421931860E-17, -3.469127814946512892E-15 ) ) ;
#51748 = ADVANCED_FACE ( 'NONE', ( #18497 ), #49078, .T. ) ;
#51750 = ORIENTED_EDGE ( 'NONE', *, *, #13172, .F. ) ;
#51749 = CARTESIAN_POINT ( 'NONE',  ( 2.899286259009682620, 1.011320371384342831, 7.788326766693353775 ) ) ;
#51751 = CARTESIAN_POINT ( 'NONE',  ( -14.47334165536100059, 0.000000000000000000, 0.000000000000000000 ) ) ;
#51752 = EDGE_CURVE ( 'NONE', #27004, #50535, #61709, .T. ) ;
#51753 = CARTESIAN_POINT ( 'NONE',  ( 2.556980015513814486, -7.348538402679465342, -2.429125721802482207 ) ) ;
#51754 = ORIENTED_EDGE ( 'NONE', *, *, #6642, .F. ) ;
#51755 = ADVANCED_FACE ( 'NONE', ( #13459 ), #39389, .T. ) ;
#51756 = DIRECTION ( 'NONE',  ( 0.000000000000000000, -0.01356324068817998940, 0.9999080150203990547 ) ) ;
#51757 = LINE ( 'NONE', #16503, #2239 ) ;
#51758 = CARTESIAN_POINT ( 'NONE',  ( 35.00000000000000000, -12.71517666308947092, 0.9416912585475696318 ) ) ;
#51759 = CARTESIAN_POINT ( 'NONE',  ( -3.347463755625758264, -12.75767721842421665, 4.430665912812002283 ) ) ;
#51760 = CARTESIAN_POINT ( 'NONE',  ( -9.264327559741124318, 8.341203664785947325, -8.636428847717205315 ) ) ;
#51761 = EDGE_CURVE ( 'NONE', #30430, #50238, #23519, .T. ) ;
#51762 = CARTESIAN_POINT ( 'NONE',  ( 0.000000000000000000, 0.8935325819928834346, 7.446583077151348817 ) ) ;
#51764 = ORIENTED_EDGE ( 'NONE', *, *, #24533, .T. ) ;
#51763 = LINE ( 'NONE', #45774, #28672 ) ;
#51765 = ORIENTED_EDGE ( 'NONE', *, *, #46475, .T. ) ;
#51766 = CARTESIAN_POINT ( 'NONE',  ( 24.89709673309864257, -0.9453300160761306525, -11.96437408882576925 ) ) ;
#51767 = ORIENTED_EDGE ( 'NONE', *, *, #52516, .F. ) ;
#51768 = SURFACE_SIDE_STYLE ('',( #61717 ) ) ;
#51769 = DIRECTION ( 'NONE',  ( 0.000000000000000000, 0.6876994588534246500, -0.7259954919231293990 ) ) ;
#51770 = CARTESIAN_POINT ( 'NONE',  ( -17.71793285162545928, 3.743050124886382335, 11.40313316626405182 ) ) ;
#51771 = CARTESIAN_POINT ( 'NONE',  ( 35.00000000000000000, -7.882940143791697274, 10.02106554660716853 ) ) ;
#51772 = ORIENTED_EDGE ( 'NONE', *, *, #26860, .T. ) ;
#51773 = CARTESIAN_POINT ( 'NONE',  ( -22.31328051695926007, -3.401210163132568187, -1.671726071983963946 ) ) ;
#51774 = CYLINDRICAL_SURFACE ( 'NONE', #24097, 5.000000000000000888 ) ;
#51775 = CARTESIAN_POINT ( 'NONE',  ( -35.00000000000000000, 0.000000000000000000, 0.000000000000000000 ) ) ;
#51776 = ORIENTED_EDGE ( 'NONE', *, *, #22832, .T. ) ;
#51777 = ORIENTED_EDGE ( 'NONE', *, *, #34994, .F. ) ;
#51778 = CARTESIAN_POINT ( 'NONE',  ( 29.03109630806826758, -11.07829921360117353, 7.725641260898457041 ) ) ;
#51779 = ORIENTED_EDGE ( 'NONE', *, *, #62032, .F. ) ;
#51780 = CARTESIAN_POINT ( 'NONE',  ( 21.94670809694110147, -11.54116911556738145, -3.292040187117030392 ) ) ;
#51781 = AXIS2_PLACEMENT_3D ( 'NONE', #58081, #62082, #31486 ) ;
#51782 = CARTESIAN_POINT ( 'NONE',  ( 5.515539859299206427, -0.005991790098944305316, -0.0008592514567752725574 ) ) ;
#51783 = DIRECTION ( 'NONE',  ( 0.000000000000000000, 0.000000000000000000, -1.000000000000000000 ) ) ;
#51784 = CARTESIAN_POINT ( 'NONE',  ( 0.9232167919969107572, 12.34114433434357139, 1.756271097262108505 ) ) ;
#51785 = EDGE_CURVE ( 'NONE', #62115, #49238, #4500, .T. ) ;
#51786 = DIRECTION ( 'NONE',  ( -1.000000000000000000, 0.000000000000000000, 0.000000000000000000 ) ) ;
#51787 = CARTESIAN_POINT ( 'NONE',  ( 36.00000000000000711, -10.84030624090611283, -6.711949091238110121 ) ) ;
#51788 = AXIS2_PLACEMENT_3D ( 'NONE', #21838, #1872, #36786 ) ;
#51789 = LINE ( 'NONE', #61406, #1514 ) ;
#51790 = ORIENTED_EDGE ( 'NONE', *, *, #2689, .F. ) ;
#51791 = CYLINDRICAL_SURFACE ( 'NONE', #1878, 12.18650000000000055 ) ;
#51792 = CARTESIAN_POINT ( 'NONE',  ( 2.705197763288552881, 4.134294772210017399, -6.601241161176638172 ) ) ;
#51793 = CARTESIAN_POINT ( 'NONE',  ( 37.00000000000000711, 4.705694406421931860E-17, -3.469127814946512892E-15 ) ) ;
#51794 = CARTESIAN_POINT ( 'NONE',  ( 37.00000000000000711, 6.303578524887092804, 10.42955799785312898 ) ) ;
#51795 = LINE ( 'NONE', #20545, #22289 ) ;
#51796 = CARTESIAN_POINT ( 'NONE',  ( 5.530133899448235191, -0.01149180883054594197, 0.01111090067015119663 ) ) ;
#51797 = EDGE_CURVE ( 'NONE', #14607, #45697, #5502, .T. ) ;
#51798 = CARTESIAN_POINT ( 'NONE',  ( 5.515188684475870851, 0.002166413411657351282, -0.004893136156457789619 ) ) ;
#51799 = ORIENTED_EDGE ( 'NONE', *, *, #13110, .F. ) ;
#51800 = VERTEX_POINT ( 'NONE', #9133 ) ;
#51801 = EDGE_CURVE ( 'NONE', #40209, #9770, #45826, .T. ) ;
#51802 = CARTESIAN_POINT ( 'NONE',  ( -37.00000000000000711, 9.430788938294160317, -7.718225330433705622 ) ) ;
#51803 = VERTEX_POINT ( 'NONE', #13779 ) ;
#51804 = CARTESIAN_POINT ( 'NONE',  ( 2.241352910868908310, -2.532612177304491397, 7.202080440908734005 ) ) ;
#51805 = CARTESIAN_POINT ( 'NONE',  ( 2.000000000000001776, 5.997115278587678233, -3.485633455389450130 ) ) ;
#51806 = CARTESIAN_POINT ( 'NONE',  ( 1.633930747252541504, -10.17701904908771127, -7.601388527387344496 ) ) ;
#51807 = DIRECTION ( 'NONE',  ( 0.000000000000000000, -1.000000000000000000, 0.000000000000000000 ) ) ;
#51808 = EDGE_CURVE ( 'NONE', #59054, #65435, #29416, .T. ) ;
#51809 = ORIENTED_EDGE ( 'NONE', *, *, #44579, .F. ) ;
#51810 = DIRECTION ( 'NONE',  ( 0.3939253465568943735, 0.8669868725995579783, -0.3052156353794294175 ) ) ;
#51811 = CARTESIAN_POINT ( 'NONE',  ( 36.00000000000000711, 10.68873102412842435, -6.950793414699834472 ) ) ;
#51812 = CARTESIAN_POINT ( 'NONE',  ( 1.634816307076136122, -12.61459884932949294, 1.494046826342531054 ) ) ;
#51813 = CARTESIAN_POINT ( 'NONE',  ( -46.20808592110950741, -0.7439837506150833724, 13.26238176883679643 ) ) ;
#51814 = CIRCLE ( 'NONE', #46483, 12.74999999999999822 ) ;
#51815 = CARTESIAN_POINT ( 'NONE',  ( 0.3675815128205912052, 9.235491948680007113, 8.093875121226108860 ) ) ;
#51816 = CARTESIAN_POINT ( 'NONE',  ( 2.256373768223415066, 2.737361830682320640, 7.132139410180973194 ) ) ;
#51817 = CIRCLE ( 'NONE', #7219, 2.899999999999995914 ) ;
#51818 = VERTEX_POINT ( 'NONE', #9444 ) ;
#51819 = ORIENTED_EDGE ( 'NONE', *, *, #60065, .F. ) ;
#51820 = CARTESIAN_POINT ( 'NONE',  ( -37.00000000000000711, -10.92721691015459307, 4.309077947445612899 ) ) ;
#51821 = CARTESIAN_POINT ( 'NONE',  ( 29.51976981715666781, -4.571419055710073565, 11.09513982864076276 ) ) ;
#51822 = DIRECTION ( 'NONE',  ( 0.000000000000000000, -0.6051742151937558045, -0.7960930657056509707 ) ) ;
#51823 = AXIS2_PLACEMENT_3D ( 'NONE', #24064, #63296, #28074 ) ;
#51824 = CARTESIAN_POINT ( 'NONE',  ( -35.04660725145885891, 0.01123650152080950260, 0.004999447127041124761 ) ) ;
#51825 = CARTESIAN_POINT ( 'NONE',  ( 35.00000000000000000, 4.705694406421931860E-17, -3.469127814946512892E-15 ) ) ;
#51826 = ADVANCED_FACE ( 'NONE', ( #29108 ), #3852, .T. ) ;
#51827 = ORIENTED_EDGE ( 'NONE', *, *, #18675, .F. ) ;
#51828 = VECTOR ( 'NONE', #7771, 1000.000000000000000 ) ;
#51829 = ORIENTED_EDGE ( 'NONE', *, *, #47239, .F. ) ;
#51830 = CARTESIAN_POINT ( 'NONE',  ( -30.17816725640874154, -0.9612562749268102058, 11.96359558481438157 ) ) ;
#51831 = ADVANCED_FACE ( 'NONE', ( #18141 ), #38413, .T. ) ;
#51832 = ORIENTED_EDGE ( 'NONE', *, *, #36148, .F. ) ;
#51833 = CARTESIAN_POINT ( 'NONE',  ( -27.08416813689868263, -2.257587568255724708, 0.3912215308406081782 ) ) ;
#51834 = DIRECTION ( 'NONE',  ( 0.000000000000000000, 0.3218879778915972878, -0.9467777615094571386 ) ) ;
#51835 = DIRECTION ( 'NONE',  ( 0.000000000000000000, -0.01356324068818000328, 0.9999080150203990547 ) ) ;
#51836 = CARTESIAN_POINT ( 'NONE',  ( 3.152665057736111720, -7.281573230473792790, 3.161213418915395312 ) ) ;
#51837 = DIRECTION ( 'NONE',  ( 0.000000000000000000, -0.01356324068817998940, 0.9999080150203990547 ) ) ;
#51838 = ADVANCED_FACE ( 'NONE', ( #31060 ), #60328, .T. ) ;
#51839 = CARTESIAN_POINT ( 'NONE',  ( 1.109979610372473946, 11.08130463534589261, -5.843815872356196373 ) ) ;
#51840 = CARTESIAN_POINT ( 'NONE',  ( 1.109979610374045356, 12.41172293674789096, -1.701361252867769513 ) ) ;
#51841 = ORIENTED_EDGE ( 'NONE', *, *, #63381, .T. ) ;
#51842 = CARTESIAN_POINT ( 'NONE',  ( -9.340346724179731552, -10.24301314885845571, -6.263313883498242696 ) ) ;
#51843 = ORIENTED_EDGE ( 'NONE', *, *, #51474, .T. ) ;
#51844 = CARTESIAN_POINT ( 'NONE',  ( -9.044048956294592045, 11.38398270688161595, -3.796001806769623066 ) ) ;
#51845 = CARTESIAN_POINT ( 'NONE',  ( 36.00000000000000711, -3.307597835713331325, -12.31350058095522293 ) ) ;
#51846 = ORIENTED_EDGE ( 'NONE', *, *, #21248, .F. ) ;
#51847 = DIRECTION ( 'NONE',  ( -1.000000000000000000, 0.000000000000000000, 0.000000000000000000 ) ) ;
#51848 = VERTEX_POINT ( 'NONE', #30715 ) ;
#51849 =( BOUNDED_SURFACE ( )  B_SPLINE_SURFACE ( 3, 1, ( 
 ( #9176, #45407 ),
 ( #64692, #25137 ),
 ( #19163, #65671 ),
 ( #19503, #60063 ) ),
 .UNSPECIFIED., .F., .F., .F. ) 
 B_SPLINE_SURFACE_WITH_KNOTS ( ( 4, 4 ),
 ( 2, 2 ),
 ( 0.000000000000000000, 1.000000000000000000 ),
 ( 0.000000000000000000, 1.000000000000000000 ),
 .UNSPECIFIED. ) 
 GEOMETRIC_REPRESENTATION_ITEM ( )  RATIONAL_B_SPLINE_SURFACE ( (
 ( 1.000000000000000000, 1.000000000000000000),
 ( 0.9942764183789327692, 0.8450855930916585379),
 ( 0.9942764183789327692, 0.8450855930916585379),
 ( 1.000000000000000000, 1.000000000000000000) ) ) 
 REPRESENTATION_ITEM ( '' )  SURFACE ( )  );
#51850 = DIRECTION ( 'NONE',  ( -1.000000000000000000, 0.000000000000000000, 0.000000000000000000 ) ) ;
#51851 = CARTESIAN_POINT ( 'NONE',  ( -36.00000000000000711, 1.457575200925721237, -12.66641127287624435 ) ) ;
#51852 = CARTESIAN_POINT ( 'NONE',  ( 2.368238019615286127, 2.793778585134709225, 7.150288915654823718 ) ) ;
#51853 = ORIENTED_EDGE ( 'NONE', *, *, #52293, .T. ) ;
#51854 = ORIENTED_EDGE ( 'NONE', *, *, #61812, .T. ) ;
#51855 = CARTESIAN_POINT ( 'NONE',  ( 3.222831877979512871, 4.636616073543464722, 12.68534664307357396 ) ) ;
#51856 = EDGE_LOOP ( 'NONE', ( #54674, #21825, #40067, #59949 ) ) ;
#51857 = FACE_OUTER_BOUND ( 'NONE', #19600, .T. ) ;
#51858 = ORIENTED_EDGE ( 'NONE', *, *, #36253, .T. ) ;
#51859 = ORIENTED_EDGE ( 'NONE', *, *, #12887, .T. ) ;
#51860 = VERTEX_POINT ( 'NONE', #51370 ) ;
#51861 = DIRECTION ( 'NONE',  ( -1.000000000000000000, 0.000000000000000000, -0.000000000000000000 ) ) ;
#51863 = AXIS2_PLACEMENT_3D ( 'NONE', #2659, #18902, #22920 ) ;
#51862 = DIRECTION ( 'NONE',  ( 0.000000000000000000, -1.000000000000000000, 0.000000000000000000 ) ) ;
#51864 = EDGE_CURVE ( 'NONE', #26639, #61504, #17151, .T. ) ;
#51865 = CARTESIAN_POINT ( 'NONE',  ( 3.152665057734131526, -0.9030954876737319337, -7.886634106564212487 ) ) ;
#51866 = CARTESIAN_POINT ( 'NONE',  ( 2.247206125382826603, 2.720255231378031713, -7.135412558555523255 ) ) ;
#51867 = CYLINDRICAL_SURFACE ( 'NONE', #58212, 5.000000000000000000 ) ;
#51868 = ORIENTED_EDGE ( 'NONE', *, *, #65588, .F. ) ;
#51869 = CARTESIAN_POINT ( 'NONE',  ( -47.00000000000000711, 0.000000000000000000, 0.000000000000000000 ) ) ;
#51870 = EDGE_CURVE ( 'NONE', #7543, #47037, #37230, .T. ) ;
#51871 = AXIS2_PLACEMENT_3D ( 'NONE', #39935, #44927, #18702 ) ;
#51872 = CIRCLE ( 'NONE', #14709, 4.999999999999999112 ) ;
#51873 = VERTEX_POINT ( 'NONE', #56683 ) ;
#51874 =( BOUNDED_CURVE ( )  B_SPLINE_CURVE ( 3, ( #65789, #36196, #14925, #35218 ),
 .UNSPECIFIED., .F., .F. ) 
 B_SPLINE_CURVE_WITH_KNOTS ( ( 4, 4 ),
 ( 4.370225155591277222, 4.394090018125422326 ),
 .UNSPECIFIED. ) 
 CURVE ( )  GEOMETRIC_REPRESENTATION_ITEM ( )  RATIONAL_B_SPLINE_CURVE ( ( 1.000000000000000000, 0.9999525395911521564, 0.9999525395911521564, 1.000000000000000000 ) ) 
 REPRESENTATION_ITEM ( '' )  );
#51875 = DIRECTION ( 'NONE',  ( 0.000000000000000000, -0.01356324068817991828, 0.9999080150203990547 ) ) ;
#51876 = CARTESIAN_POINT ( 'NONE',  ( -27.08429572838383947, 0.5764601019426045525, 2.217805374070519253 ) ) ;
#51877 = AXIS2_PLACEMENT_3D ( 'NONE', #43015, #62967, #7426 ) ;
#51878 = CARTESIAN_POINT ( 'NONE',  ( 0.2653141516239115871, 0.04404488958248177488, -12.24612533180317797 ) ) ;
#51879 = CARTESIAN_POINT ( 'NONE',  ( 0.2801149460245143108, -8.024198546827411960, -9.257544930777235948 ) ) ;
#51880 = DIRECTION ( 'NONE',  ( -1.000000000000000000, 0.000000000000000000, 0.000000000000000000 ) ) ;
#51881 = FACE_OUTER_BOUND ( 'NONE', #6408, .T. ) ;
#51882 = EDGE_CURVE ( 'NONE', #44077, #58033, #29917, .T. ) ;
#51883 = CIRCLE ( 'NONE', #31669, 2.899999999999995026 ) ;
#51884 = EDGE_LOOP ( 'NONE', ( #53362, #27461, #17424, #51272 ) ) ;
#51885 = DIRECTION ( 'NONE',  ( 0.000000000000000000, 0.000000000000000000, 1.000000000000000000 ) ) ;
#51886 = VERTEX_POINT ( 'NONE', #45692 ) ;
#51887 = DIRECTION ( 'NONE',  ( 0.000000000000000000, 0.9105187689795940509, -0.4134677391718546424 ) ) ;
#51888 = CARTESIAN_POINT ( 'NONE',  ( -3.987543989681920920, -25.89241204356462589, -15.41372194231675508 ) ) ;
#51889 = CARTESIAN_POINT ( 'NONE',  ( 7.964047368509785230, -27.27321649430781392, 15.08844977892396777 ) ) ;
#51890 = CARTESIAN_POINT ( 'NONE',  ( -27.08588607604433562, -0.6046196991082997130, -2.215240480751995644 ) ) ;
#51891 = CARTESIAN_POINT ( 'NONE',  ( -35.00000000000000000, -12.14284015767849390, -1.030638227056693834 ) ) ;
#51892 = ADVANCED_FACE ( 'NONE', ( #25096 ), #46040, .T. ) ;
#51893 = EDGE_CURVE ( 'NONE', #27609, #54327, #11116, .T. ) ;
#51894 = ORIENTED_EDGE ( 'NONE', *, *, #22925, .F. ) ;
#51895 = B_SPLINE_CURVE_WITH_KNOTS ( 'NONE', 3,
 ( #48462, #8858, #58430, #27833, #12515, #53103, #39104, #23502, #43433, #49451, #63080, #13818, #7892, #38462, #64373, #33140, #49122, #63388, #53770 ),
 .UNSPECIFIED., .F., .F.,
 ( 4, 3, 3, 3, 3, 3, 4 ),
 ( 1.226634733346813749E-18, 2.836829842860796018E-05, 4.224792512343430404E-05, 5.612066614708130128E-05, 6.998859278151969301E-05, 9.832141287888942582E-05, 0.0001178161482480163323 ),
 .UNSPECIFIED. ) ;
#51896 = DIRECTION ( 'NONE',  ( 0.000000000000000000, -0.7617968321374811724, -0.6478160128812026075 ) ) ;
#51897 = CARTESIAN_POINT ( 'NONE',  ( -14.47334165536099881, 0.000000000000000000, 0.000000000000000000 ) ) ;
#51898 = CARTESIAN_POINT ( 'NONE',  ( 21.49227063098244628, 11.34819223667060406, -3.922596895461145650 ) ) ;
#51899 = CARTESIAN_POINT ( 'NONE',  ( 21.97974065927837017, -13.30026544007890266, -2.341972921265582208 ) ) ;
#51900 = ADVANCED_FACE ( 'NONE', ( #61313 ), #20099, .T. ) ;
#51901 = AXIS2_PLACEMENT_3D ( 'NONE', #55561, #4714, #10988 ) ;
#51902 = B_SPLINE_CURVE_WITH_KNOTS ( 'NONE', 3,
 ( #35656, #31337, #36960, #46625, #751, #10383, #51313, #5421, #41629, #16378, #439, #21351, #20708, #16021, #5763, #40983 ),
 .UNSPECIFIED., .F., .F.,
 ( 4, 3, 3, 3, 3, 4 ),
 ( 0.000000000000000000, 0.0002999043160757465022, 0.0005998071753051236604, 0.0008997092107374906646, 0.001204458948196612204, 0.001510329163478418878 ),
 .UNSPECIFIED. ) ;
#51903 = DIRECTION ( 'NONE',  ( 0.000000000000000000, 0.000000000000000000, 1.000000000000000000 ) ) ;
#51904 = CIRCLE ( 'NONE', #62453, 5.000000000000000888 ) ;
#51905 = CARTESIAN_POINT ( 'NONE',  ( -37.00000000000000711, 11.23004253107764505, 4.732539170486304236 ) ) ;
#51906 = DIRECTION ( 'NONE',  ( 0.000000000000000000, 0.01356324068817998940, -0.9999080150203990547 ) ) ;
#51907 = DIRECTION ( 'NONE',  ( -1.000000000000000000, 0.000000000000000000, 0.000000000000000000 ) ) ;
#51908 = ADVANCED_FACE ( 'NONE', ( #26085 ), #495, .T. ) ;
#51909 = CIRCLE ( 'NONE', #60375, 12.74999999999999822 ) ;
#51910 = VERTEX_POINT ( 'NONE', #41029 ) ;
#51911 = ADVANCED_FACE ( 'NONE', ( #15102 ), #14756, .T. ) ;
#51912 = VECTOR ( 'NONE', #16322, 1000.000000000000000 ) ;
#51913 = EDGE_LOOP ( 'NONE', ( #25324, #57412, #2441, #8807 ) ) ;
#51914 = CARTESIAN_POINT ( 'NONE',  ( 2.717984159219906992, -6.602931111513720808, 4.139692542159457034 ) ) ;
#51915 = CARTESIAN_POINT ( 'NONE',  ( 40.80553070818749006, -1.699139512677865227, -18.07784515657013102 ) ) ;
#51916 = DIRECTION ( 'NONE',  ( 0.000000000000000000, -0.04924826701375289995, -0.9987865678893274035 ) ) ;
#51917 = AXIS2_PLACEMENT_3D ( 'NONE', #25606, #3, #35241 ) ;
#51918 = LINE ( 'NONE', #16975, #41381 ) ;
#51919 = ORIENTED_EDGE ( 'NONE', *, *, #1136, .T. ) ;
#51920 = ORIENTED_EDGE ( 'NONE', *, *, #33904, .T. ) ;
#51921 = AXIS2_PLACEMENT_3D ( 'NONE', #50157, #56798, #4612 ) ;
#51922 = ORIENTED_EDGE ( 'NONE', *, *, #7585, .T. ) ;
#51923 = DIRECTION ( 'NONE',  ( 1.000000000000000000, 0.000000000000000000, 0.000000000000000000 ) ) ;
#51924 = LINE ( 'NONE', #50935, #11948 ) ;
#51926 = EDGE_CURVE ( 'NONE', #47572, #31395, #2319, .T. ) ;
#51925 = VERTEX_POINT ( 'NONE', #55348 ) ;
#51927 = CARTESIAN_POINT ( 'NONE',  ( -17.97366836756218689, 4.334172528176946315, -11.19214901861635170 ) ) ;
#51928 = DIRECTION ( 'NONE',  ( 0.000000000000000000, 0.000000000000000000, 1.000000000000000000 ) ) ;
#51929 = ORIENTED_EDGE ( 'NONE', *, *, #58622, .F. ) ;
#51930 = CARTESIAN_POINT ( 'NONE',  ( -27.08417568107324058, -0.3682236895270647459, -2.261355310631429916 ) ) ;
#51931 = CARTESIAN_POINT ( 'NONE',  ( 18.88852658721880928, -29.92669765328984255, -6.766054962673559992 ) ) ;
#51932 = CARTESIAN_POINT ( 'NONE',  ( 24.43856487734552019, -2.854323001380032032, 11.65700061237547658 ) ) ;
#51933 = ORIENTED_EDGE ( 'NONE', *, *, #5187, .F. ) ;
#51934 = CARTESIAN_POINT ( 'NONE',  ( -37.00000000000000711, 8.352657516904674395, 8.258652103341463047 ) ) ;
#51935 = ORIENTED_EDGE ( 'NONE', *, *, #62219, .T. ) ;
#51936 = CARTESIAN_POINT ( 'NONE',  ( 35.00000000000000000, 4.705694406421931860E-17, -3.469127814946512892E-15 ) ) ;
#51937 = ORIENTED_EDGE ( 'NONE', *, *, #29794, .T. ) ;
#51938 = CARTESIAN_POINT ( 'NONE',  ( 2.241451721903214178, 4.860585618235972127, 5.887257931662863264 ) ) ;
#51939 = LINE ( 'NONE', #41276, #58528 ) ;
#51940 = CARTESIAN_POINT ( 'NONE',  ( 36.00000000000000711, 11.59605747147793942, 5.300372733891517640 ) ) ;
#51942 = DIRECTION ( 'NONE',  ( 1.000000000000000000, 0.000000000000000000, 0.000000000000000000 ) ) ;
#51941 = AXIS2_PLACEMENT_3D ( 'NONE', #12284, #2994, #42200 ) ;
#51943 = CARTESIAN_POINT ( 'NONE',  ( 9.953255994279757601, 1.096471986029277312, 11.95103177947028605 ) ) ;
#51944 = CYLINDRICAL_SURFACE ( 'NONE', #34499, 13.50000000000000178 ) ;
#51945 = DIRECTION ( 'NONE',  ( -1.000000000000000000, 0.000000000000000000, 0.000000000000000000 ) ) ;
#51946 = EDGE_LOOP ( 'NONE', ( #1576, #51754, #42262, #63714 ) ) ;
#51947 = DIRECTION ( 'NONE',  ( -1.000000000000000000, 0.000000000000000000, 0.000000000000000000 ) ) ;
#51948 = EDGE_CURVE ( 'NONE', #32729, #19643, #803, .T. ) ;
#51949 = VERTEX_POINT ( 'NONE', #5484 ) ;
#51950 = CIRCLE ( 'NONE', #24302, 5.000000000000000888 ) ;
#51951 = CARTESIAN_POINT ( 'NONE',  ( 2.507146904658100972, -5.774795220010153329, -5.128007631637124142 ) ) ;
#51952 = EDGE_LOOP ( 'NONE', ( #51441, #26867, #7245, #3460 ) ) ;
#51953 = CARTESIAN_POINT ( 'NONE',  ( -17.49435431676402786, 7.621753754644457146, 9.270964220055409655 ) ) ;
#51954 = DIRECTION ( 'NONE',  ( -1.000000000000000000, -0.000000000000000000, -0.000000000000000000 ) ) ;
#51955 = DIRECTION ( 'NONE',  ( 0.000000000000000000, -0.01356324068817998940, 0.9999080150203990547 ) ) ;
#51956 = VECTOR ( 'NONE', #28189, 1000.000000000000000 ) ;
#51957 = AXIS2_PLACEMENT_3D ( 'NONE', #19839, #38816, #19178 ) ;
#51958 = CARTESIAN_POINT ( 'NONE',  ( 2.244591118395374174, 7.211060161905881394, 2.510215291313116381 ) ) ;
#51959 = ADVANCED_FACE ( 'NONE', ( #50383 ), #5852, .F. ) ;
#51960 = ORIENTED_EDGE ( 'NONE', *, *, #32394, .T. ) ;
#51961 = CARTESIAN_POINT ( 'NONE',  ( 0.3665391374699465965, -7.691255657244358446, 9.576575648338991442 ) ) ;
#51962 = AXIS2_PLACEMENT_3D ( 'NONE', #6268, #61133, #56128 ) ;
#51963 = ORIENTED_EDGE ( 'NONE', *, *, #8732, .F. ) ;
#51964 = CARTESIAN_POINT ( 'NONE',  ( 2.994568964204194383, -6.289764245798251885, 4.756002438591050208 ) ) ;
#51965 = LINE ( 'NONE', #52933, #63191 ) ;
#51966 = DIRECTION ( 'NONE',  ( -1.000000000000000000, 0.000000000000000000, 0.000000000000000000 ) ) ;
#51967 = EDGE_CURVE ( 'NONE', #23545, #16620, #7096, .T. ) ;
#51968 = ORIENTED_EDGE ( 'NONE', *, *, #48956, .F. ) ;
#51969 = VECTOR ( 'NONE', #24072, 1000.000000000000000 ) ;
#51970 = CARTESIAN_POINT ( 'NONE',  ( 0.3675815128205894289, -4.447030445008105737, -11.44679196252413789 ) ) ;
#51971 = EDGE_CURVE ( 'NONE', #26131, #22816, #52348, .T. ) ;
#51972 = LINE ( 'NONE', #62255, #7438 ) ;
#51973 = LINE ( 'NONE', #61179, #16127 ) ;
#51974 = CARTESIAN_POINT ( 'NONE',  ( 37.00000000000000711, 11.74614673114903773, 0.01609748574448878478 ) ) ;
#51975 = CARTESIAN_POINT ( 'NONE',  ( 35.00000000000000000, 0.7536123767498499326, -11.72195762423410414 ) ) ;
#51976 = DIRECTION ( 'NONE',  ( -0.8867529933577791290, 0.000000000000000000, -0.4622435816439406930 ) ) ;
#51977 = CARTESIAN_POINT ( 'NONE',  ( 1.459561108992812439, 4.912799202118954156, 11.65083230253652324 ) ) ;
#51978 = CARTESIAN_POINT ( 'NONE',  ( 1.719304012340734822, -3.626341562669572305, -12.20344780066098345 ) ) ;
#51979 = ADVANCED_FACE ( 'NONE', ( #1481 ), #38003, .T. ) ;
#51980 = AXIS2_PLACEMENT_3D ( 'NONE', #54432, #18541, #9173 ) ;
#51981 = ORIENTED_EDGE ( 'NONE', *, *, #48789, .T. ) ;
#51982 = DIRECTION ( 'NONE',  ( 1.000000000000000000, -0.000000000000000000, -0.000000000000000000 ) ) ;
#51983 = DIRECTION ( 'NONE',  ( -0.7290028908350527637, 0.000000000000000000, 0.6845106172691086677 ) ) ;
#51984 = ORIENTED_EDGE ( 'NONE', *, *, #11308, .F. ) ;
#51985 = CYLINDRICAL_SURFACE ( 'NONE', #2585, 4.094603870727468120 ) ;
#51986 = CARTESIAN_POINT ( 'NONE',  ( 0.6844764289427172077, 0.5169738502507784661, -11.99252702960889927 ) ) ;
#51987 = ORIENTED_EDGE ( 'NONE', *, *, #16980, .F. ) ;
#51988 = DIRECTION ( 'NONE',  ( 1.000000000000000000, 0.000000000000000000, -0.000000000000000000 ) ) ;
#51989 = ORIENTED_EDGE ( 'NONE', *, *, #7728, .F. ) ;
#51990 = CARTESIAN_POINT ( 'NONE',  ( 0.3632410797595241880, -5.910360611678902032, 10.76277061791638801 ) ) ;
#51991 = EDGE_LOOP ( 'NONE', ( #37643, #6786, #31144, #30335 ) ) ;
#51992 = ORIENTED_EDGE ( 'NONE', *, *, #34746, .F. ) ;
#51993 = CIRCLE ( 'NONE', #16961, 5.000000000000001776 ) ;
#51994 = EDGE_CURVE ( 'NONE', #42367, #43621, #49164, .T. ) ;
#51995 = CARTESIAN_POINT ( 'NONE',  ( -27.32343372485685862, -1.382463360572550259, -2.674948176236203512 ) ) ;
#51996 = VERTEX_POINT ( 'NONE', #17069 ) ;
#51997 = CARTESIAN_POINT ( 'NONE',  ( -25.16596872619400216, -6.639998712458014651, 10.00200833204654494 ) ) ;
#51998 = CARTESIAN_POINT ( 'NONE',  ( 1.198791140419921630, -11.61358959650685208, -4.776130053253331731 ) ) ;
#51999 = CARTESIAN_POINT ( 'NONE',  ( 3.152665057734113319, -5.461013642405577073, 5.761241965769066553 ) ) ;
#52000 = DIRECTION ( 'NONE',  ( 0.000000000000000000, 0.000000000000000000, -1.000000000000000000 ) ) ;
#52001 = ORIENTED_EDGE ( 'NONE', *, *, #45424, .T. ) ;
#52002 = CARTESIAN_POINT ( 'NONE',  ( 0.2638984909335716500, 4.001111175853742985, 11.57533005135180382 ) ) ;
#52003 = CARTESIAN_POINT ( 'NONE',  ( -3.456075311296388453, -27.96820792850356341, 12.23233986317338129 ) ) ;
#52004 = CARTESIAN_POINT ( 'NONE',  ( 0.000000000000000000, 5.662015959325201742, 4.918493191653995567 ) ) ;
#52006 = ORIENTED_EDGE ( 'NONE', *, *, #57277, .F. ) ;
#52005 = DIRECTION ( 'NONE',  ( 0.000000000000000000, 0.01356324068817998940, -0.9999080150203989437 ) ) ;
#52007 = CARTESIAN_POINT ( 'NONE',  ( -35.00000000000000000, -11.16627499335652374, -3.645068577060142978 ) ) ;
#52008 = ORIENTED_EDGE ( 'NONE', *, *, #45656, .F. ) ;
#52009 = LINE ( 'NONE', #41352, #1977 ) ;
#52010 = AXIS2_PLACEMENT_3D ( 'NONE', #65160, #45527, #30886 ) ;
#52011 = VERTEX_POINT ( 'NONE', #6451 ) ;
#52012 = CARTESIAN_POINT ( 'NONE',  ( -10.00000000000000178, 0.000000000000000000, 0.000000000000000000 ) ) ;
#52013 = DIRECTION ( 'NONE',  ( -0.000000000000000000, -0.000000000000000000, -1.000000000000000000 ) ) ;
#52014 = DIRECTION ( 'NONE',  ( 1.000000000000000000, 0.000000000000000000, 0.000000000000000000 ) ) ;
#52015 = ORIENTED_EDGE ( 'NONE', *, *, #36622, .T. ) ;
#52016 = CARTESIAN_POINT ( 'NONE',  ( 0.3675815128205894289, 8.093875121226078662, 9.235491948680033758 ) ) ;
#52017 = CARTESIAN_POINT ( 'NONE',  ( -22.27384469013076185, -2.154627400808021509, -2.985904959940910874 ) ) ;
#52018 = CARTESIAN_POINT ( 'NONE',  ( 0.3632410797595232443, -12.04386719438561570, 2.390576695689066167 ) ) ;
#52019 = B_SPLINE_CURVE_WITH_KNOTS ( 'NONE', 3,
 ( #50950, #20028, #60261, #65558, #40293, #15364, #5399, #29999, #20351, #40633, #56248, #64909, #34965, #24354, #35637, #19390, #55271, #34649, #39655, #59957, #54945, #9374, #29659, #52604, #26010, #46605 ),
 .UNSPECIFIED., .F., .F.,
 ( 4, 2, 2, 2, 2, 2, 2, 2, 2, 2, 2, 2, 4 ),
 ( 7.152448122690996019E-18, 0.001355494837136931013, 0.002033242255705391098, 0.002710989674273851183, 0.004066484511410767451, 0.004744231929979227103, 0.005421979348547687622, 0.006099726767116149875, 0.006777474185684612996, 0.007455221604253076118, 0.008132969022821540106, 0.009488463859958469818, 0.01084395869709539779 ),
 .UNSPECIFIED. ) ;
#52020 = VERTEX_POINT ( 'NONE', #22736 ) ;
#52021 = EDGE_CURVE ( 'NONE', #29441, #65378, #12397, .T. ) ;
#52022 = ORIENTED_EDGE ( 'NONE', *, *, #7127, .T. ) ;
#52023 = LINE ( 'NONE', #58002, #46543 ) ;
#52024 = VERTEX_POINT ( 'NONE', #22060 ) ;
#52025 = EDGE_CURVE ( 'NONE', #52648, #33594, #39444, .T. ) ;
#52026 = ORIENTED_EDGE ( 'NONE', *, *, #52569, .F. ) ;
#52027 = DIRECTION ( 'NONE',  ( 1.000000000000000000, 0.000000000000000000, -0.000000000000000000 ) ) ;
#52028 = CARTESIAN_POINT ( 'NONE',  ( 35.00000000000000000, 2.185196060784047045, 11.54110654723646157 ) ) ;
#52029 = CARTESIAN_POINT ( 'NONE',  ( -37.25000000000000711, 5.493969937218003549E-16, -4.500000000000000888 ) ) ;
#52030 = CARTESIAN_POINT ( 'NONE',  ( 0.000000000000000000, -0.7281529553921430864, -7.464569195442815719 ) ) ;
#52031 = CARTESIAN_POINT ( 'NONE',  ( -37.00000000000000711, -5.927257550915394191, 10.64792938439753378 ) ) ;
#52032 = FACE_OUTER_BOUND ( 'NONE', #25022, .T. ) ;
#52033 = AXIS2_PLACEMENT_3D ( 'NONE', #33240, #52871, #38558 ) ;
#52034 = VECTOR ( 'NONE', #2980, 1000.000000000000000 ) ;
#52035 = ADVANCED_FACE ( 'NONE', ( #52978 ), #17744, .T. ) ;
#52036 = CARTESIAN_POINT ( 'NONE',  ( 1.719304012342639965, 12.38166659047149487, -2.961219984262613458 ) ) ;
#52037 = ORIENTED_EDGE ( 'NONE', *, *, #53318, .F. ) ;
#52038 = LINE ( 'NONE', #37047, #64651 ) ;
#52039 = ADVANCED_FACE ( 'NONE', ( #27699 ), #1134, .T. ) ;
#52040 = CARTESIAN_POINT ( 'NONE',  ( -4.023342348990911255, -9.886260852804344523, 6.816691047944269499 ) ) ;
#52041 = CARTESIAN_POINT ( 'NONE',  ( 2.000000000000001776, 0.000000000000000000, 0.000000000000000000 ) ) ;
#52042 = B_SPLINE_CURVE_WITH_KNOTS ( 'NONE', 3,
 ( #14489, #55069, #50433, #23517, #41743, #20150, #20486, #46410, #16149, #60722 ),
 .UNSPECIFIED., .F., .F.,
 ( 4, 3, 3, 4 ),
 ( 9.215718466126787689E-19, 6.607638129004467199E-05, 9.911389841680512771E-05, 0.0001667630577588622028 ),
 .UNSPECIFIED. ) ;
#52043 = CARTESIAN_POINT ( 'NONE',  ( -35.00000000000000000, 0.000000000000000000, 0.000000000000000000 ) ) ;
#52044 = EDGE_CURVE ( 'NONE', #30121, #48464, #12726, .T. ) ;
#52045 =( BOUNDED_CURVE ( )  B_SPLINE_CURVE ( 3, ( #43723, #64004, #18487, #38743 ),
 .UNSPECIFIED., .F., .F. ) 
 B_SPLINE_CURVE_WITH_KNOTS ( ( 4, 4 ),
 ( 1.841109206681600385, 1.865537793031380120 ),
 .UNSPECIFIED. ) 
 CURVE ( )  GEOMETRIC_REPRESENTATION_ITEM ( )  RATIONAL_B_SPLINE_CURVE ( ( 1.000000000000000000, 0.9999502709656691302, 0.9999502709656691302, 1.000000000000000000 ) ) 
 REPRESENTATION_ITEM ( '' )  );
#52046 = CARTESIAN_POINT ( 'NONE',  ( 0.2653519890518179492, 12.06014856238023469, -2.126538543977954721 ) ) ;
#52047 = CARTESIAN_POINT ( 'NONE',  ( -27.08429572838383947, 2.217805374070540125, -0.5764601019425888984 ) ) ;
#52048 = ORIENTED_EDGE ( 'NONE', *, *, #65519, .T. ) ;
#52049 = DIRECTION ( 'NONE',  ( 0.3939253465568944290, -0.8603393047164960006, -0.3234796780324333820 ) ) ;
#52050 = CARTESIAN_POINT ( 'NONE',  ( 2.941278708680199916, 5.383216837018941270, 2.952340773940127949 ) ) ;
#52051 = CARTESIAN_POINT ( 'NONE',  ( -25.54417658651491863, 4.240019242199842608, 11.22596262356930197 ) ) ;
#52052 = CARTESIAN_POINT ( 'NONE',  ( 2.000000000000001776, -6.936109781200700652, 2.853135311045000400 ) ) ;
#52053 = AXIS2_PLACEMENT_3D ( 'NONE', #49800, #8572, #18891 ) ;
#52054 = DIRECTION ( 'NONE',  ( 1.000000000000000000, -0.000000000000000000, -0.000000000000000000 ) ) ;
#52055 = CARTESIAN_POINT ( 'NONE',  ( 3.152665057733776699, 4.377619405892044568, -6.622010822086680015 ) ) ;
#52056 = VERTEX_POINT ( 'NONE', #62289 ) ;
#52057 = DIRECTION ( 'NONE',  ( -1.000000000000000000, -0.000000000000000000, 0.000000000000000000 ) ) ;
#52058 = CARTESIAN_POINT ( 'NONE',  ( 2.354167843600960097, -6.278647867796540716, 25.00000000000000000 ) ) ;
#52059 = CARTESIAN_POINT ( 'NONE',  ( -27.19357181888462094, -12.48377454417556542, 5.138615876886901468 ) ) ;
#52060 = ORIENTED_EDGE ( 'NONE', *, *, #63777, .T. ) ;
#52061 = CARTESIAN_POINT ( 'NONE',  ( 0.000000000000000000, 5.662015959325264802, -4.918493191653922736 ) ) ;
#52062 = DIRECTION ( 'NONE',  ( 1.000000000000000000, 0.000000000000000000, 0.000000000000000000 ) ) ;
#52063 = CARTESIAN_POINT ( 'NONE',  ( 0.2655924914740778742, -10.62761259256412671, -6.084990060696620517 ) ) ;
#52065 = ORIENTED_EDGE ( 'NONE', *, *, #1952, .F. ) ;
#52064 = CARTESIAN_POINT ( 'NONE',  ( 35.00000000000000000, -6.280308599560208371, -9.926225166347007800 ) ) ;
#52066 = CARTESIAN_POINT ( 'NONE',  ( 2.000000000000001776, -3.859771122242995123, -5.613913289150092467 ) ) ;
#52067 = ADVANCED_FACE ( 'NONE', ( #16744 ), #11426, .T. ) ;
#52068 = AXIS2_PLACEMENT_3D ( 'NONE', #31830, #52145, #1613 ) ;
#52069 = CIRCLE ( 'NONE', #12793, 12.18649999999999878 ) ;
#52070 = CARTESIAN_POINT ( 'NONE',  ( 3.152665057734040488, 0.000000000000000000, 0.000000000000000000 ) ) ;
#52071 = ORIENTED_EDGE ( 'NONE', *, *, #47635, .F. ) ;
#52072 = DIRECTION ( 'NONE',  ( -1.000000000000000000, 0.000000000000000000, 0.000000000000000000 ) ) ;
#52073 = DIRECTION ( 'NONE',  ( 0.2475719085175098200, -2.922992529533354589E-16, -0.9688695217174487784 ) ) ;
#52074 = CARTESIAN_POINT ( 'NONE',  ( -27.20102706715914209, -2.585824624629331492, -0.5453431011645174520 ) ) ;
#52075 = DIRECTION ( 'NONE',  ( 0.000000000000000000, 0.000000000000000000, 1.000000000000000000 ) ) ;
#52076 = CARTESIAN_POINT ( 'NONE',  ( 10.48620311856346454, 8.250315036047107142, 25.00000000000000000 ) ) ;
#52077 = CARTESIAN_POINT ( 'NONE',  ( 35.00000000000000000, 11.17622378668006355, -3.614449339633533764 ) ) ;
#52079 = ORIENTED_EDGE ( 'NONE', *, *, #40871, .F. ) ;
#52078 = CARTESIAN_POINT ( 'NONE',  ( 0.2739690278137280055, 11.44648082006011869, -4.360944092821339879 ) ) ;
#52080 = B_SPLINE_CURVE_WITH_KNOTS ( 'NONE', 3,
 ( #740, #32292, #7346, #42934, #37280, #31957, #12338, #1409, #11359, #46612, #16365, #47932, #2044, #22308, #52609, #6385 ),
 .UNSPECIFIED., .F., .F.,
 ( 4, 3, 3, 3, 3, 4 ),
 ( 0.000000000000000000, 0.0002999043160757426532, 0.0005998071753051154205, 0.0008997092107374793889, 0.001204458948196636056, 0.001510329163478481979 ),
 .UNSPECIFIED. ) ;
#52081 = VERTEX_POINT ( 'NONE', #32359 ) ;
#52082 = CARTESIAN_POINT ( 'NONE',  ( 0.000000000000000000, 6.253963800348250501, 4.139799123621038746 ) ) ;
#52083 = ORIENTED_EDGE ( 'NONE', *, *, #48152, .T. ) ;
#52084 = LINE ( 'NONE', #32436, #18838 ) ;
#52085 = VECTOR ( 'NONE', #63271, 1000.000000000000000 ) ;
#52086 = ADVANCED_FACE ( 'NONE', ( #62953 ), #37017, .T. ) ;
#52087 = FACE_OUTER_BOUND ( 'NONE', #57321, .T. ) ;
#52089 = EDGE_LOOP ( 'NONE', ( #32986, #48905, #52340, #58630 ) ) ;
#52088 = AXIS2_PLACEMENT_3D ( 'NONE', #11075, #30368, #20388 ) ;
#52090 = CARTESIAN_POINT ( 'NONE',  ( -35.00000000000000000, 12.12087942037211263, -1.262958560998631796 ) ) ;
#52091 = DIRECTION ( 'NONE',  ( -1.000000000000000000, 0.000000000000000000, 0.000000000000000000 ) ) ;
#52092 = ADVANCED_FACE ( 'NONE', ( #28365 ), #44078, .F. ) ;
#52093 = DIRECTION ( 'NONE',  ( 0.000000000000000000, 0.9289767198167924178, -0.3701381553399118451 ) ) ;
#52094 = VERTEX_POINT ( 'NONE', #39650 ) ;
#52095 = ORIENTED_EDGE ( 'NONE', *, *, #29704, .T. ) ;
#52096 = CARTESIAN_POINT ( 'NONE',  ( 2.524535260912411871, 7.569872524928948465, -1.559291270914444638 ) ) ;
#52097 = ADVANCED_FACE ( 'NONE', ( #8749 ), #48377, .F. ) ;
#52098 = ORIENTED_EDGE ( 'NONE', *, *, #56558, .T. ) ;
#52099 = CIRCLE ( 'NONE', #23424, 12.74999999999999822 ) ;
#52100 = DIRECTION ( 'NONE',  ( 1.000000000000000000, -0.000000000000000000, 0.000000000000000000 ) ) ;
#52101 = FACE_OUTER_BOUND ( 'NONE', #42408, .T. ) ;
#52102 = CARTESIAN_POINT ( 'NONE',  ( 35.00000000000000000, -10.64792938439759595, -5.927257550915285833 ) ) ;
#52103 = CARTESIAN_POINT ( 'NONE',  ( -27.08430418657510685, 0.9470735946412849326, -2.086666645150412336 ) ) ;
#52104 = DIRECTION ( 'NONE',  ( -1.000000000000000000, 0.000000000000000000, 0.000000000000000000 ) ) ;
#52105 = CARTESIAN_POINT ( 'NONE',  ( 2.373367633546870525, -7.591069096729003540, 1.154895193356608063 ) ) ;
#52106 = ADVANCED_FACE ( 'NONE', ( #54646 ), #63594, .F. ) ;
#52107 = CARTESIAN_POINT ( 'NONE',  ( 36.00000000000000711, -12.57916205664482767, -2.080187960898522537 ) ) ;
#52108 = AXIS2_PLACEMENT_3D ( 'NONE', #35127, #25495, #56417 ) ;
#52109 = ORIENTED_EDGE ( 'NONE', *, *, #1173, .T. ) ;
#52110 = CARTESIAN_POINT ( 'NONE',  ( 0.3675815128205894289, 12.27743992903066328, -0.2638082659428851451 ) ) ;
#52111 = ADVANCED_FACE ( 'NONE', ( #29030 ), #50884, .F. ) ;
#52112 = ORIENTED_EDGE ( 'NONE', *, *, #48685, .F. ) ;
#52113 = CIRCLE ( 'NONE', #54260, 12.74999999999999822 ) ;
#52114 = FACE_OUTER_BOUND ( 'NONE', #56261, .T. ) ;
#52115 = CARTESIAN_POINT ( 'NONE',  ( -35.04709527796842394, 0.001082316405385738700, -0.01231589140599127774 ) ) ;
#52116 = FACE_OUTER_BOUND ( 'NONE', #59864, .T. ) ;
#52117 = CARTESIAN_POINT ( 'NONE',  ( 2.259830038564999199, -3.938923657569452619, 6.546987858513363179 ) ) ;
#52118 = DIRECTION ( 'NONE',  ( -1.000000000000000000, 0.000000000000000000, 0.000000000000000000 ) ) ;
#52119 = CARTESIAN_POINT ( 'NONE',  ( 1.000000000000000888, -6.664893814313742837, 3.439359016433467087 ) ) ;
#52120 = EDGE_CURVE ( 'NONE', #57823, #61028, #54343, .T. ) ;
#52121 = VERTEX_POINT ( 'NONE', #58983 ) ;
#52122 = CIRCLE ( 'NONE', #33020, 4.999999999999999112 ) ;
#52123 = CIRCLE ( 'NONE', #60611, 5.000000000000001776 ) ;
#52124 = ORIENTED_EDGE ( 'NONE', *, *, #3565, .F. ) ;
#52125 = VECTOR ( 'NONE', #62354, 1000.000000000000000 ) ;
#52126 = DIRECTION ( 'NONE',  ( 1.000000000000000000, -0.000000000000000000, 0.000000000000000000 ) ) ;
#52127 = ADVANCED_FACE ( 'NONE', ( #8096 ), #61937, .F. ) ;
#52128 = ORIENTED_EDGE ( 'NONE', *, *, #2604, .F. ) ;
#52129 = AXIS2_PLACEMENT_3D ( 'NONE', #22835, #62080, #37113 ) ;
#52130 = DIRECTION ( 'NONE',  ( 0.000000000000000000, 0.9635499925192236859, -0.2675283385292183680 ) ) ;
#52131 = DIRECTION ( 'NONE',  ( 0.000000000000000000, -0.01356324068817992175, 0.9999080150203990547 ) ) ;
#52132 = EDGE_CURVE ( 'NONE', #17330, #65715, #6527, .T. ) ;
#52133 = LINE ( 'NONE', #1603, #62804 ) ;
#52134 = LINE ( 'NONE', #31818, #31778 ) ;
#52135 = ORIENTED_EDGE ( 'NONE', *, *, #60361, .T. ) ;
#52136 = CARTESIAN_POINT ( 'NONE',  ( 0.3632410797595242991, 12.13515851238022591, 1.872837903657238234 ) ) ;
#52137 = CARTESIAN_POINT ( 'NONE',  ( 35.00000000000000000, 4.339012074899953220, -10.91536515067649660 ) ) ;
#52138 = CARTESIAN_POINT ( 'NONE',  ( 1.459561108992816436, -1.570807238541338524, 12.54631635028845515 ) ) ;
#52139 = DIRECTION ( 'NONE',  ( -1.000000000000000000, -1.836970198721029688E-16, 0.000000000000000000 ) ) ;
#52140 = VECTOR ( 'NONE', #27536, 1000.000000000000000 ) ;
#52141 = AXIS2_PLACEMENT_3D ( 'NONE', #33626, #27002, #47298 ) ;
#52142 = AXIS2_PLACEMENT_3D ( 'NONE', #23679, #18698, #38956 ) ;
#52143 = CARTESIAN_POINT ( 'NONE',  ( 0.2956976708475442805, 6.317697191869785733, -10.50256636126820453 ) ) ;
#52144 = AXIS2_PLACEMENT_3D ( 'NONE', #37156, #31838, #6601 ) ;
#52145 = DIRECTION ( 'NONE',  ( 1.000000000000000000, 0.000000000000000000, 0.000000000000000000 ) ) ;
#52146 = ORIENTED_EDGE ( 'NONE', *, *, #8194, .F. ) ;
#52147 = VECTOR ( 'NONE', #12471, 1000.000000000000000 ) ;
#52148 = CARTESIAN_POINT ( 'NONE',  ( -15.04954985558960878, -34.74586518154888637, -6.983850705393018998 ) ) ;
#52149 = ORIENTED_EDGE ( 'NONE', *, *, #1173, .F. ) ;
#52150 = FACE_OUTER_BOUND ( 'NONE', #7265, .T. ) ;
#52151 = CARTESIAN_POINT ( 'NONE',  ( 0.3675815128205912052, 6.367184624550311867, -10.50067073900645198 ) ) ;
#52152 = CONICAL_SURFACE ( 'NONE', #60631, 7.938172270156617749, 1.280189991382167047 ) ;
#52153 = FACE_OUTER_BOUND ( 'NONE', #2518, .T. ) ;
#52154 = CYLINDRICAL_SURFACE ( 'NONE', #43701, 12.18649999999999878 ) ;
#52155 = EDGE_CURVE ( 'NONE', #55446, #62557, #58653, .T. ) ;
#52156 = ORIENTED_EDGE ( 'NONE', *, *, #22188, .T. ) ;
#52157 = VERTEX_POINT ( 'NONE', #13077 ) ;
#52158 = FACE_OUTER_BOUND ( 'NONE', #34700, .T. ) ;
#52159 = ORIENTED_EDGE ( 'NONE', *, *, #50092, .T. ) ;
#52160 = CARTESIAN_POINT ( 'NONE',  ( 3.403981455603509065, 7.616542962421854135, 9.282725052014482614 ) ) ;
#52161 = DIRECTION ( 'NONE',  ( 0.000000000000000000, -0.9289767198167871998, -0.3701381553399247792 ) ) ;
#52162 = DIRECTION ( 'NONE',  ( -1.000000000000000000, 0.000000000000000000, 0.000000000000000000 ) ) ;
#52163 = CARTESIAN_POINT ( 'NONE',  ( -37.00000000000000711, 0.000000000000000000, 0.000000000000000000 ) ) ;
#52164 = CARTESIAN_POINT ( 'NONE',  ( 2.430348790455934882, 7.694949746373333177, -0.1949172018036633425 ) ) ;
#52165 = B_SPLINE_CURVE_WITH_KNOTS ( 'NONE', 3,
 ( #56251, #37537, #22912, #43165, #40966, #46296, #7263, #7604, #28218, #12916, #10693, #36293, #57841, #5745, #33197, #736, #12259, #20995, #26324 ),
 .UNSPECIFIED., .F., .F.,
 ( 4, 3, 3, 3, 3, 3, 4 ),
 ( 6.662331925613552201E-18, 2.825908398831382330E-05, 4.208813692483990936E-05, 5.591713746943949807E-05, 6.279584083232014977E-05, 9.105792820296881071E-05, 0.0001153131102488856488 ),
 .UNSPECIFIED. ) ;
#52166 = CARTESIAN_POINT ( 'NONE',  ( 2.251139882114759239, 5.770207524085092743, 5.003859976904558415 ) ) ;
#52167 = CARTESIAN_POINT ( 'NONE',  ( 1.375507693222091099, 12.51366828189792635, -1.606074886183993744 ) ) ;
#52168 = VERTEX_POINT ( 'NONE', #34333 ) ;
#52169 = AXIS2_PLACEMENT_3D ( 'NONE', #132, #40028, #5127 ) ;
#52170 = EDGE_CURVE ( 'NONE', #12280, #3409, #3369, .T. ) ;
#52171 = CARTESIAN_POINT ( 'NONE',  ( 0.2646305136544072623, -10.67138229758233692, 6.008537389229382519 ) ) ;
#52172 = VERTEX_POINT ( 'NONE', #53970 ) ;
#52173 = B_SPLINE_CURVE_WITH_KNOTS ( 'NONE', 3,
 ( #2064, #7052, #27325, #22328, #42599, #2413, #19002, #23014, #59246, #2758, #63886, #37960, #43596, #27648, #34285, #8365 ),
 .UNSPECIFIED., .F., .F.,
 ( 4, 3, 3, 3, 3, 4 ),
 ( 0.000000000000000000, 6.991367980366665303E-05, 0.0001398269368981414106, 0.0002097400188389170336, 0.0002811534801551458644, 0.0003526297678872614009 ),
 .UNSPECIFIED. ) ;
#52174 = CARTESIAN_POINT ( 'NONE',  ( -37.00000000000000711, 8.624332853796195408, -9.390600770287900190 ) ) ;
#52175 = CARTESIAN_POINT ( 'NONE',  ( 21.59694336868049902, -12.74990532528425291, -4.441854890391109478 ) ) ;
#52177 = CARTESIAN_POINT ( 'NONE',  ( 37.00000000000000711, 4.705694406421931860E-17, -3.469127814946512892E-15 ) ) ;
#52176 = VECTOR ( 'NONE', #62428, 1000.000000000000000 ) ;
#52178 = VECTOR ( 'NONE', #61279, 1000.000000000000000 ) ;
#52179 = CIRCLE ( 'NONE', #33064, 2.899999999999994138 ) ;
#52180 = ADVANCED_FACE ( 'NONE', ( #44302 ), #39311, .T. ) ;
#52181 = CARTESIAN_POINT ( 'NONE',  ( 35.00000000000000000, -9.677500615117850202, 6.657191900728419043 ) ) ;
#52182 = ORIENTED_EDGE ( 'NONE', *, *, #29161, .T. ) ;
#52183 = DIRECTION ( 'NONE',  ( 1.000000000000000000, -0.000000000000000000, -0.000000000000000000 ) ) ;
#52184 = CARTESIAN_POINT ( 'NONE',  ( -18.91767133624980701, -29.93867241416544189, -6.768471019338287320 ) ) ;
#52185 = DIRECTION ( 'NONE',  ( -1.000000000000000000, -0.000000000000000000, 0.000000000000000000 ) ) ;
#52186 = ORIENTED_EDGE ( 'NONE', *, *, #43297, .F. ) ;
#52187 = ORIENTED_EDGE ( 'NONE', *, *, #7460, .F. ) ;
#52188 = CARTESIAN_POINT ( 'NONE',  ( 3.435435718939642946, 5.961994453915724357, 12.11397542276001538 ) ) ;
#52189 = EDGE_CURVE ( 'NONE', #49613, #30052, #61552, .T. ) ;
#52190 = EDGE_LOOP ( 'NONE', ( #27286, #16367 ) ) ;
#52191 = VERTEX_POINT ( 'NONE', #24690 ) ;
#52192 = EDGE_LOOP ( 'NONE', ( #51000, #6450, #37792, #45764 ) ) ;
#52193 = ORIENTED_EDGE ( 'NONE', *, *, #45729, .F. ) ;
#52194 = CIRCLE ( 'NONE', #6574, 12.18650000000000055 ) ;
#52195 = CARTESIAN_POINT ( 'NONE',  ( 2.241449424704146320, -7.152834201978780726, 2.668712484599937707 ) ) ;
#52196 = CYLINDRICAL_SURFACE ( 'NONE', #49645, 13.50000000000000178 ) ;
#52197 = VECTOR ( 'NONE', #57884, 1000.000000000000000 ) ;
#52198 = CARTESIAN_POINT ( 'NONE',  ( 2.000000000000001776, 0.000000000000000000, 0.000000000000000000 ) ) ;
#52199 = DIRECTION ( 'NONE',  ( 1.000000000000000000, -0.000000000000000000, -0.000000000000000000 ) ) ;
#52200 = DIRECTION ( 'NONE',  ( 0.000000000000000000, 0.01356324068817992175, -0.9999080150203990547 ) ) ;
#52201 = ORIENTED_EDGE ( 'NONE', *, *, #20140, .T. ) ;
#52202 = CARTESIAN_POINT ( 'NONE',  ( 0.000000000000000000, 5.997115278587678233, -3.485633455389450130 ) ) ;
#52203 = VERTEX_POINT ( 'NONE', #40628 ) ;
#52204 = CYLINDRICAL_SURFACE ( 'NONE', #5063, 4.999999999999999112 ) ;
#52205 = ADVANCED_FACE ( 'NONE', ( #15665 ), #25666, .T. ) ;
#52206 = CARTESIAN_POINT ( 'NONE',  ( 2.931247277082547509, 4.765826751677452400, 6.255823895766906340 ) ) ;
#52207 = AXIS2_PLACEMENT_3D ( 'NONE', #37691, #2460, #57320 ) ;
#52208 = FACE_OUTER_BOUND ( 'NONE', #33746, .T. ) ;
#52209 = EDGE_CURVE ( 'NONE', #49715, #2584, #53008, .T. ) ;
#52210 = CYLINDRICAL_SURFACE ( 'NONE', #20128, 4.999999999999999112 ) ;
#52211 = CARTESIAN_POINT ( 'NONE',  ( 0.2646305136544065406, 11.55263159009958684, 4.064188116014585184 ) ) ;
#52212 = AXIS2_PLACEMENT_3D ( 'NONE', #55785, #34507, #54808 ) ;
#52213 = DIRECTION ( 'NONE',  ( 0.000000000000000000, -1.000000000000000000, 0.000000000000000000 ) ) ;
#52214 = EDGE_CURVE ( 'NONE', #44685, #65319, #33089, .T. ) ;
#52215 = ORIENTED_EDGE ( 'NONE', *, *, #62566, .T. ) ;
#52216 = DIRECTION ( 'NONE',  ( 0.000000000000000000, 0.7617968321374855023, 0.6478160128811973895 ) ) ;
#52217 = ADVANCED_FACE ( 'NONE', ( #44967 ), #56244, .T. ) ;
#52218 = AXIS2_PLACEMENT_3D ( 'NONE', #36119, #61733, #55782 ) ;
#52219 = ORIENTED_EDGE ( 'NONE', *, *, #43547, .F. ) ;
#52220 = CARTESIAN_POINT ( 'NONE',  ( 0.3109076770649061849, 10.73466383006821445, 5.925244271826481501 ) ) ;
#52221 = CARTESIAN_POINT ( 'NONE',  ( -7.856485614137358908, -26.39148214816155047, -14.61473980079826340 ) ) ;
#52222 = CARTESIAN_POINT ( 'NONE',  ( 1.719304012338836563, 0.7661785589583339773, 12.70777170743865980 ) ) ;
#52223 = EDGE_CURVE ( 'NONE', #27379, #23284, #730, .T. ) ;
#52224 = CIRCLE ( 'NONE', #42486, 4.999999999999999112 ) ;
#52226 = AXIS2_PLACEMENT_3D ( 'NONE', #61451, #10931, #15897 ) ;
#52225 = CARTESIAN_POINT ( 'NONE',  ( 35.00000000000000000, -5.644643009979139592, -10.30098186818248074 ) ) ;
#52227 = CARTESIAN_POINT ( 'NONE',  ( 2.249013661412227805, -6.673008335691891446, 3.714035584818202285 ) ) ;
#52228 = VERTEX_POINT ( 'NONE', #14677 ) ;
#52229 = CARTESIAN_POINT ( 'NONE',  ( -35.00000000000000000, 1.903127969211188653, 11.59095880812009227 ) ) ;
#52230 = CARTESIAN_POINT ( 'NONE',  ( 0.3106921474978442399, 2.360654586927948717, -12.03191800497306296 ) ) ;
#52231 = CARTESIAN_POINT ( 'NONE',  ( 21.44135743879865430, 11.69231880031143866, -2.731539164460570657 ) ) ;
#52232 = DIRECTION ( 'NONE',  ( 1.000000000000000000, 0.000000000000000000, 0.000000000000000000 ) ) ;
#52233 = CIRCLE ( 'NONE', #30938, 5.000000000000000000 ) ;
#52234 = CIRCLE ( 'NONE', #23550, 12.74999999999999822 ) ;
#52235 = CARTESIAN_POINT ( 'NONE',  ( 1.937114397841932290, -11.53912442307259134, 5.620553190832935364 ) ) ;
#52236 = ORIENTED_EDGE ( 'NONE', *, *, #55344, .F. ) ;
#52237 = CARTESIAN_POINT ( 'NONE',  ( 2.653899356899525941, -0.2611590963044880254, -7.767552767344014342 ) ) ;
#52238 = LINE ( 'NONE', #57552, #43674 ) ;
#52239 = CIRCLE ( 'NONE', #9774, 5.000000000000001776 ) ;
#52240 = EDGE_CURVE ( 'NONE', #50233, #57324, #45960, .T. ) ;
#52241 = ORIENTED_EDGE ( 'NONE', *, *, #30449, .F. ) ;
#52242 = AXIS2_PLACEMENT_3D ( 'NONE', #17540, #33785, #7541 ) ;
#52243 = EDGE_CURVE ( 'NONE', #52558, #9981, #26782, .T. ) ;
#52244 =( BOUNDED_SURFACE ( )  B_SPLINE_SURFACE ( 3, 1, ( 
 ( #46265, #50919 ),
 ( #41577, #61866 ),
 ( #706, #11326 ),
 ( #41241, #31596 ) ),
 .UNSPECIFIED., .F., .F., .F. ) 
 B_SPLINE_SURFACE_WITH_KNOTS ( ( 4, 4 ),
 ( 2, 2 ),
 ( 0.000000000000000000, 1.000000000000000000 ),
 ( 0.000000000000000000, 1.000000000000000000 ),
 .UNSPECIFIED. ) 
 GEOMETRIC_REPRESENTATION_ITEM ( )  RATIONAL_B_SPLINE_SURFACE ( (
 ( 1.000000000000000000, 1.000000000000000000),
 ( 0.6933888150995267674, 0.9895912004443193632),
 ( 0.6933888150995267674, 0.9895912004443193632),
 ( 1.000000000000000000, 1.000000000000000000) ) ) 
 REPRESENTATION_ITEM ( '' )  SURFACE ( )  );
#52245 = ORIENTED_EDGE ( 'NONE', *, *, #19511, .F. ) ;
#52246 = CARTESIAN_POINT ( 'NONE',  ( 0.2653519991613825790, 2.104847849998860543, 12.06397323649776787 ) ) ;
#52247 = CARTESIAN_POINT ( 'NONE',  ( 30.43939922888039007, -3.192189569316896236, -23.38849890424057421 ) ) ;
#52248 = DIRECTION ( 'NONE',  ( 0.000000000000000000, 0.01356324068817991828, -0.9999080150203990547 ) ) ;
#52249 = AXIS2_PLACEMENT_3D ( 'NONE', #64501, #53239, #23303 ) ;
#52250 = CARTESIAN_POINT ( 'NONE',  ( 0.2647959493198558945, -1.981611532097627970, 12.08462848595694084 ) ) ;
#52251 = ORIENTED_EDGE ( 'NONE', *, *, #64607, .T. ) ;
#52252 = CIRCLE ( 'NONE', #23582, 5.000000000000000888 ) ;
#52253 = EDGE_CURVE ( 'NONE', #44894, #64219, #58671, .T. ) ;
#52254 = ORIENTED_EDGE ( 'NONE', *, *, #22030, .T. ) ;
#52255 = ORIENTED_EDGE ( 'NONE', *, *, #58570, .F. ) ;
#52256 = CARTESIAN_POINT ( 'NONE',  ( -35.00000000000000000, 6.946017217729938409, 10.01317267707888981 ) ) ;
#52257 = CARTESIAN_POINT ( 'NONE',  ( 37.00000000000000711, -11.86701198550353986, 2.772148766916240348 ) ) ;
#52258 = EDGE_LOOP ( 'NONE', ( #45046, #45210, #22642, #54888 ) ) ;
#52259 = CARTESIAN_POINT ( 'NONE',  ( -17.60261755426340713, 3.558939319148466396, -11.46150330649539306 ) ) ;
#52260 = AXIS2_PLACEMENT_3D ( 'NONE', #47691, #12104, #41371 ) ;
#52261 = CARTESIAN_POINT ( 'NONE',  ( 145.1370849898475797, 3.309064568108273190E-14, 0.000000000000000000 ) ) ;
#52262 = ORIENTED_EDGE ( 'NONE', *, *, #31647, .F. ) ;
#52263 = CARTESIAN_POINT ( 'NONE',  ( 0.2648978790185593790, 11.55204314799269305, -4.063980959784929681 ) ) ;
#52264 =( BOUNDED_SURFACE ( )  B_SPLINE_SURFACE ( 3, 1, ( 
 ( #23991, #23004 ),
 ( #47944, #52924 ),
 ( #2402, #2748 ),
 ( #63536, #13018 ) ),
 .UNSPECIFIED., .F., .F., .F. ) 
 B_SPLINE_SURFACE_WITH_KNOTS ( ( 4, 4 ),
 ( 2, 2 ),
 ( 0.000000000000000000, 1.000000000000000000 ),
 ( 0.000000000000000000, 1.000000000000000000 ),
 .UNSPECIFIED. ) 
 GEOMETRIC_REPRESENTATION_ITEM ( )  RATIONAL_B_SPLINE_SURFACE ( (
 ( 1.000000000000000000, 1.000000000000000000),
 ( 0.9932032654565553509, 0.8386279382598740284),
 ( 0.9932032654565553509, 0.8386279382598740284),
 ( 1.000000000000000000, 1.000000000000000000) ) ) 
 REPRESENTATION_ITEM ( '' )  SURFACE ( )  );
#52265 = DIRECTION ( 'NONE',  ( -1.000000000000000000, 0.000000000000000000, 0.000000000000000000 ) ) ;
#52266 = CARTESIAN_POINT ( 'NONE',  ( 2.262775599887391298, 7.131180968652119923, 2.745802076337088060 ) ) ;
#52267 = EDGE_LOOP ( 'NONE', ( #57165, #28892, #62485, #35739 ) ) ;
#52268 = DIRECTION ( 'NONE',  ( 1.000000000000000000, 0.000000000000000000, 0.000000000000000000 ) ) ;
#52269 = EDGE_CURVE ( 'NONE', #48664, #37930, #20021, .T. ) ;
#52270 = ORIENTED_EDGE ( 'NONE', *, *, #27939, .T. ) ;
#52271 = CARTESIAN_POINT ( 'NONE',  ( 35.00000000000000000, -12.16893194857552452, -3.805206332242430101 ) ) ;
#52272 = VECTOR ( 'NONE', #18875, 1000.000000000000000 ) ;
#52273 = CARTESIAN_POINT ( 'NONE',  ( -17.67260731600310208, -7.949547442848166945, 10.91509878626014540 ) ) ;
#52274 = EDGE_CURVE ( 'NONE', #29168, #13166, #5738, .T. ) ;
#52275 = CARTESIAN_POINT ( 'NONE',  ( 0.8745425597524942862, -31.03649492335442872, -14.44372008463391310 ) ) ;
#52276 = CYLINDRICAL_SURFACE ( 'NONE', #31539, 4.999999999999999112 ) ;
#52277 = CIRCLE ( 'NONE', #4470, 12.18650000000000055 ) ;
#52278 = AXIS2_PLACEMENT_3D ( 'NONE', #65402, #40465, #30805 ) ;
#52280 = AXIS2_PLACEMENT_3D ( 'NONE', #20207, #15218, #54821 ) ;
#52279 = CYLINDRICAL_SURFACE ( 'NONE', #30370, 4.999999999999999112 ) ;
#52281 = DIRECTION ( 'NONE',  ( 1.000000000000000000, 0.000000000000000000, 0.000000000000000000 ) ) ;
#52282 = CARTESIAN_POINT ( 'NONE',  ( 5.515188684475870851, -0.001283816547385159676, -0.005194992164431768387 ) ) ;
#52283 = CARTESIAN_POINT ( 'NONE',  ( 9.188001832116450274, 6.971707373100242577, -9.768769640225654527 ) ) ;
#52284 = ORIENTED_EDGE ( 'NONE', *, *, #45390, .T. ) ;
#52285 = CARTESIAN_POINT ( 'NONE',  ( -35.00000000000000000, -2.772148766916031182, -11.86701198550359315 ) ) ;
#52286 = ORIENTED_EDGE ( 'NONE', *, *, #152, .T. ) ;
#52287 = FACE_OUTER_BOUND ( 'NONE', #36471, .T. ) ;
#52288 = CARTESIAN_POINT ( 'NONE',  ( 2.305787727787083519, -5.756228004061423320, -5.047606869483115766 ) ) ;
#52289 = ORIENTED_EDGE ( 'NONE', *, *, #35349, .F. ) ;
#52290 = DIRECTION ( 'NONE',  ( 0.000000000000000000, 0.3218879778915972878, -0.9467777615094571386 ) ) ;
#52291 = CARTESIAN_POINT ( 'NONE',  ( 2.305787727787085295, 7.566723232958088019, -1.164987321564654676 ) ) ;
#52292 = CARTESIAN_POINT ( 'NONE',  ( 1.000000000000000888, 7.248432822490259220, 1.926193556693033271 ) ) ;
#52293 = EDGE_CURVE ( 'NONE', #19282, #62401, #20383, .T. ) ;
#52294 = ORIENTED_EDGE ( 'NONE', *, *, #60960, .T. ) ;
#52295 = AXIS2_PLACEMENT_3D ( 'NONE', #34129, #64390, #25149 ) ;
#52296 = ORIENTED_EDGE ( 'NONE', *, *, #23188, .T. ) ;
#52297 = LINE ( 'NONE', #6737, #3548 ) ;
#52298 = EDGE_CURVE ( 'NONE', #10001, #10138, #55457, .T. ) ;
#52299 = ORIENTED_EDGE ( 'NONE', *, *, #26904, .T. ) ;
#52300 = CARTESIAN_POINT ( 'NONE',  ( -22.31328051695926007, 3.401210163132566411, 1.671726071983929307 ) ) ;
#52301 = CIRCLE ( 'NONE', #23620, 12.73084802173761787 ) ;
#52302 = DIRECTION ( 'NONE',  ( -1.000000000000000000, 0.000000000000000000, 0.000000000000000000 ) ) ;
#52303 = ADVANCED_FACE ( 'NONE', ( #60253 ), #45609, .T. ) ;
#52304 = CARTESIAN_POINT ( 'NONE',  ( -35.00000000000000000, -5.921969905510425569, 10.14408668126211488 ) ) ;
#52305 = ORIENTED_EDGE ( 'NONE', *, *, #23954, .F. ) ;
#52306 = B_SPLINE_CURVE_WITH_KNOTS ( 'NONE', 3,
 ( #2820, #38355, #23747, #22761, #18437, #43670 ),
 .UNSPECIFIED., .F., .F.,
 ( 4, 2, 4 ),
 ( 0.000000000000000000, 0.0004528561986909402357, 0.0009057123973818806883 ),
 .UNSPECIFIED. ) ;
#52307 = CARTESIAN_POINT ( 'NONE',  ( 0.2869720083484340045, -12.02930764912520445, -2.332746648244325982 ) ) ;
#52308 = EDGE_CURVE ( 'NONE', #32446, #17391, #21473, .T. ) ;
#52309 = AXIS2_PLACEMENT_3D ( 'NONE', #38188, #63782, #37554 ) ;
#52310 = DIRECTION ( 'NONE',  ( 0.000000000000000000, 0.000000000000000000, 1.000000000000000000 ) ) ;
#52311 = FACE_OUTER_BOUND ( 'NONE', #3732, .T. ) ;
#52312 = DIRECTION ( 'NONE',  ( -1.000000000000000000, -0.000000000000000000, 0.000000000000000000 ) ) ;
#52313 = CARTESIAN_POINT ( 'NONE',  ( 0.2833330754217419090, -5.950193237802332114, -10.71034013638385929 ) ) ;
#52314 = CARTESIAN_POINT ( 'NONE',  ( 35.00000000000000000, -7.251710744571640888, -9.240395740215610942 ) ) ;
#52315 = PLANE ( 'NONE',  #63300 ) ;
#52316 = LINE ( 'NONE', #41654, #56637 ) ;
#52317 = VECTOR ( 'NONE', #5381, 1000.000000000000000 ) ;
#52318 = AXIS2_PLACEMENT_3D ( 'NONE', #2997, #38553, #8951 ) ;
#52319 = VECTOR ( 'NONE', #33725, 999.9999999999998863 ) ;
#52320 = ORIENTED_EDGE ( 'NONE', *, *, #37244, .T. ) ;
#52321 = CARTESIAN_POINT ( 'NONE',  ( -18.08686583997218733, 5.370770984569721129, 12.38794726521413736 ) ) ;
#52322 = CARTESIAN_POINT ( 'NONE',  ( 0.3053067050349178579, -12.25734436043224740, -0.2307671807673560560 ) ) ;
#52323 = ADVANCED_FACE ( 'NONE', ( #10358 ), #61239, .T. ) ;
#52324 = VERTEX_POINT ( 'NONE', #11034 ) ;
#52325 = LINE ( 'NONE', #6764, #9849 ) ;
#52326 = CARTESIAN_POINT ( 'NONE',  ( 0.000000000000000000, 0.000000000000000000, 0.000000000000000000 ) ) ;
#52327 = ORIENTED_EDGE ( 'NONE', *, *, #26203, .F. ) ;
#52328 = CARTESIAN_POINT ( 'NONE',  ( 2.249013661412875731, 6.552953334857355649, 3.921976945966711092 ) ) ;
#52329 = ORIENTED_EDGE ( 'NONE', *, *, #23088, .T. ) ;
#52330 = CARTESIAN_POINT ( 'NONE',  ( -35.00000000000000000, 5.391785509270962784, 10.43555801961477236 ) ) ;
#52331 = ORIENTED_EDGE ( 'NONE', *, *, #47004, .T. ) ;
#52332 = ORIENTED_EDGE ( 'NONE', *, *, #46864, .F. ) ;
#52333 = AXIS2_PLACEMENT_3D ( 'NONE', #61221, #9343, #55906 ) ;
#52334 = CARTESIAN_POINT ( 'NONE',  ( 2.276905613633649850, -7.130967020394715306, 2.759436818562468030 ) ) ;
#52335 = ORIENTED_EDGE ( 'NONE', *, *, #60475, .T. ) ;
#52336 = CYLINDRICAL_SURFACE ( 'NONE', #52509, 5.000000000000000888 ) ;
#52337 = DIRECTION ( 'NONE',  ( 1.000000000000000000, 0.000000000000000000, 0.000000000000000000 ) ) ;
#52338 = CARTESIAN_POINT ( 'NONE',  ( 22.88594695219327235, -4.822122601967141264, -12.60940655271284427 ) ) ;
#52339 = DIRECTION ( 'NONE',  ( 1.000000000000000000, 0.000000000000000000, 0.000000000000000000 ) ) ;
#52340 = ORIENTED_EDGE ( 'NONE', *, *, #28314, .F. ) ;
#52341 = VECTOR ( 'NONE', #58216, 1000.000000000000000 ) ;
#52342 = CARTESIAN_POINT ( 'NONE',  ( 29.03457606387295087, 7.862146963512124387, 10.97436308512422265 ) ) ;
#52343 = CIRCLE ( 'NONE', #3474, 7.938172270156617749 ) ;
#52344 = CARTESIAN_POINT ( 'NONE',  ( -5.492202615392249854, -31.64503107144835070, 13.74436444834396021 ) ) ;
#52345 = CARTESIAN_POINT ( 'NONE',  ( -22.46509356695198889, -4.154553862421328070, -0.8809186187926377753 ) ) ;
#52347 = VERTEX_POINT ( 'NONE', #52900 ) ;
#52346 = CARTESIAN_POINT ( 'NONE',  ( -24.39341069969850295, 9.142292985779414849, 7.776119890389081135 ) ) ;
#52348 = LINE ( 'NONE', #33010, #58615 ) ;
#52349 = EDGE_CURVE ( 'NONE', #12370, #45713, #42666, .T. ) ;
#52350 = ORIENTED_EDGE ( 'NONE', *, *, #54866, .F. ) ;
#52351 = CARTESIAN_POINT ( 'NONE',  ( 0.2653141617321045920, 9.409385893408607870, -7.837919552760626019 ) ) ;
#52352 = ORIENTED_EDGE ( 'NONE', *, *, #462, .F. ) ;
#52353 = CARTESIAN_POINT ( 'NONE',  ( 21.65883687731333751, -11.04763598250161749, -4.689338699165349844 ) ) ;
#52354 = DIRECTION ( 'NONE',  ( 0.000000000000000000, -0.04924826701373159060, -0.9987865678893284027 ) ) ;
#52355 = EDGE_CURVE ( 'NONE', #61028, #10755, #2381, .T. ) ;
#52356 = CARTESIAN_POINT ( 'NONE',  ( 2.000000000000001776, -6.338823199656690832, 2.816798305433647620 ) ) ;
#52357 = EDGE_LOOP ( 'NONE', ( #42623, #28582, #4519, #9160 ) ) ;
#52358 = DIRECTION ( 'NONE',  ( 0.000000000000000000, -0.01356324068817998940, 0.9999080150203990547 ) ) ;
#52359 = CARTESIAN_POINT ( 'NONE',  ( -37.00000000000000711, 0.000000000000000000, 0.000000000000000000 ) ) ;
#52360 = CARTESIAN_POINT ( 'NONE',  ( -22.27719381268171261, -3.550654232855433357, -0.9730858478813990686 ) ) ;
#52361 = ORIENTED_EDGE ( 'NONE', *, *, #36230, .T. ) ;
#52362 = VERTEX_POINT ( 'NONE', #46937 ) ;
#52363 = CARTESIAN_POINT ( 'NONE',  ( -35.00000000000000000, 2.185196060783882288, 11.54110654723649709 ) ) ;
#52364 = EDGE_LOOP ( 'NONE', ( #46268, #5316, #22297, #4111 ) ) ;
#52365 = ORIENTED_EDGE ( 'NONE', *, *, #52021, .F. ) ;
#52367 = VECTOR ( 'NONE', #36865, 1000.000000000000000 ) ;
#52366 = DIRECTION ( 'NONE',  ( 0.000000000000000000, 0.3218879778915905154, -0.9467777615094595811 ) ) ;
#52368 = CARTESIAN_POINT ( 'NONE',  ( 35.00000000000000000, 4.705694406421931860E-17, -3.469127814946512892E-15 ) ) ;
#52369 = CARTESIAN_POINT ( 'NONE',  ( 35.00000000000000000, -11.66953048682396954, 3.511814412392239682 ) ) ;
#52370 = DIRECTION ( 'NONE',  ( -0.9606638835031803270, -0.2689826995745344118, 0.06908842350339121363 ) ) ;
#52371 = CYLINDRICAL_SURFACE ( 'NONE', #44388, 12.18649999999999878 ) ;
#52372 = EDGE_CURVE ( 'NONE', #4532, #33015, #2363, .T. ) ;
#52373 = AXIS2_PLACEMENT_3D ( 'NONE', #27837, #58780, #43114 ) ;
#52374 = DIRECTION ( 'NONE',  ( 1.000000000000000000, 0.000000000000000000, 0.000000000000000000 ) ) ;
#52375 = VECTOR ( 'NONE', #44282, 1000.000000000000114 ) ;
#52376 = DIRECTION ( 'NONE',  ( 1.000000000000000000, -0.000000000000000000, 0.000000000000000000 ) ) ;
#52377 = EDGE_LOOP ( 'NONE', ( #19996, #33667, #16559, #1744 ) ) ;
#52378 = VECTOR ( 'NONE', #13347, 1000.000000000000000 ) ;
#52379 = CARTESIAN_POINT ( 'NONE',  ( -22.29677679919927513, -3.097220482904027072, 2.096973157017371747 ) ) ;
#52380 = CARTESIAN_POINT ( 'NONE',  ( 35.00000000000000000, 11.73808581813437080, -0.4353888892050498116 ) ) ;
#52381 = EDGE_CURVE ( 'NONE', #63113, #64447, #22299, .T. ) ;
#52382 = CIRCLE ( 'NONE', #21571, 12.74999999999999822 ) ;
#52383 = CYLINDRICAL_SURFACE ( 'NONE', #56595, 12.75000000000000178 ) ;
#52384 = CARTESIAN_POINT ( 'NONE',  ( 0.2652384770603659070, 12.07140968216696741, -2.061429379240358628 ) ) ;
#52385 = VECTOR ( 'NONE', #3206, 1000.000000000000000 ) ;
#52386 = CARTESIAN_POINT ( 'NONE',  ( 8.810907765906716094, 2.660651897896487483, -11.70423931794396211 ) ) ;
#52387 = VERTEX_POINT ( 'NONE', #41609 ) ;
#52388 = CARTESIAN_POINT ( 'NONE',  ( -41.00000000000000711, -25.45369917733757603, 1.516638822270954590 ) ) ;
#52389 = CARTESIAN_POINT ( 'NONE',  ( -37.00000000000000711, 0.9416912585474421782, 12.71517666308948513 ) ) ;
#52390 = CARTESIAN_POINT ( 'NONE',  ( 0.3665391374699472626, -12.27992639892678461, 0.2638605131386739244 ) ) ;
#52391 = CARTESIAN_POINT ( 'NONE',  ( -17.54726996257253191, -12.93490414535027710, 3.865003848717349033 ) ) ;
#52392 = CARTESIAN_POINT ( 'NONE',  ( -24.84400141115547456, 8.878028940934107993, 8.075574810441137785 ) ) ;
#52393 = CARTESIAN_POINT ( 'NONE',  ( -24.79772874291392526, -10.35329051066264761, 8.670239208206227843 ) ) ;
#52394 = EDGE_CURVE ( 'NONE', #28876, #8359, #51520, .T. ) ;
#52395 = ORIENTED_EDGE ( 'NONE', *, *, #45056, .T. ) ;
#52396 = DIRECTION ( 'NONE',  ( 0.000000000000000000, -0.9999080150203989437, -0.01356324068819032662 ) ) ;
#52397 = CARTESIAN_POINT ( 'NONE',  ( -2.532614230583023041, 12.88560382747354005, 4.026315189028235153 ) ) ;
#52398 = CARTESIAN_POINT ( 'NONE',  ( -8.891032880924177206, 25.00000000000000000, -3.860857758255646921 ) ) ;
#52399 = FACE_OUTER_BOUND ( 'NONE', #44215, .T. ) ;
#52400 = ORIENTED_EDGE ( 'NONE', *, *, #10474, .T. ) ;
#52401 = ADVANCED_FACE ( 'NONE', ( #11351 ), #41933, .T. ) ;
#52402 = CARTESIAN_POINT ( 'NONE',  ( 2.305787727787084407, 6.711944854845823372, 3.682701754025536012 ) ) ;
#52403 = CARTESIAN_POINT ( 'NONE',  ( -35.00000000000000000, -12.05416472667164207, -1.791059740004549372 ) ) ;
#52404 = CIRCLE ( 'NONE', #59853, 2.899999999999994582 ) ;
#52405 = AXIS2_PLACEMENT_3D ( 'NONE', #44002, #69, #25673 ) ;
#52407 = VERTEX_POINT ( 'NONE', #62871 ) ;
#52406 = CARTESIAN_POINT ( 'NONE',  ( 41.00000000000000711, -45.00200000000000244, -4.500000000000000888 ) ) ;
#52408 = CYLINDRICAL_SURFACE ( 'NONE', #18290, 2.899999999999994582 ) ;
#52409 = AXIS2_PLACEMENT_3D ( 'NONE', #63636, #65598, #9756 ) ;
#52410 = CONICAL_SURFACE ( 'NONE', #62980, 7.938172270156617749, 1.280189991382167047 ) ;
#52411 = EDGE_CURVE ( 'NONE', #4408, #47167, #7665, .T. ) ;
#52412 = DIRECTION ( 'NONE',  ( 1.000000000000000000, 0.000000000000000000, 0.000000000000000000 ) ) ;
#52413 = ORIENTED_EDGE ( 'NONE', *, *, #54572, .F. ) ;
#52414 = CARTESIAN_POINT ( 'NONE',  ( 0.3537226245948351666, -9.569332148897514045, 7.688925565304987053 ) ) ;
#52415 = CARTESIAN_POINT ( 'NONE',  ( 0.2638984909335720941, -5.950360275955130618, 10.70468911391662381 ) ) ;
#52416 = DIRECTION ( 'NONE',  ( 1.000000000000000000, 0.000000000000000000, 0.000000000000000000 ) ) ;
#52417 = CARTESIAN_POINT ( 'NONE',  ( -3.460650213238962269, -8.804360588126725062, 10.24121041136440802 ) ) ;
#52418 = CARTESIAN_POINT ( 'NONE',  ( 0.2911222467163546712, -11.44063169461053064, -4.392242282524980723 ) ) ;
#52419 = CIRCLE ( 'NONE', #51390, 5.000000000000000888 ) ;
#52420 = CARTESIAN_POINT ( 'NONE',  ( 0.3675815128205894289, 11.62724744438065727, 3.951233083390508050 ) ) ;
#52422 = ORIENTED_EDGE ( 'NONE', *, *, #34090, .F. ) ;
#52421 = CARTESIAN_POINT ( 'NONE',  ( 1.719304012338836563, 0.7661785589583339773, 12.70777170743865980 ) ) ;
#52423 = CARTESIAN_POINT ( 'NONE',  ( -22.27722022243424149, 2.391991868237167917, 2.798846704197218482 ) ) ;
#52424 = EDGE_CURVE ( 'NONE', #34070, #34540, #42923, .T. ) ;
#52425 = EDGE_CURVE ( 'NONE', #54245, #26733, #31012, .T. ) ;
#52426 = ORIENTED_EDGE ( 'NONE', *, *, #16212, .T. ) ;
#52427 = DIRECTION ( 'NONE',  ( 0.000000000000000000, 0.01356324068817998940, -0.9999080150203990547 ) ) ;
#52428 = CIRCLE ( 'NONE', #50288, 12.18650000000000055 ) ;
#52429 = ORIENTED_EDGE ( 'NONE', *, *, #17635, .F. ) ;
#52430 = B_SPLINE_CURVE_WITH_KNOTS ( 'NONE', 3,
 ( #34087, #54409, #8841, #29130, #9154, #4177, #33764, #28787, #23478, #49431, #43090, #38097, #23148, #24443, #4522, #10461, #46068, #35724, #60041 ),
 .UNSPECIFIED., .F., .F.,
 ( 4, 3, 3, 3, 3, 3, 4 ),
 ( 7.198522745683553356E-18, 4.457896483014757189E-05, 6.639290541542080333E-05, 8.820687556478888647E-05, 0.0001100173248778924787, 0.0001545671401658117229, 0.0001830328308068602031 ),
 .UNSPECIFIED. ) ;
#52431 = CARTESIAN_POINT ( 'NONE',  ( 1.372161826076367719, -11.63973780005248670, 4.864129100816739104 ) ) ;
#52432 = CIRCLE ( 'NONE', #45010, 12.18649999999999878 ) ;
#52433 = CARTESIAN_POINT ( 'NONE',  ( -2.952869152607106251, 11.39722960915212724, 3.755417052241485365 ) ) ;
#52434 = DIRECTION ( 'NONE',  ( 0.000000000000000000, 0.7617968321374899432, 0.6478160128811920604 ) ) ;
#52435 = ORIENTED_EDGE ( 'NONE', *, *, #13862, .T. ) ;
#52436 = AXIS2_PLACEMENT_3D ( 'NONE', #48342, #33352, #7759 ) ;
#52437 = FACE_OUTER_BOUND ( 'NONE', #64923, .T. ) ;
#52438 = CARTESIAN_POINT ( 'NONE',  ( -35.00000000000000000, 8.534258022646220354, -8.699265615722891809 ) ) ;
#52439 = ORIENTED_EDGE ( 'NONE', *, *, #53787, .T. ) ;
#52440 = AXIS2_PLACEMENT_3D ( 'NONE', #24207, #44472, #7618 ) ;
#52441 = ORIENTED_EDGE ( 'NONE', *, *, #11242, .F. ) ;
#52442 = CARTESIAN_POINT ( 'NONE',  ( 29.20601902130347227, -10.31618498597828371, 8.717929643690714769 ) ) ;
#52443 = ORIENTED_EDGE ( 'NONE', *, *, #63516, .F. ) ;
#52444 = DIRECTION ( 'NONE',  ( 1.000000000000000000, 0.000000000000000000, 0.000000000000000000 ) ) ;
#52445 = LINE ( 'NONE', #16531, #33026 ) ;
#52446 = CARTESIAN_POINT ( 'NONE',  ( 9.042193032038563061, 3.535237157306648115, 13.03118443932375925 ) ) ;
#52447 = CARTESIAN_POINT ( 'NONE',  ( 1.372161826075798174, 12.51237317864360854, 1.607409531431936323 ) ) ;
#52448 = DIRECTION ( 'NONE',  ( 1.000000000000000000, -0.000000000000000000, -0.000000000000000000 ) ) ;
#52449 = CARTESIAN_POINT ( 'NONE',  ( 2.941278708680199916, 3.842273877444562835, 4.788765081995642880 ) ) ;
#52450 = VECTOR ( 'NONE', #36869, 1000.000000000000000 ) ;
#52451 = DIRECTION ( 'NONE',  ( -1.000000000000000000, 0.000000000000000000, 0.000000000000000000 ) ) ;
#52452 = VERTEX_POINT ( 'NONE', #6709 ) ;
#52453 =( BOUNDED_SURFACE ( )  B_SPLINE_SURFACE ( 3, 1, ( 
 ( #32669, #17417 ),
 ( #47669, #37695 ),
 ( #52980, #31393 ),
 ( #51694, #6136 ) ),
 .UNSPECIFIED., .F., .F., .F. ) 
 B_SPLINE_SURFACE_WITH_KNOTS ( ( 4, 4 ),
 ( 2, 2 ),
 ( 0.000000000000000000, 1.000000000000000000 ),
 ( 0.000000000000000000, 1.000000000000000000 ),
 .UNSPECIFIED. ) 
 GEOMETRIC_REPRESENTATION_ITEM ( )  RATIONAL_B_SPLINE_SURFACE ( (
 ( 1.000000000000000000, 1.000000000000000000),
 ( 0.9856612449720755231, 0.9999558406602322425),
 ( 0.9856612449720755231, 0.9999558406602322425),
 ( 1.000000000000000000, 1.000000000000000000) ) ) 
 REPRESENTATION_ITEM ( '' )  SURFACE ( )  );
#52454 = CARTESIAN_POINT ( 'NONE',  ( 0.9232167919969138659, 12.45862789703290296, -0.4134278310083473462 ) ) ;
#52455 = VERTEX_POINT ( 'NONE', #26986 ) ;
#52456 = CARTESIAN_POINT ( 'NONE',  ( 3.152665057733776699, 4.377619405892044568, -6.622010822086680015 ) ) ;
#52457 = CARTESIAN_POINT ( 'NONE',  ( -22.28506771379528573, -2.571716811880550679, 2.697635452840744463 ) ) ;
#52459 = CARTESIAN_POINT ( 'NONE',  ( -9.036293593347389574, 11.24548700741398477, -4.203574557735506367 ) ) ;
#52458 = AXIS2_PLACEMENT_3D ( 'NONE', #43807, #64086, #29475 ) ;
#52460 = DIRECTION ( 'NONE',  ( -1.000000000000000000, 0.000000000000000000, 0.000000000000000000 ) ) ;
#52461 = AXIS2_PLACEMENT_3D ( 'NONE', #20578, #24573, #34845 ) ;
#52462 = CARTESIAN_POINT ( 'NONE',  ( -35.00000000000000000, 0.000000000000000000, 0.000000000000000000 ) ) ;
#52463 = EDGE_LOOP ( 'NONE', ( #62954, #59833, #29684, #32638 ) ) ;
#52464 = VECTOR ( 'NONE', #31751, 1000.000000000000000 ) ;
#52465 = EDGE_CURVE ( 'NONE', #31213, #27713, #47280, .T. ) ;
#52466 = VERTEX_POINT ( 'NONE', #42239 ) ;
#52467 = CIRCLE ( 'NONE', #42899, 7.580821595991582562 ) ;
#52468 = ORIENTED_EDGE ( 'NONE', *, *, #16873, .T. ) ;
#52469 = DIRECTION ( 'NONE',  ( 1.000000000000000000, 0.000000000000000000, 0.000000000000000000 ) ) ;
#52470 = DIRECTION ( 'NONE',  ( 0.000000000000000000, 0.3554799084908968343, 0.9346839223284540976 ) ) ;
#52471 = AXIS2_PLACEMENT_3D ( 'NONE', #34447, #4194, #64682 ) ;
#52472 = DIRECTION ( 'NONE',  ( 0.000000000000000000, 0.9551603052523468529, -0.2960891610144545938 ) ) ;
#52473 = CARTESIAN_POINT ( 'NONE',  ( -22.70624764888619751, 2.547047087672855259, 4.591418580540040928 ) ) ;
#52474 = EDGE_LOOP ( 'NONE', ( #24616, #41422, #37001, #33530 ) ) ;
#52475 = CARTESIAN_POINT ( 'NONE',  ( 0.3223008802179259114, 12.11889957318022581, 1.888629463821725141 ) ) ;
#52476 = DIRECTION ( 'NONE',  ( -1.000000000000000000, -0.000000000000000000, 0.000000000000000000 ) ) ;
#52477 = CARTESIAN_POINT ( 'NONE',  ( 2.305787727787084407, -1.164987321564783684, 7.566723232958066703 ) ) ;
#52478 = CARTESIAN_POINT ( 'NONE',  ( -42.06985574703969633, -1.486553742990790239, 18.28338660486113554 ) ) ;
#52479 = AXIS2_PLACEMENT_3D ( 'NONE', #11912, #52514, #6946 ) ;
#52480 = EDGE_CURVE ( 'NONE', #54776, #39567, #62531, .T. ) ;
#52481 = LINE ( 'NONE', #21204, #46904 ) ;
#52482 = CARTESIAN_POINT ( 'NONE',  ( 3.780834652287974773, 8.352030633203080257, 10.60629927458383115 ) ) ;
#52483 = ORIENTED_EDGE ( 'NONE', *, *, #13190, .F. ) ;
#52484 = ADVANCED_FACE ( 'NONE', ( #27294 ), #57561, .T. ) ;
#52485 = AXIS2_PLACEMENT_3D ( 'NONE', #3876, #25123, #19485 ) ;
#52486 = CARTESIAN_POINT ( 'NONE',  ( -17.34314652423584491, -28.58740822003687754, -8.955725788651514918 ) ) ;
#52487 = ORIENTED_EDGE ( 'NONE', *, *, #5118, .T. ) ;
#52488 = EDGE_CURVE ( 'NONE', #12917, #35544, #7804, .T. ) ;
#52489 = CARTESIAN_POINT ( 'NONE',  ( 10.75853767213705225, 7.830989516993144051, -10.99661780661415733 ) ) ;
#52490 = DIRECTION ( 'NONE',  ( -1.000000000000000000, 0.000000000000000000, 0.000000000000000000 ) ) ;
#52491 = CARTESIAN_POINT ( 'NONE',  ( 2.305787727787083519, -7.249469779319894336, -2.461236246751144829 ) ) ;
#52492 = DIRECTION ( 'NONE',  ( -1.000000000000000000, 0.000000000000000000, -0.000000000000000000 ) ) ;
#52493 = CARTESIAN_POINT ( 'NONE',  ( 2.080613030138688480, 0.000000000000000000, 0.000000000000000000 ) ) ;
#52494 = VECTOR ( 'NONE', #51954, 1000.000000000000000 ) ;
#52495 = VERTEX_POINT ( 'NONE', #54562 ) ;
#52497 = VERTEX_POINT ( 'NONE', #64195 ) ;
#52496 = EDGE_CURVE ( 'NONE', #32830, #35021, #27832, .T. ) ;
#52498 = DIRECTION ( 'NONE',  ( 0.000000000000000000, 0.000000000000000000, 1.000000000000000000 ) ) ;
#52499 = VERTEX_POINT ( 'NONE', #12644 ) ;
#52500 = CARTESIAN_POINT ( 'NONE',  ( -27.08418179957658367, -2.244544746853583295, 0.4604195552868128871 ) ) ;
#52501 = CARTESIAN_POINT ( 'NONE',  ( -22.27384469013076185, 3.548341908721034166, 0.9835229356381993693 ) ) ;
#52502 = CARTESIAN_POINT ( 'NONE',  ( -37.00000000000000711, 0.000000000000000000, 0.000000000000000000 ) ) ;
#52503 = CARTESIAN_POINT ( 'NONE',  ( 0.8320506296491597675, 3.891425424503466068, -11.81055997318801154 ) ) ;
#52504 = DIRECTION ( 'NONE',  ( 0.000000000000000000, -0.01356324068817991828, 0.9999080150203990547 ) ) ;
#52505 = EDGE_CURVE ( 'NONE', #35632, #33360, #61814, .T. ) ;
#52506 = CARTESIAN_POINT ( 'NONE',  ( 2.257661810676415914, -1.193649218120645283, 7.546014018371156595 ) ) ;
#52507 = CARTESIAN_POINT ( 'NONE',  ( -20.79170840334646542, 12.91784323155722980, -3.921648409140116698 ) ) ;
#52508 = ORIENTED_EDGE ( 'NONE', *, *, #2841, .F. ) ;
#52509 = AXIS2_PLACEMENT_3D ( 'NONE', #2449, #22051, #21405 ) ;
#52510 = ORIENTED_EDGE ( 'NONE', *, *, #43612, .F. ) ;
#52511 = CIRCLE ( 'NONE', #25969, 12.18649999999999878 ) ;
#52512 = DIRECTION ( 'NONE',  ( -1.000000000000000000, 0.000000000000000000, 0.000000000000000000 ) ) ;
#52513 = VERTEX_POINT ( 'NONE', #44231 ) ;
#52514 = DIRECTION ( 'NONE',  ( 1.000000000000000000, -0.000000000000000000, 0.000000000000000000 ) ) ;
#52515 = CARTESIAN_POINT ( 'NONE',  ( 5.530133899448235191, 0.01594518557925638305, -0.001124651387254824511 ) ) ;
#52516 = EDGE_CURVE ( 'NONE', #32335, #51910, #18310, .T. ) ;
#52517 = CARTESIAN_POINT ( 'NONE',  ( -27.10307689719148172, 1.703783570823889093, 1.615391801699764374 ) ) ;
#52518 = ORIENTED_EDGE ( 'NONE', *, *, #7054, .T. ) ;
#52519 = FACE_OUTER_BOUND ( 'NONE', #45610, .T. ) ;
#52520 = CARTESIAN_POINT ( 'NONE',  ( -35.00000000000000000, 11.05394794832836780, -5.130401251914613603 ) ) ;
#52521 = CARTESIAN_POINT ( 'NONE',  ( 36.00000000000000711, -6.265926637539571686, -11.10408318471057498 ) ) ;
#52522 = VERTEX_POINT ( 'NONE', #8665 ) ;
#52524 = EDGE_CURVE ( 'NONE', #32577, #37992, #50154, .T. ) ;
#52523 = ORIENTED_EDGE ( 'NONE', *, *, #18769, .F. ) ;
#52525 = CARTESIAN_POINT ( 'NONE',  ( 3.117994775788107020, 4.258268480479466156, 12.81686186562924057 ) ) ;
#52526 = VERTEX_POINT ( 'NONE', #58569 ) ;
#52527 = VERTEX_POINT ( 'NONE', #7684 ) ;
#52528 = AXIS2_PLACEMENT_3D ( 'NONE', #33041, #12423, #22767 ) ;
#52529 = VERTEX_POINT ( 'NONE', #12994 ) ;
#52530 = ORIENTED_EDGE ( 'NONE', *, *, #10200, .F. ) ;
#52531 = CARTESIAN_POINT ( 'NONE',  ( 0.2767916011545388799, 4.367596755337448400, 11.44495079483525757 ) ) ;
#52533 = VECTOR ( 'NONE', #61193, 1000.000000000000000 ) ;
#52532 = CIRCLE ( 'NONE', #21766, 5.000000000000000888 ) ;
#52534 = CARTESIAN_POINT ( 'NONE',  ( 2.258463476536308079, 5.014277205346122201, -5.764393264552794882 ) ) ;
#52535 = DIRECTION ( 'NONE',  ( 1.000000000000000000, 0.000000000000000000, 0.000000000000000000 ) ) ;
#52536 = CARTESIAN_POINT ( 'NONE',  ( 2.255723233588950105, 2.736592204236748760, -7.132203433012263893 ) ) ;
#52537 = DIRECTION ( 'NONE',  ( -0.3939253465568943180, -0.9068155327749422012, -0.1500280335741567828 ) ) ;
#52538 = CARTESIAN_POINT ( 'NONE',  ( -22.31328051695926007, -3.401210163132568187, -1.671726071983963946 ) ) ;
#52539 = EDGE_LOOP ( 'NONE', ( #63765, #35067, #15932, #7846 ) ) ;
#52540 = DIRECTION ( 'NONE',  ( 0.000000000000000000, 0.01356324068817998940, -0.9999080150203989437 ) ) ;
#52541 = AXIS2_PLACEMENT_3D ( 'NONE', #35047, #20442, #45373 ) ;
#52542 = CARTESIAN_POINT ( 'NONE',  ( -22.27718150314433387, 2.721613812022976031, -2.479231311682823957 ) ) ;
#52543 = CARTESIAN_POINT ( 'NONE',  ( 2.273267844205329791, 3.690689057641470150, -6.695181685740229760 ) ) ;
#52544 = CARTESIAN_POINT ( 'NONE',  ( 0.2657645697724682066, -2.275433120353170136, 12.03308811492268582 ) ) ;
#52545 = DIRECTION ( 'NONE',  ( 0.000000000000000000, -0.01356324068817998940, 0.9999080150203990547 ) ) ;
#52546 = CARTESIAN_POINT ( 'NONE',  ( -36.00000000000000711, 0.1414404973752139416, 12.74921544981111232 ) ) ;
#52547 = EDGE_CURVE ( 'NONE', #64733, #3364, #33919, .T. ) ;
#52548 = AXIS2_PLACEMENT_3D ( 'NONE', #36896, #1675, #52213 ) ;
#52549 = VERTEX_POINT ( 'NONE', #18667 ) ;
#52550 = CARTESIAN_POINT ( 'NONE',  ( -36.00000000000000711, -11.47561260193580956, 5.556331110570368992 ) ) ;
#52551 = EDGE_CURVE ( 'NONE', #40530, #58005, #13324, .T. ) ;
#52552 = ORIENTED_EDGE ( 'NONE', *, *, #65148, .F. ) ;
#52553 = LINE ( 'NONE', #1991, #40180 ) ;
#52554 = CARTESIAN_POINT ( 'NONE',  ( 0.2676618633000454328, -0.1607051348608467545, 12.24591287309139176 ) ) ;
#52555 = CARTESIAN_POINT ( 'NONE',  ( 2.941278708680199916, -2.226055275041753045, -5.721889327162172911 ) ) ;
#52556 = DIRECTION ( 'NONE',  ( -1.000000000000000000, -0.000000000000000000, 0.000000000000000000 ) ) ;
#52557 = LINE ( 'NONE', #27924, #16945 ) ;
#52558 = VERTEX_POINT ( 'NONE', #18331 ) ;
#52559 = AXIS2_PLACEMENT_3D ( 'NONE', #25656, #5060, #50937 ) ;
#52560 = ADVANCED_FACE ( 'NONE', ( #8991 ), #29274, .T. ) ;
#52561 = CARTESIAN_POINT ( 'NONE',  ( 0.3675815128205894289, 10.50067073900660652, -6.367184624550055183 ) ) ;
#52562 = CARTESIAN_POINT ( 'NONE',  ( 0.3218525148189809726, 2.370084734146373773, -12.03385614540601445 ) ) ;
#52563 = DIRECTION ( 'NONE',  ( 0.000000000000000000, -0.01356324068817998940, 0.9999080150203990547 ) ) ;
#52564 = CARTESIAN_POINT ( 'NONE',  ( 3.202861212844931416, -30.72210164159599088, -15.08749394223872642 ) ) ;
#52565 = EDGE_CURVE ( 'NONE', #20824, #38497, #2918, .T. ) ;
#52566 = DIRECTION ( 'NONE',  ( -1.000000000000000000, 0.000000000000000000, 0.000000000000000000 ) ) ;
#52567 = AXIS2_PLACEMENT_3D ( 'NONE', #25449, #9480, #4863 ) ;
#52568 = EDGE_LOOP ( 'NONE', ( #5021, #41607, #29272, #59734 ) ) ;
#52569 = EDGE_CURVE ( 'NONE', #4335, #18175, #14718, .T. ) ;
#52570 = CARTESIAN_POINT ( 'NONE',  ( 5.514970785353741078, -0.004532877335078719372, -0.001326349372336280402 ) ) ;
#52571 = EDGE_CURVE ( 'NONE', #27962, #18185, #12611, .T. ) ;
#52572 = CARTESIAN_POINT ( 'NONE',  ( -37.00000000000000711, -12.54989509947649573, -2.250029553613892563 ) ) ;
#52573 = AXIS2_PLACEMENT_3D ( 'NONE', #8345, #4019, #48928 ) ;
#52574 = EDGE_LOOP ( 'NONE', ( #37162, #14240, #26124, #58716 ) ) ;
#52575 = VERTEX_POINT ( 'NONE', #4997 ) ;
#52576 = CARTESIAN_POINT ( 'NONE',  ( 2.440552418640497212, -3.678171968408280978, -6.765628357760817835 ) ) ;
#52577 = FACE_OUTER_BOUND ( 'NONE', #15653, .T. ) ;
#52578 = CARTESIAN_POINT ( 'NONE',  ( 0.5547464869798254261, -7.697709668896136392, 9.648168635481816580 ) ) ;
#52579 = EDGE_CURVE ( 'NONE', #65758, #19449, #19300, .T. ) ;
#52580 = FACE_OUTER_BOUND ( 'NONE', #19748, .T. ) ;
#52581 = EDGE_LOOP ( 'NONE', ( #35785, #22829, #19768, #32011 ) ) ;
#52582 = ADVANCED_FACE ( 'NONE', ( #25931 ), #55527, .T. ) ;
#52583 = VERTEX_POINT ( 'NONE', #64821 ) ;
#52584 = ORIENTED_EDGE ( 'NONE', *, *, #49324, .T. ) ;
#52585 = DIRECTION ( 'NONE',  ( -1.000000000000000000, 0.000000000000000000, 0.000000000000000000 ) ) ;
#52586 = EDGE_CURVE ( 'NONE', #36878, #14755, #41640, .T. ) ;
#52587 = AXIS2_PLACEMENT_3D ( 'NONE', #14400, #10724, #39685 ) ;
#52588 = CARTESIAN_POINT ( 'NONE',  ( -35.00000000000000000, -11.35427606708809556, 4.426194442447198618 ) ) ;
#52589 = VERTEX_POINT ( 'NONE', #39896 ) ;
#52590 = EDGE_CURVE ( 'NONE', #21600, #51800, #9781, .T. ) ;
#52591 = DIRECTION ( 'NONE',  ( -1.000000000000000000, -0.000000000000000000, -0.000000000000000000 ) ) ;
#52592 = ADVANCED_FACE ( 'NONE', ( #25255 ), #9621, .T. ) ;
#52593 = CARTESIAN_POINT ( 'NONE',  ( 2.000000000000001776, 0.000000000000000000, 0.000000000000000000 ) ) ;
#52594 = ORIENTED_EDGE ( 'NONE', *, *, #17301, .F. ) ;
#52595 = CARTESIAN_POINT ( 'NONE',  ( 0.2653519991613838558, 11.51519138201636139, -4.167757449530301805 ) ) ;
#52596 = CARTESIAN_POINT ( 'NONE',  ( 8.295782569429569264, -27.33295754267981792, -14.98640435464887588 ) ) ;
#52597 = CARTESIAN_POINT ( 'NONE',  ( 2.241352910868908754, 7.145045428366577411, 2.689314586382375527 ) ) ;
#52598 = ORIENTED_EDGE ( 'NONE', *, *, #14772, .F. ) ;
#52599 = EDGE_CURVE ( 'NONE', #42626, #21283, #28879, .T. ) ;
#52600 = CARTESIAN_POINT ( 'NONE',  ( -35.00000000000000000, -1.262958560998674429, -12.12087942037211086 ) ) ;
#52601 = ORIENTED_EDGE ( 'NONE', *, *, #46390, .T. ) ;
#52602 = COLOUR_RGB ( '', 0.72549020, 0.75294118, 0.79215686) ;
#52603 = CARTESIAN_POINT ( 'NONE',  ( 1.283627346226908550, 7.660435136228973541, -9.985833283678474004 ) ) ;
#52604 = CARTESIAN_POINT ( 'NONE',  ( 10.56078269551218085, -11.97184738340593846, -0.8518863164657939357 ) ) ;
#52605 = CARTESIAN_POINT ( 'NONE',  ( -19.62362846926599147, -4.052573403833378052, 11.29610975316521504 ) ) ;
#52606 = DIRECTION ( 'NONE',  ( 1.000000000000000000, 0.000000000000000000, -0.000000000000000000 ) ) ;
#52607 = CARTESIAN_POINT ( 'NONE',  ( 0.2638984909335720941, 9.252728947331188891, -8.023974293733084906 ) ) ;
#52608 = FACE_OUTER_BOUND ( 'NONE', #57474, .T. ) ;
#52609 = CARTESIAN_POINT ( 'NONE',  ( 0.4626703367448980475, 6.399577980714960646, -10.51809671647423450 ) ) ;
#52610 = CARTESIAN_POINT ( 'NONE',  ( 6.646157311995629868, -5.064915162312895625, -10.88629149749473157 ) ) ;
#52611 = ORIENTED_EDGE ( 'NONE', *, *, #59871, .F. ) ;
#52612 = LINE ( 'NONE', #36641, #3509 ) ;
#52613 = ORIENTED_EDGE ( 'NONE', *, *, #2350, .T. ) ;
#52614 = CYLINDRICAL_SURFACE ( 'NONE', #65645, 12.18650000000000055 ) ;
#52615 = CARTESIAN_POINT ( 'NONE',  ( 2.305787727787084407, 6.711944854845823372, 3.682701754025536012 ) ) ;
#52616 = EDGE_LOOP ( 'NONE', ( #9646, #61163 ) ) ;
#52617 = DIRECTION ( 'NONE',  ( -0.3865475372811021937, -0.9046932595863059756, 0.1791957239473633001 ) ) ;
#52618 = CARTESIAN_POINT ( 'NONE',  ( 0.2671309869109507185, 12.03155065772887689, -2.286013846429900465 ) ) ;
#52619 = DIRECTION ( 'NONE',  ( 1.000000000000000000, 0.000000000000000000, 0.000000000000000000 ) ) ;
#52620 = AXIS2_PLACEMENT_3D ( 'NONE', #48746, #28773, #3199 ) ;
#52621 = ORIENTED_EDGE ( 'NONE', *, *, #19984, .T. ) ;
#52622 = EDGE_CURVE ( 'NONE', #35981, #12311, #40212, .T. ) ;
#52623 = ORIENTED_EDGE ( 'NONE', *, *, #36524, .T. ) ;
#52624 = CARTESIAN_POINT ( 'NONE',  ( 41.00000000000000711, -45.00200000000000244, 4.499999999999997335 ) ) ;
#52625 = ORIENTED_EDGE ( 'NONE', *, *, #51033, .F. ) ;
#52626 = CARTESIAN_POINT ( 'NONE',  ( 2.665405856346783953, 3.808819464940546684, -8.776564688671568248 ) ) ;
#52627 = CARTESIAN_POINT ( 'NONE',  ( 0.000000000000000000, -5.888698556700742159, -3.665823448873470003 ) ) ;
#52628 = DIRECTION ( 'NONE',  ( -1.000000000000000000, 0.000000000000000000, -0.000000000000000000 ) ) ;
#52629 = CARTESIAN_POINT ( 'NONE',  ( 1.452237505248555660, 0.5922625322517017787, 12.64182585313126239 ) ) ;
#52630 = CARTESIAN_POINT ( 'NONE',  ( 35.00000000000000000, 11.29812557209481483, 3.213188559034117819 ) ) ;
#52631 = ORIENTED_EDGE ( 'NONE', *, *, #14107, .T. ) ;
#52632 = EDGE_CURVE ( 'NONE', #662, #54975, #214, .T. ) ;
#52633 = DIRECTION ( 'NONE',  ( 0.000000000000000000, -0.01356324068817999114, 0.9999080150203989437 ) ) ;
#52634 = AXIS2_PLACEMENT_3D ( 'NONE', #31900, #16953, #57204 ) ;
#52635 = CARTESIAN_POINT ( 'NONE',  ( 2.835339799623983748, -7.649567297875982774, -1.682641786445519871 ) ) ;
#52636 = CARTESIAN_POINT ( 'NONE',  ( -35.00000000000000000, -11.65150730582933392, -1.488153103997089888 ) ) ;
#52637 = CARTESIAN_POINT ( 'NONE',  ( 2.889800649504073782, 6.039722463373538908, 0.9965440656173926159 ) ) ;
#52638 = CARTESIAN_POINT ( 'NONE',  ( 35.00000000000000000, -10.14433819232439049, -6.753013023069681431 ) ) ;
#52639 = ADVANCED_FACE ( 'NONE', ( #29580 ), #54871, .T. ) ;
#52640 = DIRECTION ( 'NONE',  ( 0.000000000000000000, -0.4698238015817237101, -0.8827602140260384367 ) ) ;
#52641 = STYLED_ITEM ( 'NONE', ( #43820 ), #19082 ) ;
#52642 = CARTESIAN_POINT ( 'NONE',  ( 47.00000000000000711, 4.705694406421931860E-17, -3.469127814946512892E-15 ) ) ;
#52643 = CARTESIAN_POINT ( 'NONE',  ( -22.71097035706202405, -0.4203397252017116448, 4.965150228107737540 ) ) ;
#52644 = B_SPLINE_CURVE_WITH_KNOTS ( 'NONE', 3,
 ( #46907, #62192, #41239, #42213, #7000, #47560, #62504, #26613, #37237, #36255, #11324, #1366, #62841, #11972, #11001, #31286 ),
 .UNSPECIFIED., .F., .F.,
 ( 4, 3, 3, 3, 3, 4 ),
 ( 0.000000000000000000, 0.0002999043160757375033, 0.0005998071753051059879, 0.0008997092107374648606, 0.001204458948196129734, 0.001510329163477479742 ),
 .UNSPECIFIED. ) ;
#52645 = VERTEX_POINT ( 'NONE', #9293 ) ;
#52646 = LINE ( 'NONE', #1772, #27814 ) ;
#52647 = CARTESIAN_POINT ( 'NONE',  ( -35.00000000000000000, 7.094637218249357780, 10.59380114696472397 ) ) ;
#52648 = VERTEX_POINT ( 'NONE', #5315 ) ;
#52649 = CARTESIAN_POINT ( 'NONE',  ( -22.27716857039623477, -3.591587580808000002, 0.8090275962000568200 ) ) ;
#52650 = CARTESIAN_POINT ( 'NONE',  ( -4.975205859172449507, -1.416020129149132778, -13.42553116244733680 ) ) ;
#52651 = VERTEX_POINT ( 'NONE', #65796 ) ;
#52652 = DIRECTION ( 'NONE',  ( -1.000000000000000000, -0.000000000000000000, -0.000000000000000000 ) ) ;
#52653 = ORIENTED_EDGE ( 'NONE', *, *, #14563, .F. ) ;
#52654 = CARTESIAN_POINT ( 'NONE',  ( -29.43980975494970309, -3.641506875706030488, 25.00000000000000000 ) ) ;
#52655 = ORIENTED_EDGE ( 'NONE', *, *, #64087, .T. ) ;
#52656 = ORIENTED_EDGE ( 'NONE', *, *, #46782, .F. ) ;
#52657 = EDGE_CURVE ( 'NONE', #26251, #35019, #43458, .T. ) ;
#52658 = DIRECTION ( 'NONE',  ( -1.000000000000000000, -1.836970198721029688E-16, 0.000000000000000000 ) ) ;
#52659 = VERTEX_POINT ( 'NONE', #15600 ) ;
#52660 = EDGE_CURVE ( 'NONE', #61666, #30718, #35865, .T. ) ;
#52661 = CARTESIAN_POINT ( 'NONE',  ( 35.00000000000000000, -10.49591321039684289, -5.273331777780305707 ) ) ;
#52662 = CARTESIAN_POINT ( 'NONE',  ( 3.152665057734040488, 0.000000000000000000, 0.000000000000000000 ) ) ;
#52663 = CARTESIAN_POINT ( 'NONE',  ( 22.68159425457230682, -4.559965384753717821, -12.70733236524612764 ) ) ;
#52664 = CARTESIAN_POINT ( 'NONE',  ( 1.547277799339609405, -0.6737945300328305187, -12.65564732076297361 ) ) ;
#52665 = ORIENTED_EDGE ( 'NONE', *, *, #53993, .F. ) ;
#52666 = CARTESIAN_POINT ( 'NONE',  ( -4.975205859172452172, -1.416020129149132778, -11.91616074890918675 ) ) ;
#52667 = CARTESIAN_POINT ( 'NONE',  ( 9.075728589825974524, -28.84360970496452126, 9.643933591119377979 ) ) ;
#52668 = CARTESIAN_POINT ( 'NONE',  ( 0.3665391374699467075, -6.368473106897203806, 10.50279796150434741 ) ) ;
#52670 = VERTEX_POINT ( 'NONE', #19639 ) ;
#52669 = CARTESIAN_POINT ( 'NONE',  ( 12.47628546223243617, 0.000000000000000000, -13.50000000000000178 ) ) ;
#52671 = EDGE_CURVE ( 'NONE', #59777, #34070, #57689, .T. ) ;
#52672 = DIRECTION ( 'NONE',  ( -1.000000000000000000, 0.000000000000000000, 0.000000000000000000 ) ) ;
#52673 = ORIENTED_EDGE ( 'NONE', *, *, #53336, .T. ) ;
#52674 = CARTESIAN_POINT ( 'NONE',  ( 0.2650492594609249464, 9.451471004987441304, -7.786980091309354535 ) ) ;
#52675 = VERTEX_POINT ( 'NONE', #47205 ) ;
#52676 = CARTESIAN_POINT ( 'NONE',  ( 24.82652845881425208, -8.390869743685021476, -8.578654028722157321 ) ) ;
#52677 = CARTESIAN_POINT ( 'NONE',  ( -27.10719052120871098, 0.6736837626858914740, 2.261993590776020469 ) ) ;
#52678 = FACE_OUTER_BOUND ( 'NONE', #22021, .T. ) ;
#52679 = EDGE_LOOP ( 'NONE', ( #24548, #38909, #5468, #9693 ) ) ;
#52680 = DIRECTION ( 'NONE',  ( 1.000000000000000000, -0.000000000000000000, 0.000000000000000000 ) ) ;
#52681 = CARTESIAN_POINT ( 'NONE',  ( -37.00000000000000711, 5.273331777780488672, -10.49591321039675229 ) ) ;
#52682 = DIRECTION ( 'NONE',  ( 0.000000000000000000, -0.01356324068817998940, 0.9999080150203990547 ) ) ;
#52683 = ORIENTED_EDGE ( 'NONE', *, *, #29888, .T. ) ;
#52684 = VERTEX_POINT ( 'NONE', #31868 ) ;
#52685 = DIRECTION ( 'NONE',  ( 1.000000000000000000, 0.000000000000000000, -0.000000000000000000 ) ) ;
#52686 = VERTEX_POINT ( 'NONE', #26905 ) ;
#52687 = ORIENTED_EDGE ( 'NONE', *, *, #1449, .F. ) ;
#52688 = CYLINDRICAL_SURFACE ( 'NONE', #52973, 12.74999999999999822 ) ;
#52689 = CARTESIAN_POINT ( 'NONE',  ( 37.00000000000000711, -3.827046518385000429, 11.56998259273181162 ) ) ;
#52690 = DIRECTION ( 'NONE',  ( 1.000000000000000000, 0.000000000000000000, -0.000000000000000000 ) ) ;
#52691 = CARTESIAN_POINT ( 'NONE',  ( -22.30861784526116054, 1.070462554923830245, 3.620936716852743764 ) ) ;
#52692 = CYLINDRICAL_SURFACE ( 'NONE', #43351, 12.74999999999999822 ) ;
#52693 = CARTESIAN_POINT ( 'NONE',  ( 2.000000000000001776, 1.779948802829816490, 6.576141558201244131 ) ) ;
#52694 = ADVANCED_FACE ( 'NONE', ( #62457 ), #41194, .T. ) ;
#52695 = VECTOR ( 'NONE', #9074, 1000.000000000000000 ) ;
#52696 = DIRECTION ( 'NONE',  ( 1.000000000000000000, -0.000000000000000000, 0.000000000000000000 ) ) ;
#52697 = ADVANCED_FACE ( 'NONE', ( #1961 ), #16879, .F. ) ;
#52698 = CIRCLE ( 'NONE', #37818, 12.18650000000000233 ) ;
#52699 = ORIENTED_EDGE ( 'NONE', *, *, #25059, .T. ) ;
#52700 = CARTESIAN_POINT ( 'NONE',  ( -37.00000000000000711, 11.80185301892987582, -4.824807283153995208 ) ) ;
#52701 = CARTESIAN_POINT ( 'NONE',  ( -22.31099767395440736, -3.142100240805189237, 2.106713667647948540 ) ) ;
#52702 = EDGE_CURVE ( 'NONE', #886, #37463, #16203, .T. ) ;
#52703 = DIRECTION ( 'NONE',  ( 0.9582930651793754029, 0.2851010602429193685, -0.01979360193296059167 ) ) ;
#52704 = CARTESIAN_POINT ( 'NONE',  ( 47.00000000000000711, 4.705694406421931860E-17, -3.469127814946512892E-15 ) ) ;
#52705 = CARTESIAN_POINT ( 'NONE',  ( 5.520433897694421610, 0.01120198501134835739, 0.01006947824912426785 ) ) ;
#52706 = CYLINDRICAL_SURFACE ( 'NONE', #6501, 12.75000000000000178 ) ;
#52707 = CARTESIAN_POINT ( 'NONE',  ( 10.09531169970623488, 1.650681656277897869, -11.88740217892082995 ) ) ;
#52708 = EDGE_CURVE ( 'NONE', #30956, #2445, #19403, .T. ) ;
#52710 = ORIENTED_EDGE ( 'NONE', *, *, #56280, .T. ) ;
#52709 = EDGE_CURVE ( 'NONE', #32709, #45989, #57502, .T. ) ;
#52711 = FACE_OUTER_BOUND ( 'NONE', #62278, .T. ) ;
#52712 = CARTESIAN_POINT ( 'NONE',  ( 0.3160775863651107964, -1.892533050396085992, -12.11619190710940686 ) ) ;
#52713 = CARTESIAN_POINT ( 'NONE',  ( -23.18047892478189453, -2.037851053449323935, -4.338318103648305168 ) ) ;
#52714 = CARTESIAN_POINT ( 'NONE',  ( -41.00000000000000711, -45.00200000000000244, 4.499999999999997335 ) ) ;
#52715 = EDGE_CURVE ( 'NONE', #36890, #52926, #23714, .T. ) ;
#52716 = DIRECTION ( 'NONE',  ( -1.000000000000000000, 0.000000000000000000, 0.000000000000000000 ) ) ;
#52717 = DIRECTION ( 'NONE',  ( 0.000000000000000000, 0.01356324068817998940, -0.9999080150203990547 ) ) ;
#52718 = ORIENTED_EDGE ( 'NONE', *, *, #37311, .T. ) ;
#52719 = CARTESIAN_POINT ( 'NONE',  ( -35.00000000000000000, -4.237620530777717498, -11.42599468261433771 ) ) ;
#52720 = CARTESIAN_POINT ( 'NONE',  ( -27.46687570686240676, -13.11534287648462360, -3.247842855528481731 ) ) ;
#52721 = CARTESIAN_POINT ( 'NONE',  ( 0.2833330754217431302, 9.254504746325796560, 8.029341648258402131 ) ) ;
#52722 = CARTESIAN_POINT ( 'NONE',  ( -25.00000000000000355, -28.99999999999999645, 5.000000000000000888 ) ) ;
#52723 = ORIENTED_EDGE ( 'NONE', *, *, #39752, .F. ) ;
#52724 = CARTESIAN_POINT ( 'NONE',  ( 0.3632410797595245766, 2.390576695689105247, 12.04386719438560327 ) ) ;
#52725 = CYLINDRICAL_SURFACE ( 'NONE', #21348, 5.000000000000000888 ) ;
#52726 = ORIENTED_EDGE ( 'NONE', *, *, #55672, .T. ) ;
#52727 = CARTESIAN_POINT ( 'NONE',  ( 0.000000000000000000, -7.484036900328561615, -0.4890722589970097345 ) ) ;
#52728 = ADVANCED_FACE ( 'NONE', ( #20920 ), #37188, .T. ) ;
#52729 = VECTOR ( 'NONE', #63657, 1000.000000000000000 ) ;
#52730 = DIRECTION ( 'NONE',  ( -1.000000000000000000, 0.000000000000000000, 0.000000000000000000 ) ) ;
#52731 = VERTEX_POINT ( 'NONE', #41863 ) ;
#52732 = EDGE_CURVE ( 'NONE', #63997, #36620, #14062, .T. ) ;
#52733 = DIRECTION ( 'NONE',  ( 0.000000000000000000, 0.8369827122275362852, 0.5472293298355244140 ) ) ;
#52734 = DIRECTION ( 'NONE',  ( 1.000000000000000000, 0.000000000000000000, -0.000000000000000000 ) ) ;
#52736 = VECTOR ( 'NONE', #39941, 1000.000000000000000 ) ;
#52735 = DIRECTION ( 'NONE',  ( 0.000000000000000000, 0.01356324068817998940, -0.9999080150203990547 ) ) ;
#52737 = DIRECTION ( 'NONE',  ( -1.000000000000000000, 0.000000000000000000, 0.000000000000000000 ) ) ;
#52738 = CARTESIAN_POINT ( 'NONE',  ( 0.2676618633000468206, -11.45242956837284432, -4.339362305359559357 ) ) ;
#52739 = CARTESIAN_POINT ( 'NONE',  ( 35.00000000000000000, -7.376655759824808811, 9.700295462048739381 ) ) ;
#52741 = VERTEX_POINT ( 'NONE', #36554 ) ;
#52740 = CARTESIAN_POINT ( 'NONE',  ( -2.812344914800139151, 12.94091111974183050, 3.845999582511304027 ) ) ;
#52742 = CARTESIAN_POINT ( 'NONE',  ( 9.775898761646960367, 6.948960757856110781, 11.57769295466150083 ) ) ;
#52743 = EDGE_LOOP ( 'NONE', ( #43896, #47506, #46336, #8924 ) ) ;
#52744 = CARTESIAN_POINT ( 'NONE',  ( -22.30625920655495165, -3.687109008463848703, -0.8854385781085442053 ) ) ;
#52745 = ORIENTED_EDGE ( 'NONE', *, *, #17642, .T. ) ;
#52746 = APPLICATION_PROTOCOL_DEFINITION ( 'draft international standard', 'automotive_design', 1998, #17072 ) ;
#52747 = FACE_OUTER_BOUND ( 'NONE', #38958, .T. ) ;
#52748 = CARTESIAN_POINT ( 'NONE',  ( 3.152665057734130638, -4.725420687650661478, -6.378477742800524375 ) ) ;
#52749 = CARTESIAN_POINT ( 'NONE',  ( 2.556980015514155102, 1.570584617272727357, 7.578583798307265695 ) ) ;
#52750 = CARTESIAN_POINT ( 'NONE',  ( -47.72075422404362399, -0.4543357781461417333, 7.770873616088293190 ) ) ;
#52751 = CARTESIAN_POINT ( 'NONE',  ( 37.00000000000000711, 7.971186206369473837, -9.217970097227755844 ) ) ;
#52752 = ORIENTED_EDGE ( 'NONE', *, *, #36722, .T. ) ;
#52753 = CARTESIAN_POINT ( 'NONE',  ( -24.55403303652017399, -6.841724855681644790, 9.860983143791417049 ) ) ;
#52754 = DIRECTION ( 'NONE',  ( 1.000000000000000000, -0.000000000000000000, -0.000000000000000000 ) ) ;
#52755 = VERTEX_POINT ( 'NONE', #31554 ) ;
#52756 = VERTEX_POINT ( 'NONE', #16603 ) ;
#52757 = CARTESIAN_POINT ( 'NONE',  ( 1.452237505248552996, -4.880303821311088974, 11.67686475128078172 ) ) ;
#52758 = ORIENTED_EDGE ( 'NONE', *, *, #63633, .T. ) ;
#52759 = DIRECTION ( 'NONE',  ( 0.000000000000000000, 0.3218879778915904044, -0.9467777615094594701 ) ) ;
#52760 = CARTESIAN_POINT ( 'NONE',  ( -10.90165637463012516, -7.508992741355087652, 9.360289953322833867 ) ) ;
#52761 = CARTESIAN_POINT ( 'NONE',  ( 2.000000000000001776, 6.470132594555847660, -2.133363481234036296 ) ) ;
#52762 = CARTESIAN_POINT ( 'NONE',  ( -27.08871896697694126, 0.9878677378267041176, -2.082324523415897577 ) ) ;
#52763 = CARTESIAN_POINT ( 'NONE',  ( 2.000000000000001776, -6.662861565602053560, -1.421313227905724341 ) ) ;
#52764 = CARTESIAN_POINT ( 'NONE',  ( 2.573738926104375935, -7.664876274722922211, 1.112690714006513204 ) ) ;
#52765 = CARTESIAN_POINT ( 'NONE',  ( 2.261269890822072970, 7.499479675451366845, 1.464004156081675889 ) ) ;
#52766 = EDGE_CURVE ( 'NONE', #46638, #2528, #63992, .T. ) ;
#52767 = VERTEX_POINT ( 'NONE', #63128 ) ;
#52768 = CARTESIAN_POINT ( 'NONE',  ( 37.00000000000000711, 4.705694406421931860E-17, -3.469127814946512892E-15 ) ) ;
#52769 = ORIENTED_EDGE ( 'NONE', *, *, #61158, .F. ) ;
#52770 = CARTESIAN_POINT ( 'NONE',  ( -36.00000000000000711, -12.42372387097880626, -2.865935305911760267 ) ) ;
#52771 = CARTESIAN_POINT ( 'NONE',  ( -9.274221350650309503, -12.48030023152219670, -5.158876694329755708 ) ) ;
#52772 = CARTESIAN_POINT ( 'NONE',  ( 2.284126774967659479, -3.960764882115048735, 6.543266298866119435 ) ) ;
#52773 = CARTESIAN_POINT ( 'NONE',  ( -37.00000000000000711, 11.39945968423479883, -5.710938531231588122 ) ) ;
#52774 = VERTEX_POINT ( 'NONE', #13251 ) ;
#52775 = ORIENTED_EDGE ( 'NONE', *, *, #43573, .F. ) ;
#52776 = EDGE_CURVE ( 'NONE', #31867, #22729, #42710, .T. ) ;
#52777 = CARTESIAN_POINT ( 'NONE',  ( 0.000000000000000000, -0.08317740279924559776, -7.499538753794370294 ) ) ;
#52778 = CIRCLE ( 'NONE', #65471, 12.73084802173761787 ) ;
#52779 = ORIENTED_EDGE ( 'NONE', *, *, #11581, .T. ) ;
#52780 = CARTESIAN_POINT ( 'NONE',  ( 0.2647959493198551173, 7.758440170207294706, -9.474789498086916950 ) ) ;
#52781 = LINE ( 'NONE', #27491, #33539 ) ;
#52782 = CARTESIAN_POINT ( 'NONE',  ( 0.9232167919969127556, -9.809608956680815339, -7.691547553333223597 ) ) ;
#52783 = DIRECTION ( 'NONE',  ( -1.000000000000000000, 0.000000000000000000, 0.000000000000000000 ) ) ;
#52784 = ORIENTED_EDGE ( 'NONE', *, *, #35083, .T. ) ;
#52785 = CARTESIAN_POINT ( 'NONE',  ( 2.705197763288538670, 2.399370654839271477, 7.410249563424426533 ) ) ;
#52786 = DIRECTION ( 'NONE',  ( 1.000000000000000000, 0.000000000000000000, -0.000000000000000000 ) ) ;
#52787 = CARTESIAN_POINT ( 'NONE',  ( 2.589278595513820225, -1.107986312493286496, 7.670769623692575756 ) ) ;
#52788 = CARTESIAN_POINT ( 'NONE',  ( 2.000000000000001776, -6.883677378339447372, -0.8544109087186817497 ) ) ;
#52789 = CARTESIAN_POINT ( 'NONE',  ( 0.000000000000000000, 0.000000000000000000, 0.000000000000000000 ) ) ;
#52790 = CARTESIAN_POINT ( 'NONE',  ( 2.889800649504073782, 3.986129653162648001, 4.645655809191377550 ) ) ;
#52791 = EDGE_LOOP ( 'NONE', ( #8295, #53075, #19183, #38 ) ) ;
#52792 = CARTESIAN_POINT ( 'NONE',  ( -11.75561129372955094, -29.30098385689620244, -6.671426272441853378 ) ) ;
#52793 = ORIENTED_EDGE ( 'NONE', *, *, #2651, .T. ) ;
#52794 = CYLINDRICAL_SURFACE ( 'NONE', #18534, 12.18649999999999878 ) ;
#52795 = CARTESIAN_POINT ( 'NONE',  ( 35.00000000000000000, -11.30684963584392477, -4.545979934229371189 ) ) ;
#52796 = CARTESIAN_POINT ( 'NONE',  ( 0.2655924914740778742, 12.24627751708824341, -0.04405032194307659937 ) ) ;
#52797 = FACE_OUTER_BOUND ( 'NONE', #45524, .T. ) ;
#52798 = CARTESIAN_POINT ( 'NONE',  ( 35.00000000000000000, -9.908974237959688125, -6.307491713048997362 ) ) ;
#52799 = EDGE_CURVE ( 'NONE', #46276, #55675, #15143, .T. ) ;
#52800 = ORIENTED_EDGE ( 'NONE', *, *, #20493, .T. ) ;
#52801 = EDGE_LOOP ( 'NONE', ( #47698, #1844, #56704, #44328 ) ) ;
#52802 = CARTESIAN_POINT ( 'NONE',  ( 0.2646305136544072623, 7.972778379581675345, -9.296005949277148517 ) ) ;
#52803 = ORIENTED_EDGE ( 'NONE', *, *, #36834, .T. ) ;
#52804 = CARTESIAN_POINT ( 'NONE',  ( 0.6825652211286046267, 0.5155054322761191132, 11.99253999668229653 ) ) ;
#52805 = DIRECTION ( 'NONE',  ( 0.000000000000000000, 0.000000000000000000, 1.000000000000000000 ) ) ;
#52806 = CARTESIAN_POINT ( 'NONE',  ( 2.903928887688015159, 8.528865300113499970, -2.041797854847570370 ) ) ;
#52807 = CARTESIAN_POINT ( 'NONE',  ( 0.4613984246114881116, 3.943860067443805129, -11.66278164635730619 ) ) ;
#52808 = DIRECTION ( 'NONE',  ( -1.000000000000000000, 0.000000000000000000, 0.000000000000000000 ) ) ;
#52809 = CARTESIAN_POINT ( 'NONE',  ( 5.515188684475870851, 0.003709313826049746507, -0.003857086913166404493 ) ) ;
#52810 = DIRECTION ( 'NONE',  ( 1.000000000000000000, 0.000000000000000000, 0.000000000000000000 ) ) ;
#52811 = ORIENTED_EDGE ( 'NONE', *, *, #63625, .F. ) ;
#52812 = ORIENTED_EDGE ( 'NONE', *, *, #9137, .F. ) ;
#52813 = CARTESIAN_POINT ( 'NONE',  ( 1.459561108993326473, -5.767168887069098915, 11.25243317554898859 ) ) ;
#52814 = EDGE_LOOP ( 'NONE', ( #4969, #5485, #7606, #24766 ) ) ;
#52815 = CIRCLE ( 'NONE', #23064, 5.000000000000000888 ) ;
#52816 =( NAMED_UNIT ( * ) PLANE_ANGLE_UNIT ( ) SI_UNIT ( $, .RADIAN. ) );
#52817 = CARTESIAN_POINT ( 'NONE',  ( 35.00000000000000000, 4.705694406421931860E-17, -3.469127814946512892E-15 ) ) ;
#52818 = EDGE_CURVE ( 'NONE', #59168, #25513, #52343, .T. ) ;
#52819 = CARTESIAN_POINT ( 'NONE',  ( 8.621148270653568702, 25.00000000000000000, -5.251012286260225537 ) ) ;
#52820 = AXIS2_PLACEMENT_3D ( 'NONE', #4000, #19291, #5222 ) ;
#52821 = CARTESIAN_POINT ( 'NONE',  ( 35.00000000000000000, 4.705694406421931860E-17, -3.469127814946512892E-15 ) ) ;
#52822 = ORIENTED_EDGE ( 'NONE', *, *, #53823, .T. ) ;
#52823 = CARTESIAN_POINT ( 'NONE',  ( 1.937114397841935398, -0.9020203649530801338, -12.80345148322680160 ) ) ;
#52824 =( BOUNDED_CURVE ( )  B_SPLINE_CURVE ( 3, ( #42963, #63900, #58616, #17710 ),
 .UNSPECIFIED., .F., .F. ) 
 B_SPLINE_CURVE_WITH_KNOTS ( ( 4, 4 ),
 ( 1.252925267387246189, 1.274022647499400307 ),
 .UNSPECIFIED. ) 
 CURVE ( )  GEOMETRIC_REPRESENTATION_ITEM ( )  RATIONAL_B_SPLINE_CURVE ( ( 1.000000000000000000, 0.9999629087233127267, 0.9999629087233127267, 1.000000000000000000 ) ) 
 REPRESENTATION_ITEM ( '' )  );
#52825 = LINE ( 'NONE', #16266, #12682 ) ;
#52826 = CARTESIAN_POINT ( 'NONE',  ( -36.00000000000000711, -5.865551165831157654, 11.32068061209293219 ) ) ;
#52827 = ORIENTED_EDGE ( 'NONE', *, *, #28482, .T. ) ;
#52828 = VERTEX_POINT ( 'NONE', #13555 ) ;
#52829 = CARTESIAN_POINT ( 'NONE',  ( 3.417879546546324310, 5.772183446363515991, 12.20553527385939141 ) ) ;
#52830 = ORIENTED_EDGE ( 'NONE', *, *, #12305, .F. ) ;
#52831 = VERTEX_POINT ( 'NONE', #22909 ) ;
#52832 = CARTESIAN_POINT ( 'NONE',  ( 2.000000000000001776, 0.000000000000000000, 0.000000000000000000 ) ) ;
#52833 = ORIENTED_EDGE ( 'NONE', *, *, #4909, .T. ) ;
#52834 = ORIENTED_EDGE ( 'NONE', *, *, #17485, .T. ) ;
#52835 = CARTESIAN_POINT ( 'NONE',  ( 2.241509619876137283, -7.187074272457174118, 2.575142053947843124 ) ) ;
#52836 = CARTESIAN_POINT ( 'NONE',  ( 2.261269890821711481, 5.017604628138070844, -5.762737836065258357 ) ) ;
#52837 = EDGE_CURVE ( 'NONE', #61990, #23681, #34168, .T. ) ;
#52838 = DIRECTION ( 'NONE',  ( 0.000000000000000000, -0.3218879778916040602, 0.9467777615094549182 ) ) ;
#52839 = CARTESIAN_POINT ( 'NONE',  ( 0.2648978790185584908, 7.972372351883154629, -9.295532325666371776 ) ) ;
#52840 = CARTESIAN_POINT ( 'NONE',  ( 35.00000000000000000, 6.036400161834703404, 10.07641281632170838 ) ) ;
#52841 = DIRECTION ( 'NONE',  ( -1.000000000000000000, -0.000000000000000000, 0.000000000000000000 ) ) ;
#52842 = EDGE_CURVE ( 'NONE', #33705, #63532, #20427, .T. ) ;
#52843 = ORIENTED_EDGE ( 'NONE', *, *, #13348, .F. ) ;
#52844 = DIRECTION ( 'NONE',  ( -1.000000000000000000, 0.000000000000000000, 0.000000000000000000 ) ) ;
#52845 = DIRECTION ( 'NONE',  ( -1.000000000000000000, -0.000000000000000000, 0.000000000000000000 ) ) ;
#52846 = EDGE_CURVE ( 'NONE', #58393, #33730, #12913, .T. ) ;
#52847 = CARTESIAN_POINT ( 'NONE',  ( 0.2655924914740778187, -0.04405032194311705313, 12.24627751708824341 ) ) ;
#52848 = CARTESIAN_POINT ( 'NONE',  ( 0.2648978790185619880, -7.972372351882965447, -9.295532325666529871 ) ) ;
#52849 = CARTESIAN_POINT ( 'NONE',  ( 47.00000000000000711, 4.705694406421931860E-17, -3.469127814946512892E-15 ) ) ;
#52850 = CARTESIAN_POINT ( 'NONE',  ( 0.3223008802179319621, -11.60682919296348281, -3.964361764750287787 ) ) ;
#52851 = AXIS2_PLACEMENT_3D ( 'NONE', #23305, #37617, #12646 ) ;
#52852 = ORIENTED_EDGE ( 'NONE', *, *, #35123, .T. ) ;
#52853 = EDGE_CURVE ( 'NONE', #36890, #56049, #17593, .T. ) ;
#52854 = DIRECTION ( 'NONE',  ( -1.000000000000000000, 0.000000000000000000, 0.000000000000000000 ) ) ;
#52855 = CIRCLE ( 'NONE', #31615, 4.999999999999999112 ) ;
#52856 = ORIENTED_EDGE ( 'NONE', *, *, #12653, .F. ) ;
#52857 = EDGE_CURVE ( 'NONE', #49536, #9428, #22575, .T. ) ;
#52858 = CYLINDRICAL_SURFACE ( 'NONE', #50838, 5.000000000000000888 ) ;
#52859 = CARTESIAN_POINT ( 'NONE',  ( 2.258463476536643366, 5.939075453322746334, -4.806099079317481149 ) ) ;
#52860 = DIRECTION ( 'NONE',  ( 0.000000000000000000, 0.000000000000000000, 1.000000000000000000 ) ) ;
#52861 = CARTESIAN_POINT ( 'NONE',  ( -25.86628395826706850, 25.00000000000000000, 10.84354029019568522 ) ) ;
#52862 = CARTESIAN_POINT ( 'NONE',  ( 2.573738926104374158, -4.796056562246135968, -6.081632213771440476 ) ) ;
#52863 = ORIENTED_EDGE ( 'NONE', *, *, #62003, .F. ) ;
#52864 = CARTESIAN_POINT ( 'NONE',  ( 1.194176325881332490, 10.60746084433564462, -6.717888447700713250 ) ) ;
#52865 = CARTESIAN_POINT ( 'NONE',  ( -36.00000000000000711, 12.49688848680888142, -2.527899948230499572 ) ) ;
#52866 = DIRECTION ( 'NONE',  ( 1.000000000000000000, 0.000000000000000000, -0.000000000000000000 ) ) ;
#52867 = CIRCLE ( 'NONE', #24183, 12.18650000000000055 ) ;
#52868 = CARTESIAN_POINT ( 'NONE',  ( -4.050859062405498534, 11.17340644476572109, 7.587242358561010924 ) ) ;
#52869 = AXIS2_PLACEMENT_3D ( 'NONE', #35305, #55618, #20027 ) ;
#52870 = EDGE_CURVE ( 'NONE', #853, #49572, #58709, .T. ) ;
#52871 = DIRECTION ( 'NONE',  ( 0.000000000000000000, 1.000000000000000000, 0.000000000000000000 ) ) ;
#52872 = ORIENTED_EDGE ( 'NONE', *, *, #62506, .T. ) ;
#52873 = CARTESIAN_POINT ( 'NONE',  ( 2.177405672430317463, -5.005033771133682308, 10.01846874165406476 ) ) ;
#52874 = DIRECTION ( 'NONE',  ( 0.000000000000000000, 0.000000000000000000, -1.000000000000000000 ) ) ;
#52875 = EDGE_LOOP ( 'NONE', ( #33787, #36746, #39598, #56512 ) ) ;
#52876 = CARTESIAN_POINT ( 'NONE',  ( 37.00000000000000711, 4.705694406421931860E-17, -3.469127814946512892E-15 ) ) ;
#52877 = ORIENTED_EDGE ( 'NONE', *, *, #38585, .T. ) ;
#52878 = CARTESIAN_POINT ( 'NONE',  ( -18.37106647529896719, 3.948826690502797998, 11.33420767669607443 ) ) ;
#52879 = CARTESIAN_POINT ( 'NONE',  ( -22.65999102136914445, 4.450325798697177149, -1.886119913916055602 ) ) ;
#52880 = LINE ( 'NONE', #2705, #45994 ) ;
#52881 = CARTESIAN_POINT ( 'NONE',  ( 1.459561108993324030, -7.633517148169429944, 10.08002506399545517 ) ) ;
#52882 = CARTESIAN_POINT ( 'NONE',  ( -22.28121537037576871, -2.114437713163344501, -3.028566507474733882 ) ) ;
#52883 = ORIENTED_EDGE ( 'NONE', *, *, #43284, .T. ) ;
#52884 = ORIENTED_EDGE ( 'NONE', *, *, #49128, .T. ) ;
#52885 = ORIENTED_EDGE ( 'NONE', *, *, #50993, .T. ) ;
#52886 = DIRECTION ( 'NONE',  ( 1.000000000000000000, 0.000000000000000000, 0.000000000000000000 ) ) ;
#52887 = EDGE_CURVE ( 'NONE', #15452, #43301, #52301, .T. ) ;
#52888 = LINE ( 'NONE', #7321, #18336 ) ;
#52889 = ORIENTED_EDGE ( 'NONE', *, *, #3052, .F. ) ;
#52890 = CARTESIAN_POINT ( 'NONE',  ( 0.000000000000000000, 0.000000000000000000, 0.000000000000000000 ) ) ;
#52891 = DIRECTION ( 'NONE',  ( -1.000000000000000000, 0.000000000000000000, 0.000000000000000000 ) ) ;
#52893 = ORIENTED_EDGE ( 'NONE', *, *, #14998, .T. ) ;
#52892 = AXIS2_PLACEMENT_3D ( 'NONE', #13184, #17842, #58087 ) ;
#52894 = CARTESIAN_POINT ( 'NONE',  ( 0.2650492433740066489, 11.46945725111973147, -4.291726136518433599 ) ) ;
#52895 = CARTESIAN_POINT ( 'NONE',  ( 35.00000000000000000, -11.32068061209299081, -5.865551165831040414 ) ) ;
#52896 = CARTESIAN_POINT ( 'NONE',  ( 24.83648533618617193, -1.531185848485796530, 11.90359809980858330 ) ) ;
#52897 = ORIENTED_EDGE ( 'NONE', *, *, #8149, .T. ) ;
#52898 = ORIENTED_EDGE ( 'NONE', *, *, #40939, .T. ) ;
#52899 = AXIS2_PLACEMENT_3D ( 'NONE', #3472, #3134, #59301 ) ;
#52900 = CARTESIAN_POINT ( 'NONE',  ( 35.00000000000000000, 11.78977382767499549, -4.245927698352105928 ) ) ;
#52901 = ORIENTED_EDGE ( 'NONE', *, *, #62091, .F. ) ;
#52902 = B_SPLINE_CURVE_WITH_KNOTS ( 'NONE', 3,
 ( #28253, #53197, #7643, #63807, #18288, #49840, #8617, #65120, #14560, #4950, #40503, #39855, #34838, #55144, #34206, #33881, #45174, #19258, #65752 ),
 .UNSPECIFIED., .F., .F.,
 ( 4, 3, 3, 3, 3, 3, 4 ),
 ( 0.000000000000000000, 2.836829843012721202E-05, 4.224792512550943312E-05, 5.612066614913196127E-05, 6.998859278354792356E-05, 9.832141288087241804E-05, 0.0001178161482478536071 ),
 .UNSPECIFIED. ) ;
#52903 = CARTESIAN_POINT ( 'NONE',  ( 8.460324815083970051, 3.946969223371512125, -12.91307448586167617 ) ) ;
#52904 = VERTEX_POINT ( 'NONE', #2648 ) ;
#52905 = CIRCLE ( 'NONE', #16776, 5.000000000000000000 ) ;
#52906 = CARTESIAN_POINT ( 'NONE',  ( 2.251139882113958990, 3.710800524304825654, 6.675617500148614880 ) ) ;
#52907 = CARTESIAN_POINT ( 'NONE',  ( 0.000000000000000000, -7.387287142779349836, 1.295372019972131028 ) ) ;
#52908 = CARTESIAN_POINT ( 'NONE',  ( -35.00000000000000000, -6.036400161834495570, -10.07641281632183983 ) ) ;
#52909 = DIRECTION ( 'NONE',  ( -1.000000000000000000, 0.000000000000000000, -0.000000000000000000 ) ) ;
#52910 = EDGE_CURVE ( 'NONE', #21432, #33447, #60775, .T. ) ;
#52911 = CARTESIAN_POINT ( 'NONE',  ( 0.7400311444011714590, 11.53023780418231858, -4.574267895796732653 ) ) ;
#52912 = DIRECTION ( 'NONE',  ( 0.000000000000000000, 0.01356324068817992175, -0.9999080150203990547 ) ) ;
#52913 = CARTESIAN_POINT ( 'NONE',  ( 0.000000000000000000, -6.997684042076877553, -2.698595569414293127 ) ) ;
#52914 = ORIENTED_EDGE ( 'NONE', *, *, #9296, .F. ) ;
#52915 = CARTESIAN_POINT ( 'NONE',  ( 35.00000000000000000, 10.68873102412842258, -6.950793414699832695 ) ) ;
#52916 = ORIENTED_EDGE ( 'NONE', *, *, #52223, .T. ) ;
#52917 = CARTESIAN_POINT ( 'NONE',  ( 0.2648978790185584908, -4.312320170909314854, 11.46165506714226900 ) ) ;
#52918 = ADVANCED_FACE ( 'NONE', ( #18245 ), #40595, .T. ) ;
#52919 = DIRECTION ( 'NONE',  ( 1.000000000000000000, 0.000000000000000000, 0.000000000000000000 ) ) ;
#52920 = EDGE_CURVE ( 'NONE', #50194, #2564, #43163, .T. ) ;
#52921 = ORIENTED_EDGE ( 'NONE', *, *, #27101, .F. ) ;
#52922 = CARTESIAN_POINT ( 'NONE',  ( -18.12908327424137767, 6.849030978105520973, 9.857092249840578191 ) ) ;
#52923 = CARTESIAN_POINT ( 'NONE',  ( 0.3632410797595208574, 12.04386719438563169, -2.390576695688982234 ) ) ;
#52924 = CARTESIAN_POINT ( 'NONE',  ( -22.27218376572352554, 2.630375585211922385, 2.577901515391789466 ) ) ;
#52925 = ORIENTED_EDGE ( 'NONE', *, *, #561, .T. ) ;
#52926 = VERTEX_POINT ( 'NONE', #12566 ) ;
#52927 = ADVANCED_FACE ( 'NONE', ( #32846 ), #18894, .T. ) ;
#52928 = CARTESIAN_POINT ( 'NONE',  ( 2.907497136251082193, -6.976431712756687276, -3.613027414876620824 ) ) ;
#52929 = CIRCLE ( 'NONE', #907, 7.499999999999988454 ) ;
#52930 = VERTEX_POINT ( 'NONE', #53820 ) ;
#52931 = EDGE_CURVE ( 'NONE', #16286, #12785, #49121, .T. ) ;
#52932 = CARTESIAN_POINT ( 'NONE',  ( 2.406456491626382199, -10.00134798414796578, -2.970787154401012931 ) ) ;
#52933 = CARTESIAN_POINT ( 'NONE',  ( -35.00000000000000000, 9.821084925794572484, 7.215058775251292467 ) ) ;
#52934 = DIRECTION ( 'NONE',  ( 0.000000000000000000, 0.9985334138511235968, 0.05413890858542115547 ) ) ;
#52935 = FACE_OUTER_BOUND ( 'NONE', #820, .T. ) ;
#52936 = ORIENTED_EDGE ( 'NONE', *, *, #33875, .T. ) ;
#52937 = DIRECTION ( 'NONE',  ( 0.000000000000000000, 0.01356324068817992175, -0.9999080150203990547 ) ) ;
#52938 = EDGE_CURVE ( 'NONE', #34267, #39065, #31055, .T. ) ;
#52939 = ADVANCED_FACE ( 'NONE', ( #59142, #8575 ), #49174, .T. ) ;
#52940 = AXIS2_PLACEMENT_3D ( 'NONE', #13289, #39856, #18289 ) ;
#52941 = AXIS2_PLACEMENT_3D ( 'NONE', #30405, #497, #29733 ) ;
#52942 = CARTESIAN_POINT ( 'NONE',  ( 14.99320290036090064, -28.92253633446381400, -11.50449902612428055 ) ) ;
#52943 = DIRECTION ( 'NONE',  ( 0.000000000000000000, -0.9987865678893271815, 0.04924826701375695226 ) ) ;
#52944 = ADVANCED_FACE ( 'NONE', ( #60421 ), #54801, .T. ) ;
#52945 = CARTESIAN_POINT ( 'NONE',  ( 22.62448365577994736, 12.20317485621798781, -5.782486214010236658 ) ) ;
#52946 = DIRECTION ( 'NONE',  ( 0.000000000000000000, 0.01356324068817300540, -0.9999080150203989437 ) ) ;
#52947 = CARTESIAN_POINT ( 'NONE',  ( 35.00000000000000000, 11.13736569743274174, -4.946702696913213515 ) ) ;
#52948 = CARTESIAN_POINT ( 'NONE',  ( 0.3675815128205894289, 4.447030445008180344, 11.44679196252410946 ) ) ;
#52949 = CARTESIAN_POINT ( 'NONE',  ( 3.152665057734128862, 5.461013642405629476, -5.761241965769021256 ) ) ;
#52950 = VECTOR ( 'NONE', #19232, 1000.000000000000114 ) ;
#52951 = EDGE_LOOP ( 'NONE', ( #13975, #30785, #65038, #47358 ) ) ;
#52952 = CARTESIAN_POINT ( 'NONE',  ( 2.241311220309555097, -0.09281826062101325436, 7.633829235838275551 ) ) ;
#52953 = CARTESIAN_POINT ( 'NONE',  ( 0.2833330754217411318, -12.25052326018167115, -0.2021515668286960610 ) ) ;
#52954 = ORIENTED_EDGE ( 'NONE', *, *, #33030, .T. ) ;
#52955 = CARTESIAN_POINT ( 'NONE',  ( -22.30078715814471835, 3.743307663037642730, -0.2606204736986855175 ) ) ;
#52956 = CARTESIAN_POINT ( 'NONE',  ( -35.00000000000000000, -2.220215194441821360, -11.98254675519230794 ) ) ;
#52957 = ORIENTED_EDGE ( 'NONE', *, *, #65306, .T. ) ;
#52958 = LINE ( 'NONE', #62932, #22490 ) ;
#52959 = VERTEX_POINT ( 'NONE', #55106 ) ;
#52960 = CARTESIAN_POINT ( 'NONE',  ( 0.3610902822527226053, -5.910495176556258556, 10.76187877352511713 ) ) ;
#52961 = VERTEX_POINT ( 'NONE', #45791 ) ;
#52962 = ORIENTED_EDGE ( 'NONE', *, *, #21541, .T. ) ;
#52964 = EDGE_CURVE ( 'NONE', #57074, #15972, #1363, .T. ) ;
#52963 = CARTESIAN_POINT ( 'NONE',  ( -22.28236030719477512, -3.345835236227594933, -1.572829798448334815 ) ) ;
#52965 = VECTOR ( 'NONE', #54256, 1000.000000000000000 ) ;
#52966 = EDGE_LOOP ( 'NONE', ( #12310, #2384, #61878, #42432 ) ) ;
#52967 = CYLINDRICAL_SURFACE ( 'NONE', #51467, 4.999999999999998224 ) ;
#52968 = DIRECTION ( 'NONE',  ( -1.000000000000000000, 0.000000000000000000, 0.000000000000000000 ) ) ;
#52969 = DIRECTION ( 'NONE',  ( 0.000000000000000000, 0.7381862504171926576, -0.6745969609292690183 ) ) ;
#52970 = FACE_OUTER_BOUND ( 'NONE', #33774, .T. ) ;
#52971 = VERTEX_POINT ( 'NONE', #20529 ) ;
#52972 = DIRECTION ( 'NONE',  ( 0.000000000000000000, -0.01356324068817991828, 0.9999080150203990547 ) ) ;
#52973 = AXIS2_PLACEMENT_3D ( 'NONE', #32686, #37038, #11444 ) ;
#52974 = DIRECTION ( 'NONE',  ( 0.3939253465568944290, -0.1691689424289884447, 0.9034404741085536594 ) ) ;
#52975 = DIRECTION ( 'NONE',  ( -1.000000000000000000, -1.685093406416449860E-16, 1.011030131491573426E-17 ) ) ;
#52977 = ORIENTED_EDGE ( 'NONE', *, *, #1005, .F. ) ;
#52976 = CARTESIAN_POINT ( 'NONE',  ( -27.45775109278351067, -11.83395752356219255, -1.989333891161980894 ) ) ;
#52978 = FACE_OUTER_BOUND ( 'NONE', #1743, .T. ) ;
#52979 = VERTEX_POINT ( 'NONE', #15199 ) ;
#52980 = CARTESIAN_POINT ( 'NONE',  ( 5.514624014163232779, -0.002789935220458489469, -0.003060352188290538233 ) ) ;
#52981 = EDGE_CURVE ( 'NONE', #58976, #2866, #10209, .T. ) ;
#52982 = VERTEX_POINT ( 'NONE', #55777 ) ;
#52983 = CYLINDRICAL_SURFACE ( 'NONE', #9178, 5.000000000000000888 ) ;
#52984 = LINE ( 'NONE', #7102, #2409 ) ;
#52985 = AXIS2_PLACEMENT_3D ( 'NONE', #36123, #16843, #31796 ) ;
#52986 = CARTESIAN_POINT ( 'NONE',  ( 35.00000000000000000, 12.63095688309028830, -1.738225594540042884 ) ) ;
#52987 = ORIENTED_EDGE ( 'NONE', *, *, #40924, .F. ) ;
#52988 = DIRECTION ( 'NONE',  ( 0.000000000000000000, 0.01356324068817991828, -0.9999080150203990547 ) ) ;
#52989 = EDGE_CURVE ( 'NONE', #27385, #16341, #10884, .T. ) ;
#52990 = CARTESIAN_POINT ( 'NONE',  ( -22.27834755396593991, -2.447855249718982495, -2.756126180273669846 ) ) ;
#52991 = CARTESIAN_POINT ( 'NONE',  ( 13.39599373663352466, 12.21273670597637384, -5.770182307986416070 ) ) ;
#52992 = ORIENTED_EDGE ( 'NONE', *, *, #44023, .T. ) ;
#52993 = AXIS2_PLACEMENT_3D ( 'NONE', #27027, #62258, #11709 ) ;
#52994 = VERTEX_POINT ( 'NONE', #24197 ) ;
#52995 = DIRECTION ( 'NONE',  ( 1.000000000000000000, 0.000000000000000000, 0.000000000000000000 ) ) ;
#52996 = ORIENTED_EDGE ( 'NONE', *, *, #6162, .F. ) ;
#52997 = AXIS2_PLACEMENT_3D ( 'NONE', #51230, #41880, #57190 ) ;
#52998 = EDGE_CURVE ( 'NONE', #11928, #37322, #27572, .T. ) ;
#52999 = ORIENTED_EDGE ( 'NONE', *, *, #52842, .T. ) ;
#53000 = DIRECTION ( 'NONE',  ( -1.000000000000000000, 0.000000000000000000, -0.000000000000000000 ) ) ;
#53001 = DIRECTION ( 'NONE',  ( 0.000000000000000000, -0.8169148498130338609, 0.5767582926624880146 ) ) ;
#53002 = AXIS2_PLACEMENT_3D ( 'NONE', #45393, #25785, #36057 ) ;
#53003 = DIRECTION ( 'NONE',  ( -1.000000000000000000, -1.836970198721029688E-16, -0.000000000000000000 ) ) ;
#53004 = CARTESIAN_POINT ( 'NONE',  ( 5.520433897694421610, 0.01186170453199825517, -0.009283255140285221613 ) ) ;
#53005 = CYLINDRICAL_SURFACE ( 'NONE', #33763, 13.50000000000000178 ) ;
#53006 = FACE_OUTER_BOUND ( 'NONE', #52568, .T. ) ;
#53007 = DIRECTION ( 'NONE',  ( 1.000000000000000000, 0.000000000000000000, 0.000000000000000000 ) ) ;
#53008 =( BOUNDED_CURVE ( )  B_SPLINE_CURVE ( 3, ( #5070, #46289, #5394, #35301 ),
 .UNSPECIFIED., .F., .F. ) 
 B_SPLINE_CURVE_WITH_KNOTS ( ( 4, 4 ),
 ( 2.503486317769501479, 2.552693758193947282 ),
 .UNSPECIFIED. ) 
 CURVE ( )  GEOMETRIC_REPRESENTATION_ITEM ( )  RATIONAL_B_SPLINE_CURVE ( ( 1.000000000000000000, 0.9997982291625954199, 0.9997982291625954199, 1.000000000000000000 ) ) 
 REPRESENTATION_ITEM ( '' )  );
#53009 = ORIENTED_EDGE ( 'NONE', *, *, #32225, .F. ) ;
#53010 = LINE ( 'NONE', #62984, #60029 ) ;
#53011 = DIRECTION ( 'NONE',  ( -1.000000000000000000, 0.000000000000000000, 0.000000000000000000 ) ) ;
#53012 = ADVANCED_FACE ( 'NONE', ( #35133 ), #39818, .T. ) ;
#53013 = CARTESIAN_POINT ( 'NONE',  ( -28.67667724226168602, 1.888227992976679204, -0.1214114860980455846 ) ) ;
#53014 = DIRECTION ( 'NONE',  ( 1.000000000000000000, -0.000000000000000000, -0.000000000000000000 ) ) ;
#53015 = AXIS2_PLACEMENT_3D ( 'NONE', #4041, #49920, #64534 ) ;
#53016 = CYLINDRICAL_SURFACE ( 'NONE', #41722, 12.18650000000000055 ) ;
#53017 = EDGE_CURVE ( 'NONE', #43073, #47572, #2412, .T. ) ;
#53018 = CARTESIAN_POINT ( 'NONE',  ( -35.00000000000000000, 4.041347439435861943, 11.02904044024210428 ) ) ;
#53019 = ADVANCED_FACE ( 'NONE', ( #254 ), #4595, .T. ) ;
#53020 = DIRECTION ( 'NONE',  ( -0.000000000000000000, -0.000000000000000000, -1.000000000000000000 ) ) ;
#53021 = ORIENTED_EDGE ( 'NONE', *, *, #4837, .F. ) ;
#53022 = CARTESIAN_POINT ( 'NONE',  ( -27.08416974970326407, 0.4151546250413345462, 2.253221199357843929 ) ) ;
#53023 = CARTESIAN_POINT ( 'NONE',  ( 2.000000000000001776, 0.000000000000000000, 0.000000000000000000 ) ) ;
#53024 = CARTESIAN_POINT ( 'NONE',  ( -26.43258404273188233, -1.478864324198220226, -3.148308537883193647 ) ) ;
#53025 = CARTESIAN_POINT ( 'NONE',  ( 2.368238019615422463, -1.509700170844607392, -7.526794520527707810 ) ) ;
#53026 = DIRECTION ( 'NONE',  ( -1.000000000000000000, 0.000000000000000000, 0.000000000000000000 ) ) ;
#53027 = CYLINDRICAL_SURFACE ( 'NONE', #53206, 5.000000000000000888 ) ;
#53028 = AXIS2_PLACEMENT_3D ( 'NONE', #41480, #61776, #36517 ) ;
#53029 = ORIENTED_EDGE ( 'NONE', *, *, #61771, .T. ) ;
#53030 = CARTESIAN_POINT ( 'NONE',  ( 18.82996414057443957, -4.825507986298288365, 10.99672610388072869 ) ) ;
#53031 = CARTESIAN_POINT ( 'NONE',  ( 5.515188684475870851, 0.001485678338381512956, -0.005140903460551593009 ) ) ;
#53032 = DIRECTION ( 'NONE',  ( -1.000000000000000000, 0.000000000000000000, -0.000000000000000000 ) ) ;
#53033 = CARTESIAN_POINT ( 'NONE',  ( 0.9232167919969141989, -12.34114433434356606, -1.756271097262192660 ) ) ;
#53034 = ORIENTED_EDGE ( 'NONE', *, *, #52776, .F. ) ;
#53035 = CARTESIAN_POINT ( 'NONE',  ( 0.3164563675027637357, 2.365891945210813141, 12.03284811452138570 ) ) ;
#53036 = CARTESIAN_POINT ( 'NONE',  ( -27.32343372485685151, -1.625341394141119222, 2.534722478175137184 ) ) ;
#53037 = ORIENTED_EDGE ( 'NONE', *, *, #48896, .T. ) ;
#53038 = AXIS2_PLACEMENT_3D ( 'NONE', #50220, #10280, #4677 ) ;
#53039 = ORIENTED_EDGE ( 'NONE', *, *, #14168, .T. ) ;
#53040 = CARTESIAN_POINT ( 'NONE',  ( 35.00000000000000000, 4.705694406421931860E-17, -3.469127814946512892E-15 ) ) ;
#53041 = EDGE_CURVE ( 'NONE', #26195, #8028, #3933, .T. ) ;
#53042 = CARTESIAN_POINT ( 'NONE',  ( 0.2834382757448000167, -4.380429851625252446, -11.44241760114839934 ) ) ;
#53043 = ORIENTED_EDGE ( 'NONE', *, *, #43531, .T. ) ;
#53044 = FACE_OUTER_BOUND ( 'NONE', #7738, .T. ) ;
#53045 = EDGE_CURVE ( 'NONE', #5308, #49481, #2987, .T. ) ;
#53046 = CYLINDRICAL_SURFACE ( 'NONE', #30413, 12.75000000000000178 ) ;
#53047 = LINE ( 'NONE', #33737, #31200 ) ;
#53048 = LINE ( 'NONE', #32739, #85 ) ;
#53049 = CARTESIAN_POINT ( 'NONE',  ( 37.00000000000000711, -9.321877890560486435, -7.146664589317880178 ) ) ;
#53050 = CARTESIAN_POINT ( 'NONE',  ( -37.00000000000000711, -3.213188559034318992, 11.29812557209475798 ) ) ;
#53052 = ORIENTED_EDGE ( 'NONE', *, *, #60136, .F. ) ;
#53051 = CARTESIAN_POINT ( 'NONE',  ( -35.00000000000000000, -12.18632975068352842, -0.06441628369849203284 ) ) ;
#53053 = CARTESIAN_POINT ( 'NONE',  ( 1.462291587751482380, 4.914320681886612974, -11.65117843858603663 ) ) ;
#53054 = ORIENTED_EDGE ( 'NONE', *, *, #58476, .T. ) ;
#53055 = CARTESIAN_POINT ( 'NONE',  ( 23.48656543641403971, 2.894652911351478064, -11.64991943752887416 ) ) ;
#53056 = ORIENTED_EDGE ( 'NONE', *, *, #5578, .T. ) ;
#53057 = ADVANCED_FACE ( 'NONE', ( #21168 ), #47122, .T. ) ;
#53058 = ORIENTED_EDGE ( 'NONE', *, *, #44714, .T. ) ;
#53059 = FACE_OUTER_BOUND ( 'NONE', #45245, .T. ) ;
#53060 = CARTESIAN_POINT ( 'NONE',  ( -13.98431177871173858, -30.12623156650465006, 5.679219063900180942 ) ) ;
#53061 = DIRECTION ( 'NONE',  ( -1.000000000000000000, -0.000000000000000000, -0.000000000000000000 ) ) ;
#53062 = AXIS2_PLACEMENT_3D ( 'NONE', #17857, #12859, #53104 ) ;
#53063 = CIRCLE ( 'NONE', #10721, 12.18650000000000233 ) ;
#53064 = CARTESIAN_POINT ( 'NONE',  ( -34.90603985575356916, -2.603248520265800448, -21.87429913450488073 ) ) ;
#53065 = CARTESIAN_POINT ( 'NONE',  ( 0.2648978790185584908, 4.063980959785046032, 11.55204314799265042 ) ) ;
#53066 = VERTEX_POINT ( 'NONE', #61396 ) ;
#53067 = CARTESIAN_POINT ( 'NONE',  ( -22.27722015946438816, -0.6262261846986509894, -3.628085906632226632 ) ) ;
#53068 = VECTOR ( 'NONE', #20544, 1000.000000000000000 ) ;
#53069 = DIRECTION ( 'NONE',  ( 1.000000000000000000, 0.000000000000000000, 0.000000000000000000 ) ) ;
#53071 = ORIENTED_EDGE ( 'NONE', *, *, #24613, .T. ) ;
#53070 = CARTESIAN_POINT ( 'NONE',  ( 1.104777566491140561, -11.92547689818820622, -3.832109395972772337 ) ) ;
#53072 = EDGE_LOOP ( 'NONE', ( #34368, #58480, #28241, #21093 ) ) ;
#53073 = DIRECTION ( 'NONE',  ( 0.000000000000000000, 0.000000000000000000, 1.000000000000000000 ) ) ;
#53074 = EDGE_CURVE ( 'NONE', #57088, #50922, #56060, .T. ) ;
#53075 = ORIENTED_EDGE ( 'NONE', *, *, #61568, .F. ) ;
#53076 = CARTESIAN_POINT ( 'NONE',  ( 2.241352910868908310, 1.407733736974966288, -7.503490710578218703 ) ) ;
#53077 = CYLINDRICAL_SURFACE ( 'NONE', #63826, 4.500030059823568074 ) ;
#53078 = CARTESIAN_POINT ( 'NONE',  ( 12.27828125814611226, 0.5230329997979927814, 13.48988865648588664 ) ) ;
#53079 = EDGE_CURVE ( 'NONE', #21538, #51040, #30016, .T. ) ;
#53081 = CIRCLE ( 'NONE', #24396, 5.000000000000000888 ) ;
#53080 = DIRECTION ( 'NONE',  ( -1.000000000000000000, 0.000000000000000000, 0.000000000000000000 ) ) ;
#53082 = CARTESIAN_POINT ( 'NONE',  ( 35.00000000000000000, 0.7008968033240532414, 12.16632754454235332 ) ) ;
#53083 = CARTESIAN_POINT ( 'NONE',  ( 37.25000000000000711, -45.00200000000000244, 4.499999999999997335 ) ) ;
#53084 = LINE ( 'NONE', #48763, #33336 ) ;
#53085 = AXIS2_PLACEMENT_3D ( 'NONE', #6279, #41838, #31844 ) ;
#53086 = ORIENTED_EDGE ( 'NONE', *, *, #52870, .F. ) ;
#53087 = CARTESIAN_POINT ( 'NONE',  ( 0.000000000000000000, 1.058508696395052517, -6.730038252034905355 ) ) ;
#53088 = ORIENTED_EDGE ( 'NONE', *, *, #27593, .T. ) ;
#53089 = DIRECTION ( 'NONE',  ( 0.000000000000000000, -0.1387779952735886391, 0.9903235168508540687 ) ) ;
#53090 = FACE_OUTER_BOUND ( 'NONE', #13710, .T. ) ;
#53091 = LINE ( 'NONE', #7530, #55199 ) ;
#53092 = AXIS2_PLACEMENT_3D ( 'NONE', #6632, #26901, #47202 ) ;
#53093 = CARTESIAN_POINT ( 'NONE',  ( 29.20115507325780513, 4.760464791327699174, 11.01582872674790714 ) ) ;
#53094 = ADVANCED_FACE ( 'NONE', ( #20846 ), #56422, .T. ) ;
#53095 = EDGE_LOOP ( 'NONE', ( #15338, #58937, #18215, #43436 ) ) ;
#53096 = ORIENTED_EDGE ( 'NONE', *, *, #46333, .T. ) ;
#53097 = CARTESIAN_POINT ( 'NONE',  ( 0.2646305136544072623, 11.55263159009958862, 4.064188116014587848 ) ) ;
#53098 = EDGE_CURVE ( 'NONE', #45593, #8268, #16526, .T. ) ;
#53099 = ORIENTED_EDGE ( 'NONE', *, *, #5519, .F. ) ;
#53100 = CARTESIAN_POINT ( 'NONE',  ( 0.3057689695767464300, 7.702054583838595647, -9.538231270095025138 ) ) ;
#53101 = CARTESIAN_POINT ( 'NONE',  ( 5.514970785353741078, -0.002796696073589764048, 0.003805873180274775124 ) ) ;
#53102 = EDGE_CURVE ( 'NONE', #33298, #44156, #26173, .T. ) ;
#53103 = CARTESIAN_POINT ( 'NONE',  ( -27.09602251845210930, -2.092130925172070999, -1.018053071732930803 ) ) ;
#53104 = DIRECTION ( 'NONE',  ( 0.000000000000000000, 0.4198891015602657650, -0.9075754196709565624 ) ) ;
#53105 = B_SPLINE_CURVE_WITH_KNOTS ( 'NONE', 3,
 ( #18908, #49187, #33854, #8927, #34182, #24877, #59795, #19229, #18609, #29213, #24538, #54153, #45153 ),
 .UNSPECIFIED., .F., .F.,
 ( 4, 3, 3, 3, 4 ),
 ( 1.734723475976807094E-18, 6.607593386745386026E-05, 0.0001321518677373493709, 0.0001982171734706180679, 0.0002642860854759505602 ),
 .UNSPECIFIED. ) ;
#53106 = ORIENTED_EDGE ( 'NONE', *, *, #42480, .T. ) ;
#53107 = DIRECTION ( 'NONE',  ( 0.000000000000000000, 0.01356324068817992522, -0.9999080150203990547 ) ) ;
#53108 = CARTESIAN_POINT ( 'NONE',  ( -37.00000000000000711, 0.000000000000000000, 0.000000000000000000 ) ) ;
#53109 = CARTESIAN_POINT ( 'NONE',  ( 0.2653519991613819129, -10.59450977800977789, -6.142165520908282161 ) ) ;
#53110 = FACE_OUTER_BOUND ( 'NONE', #12379, .T. ) ;
#53111 = CIRCLE ( 'NONE', #37148, 7.499999999999988454 ) ;
#53112 = VECTOR ( 'NONE', #24140, 1000.000000000000000 ) ;
#53113 = CARTESIAN_POINT ( 'NONE',  ( 26.34661844826604593, 25.00000000000000000, 3.317828791472333005 ) ) ;
#53114 = DIRECTION ( 'NONE',  ( 1.000000000000000000, 0.000000000000000000, 0.000000000000000000 ) ) ;
#53115 = ORIENTED_EDGE ( 'NONE', *, *, #24719, .T. ) ;
#53116 = CARTESIAN_POINT ( 'NONE',  ( -22.27834755396593991, -3.643689482009667913, 0.5583491773602463626 ) ) ;
#53117 = DIRECTION ( 'NONE',  ( 1.000000000000000000, 0.000000000000000000, 0.000000000000000000 ) ) ;
#53118 = CARTESIAN_POINT ( 'NONE',  ( -12.31125281582930064, -29.30934768819284386, -5.548768499314231661 ) ) ;
#53119 = ORIENTED_EDGE ( 'NONE', *, *, #52524, .F. ) ;
#53120 = CARTESIAN_POINT ( 'NONE',  ( -9.039297670793269290, -2.446522702784146741, -13.27730549576870978 ) ) ;
#53121 = CARTESIAN_POINT ( 'NONE',  ( 0.5572780756284226866, -8.165890079445430771, 9.256402261579117052 ) ) ;
#53122 = CARTESIAN_POINT ( 'NONE',  ( 37.00000000000000711, -0.1414404973753014549, -12.74921544981111055 ) ) ;
#53123 = CARTESIAN_POINT ( 'NONE',  ( 0.3665391374699467075, 10.76665847464320969, -5.911453292029491102 ) ) ;
#53124 = CARTESIAN_POINT ( 'NONE',  ( 35.00000000000000000, 4.705694406421931860E-17, -3.469127814946512892E-15 ) ) ;
#53125 = CIRCLE ( 'NONE', #16996, 12.18650000000000055 ) ;
#53126 = EDGE_LOOP ( 'NONE', ( #58356, #35730, #46149, #4414, #61852, #50278 ) ) ;
#53127 = ORIENTED_EDGE ( 'NONE', *, *, #56669, .T. ) ;
#53128 = CARTESIAN_POINT ( 'NONE',  ( 0.3665391374699465965, -12.27992639892678461, 0.2638605131386725922 ) ) ;
#53129 = ORIENTED_EDGE ( 'NONE', *, *, #45323, .T. ) ;
#53130 = CIRCLE ( 'NONE', #50999, 12.18650000000000055 ) ;
#53131 = EDGE_CURVE ( 'NONE', #56731, #20463, #40276, .T. ) ;
#53132 = CARTESIAN_POINT ( 'NONE',  ( 2.000000000000001776, 6.796153407501467569, -1.388283512725773772 ) ) ;
#53133 = DIRECTION ( 'NONE',  ( 0.000000000000000000, 0.01356324068817998940, -0.9999080150203990547 ) ) ;
#53134 = CARTESIAN_POINT ( 'NONE',  ( 35.00000000000000000, -11.44858830469738109, 2.627174906297032209 ) ) ;
#53135 = FACE_OUTER_BOUND ( 'NONE', #47241, .T. ) ;
#53136 = CARTESIAN_POINT ( 'NONE',  ( 0.8375941296809088499, -7.696026447556186589, -9.769835228044549069 ) ) ;
#53137 = CARTESIAN_POINT ( 'NONE',  ( 2.258463476537679426, 5.764393264551986640, 5.014277205347752009 ) ) ;
#53138 = DIRECTION ( 'NONE',  ( 0.000000000000000000, 0.000000000000000000, 1.000000000000000000 ) ) ;
#53139 = ORIENTED_EDGE ( 'NONE', *, *, #51131, .F. ) ;
#53140 = VERTEX_POINT ( 'NONE', #27804 ) ;
#53141 = CARTESIAN_POINT ( 'NONE',  ( 35.00000000000000000, 1.771820996347156507, -11.61175578952786935 ) ) ;
#53142 = CIRCLE ( 'NONE', #29762, 5.000000000000000888 ) ;
#53143 = ORIENTED_EDGE ( 'NONE', *, *, #6039, .F. ) ;
#53144 =( NAMED_UNIT ( * ) PLANE_ANGLE_UNIT ( ) SI_UNIT ( $, .RADIAN. ) );
#53145 = CARTESIAN_POINT ( 'NONE',  ( 1.719304012338199517, 0.000000000000000000, 0.000000000000000000 ) ) ;
#53146 = CARTESIAN_POINT ( 'NONE',  ( 17.48690873012385438, 10.08597650261509671, 8.981318438147098959 ) ) ;
#53147 = ADVANCED_FACE ( 'NONE', ( #64354 ), #28451, .T. ) ;
#53148 = CARTESIAN_POINT ( 'NONE',  ( -35.00000000000000000, -5.130401251914653571, -11.05394794832835359 ) ) ;
#53149 = VERTEX_POINT ( 'NONE', #43750 ) ;
#53150 = FACE_OUTER_BOUND ( 'NONE', #21167, .T. ) ;
#53151 = DIRECTION ( 'NONE',  ( 0.000000000000000000, -0.2006870767258747135, 0.9796553971857772103 ) ) ;
#53152 = CARTESIAN_POINT ( 'NONE',  ( 2.770579946183334474, -1.653873933978927901, 7.633739187313470786 ) ) ;
#53153 = ORIENTED_EDGE ( 'NONE', *, *, #3331, .T. ) ;
#53154 = ORIENTED_EDGE ( 'NONE', *, *, #27600, .T. ) ;
#53155 = CARTESIAN_POINT ( 'NONE',  ( -35.00000000000000000, -0.7536123767499333104, 11.72195762423409704 ) ) ;
#53156 = ORIENTED_EDGE ( 'NONE', *, *, #61473, .T. ) ;
#53157 = ADVANCED_FACE ( 'NONE', ( #12827 ), #59810, .F. ) ;
#53158 = VERTEX_POINT ( 'NONE', #42752 ) ;
#53159 = CARTESIAN_POINT ( 'NONE',  ( -35.00000000000000000, 0.000000000000000000, 0.000000000000000000 ) ) ;
#53160 = VERTEX_POINT ( 'NONE', #23474 ) ;
#53161 = ORIENTED_EDGE ( 'NONE', *, *, #19608, .F. ) ;
#53162 = CARTESIAN_POINT ( 'NONE',  ( -22.27722022243423794, -2.798846704197242463, 2.391991868237150598 ) ) ;
#53163 = EDGE_CURVE ( 'NONE', #48281, #60037, #33453, .T. ) ;
#53164 = DIRECTION ( 'NONE',  ( 0.000000000000000000, 0.000000000000000000, 1.000000000000000000 ) ) ;
#53165 = AXIS2_PLACEMENT_3D ( 'NONE', #19261, #19596, #39858 ) ;
#53167 = CIRCLE ( 'NONE', #2177, 4.999999999999999112 ) ;
#53166 = FACE_BOUND ( 'NONE', #16490, .T. ) ;
#53168 = CARTESIAN_POINT ( 'NONE',  ( 0.3675815128205912052, 8.093875121226199454, -9.235491948679927177 ) ) ;
#53169 = CARTESIAN_POINT ( 'NONE',  ( 5.514970785353741078, -0.001897634820904511074, 0.004324946436530178843 ) ) ;
#53170 = CIRCLE ( 'NONE', #59521, 12.74999999999999822 ) ;
#53171 = CARTESIAN_POINT ( 'NONE',  ( 35.00000000000000000, -12.18359334611896294, -0.2661492558802951991 ) ) ;
#53172 = EDGE_LOOP ( 'NONE', ( #54869, #28951, #4124, #15519 ) ) ;
#53173 = CARTESIAN_POINT ( 'NONE',  ( -35.00000000000000000, -4.426194442447158650, -11.35427606708811155 ) ) ;
#53174 = DIRECTION ( 'NONE',  ( 0.000000000000000000, 0.000000000000000000, 1.000000000000000000 ) ) ;
#53175 = CARTESIAN_POINT ( 'NONE',  ( 37.00000000000000711, -9.752226076388938125, -6.547236723513990775 ) ) ;
#53176 = DIRECTION ( 'NONE',  ( 0.000000000000000000, 0.01356324068817998940, -0.9999080150203990547 ) ) ;
#53177 = CARTESIAN_POINT ( 'NONE',  ( 29.51976981715666781, 4.571419055710094881, 11.09513982864076276 ) ) ;
#53178 = DIRECTION ( 'NONE',  ( 0.000000000000000000, 0.7617968321374900542, 0.6478160128811920604 ) ) ;
#53179 = CARTESIAN_POINT ( 'NONE',  ( 2.000000000000001776, -6.338823199656649088, -2.816798305433765748 ) ) ;
#53180 = CARTESIAN_POINT ( 'NONE',  ( -35.00000000000000000, 9.060822531526156354, -7.474872387600913548 ) ) ;
#53181 = CARTESIAN_POINT ( 'NONE',  ( 1.287602823385183948, 5.809161206980673064, 11.16629420487727131 ) ) ;
#53182 = AXIS2_PLACEMENT_3D ( 'NONE', #63591, #48003, #12077 ) ;
#53183 = EDGE_CURVE ( 'NONE', #4358, #58669, #54476, .T. ) ;
#53184 = ORIENTED_EDGE ( 'NONE', *, *, #45109, .F. ) ;
#53185 = CYLINDRICAL_SURFACE ( 'NONE', #50342, 2.899999999999994582 ) ;
#53186 = ORIENTED_EDGE ( 'NONE', *, *, #33501, .T. ) ;
#53187 = CARTESIAN_POINT ( 'NONE',  ( 2.000000000000001776, 0.7281529553923113962, -7.464569195442801508 ) ) ;
#53188 = CARTESIAN_POINT ( 'NONE',  ( -19.26763262626409912, -29.00000000000001776, -5.969230316860659080 ) ) ;
#53189 = FACE_OUTER_BOUND ( 'NONE', #2396, .T. ) ;
#53190 = CIRCLE ( 'NONE', #12826, 5.000000000000000888 ) ;
#53191 = CARTESIAN_POINT ( 'NONE',  ( -22.27218376572352554, -2.630375585211905953, -2.577901515391840537 ) ) ;
#53192 = LINE ( 'NONE', #7639, #29641 ) ;
#53193 = ORIENTED_EDGE ( 'NONE', *, *, #52155, .T. ) ;
#53194 = CARTESIAN_POINT ( 'NONE',  ( -35.00000000000000000, 0.000000000000000000, 0.000000000000000000 ) ) ;
#53196 = AXIS2_PLACEMENT_3D ( 'NONE', #48596, #53249, #7696 ) ;
#53195 = CARTESIAN_POINT ( 'NONE',  ( 35.00000000000000000, 2.220215194442072271, 11.98254675519225287 ) ) ;
#53197 = CARTESIAN_POINT ( 'NONE',  ( -27.10422407540546885, 2.109093808474372000, 1.039355862229879524 ) ) ;
#53198 = CARTESIAN_POINT ( 'NONE',  ( 5.011577697822175992, -30.99110506585689251, -14.75067033891488144 ) ) ;
#53199 = EDGE_CURVE ( 'NONE', #62291, #50465, #19439, .T. ) ;
#53200 = AXIS2_PLACEMENT_3D ( 'NONE', #16674, #23308, #27298 ) ;
#53201 = FACE_OUTER_BOUND ( 'NONE', #57262, .T. ) ;
#53202 = EDGE_LOOP ( 'NONE', ( #43874, #54546, #40977, #9773 ) ) ;
#53203 = CARTESIAN_POINT ( 'NONE',  ( 36.00000000000000711, -10.12742074351890764, 7.745827850123114366 ) ) ;
#53204 = DIRECTION ( 'NONE',  ( -1.000000000000000000, 0.000000000000000000, -0.000000000000000000 ) ) ;
#53205 = CARTESIAN_POINT ( 'NONE',  ( 35.00000000000000000, 4.705694406421931860E-17, -3.469127814946512892E-15 ) ) ;
#53206 = AXIS2_PLACEMENT_3D ( 'NONE', #7462, #42056, #1843 ) ;
#53207 = VECTOR ( 'NONE', #64088, 1000.000000000000000 ) ;
#53208 = ORIENTED_EDGE ( 'NONE', *, *, #25982, .T. ) ;
#53209 = CARTESIAN_POINT ( 'NONE',  ( -35.00000000000000000, -5.636262487437237567, -10.80478261802188023 ) ) ;
#53211 = ORIENTED_EDGE ( 'NONE', *, *, #59439, .T. ) ;
#53210 = ADVANCED_FACE ( 'NONE', ( #44082 ), #12490, .T. ) ;
#53212 = FACE_OUTER_BOUND ( 'NONE', #2046, .T. ) ;
#53214 = CARTESIAN_POINT ( 'NONE',  ( 2.241528039335008327, -5.838210500619341659, -4.919377664485154789 ) ) ;
#53213 =( BOUNDED_SURFACE ( )  B_SPLINE_SURFACE ( 3, 1, ( 
 ( #5048, #30313 ),
 ( #55594, #25002 ),
 ( #45276, #14996 ),
 ( #65534, #35282 ) ),
 .UNSPECIFIED., .F., .F., .F. ) 
 B_SPLINE_SURFACE_WITH_KNOTS ( ( 4, 4 ),
 ( 2, 2 ),
 ( 0.000000000000000000, 1.000000000000000000 ),
 ( 0.000000000000000000, 1.000000000000000000 ),
 .UNSPECIFIED. ) 
 GEOMETRIC_REPRESENTATION_ITEM ( )  RATIONAL_B_SPLINE_SURFACE ( (
 ( 1.000000000000000000, 1.000000000000000000),
 ( 0.9942764183789327692, 0.8450855930916580938),
 ( 0.9942764183789327692, 0.8450855930916580938),
 ( 1.000000000000000000, 1.000000000000000000) ) ) 
 REPRESENTATION_ITEM ( '' )  SURFACE ( )  );
#53215 = CIRCLE ( 'NONE', #13887, 2.899999999999994582 ) ;
#53216 = CARTESIAN_POINT ( 'NONE',  ( -36.00000000000000711, -8.954052073409537016, -9.076753354954096409 ) ) ;
#53217 = CARTESIAN_POINT ( 'NONE',  ( -29.68541646480307250, -1.416020129149132334, 13.42553116244733680 ) ) ;
#53218 = CARTESIAN_POINT ( 'NONE',  ( -22.30527770659433173, -2.100259071719460024, -3.125767038151211263 ) ) ;
#53219 = EDGE_CURVE ( 'NONE', #47570, #20105, #33759, .T. ) ;
#53220 = ORIENTED_EDGE ( 'NONE', *, *, #19749, .T. ) ;
#53221 = VERTEX_POINT ( 'NONE', #58402 ) ;
#53222 = ORIENTED_EDGE ( 'NONE', *, *, #49350, .F. ) ;
#53223 = DIRECTION ( 'NONE',  ( 0.000000000000000000, -0.2006870767258747135, 0.9796553971857772103 ) ) ;
#53224 = AXIS2_PLACEMENT_3D ( 'NONE', #26897, #47198, #1644 ) ;
#53225 = CIRCLE ( 'NONE', #33039, 12.74999999999999822 ) ;
#53226 = CARTESIAN_POINT ( 'NONE',  ( 47.00000000000000711, 4.705694406421931860E-17, -3.469127814946512892E-15 ) ) ;
#53227 = ADVANCED_FACE ( 'NONE', ( #37448 ), #49095, .T. ) ;
#53228 = ORIENTED_EDGE ( 'NONE', *, *, #37073, .T. ) ;
#53229 = DIRECTION ( 'NONE',  ( 0.000000000000000000, -0.01356324068817998940, 0.9999080150203990547 ) ) ;
#53230 = AXIS2_PLACEMENT_3D ( 'NONE', #51576, #6985, #27258 ) ;
#53231 = CARTESIAN_POINT ( 'NONE',  ( -22.30527770659433173, -0.2559941915621662401, -3.757123197210725962 ) ) ;
#53232 = ORIENTED_EDGE ( 'NONE', *, *, #7197, .F. ) ;
#53233 = DIRECTION ( 'NONE',  ( -1.000000000000000000, 0.000000000000000000, 0.000000000000000000 ) ) ;
#53234 = CARTESIAN_POINT ( 'NONE',  ( 2.269879328256731110, -2.753278809616064748, -7.130835954829873202 ) ) ;
#53235 = CARTESIAN_POINT ( 'NONE',  ( 2.000000000000001776, -1.058508696395003890, 6.730038252034888480 ) ) ;
#53236 = ORIENTED_EDGE ( 'NONE', *, *, #38834, .T. ) ;
#53237 = AXIS2_PLACEMENT_3D ( 'NONE', #39061, #49412, #59690 ) ;
#53238 = VERTEX_POINT ( 'NONE', #48754 ) ;
#53239 = DIRECTION ( 'NONE',  ( -1.000000000000000000, -0.000000000000000000, 0.000000000000000000 ) ) ;
#53240 = ORIENTED_EDGE ( 'NONE', *, *, #48313, .F. ) ;
#53241 = EDGE_CURVE ( 'NONE', #46803, #64819, #38094, .T. ) ;
#53242 = CARTESIAN_POINT ( 'NONE',  ( 35.00000000000000000, 9.040300684349800164, 7.499679039483956977 ) ) ;
#53243 = ORIENTED_EDGE ( 'NONE', *, *, #16713, .T. ) ;
#53244 = AXIS2_PLACEMENT_3D ( 'NONE', #56431, #25856, #26492 ) ;
#53245 = CARTESIAN_POINT ( 'NONE',  ( 0.2646305136544065406, 0.1321451301299554348, -12.24595685781654275 ) ) ;
#53246 = DIRECTION ( 'NONE',  ( 0.000000000000000000, -0.4198891015602717602, 0.9075754196709537869 ) ) ;
#53247 = CARTESIAN_POINT ( 'NONE',  ( 35.00000000000000000, 9.040300684349800164, 7.499679039483956977 ) ) ;
#53248 = DIRECTION ( 'NONE',  ( 1.000000000000000000, -0.000000000000000000, -0.000000000000000000 ) ) ;
#53249 = DIRECTION ( 'NONE',  ( -1.000000000000000000, 0.000000000000000000, 0.000000000000000000 ) ) ;
#53250 = CARTESIAN_POINT ( 'NONE',  ( 5.515539859299206427, -0.002251761459665968176, -0.005618668168217485354 ) ) ;
#53251 = CARTESIAN_POINT ( 'NONE',  ( -27.22418447007674658, -9.103645632685440248, -7.837741149085147185 ) ) ;
#53252 = ORIENTED_EDGE ( 'NONE', *, *, #27410, .T. ) ;
#53253 = CARTESIAN_POINT ( 'NONE',  ( 37.00000000000000711, 6.657191900728455458, 9.677500615117825333 ) ) ;
#53254 = VERTEX_POINT ( 'NONE', #2886 ) ;
#53255 = DIRECTION ( 'NONE',  ( -1.000000000000000000, -1.836970198721029688E-16, 0.000000000000000000 ) ) ;
#53256 = CARTESIAN_POINT ( 'NONE',  ( 2.288423627606494648, 6.704349683465941290, 3.684511167348409888 ) ) ;
#53257 = VECTOR ( 'NONE', #17236, 1000.000000000000000 ) ;
#53258 = ORIENTED_EDGE ( 'NONE', *, *, #37931, .T. ) ;
#53259 = CARTESIAN_POINT ( 'NONE',  ( -16.85489546068752276, 8.063588271002045005, 8.887448980655202391 ) ) ;
#53260 = CARTESIAN_POINT ( 'NONE',  ( 0.3164563675027607936, 6.338687639236032290, 10.49799587805932255 ) ) ;
#53261 = CARTESIAN_POINT ( 'NONE',  ( 2.589278595512835235, -7.587119248534184734, 1.582391164331409916 ) ) ;
#53262 = ORIENTED_EDGE ( 'NONE', *, *, #28869, .F. ) ;
#53263 = AXIS2_PLACEMENT_3D ( 'NONE', #40515, #60812, #45187 ) ;
#53264 = AXIS2_PLACEMENT_3D ( 'NONE', #51726, #11153, #15785 ) ;
#53265 = VECTOR ( 'NONE', #52054, 1000.000000000000000 ) ;
#53266 = VERTEX_POINT ( 'NONE', #63049 ) ;
#53267 = LINE ( 'NONE', #43591, #10975 ) ;
#53268 = VERTEX_POINT ( 'NONE', #23143 ) ;
#53269 = CARTESIAN_POINT ( 'NONE',  ( -37.00000000000000711, 0.000000000000000000, 0.000000000000000000 ) ) ;
#53270 = DIRECTION ( 'NONE',  ( 0.000000000000000000, -0.01356324068817998940, 0.9999080150203990547 ) ) ;
#53271 = CARTESIAN_POINT ( 'NONE',  ( -2.532614230583026593, -7.965877694534051479, 10.89930238848911337 ) ) ;
#53272 = CARTESIAN_POINT ( 'NONE',  ( -35.00000000000000000, 0.000000000000000000, 0.000000000000000000 ) ) ;
#53273 = EDGE_LOOP ( 'NONE', ( #3789, #7932, #12659, #57635 ) ) ;
#53274 = CARTESIAN_POINT ( 'NONE',  ( 5.515539859299206427, -0.004509673239148459349, 0.004037661319611352689 ) ) ;
#53275 = AXIS2_PLACEMENT_3D ( 'NONE', #37440, #37774, #54057 ) ;
#53276 = EDGE_CURVE ( 'NONE', #1074, #31673, #23721, .T. ) ;
#53277 = AXIS2_PLACEMENT_3D ( 'NONE', #47632, #62916, #8716 ) ;
#53278 = CIRCLE ( 'NONE', #55397, 2.899999999999994582 ) ;
#53279 = B_SPLINE_CURVE_WITH_KNOTS ( 'NONE', 3,
 ( #63151, #23917, #21704, #23243, #17617, #12937, #46967, #54496, #1423, #7628, #27910, #43504, #43186, #28238, #28553, #37880 ),
 .UNSPECIFIED., .F., .F.,
 ( 4, 3, 3, 3, 3, 4 ),
 ( 2.266899309950898873E-15, 0.0002126834539179782880, 0.0004253519300366448929, 0.0006380165497224444702, 0.0007442707582428578252, 0.0009453531351416036505 ),
 .UNSPECIFIED. ) ;
#53280 = CARTESIAN_POINT ( 'NONE',  ( 2.573738926104376823, -7.583190312075752892, -1.575954828885333114 ) ) ;
#53281 = VECTOR ( 'NONE', #10436, 1000.000000000000000 ) ;
#53282 = CARTESIAN_POINT ( 'NONE',  ( 21.94459801178244618, 13.23030893428817123, -2.711026448255508647 ) ) ;
#53283 = CARTESIAN_POINT ( 'NONE',  ( 0.3040950598368152291, -1.881452845810457353, 12.11647736519420171 ) ) ;
#53284 = CARTESIAN_POINT ( 'NONE',  ( 0.9232058338315048962, 9.791640253608255406, -7.723624854284617314 ) ) ;
#53285 = DIRECTION ( 'NONE',  ( -1.000000000000000000, 0.000000000000000000, 0.000000000000000000 ) ) ;
#53286 = CARTESIAN_POINT ( 'NONE',  ( -22.29770266787582145, -2.703976473263631775, -2.588315884842665504 ) ) ;
#53287 = CIRCLE ( 'NONE', #3423, 12.75000000000000178 ) ;
#53288 = EDGE_CURVE ( 'NONE', #22284, #46041, #49172, .T. ) ;
#53289 = ORIENTED_EDGE ( 'NONE', *, *, #46835, .T. ) ;
#53290 = CARTESIAN_POINT ( 'NONE',  ( 12.63125402411999154, -9.907883201068845125, -6.772782016156807749 ) ) ;
#53291 = VECTOR ( 'NONE', #6556, 1000.000000000000000 ) ;
#53292 = VERTEX_POINT ( 'NONE', #7182 ) ;
#53293 = DIRECTION ( 'NONE',  ( 0.9996161839461982224, 0.02770351589312032917, -0.000000000000000000 ) ) ;
#53294 = EDGE_CURVE ( 'NONE', #29586, #57905, #34284, .T. ) ;
#53295 = CARTESIAN_POINT ( 'NONE',  ( -22.31328051695926007, 3.781397440874590732, -0.2528478350593763024 ) ) ;
#53296 = CARTESIAN_POINT ( 'NONE',  ( 0.8375941296815435644, -9.275620596396473516, -8.285008510335705623 ) ) ;
#53297 = VERTEX_POINT ( 'NONE', #47762 ) ;
#53298 = VECTOR ( 'NONE', #38149, 1000.000000000000000 ) ;
#53299 = DIRECTION ( 'NONE',  ( 1.000000000000000000, -0.000000000000000000, 0.000000000000000000 ) ) ;
#53300 = ADVANCED_FACE ( 'NONE', ( #2215 ), #22489, .T. ) ;
#53301 = ORIENTED_EDGE ( 'NONE', *, *, #37458, .T. ) ;
#53302 = DIRECTION ( 'NONE',  ( -1.000000000000000000, -1.836970198721029688E-16, -0.000000000000000000 ) ) ;
#53303 = EDGE_LOOP ( 'NONE', ( #50618, #59288, #65157, #6087 ) ) ;
#53304 = ORIENTED_EDGE ( 'NONE', *, *, #47230, .F. ) ;
#53305 = CARTESIAN_POINT ( 'NONE',  ( -10.60768675312085385, -9.408818418401033057, -7.467076076499517434 ) ) ;
#53306 = CIRCLE ( 'NONE', #21450, 3.999999999999999556 ) ;
#53307 = CARTESIAN_POINT ( 'NONE',  ( 2.251152103363644574, -7.133254101175206863, 2.729599998984383991 ) ) ;
#53308 = AXIS2_PLACEMENT_3D ( 'NONE', #27234, #21609, #57513 ) ;
#53309 = AXIS2_PLACEMENT_3D ( 'NONE', #33969, #54281, #32640 ) ;
#53310 = EDGE_CURVE ( 'NONE', #6736, #19313, #28981, .T. ) ;
#53311 = EDGE_LOOP ( 'NONE', ( #5299, #3353, #9540, #64783 ) ) ;
#53312 = FACE_OUTER_BOUND ( 'NONE', #58150, .T. ) ;
#53313 = CARTESIAN_POINT ( 'NONE',  ( 3.924654796536142243, 7.659842019319547113, 11.15136974237303669 ) ) ;
#53314 = CARTESIAN_POINT ( 'NONE',  ( -37.00000000000000711, 7.215058775251399936, -9.821084925794492548 ) ) ;
#53315 = CYLINDRICAL_SURFACE ( 'NONE', #362, 2.899999999999994582 ) ;
#53316 = ORIENTED_EDGE ( 'NONE', *, *, #19483, .T. ) ;
#53317 = CARTESIAN_POINT ( 'NONE',  ( 0.2801149460245112022, -7.723514566794048797, 9.509848747524161539 ) ) ;
#53318 = EDGE_CURVE ( 'NONE', #30510, #44234, #51309, .T. ) ;
#53319 = CARTESIAN_POINT ( 'NONE',  ( 15.64085769076060295, -34.91570230176446898, 5.822163132929507157 ) ) ;
#53320 = CARTESIAN_POINT ( 'NONE',  ( -29.66395171513434548, -2.175773247908486141, -11.80721667090971749 ) ) ;
#53322 = ORIENTED_EDGE ( 'NONE', *, *, #60930, .F. ) ;
#53321 = CARTESIAN_POINT ( 'NONE',  ( -10.00000000000000178, 0.000000000000000000, 0.000000000000000000 ) ) ;
#53323 = CARTESIAN_POINT ( 'NONE',  ( -27.75148563095054044, 11.73923255623741824, -2.552824637849768763 ) ) ;
#53324 = ORIENTED_EDGE ( 'NONE', *, *, #6729, .F. ) ;
#53325 = CARTESIAN_POINT ( 'NONE',  ( -17.54726996257253191, 12.93490414535030020, 3.865003848717349033 ) ) ;
#53326 = ORIENTED_EDGE ( 'NONE', *, *, #13311, .F. ) ;
#53327 = CARTESIAN_POINT ( 'NONE',  ( 36.00000000000000711, -11.24036214326524608, -6.018036132182126963 ) ) ;
#53328 = CIRCLE ( 'NONE', #44804, 2.899999999999995026 ) ;
#53329 = FACE_OUTER_BOUND ( 'NONE', #10314, .T. ) ;
#53330 = FACE_OUTER_BOUND ( 'NONE', #51377, .T. ) ;
#53331 = CARTESIAN_POINT ( 'NONE',  ( -2.672122885467083986, 11.33640012973147293, 3.936387307894332110 ) ) ;
#53332 = DIRECTION ( 'NONE',  ( -0.5551681190699946367, -0.8317381556525372810, 0.000000000000000000 ) ) ;
#53333 = CARTESIAN_POINT ( 'NONE',  ( 37.00000000000000711, 4.705694406421931860E-17, -3.469127814946512892E-15 ) ) ;
#53334 = CARTESIAN_POINT ( 'NONE',  ( -22.28169757117798966, -3.576542310004382941, -0.9284931499057510473 ) ) ;
#53336 = EDGE_CURVE ( 'NONE', #46419, #29012, #18867, .T. ) ;
#53335 = AXIS2_PLACEMENT_3D ( 'NONE', #30678, #61280, #47320 ) ;
#53337 = ORIENTED_EDGE ( 'NONE', *, *, #13505, .T. ) ;
#53338 = DIRECTION ( 'NONE',  ( -1.000000000000000000, 0.000000000000000000, 0.000000000000000000 ) ) ;
#53339 = ORIENTED_EDGE ( 'NONE', *, *, #17276, .F. ) ;
#53340 = AXIS2_PLACEMENT_3D ( 'NONE', #63518, #53896, #33277 ) ;
#53341 = EDGE_CURVE ( 'NONE', #17810, #26482, #32136, .T. ) ;
#53342 = ORIENTED_EDGE ( 'NONE', *, *, #21143, .F. ) ;
#53343 = DIRECTION ( 'NONE',  ( 0.000000000000000000, -0.9796553971857763221, -0.2006870767258792099 ) ) ;
#53344 = DIRECTION ( 'NONE',  ( 0.000000000000000000, 0.01356324068817998940, -0.9999080150203989437 ) ) ;
#53345 = FACE_OUTER_BOUND ( 'NONE', #12900, .T. ) ;
#53346 = CARTESIAN_POINT ( 'NONE',  ( -22.28415773361649954, 0.9981933716385181787, 3.565377603762363012 ) ) ;
#53347 = DIRECTION ( 'NONE',  ( -1.000000000000000000, -0.000000000000000000, -0.000000000000000000 ) ) ;
#53348 = CARTESIAN_POINT ( 'NONE',  ( -37.00000000000000711, -10.91536515067645041, -4.339012074900068683 ) ) ;
#53349 = LINE ( 'NONE', #28716, #20662 ) ;
#53350 = CIRCLE ( 'NONE', #3484, 2.899999999999996358 ) ;
#53351 = ORIENTED_EDGE ( 'NONE', *, *, #58536, .T. ) ;
#53352 = DIRECTION ( 'NONE',  ( -1.000000000000000000, 0.000000000000000000, 0.000000000000000000 ) ) ;
#53353 = CARTESIAN_POINT ( 'NONE',  ( -35.04683013664716640, -0.01216443238270097441, -0.002177781393209239635 ) ) ;
#53354 = AXIS2_PLACEMENT_3D ( 'NONE', #35459, #60087, #51103 ) ;
#53355 = CIRCLE ( 'NONE', #21504, 5.000000000000000888 ) ;
#53356 = ADVANCED_FACE ( 'NONE', ( #5410 ), #30467, .F. ) ;
#53357 = DIRECTION ( 'NONE',  ( 0.000000000000000000, 0.000000000000000000, 1.000000000000000000 ) ) ;
#53358 = DIRECTION ( 'NONE',  ( -1.000000000000000000, 0.000000000000000000, 0.000000000000000000 ) ) ;
#53359 = CIRCLE ( 'NONE', #24677, 5.000000000000000000 ) ;
#53360 = CARTESIAN_POINT ( 'NONE',  ( 0.2653519991613843554, 12.06397323649778563, -2.104847849998736642 ) ) ;
#53361 = CARTESIAN_POINT ( 'NONE',  ( 37.00000000000000711, -2.527899948230726057, -12.49688848680883346 ) ) ;
#53362 = ORIENTED_EDGE ( 'NONE', *, *, #16533, .T. ) ;
#53363 = DIRECTION ( 'NONE',  ( 0.000000000000000000, 0.01356324068817998940, -0.9999080150203990547 ) ) ;
#53364 = DIRECTION ( 'NONE',  ( 0.000000000000000000, -0.01356324068817999114, 0.9999080150203989437 ) ) ;
#53365 = CARTESIAN_POINT ( 'NONE',  ( 0.3665391374699465965, -8.095513416941168217, -9.237363111276849281 ) ) ;
#53366 = EDGE_CURVE ( 'NONE', #64499, #22968, #45628, .T. ) ;
#53367 = CARTESIAN_POINT ( 'NONE',  ( 6.824632601702067980, -31.95616727127245582, 13.35541573562488438 ) ) ;
#53368 = AXIS2_PLACEMENT_3D ( 'NONE', #53141, #43148, #63426 ) ;
#53369 = AXIS2_PLACEMENT_3D ( 'NONE', #24486, #3905, #24162 ) ;
#53370 = EDGE_CURVE ( 'NONE', #18752, #38246, #15682, .T. ) ;
#53371 = FACE_OUTER_BOUND ( 'NONE', #36175, .T. ) ;
#53372 = CARTESIAN_POINT ( 'NONE',  ( -25.21046028333935496, -11.50704267535209269, 7.061154338470299940 ) ) ;
#53373 = AXIS2_PLACEMENT_3D ( 'NONE', #49564, #34244, #39227 ) ;
#53374 = ORIENTED_EDGE ( 'NONE', *, *, #38275, .F. ) ;
#53375 = CARTESIAN_POINT ( 'NONE',  ( 35.00000000000000000, -8.366449238204431538, -9.621072037176965353 ) ) ;
#53376 = CARTESIAN_POINT ( 'NONE',  ( 0.3040950598368144520, -10.74226959800795811, 5.912066680610576164 ) ) ;
#53377 = CARTESIAN_POINT ( 'NONE',  ( 2.245754705088262249, -4.822435078157992550, -5.920355780194852535 ) ) ;
#53378 = DIRECTION ( 'NONE',  ( -1.000000000000000000, 0.000000000000000000, 0.000000000000000000 ) ) ;
#53379 = ORIENTED_EDGE ( 'NONE', *, *, #32131, .T. ) ;
#53380 = FACE_OUTER_BOUND ( 'NONE', #31845, .T. ) ;
#53381 = CARTESIAN_POINT ( 'NONE',  ( 0.2851083653049504285, -0.4107471485392698018, 25.00000000000000000 ) ) ;
#53382 = EDGE_CURVE ( 'NONE', #37253, #33968, #21004, .T. ) ;
#53383 = ORIENTED_EDGE ( 'NONE', *, *, #35018, .T. ) ;
#53384 = ORIENTED_EDGE ( 'NONE', *, *, #10252, .F. ) ;
#53385 = DIRECTION ( 'NONE',  ( 0.000000000000000000, 0.6745969609292609137, 0.7381862504172000961 ) ) ;
#53386 = ORIENTED_EDGE ( 'NONE', *, *, #19065, .T. ) ;
#53387 = DIRECTION ( 'NONE',  ( -1.000000000000000000, 0.000000000000000000, -0.000000000000000000 ) ) ;
#53388 = CYLINDRICAL_SURFACE ( 'NONE', #25106, 5.000000000000000888 ) ;
#53389 = CARTESIAN_POINT ( 'NONE',  ( -35.00000000000000000, -1.791059740004510070, 12.05416472667165273 ) ) ;
#53390 = LINE ( 'NONE', #39382, #37236 ) ;
#53391 = DIRECTION ( 'NONE',  ( 0.000000000000000000, -0.8696919319575130425, -0.4935949184179355131 ) ) ;
#53392 = EDGE_CURVE ( 'NONE', #50038, #49437, #13796, .T. ) ;
#53393 = DIRECTION ( 'NONE',  ( -1.000000000000000000, 0.000000000000000000, 0.000000000000000000 ) ) ;
#53395 = VERTEX_POINT ( 'NONE', #31330 ) ;
#53394 = DIRECTION ( 'NONE',  ( 1.000000000000000000, 0.000000000000000000, -0.000000000000000000 ) ) ;
#53396 = CARTESIAN_POINT ( 'NONE',  ( -22.27706485742869091, 2.580541389029920030, 2.625261754997667119 ) ) ;
#53397 = EDGE_CURVE ( 'NONE', #25053, #26284, #27933, .T. ) ;
#53398 = ORIENTED_EDGE ( 'NONE', *, *, #40682, .F. ) ;
#53399 = AXIS2_PLACEMENT_3D ( 'NONE', #54992, #14096, #20407 ) ;
#53400 = DIRECTION ( 'NONE',  ( 0.000000000000000000, -0.1387779952735679057, 0.9903235168508568442 ) ) ;
#53401 = ORIENTED_EDGE ( 'NONE', *, *, #26617, .F. ) ;
#53402 = CIRCLE ( 'NONE', #5616, 5.000000000000000888 ) ;
#53403 = VERTEX_POINT ( 'NONE', #10703 ) ;
#53404 = SHAPE_DEFINITION_REPRESENTATION ( #23801, #13953 ) ;
#53405 = CARTESIAN_POINT ( 'NONE',  ( -24.80814996009129203, 10.56471359980137592, 8.406295728485659424 ) ) ;
#53406 = ADVANCED_FACE ( 'NONE', ( #45309 ), #20040, .T. ) ;
#53407 = CARTESIAN_POINT ( 'NONE',  ( -11.13812830828974043, -32.61426855637455446, 12.21782902109530866 ) ) ;
#53409 = CARTESIAN_POINT ( 'NONE',  ( -24.47664113409060604, 11.24033395140356184, 7.479490891548917553 ) ) ;
#53408 = CIRCLE ( 'NONE', #47051, 12.18650000000000055 ) ;
#53410 = VECTOR ( 'NONE', #8390, 1000.000000000000000 ) ;
#53411 = CARTESIAN_POINT ( 'NONE',  ( 1.719304012338199517, 0.000000000000000000, 0.000000000000000000 ) ) ;
#53412 = CARTESIAN_POINT ( 'NONE',  ( -46.86486279825822265, -0.6193039491651883832, -9.927184253397708602 ) ) ;
#53413 = EDGE_CURVE ( 'NONE', #16590, #40228, #59373, .T. ) ;
#53414 = CARTESIAN_POINT ( 'NONE',  ( -36.00000000000000711, 12.57916205664481346, 2.080187960898606470 ) ) ;
#53415 = ORIENTED_EDGE ( 'NONE', *, *, #26785, .T. ) ;
#53416 =( BOUNDED_SURFACE ( )  B_SPLINE_SURFACE ( 3, 1, ( 
 ( #51573, #6022 ),
 ( #32236, #26277 ),
 ( #16951, #27255 ),
 ( #46555, #57532 ) ),
 .UNSPECIFIED., .F., .F., .F. ) 
 B_SPLINE_SURFACE_WITH_KNOTS ( ( 4, 4 ),
 ( 2, 2 ),
 ( 0.000000000000000000, 1.000000000000000000 ),
 ( 0.000000000000000000, 1.000000000000000000 ),
 .UNSPECIFIED. ) 
 GEOMETRIC_REPRESENTATION_ITEM ( )  RATIONAL_B_SPLINE_SURFACE ( (
 ( 1.000000000000000000, 1.000000000000000000),
 ( 0.9942764183789327692, 0.8450855930916580938),
 ( 0.9942764183789327692, 0.8450855930916580938),
 ( 1.000000000000000000, 1.000000000000000000) ) ) 
 REPRESENTATION_ITEM ( '' )  SURFACE ( )  );
#53417 = FACE_OUTER_BOUND ( 'NONE', #21977, .T. ) ;
#53418 = DIRECTION ( 'NONE',  ( 0.000000000000000000, 0.000000000000000000, 1.000000000000000000 ) ) ;
#53420 = ORIENTED_EDGE ( 'NONE', *, *, #10070, .F. ) ;
#53419 = CARTESIAN_POINT ( 'NONE',  ( 1.633930747252546167, -12.16309769563645915, -3.662223193115497377 ) ) ;
#53421 = ORIENTED_EDGE ( 'NONE', *, *, #42113, .T. ) ;
#53422 = EDGE_CURVE ( 'NONE', #13725, #55868, #25794, .T. ) ;
#53423 = DIRECTION ( 'NONE',  ( -1.000000000000000000, 0.000000000000000000, -0.000000000000000000 ) ) ;
#53424 = VERTEX_POINT ( 'NONE', #10065 ) ;
#53425 = AXIS2_PLACEMENT_3D ( 'NONE', #59910, #34609, #25294 ) ;
#53426 = FACE_OUTER_BOUND ( 'NONE', #40725, .T. ) ;
#53427 = CARTESIAN_POINT ( 'NONE',  ( -37.00000000000000711, -7.561043153947899498, -9.557269938331636183 ) ) ;
#53428 = CYLINDRICAL_SURFACE ( 'NONE', #22534, 2.899999999999994582 ) ;
#53429 = CARTESIAN_POINT ( 'NONE',  ( -22.28629837673888048, 3.055064048018809153, -2.102970853432551301 ) ) ;
#53430 = VECTOR ( 'NONE', #56142, 1000.000000000000114 ) ;
#53431 = DIRECTION ( 'NONE',  ( -1.000000000000000000, 0.000000000000000000, 0.000000000000000000 ) ) ;
#53432 = CARTESIAN_POINT ( 'NONE',  ( 37.00000000000000711, 4.705694406421931860E-17, -3.469127814946512892E-15 ) ) ;
#53433 = CARTESIAN_POINT ( 'NONE',  ( 2.249013661412230025, 3.921976945965425454, -6.552953334857869905 ) ) ;
#53434 = EDGE_LOOP ( 'NONE', ( #51744, #26949, #57436, #12488 ) ) ;
#53435 = DIRECTION ( 'NONE',  ( 0.000000000000000000, 0.8827602140260332186, -0.4698238015817332580 ) ) ;
#53436 = ORIENTED_EDGE ( 'NONE', *, *, #45974, .F. ) ;
#53437 = VECTOR ( 'NONE', #16188, 1000.000000000000000 ) ;
#53438 = DIRECTION ( 'NONE',  ( 0.000000000000000000, 0.000000000000000000, 1.000000000000000000 ) ) ;
#53439 = CARTESIAN_POINT ( 'NONE',  ( 2.844750968615672004, -2.990088422897184905, -7.242618984642843039 ) ) ;
#53440 = LINE ( 'NONE', #8199, #7502 ) ;
#53441 = EDGE_CURVE ( 'NONE', #9429, #3201, #44919, .T. ) ;
#53442 = ORIENTED_EDGE ( 'NONE', *, *, #54524, .T. ) ;
#53443 = CARTESIAN_POINT ( 'NONE',  ( -27.09729107899852707, 0.1622107421537268002, 2.324833743198334357 ) ) ;
#53444 = ORIENTED_EDGE ( 'NONE', *, *, #2894, .T. ) ;
#53445 = CARTESIAN_POINT ( 'NONE',  ( 0.2915757698887302962, 7.711631695122966867, -9.524403232224781135 ) ) ;
#53446 = DIRECTION ( 'NONE',  ( 0.000000000000000000, -0.9246979985058763063, -0.3807014730195119601 ) ) ;
#53447 = CARTESIAN_POINT ( 'NONE',  ( 2.266490820343225021, 1.470039317404164603, 7.500072841116502964 ) ) ;
#53448 = CARTESIAN_POINT ( 'NONE',  ( 2.247206125382826603, 1.439877054338202900, -7.499376972323885227 ) ) ;
#53449 = VERTEX_POINT ( 'NONE', #51305 ) ;
#53450 = VECTOR ( 'NONE', #16249, 1000.000000000000000 ) ;
#53451 = CARTESIAN_POINT ( 'NONE',  ( 2.639814597422731168, 2.414168779979584567, 7.382549681340915271 ) ) ;
#53452 = CARTESIAN_POINT ( 'NONE',  ( -22.27719381268171261, -2.618044180756125439, 2.588413841766863843 ) ) ;
#53453 = ADVANCED_FACE ( 'NONE', ( #45976 ), #50963, .T. ) ;
#53454 = DIRECTION ( 'NONE',  ( -1.000000000000000000, 0.000000000000000000, 0.000000000000000000 ) ) ;
#53455 = CARTESIAN_POINT ( 'NONE',  ( -46.22120612461743860, -0.7415077656649122773, -13.24100464050678916 ) ) ;
#53456 = AXIS2_PLACEMENT_3D ( 'NONE', #28734, #58699, #63984 ) ;
#53457 = AXIS2_PLACEMENT_3D ( 'NONE', #58205, #47262, #27598 ) ;
#53458 = CARTESIAN_POINT ( 'NONE',  ( 3.031336079629237013, -3.582646412484526532, 7.038432939675882238 ) ) ;
#53459 = CARTESIAN_POINT ( 'NONE',  ( -36.00000000000000711, 1.908798535168378274, 12.60630747491664039 ) ) ;
#53460 = ORIENTED_EDGE ( 'NONE', *, *, #7894, .F. ) ;
#53461 = CARTESIAN_POINT ( 'NONE',  ( 37.00000000000000711, 4.705694406421931860E-17, -3.469127814946512892E-15 ) ) ;
#53462 = CARTESIAN_POINT ( 'NONE',  ( 0.2655924914740778742, 2.169924872618063105, 12.05257978623654402 ) ) ;
#53463 = CIRCLE ( 'NONE', #58792, 5.000000000000000888 ) ;
#53464 = CARTESIAN_POINT ( 'NONE',  ( 5.515539859299206427, 0.002251761459665927844, 0.005618668168217501833 ) ) ;
#53465 = ORIENTED_EDGE ( 'NONE', *, *, #65797, .F. ) ;
#53466 = CARTESIAN_POINT ( 'NONE',  ( -17.97127638550377782, 4.326068679718637178, -12.78996018384692590 ) ) ;
#53467 = FACE_OUTER_BOUND ( 'NONE', #38168, .T. ) ;
#53468 = CARTESIAN_POINT ( 'NONE',  ( -14.47334165536100059, 0.000000000000000000, -6.000000000000000888 ) ) ;
#53469 = EDGE_CURVE ( 'NONE', #57350, #1853, #12658, .T. ) ;
#53470 = AXIS2_PLACEMENT_3D ( 'NONE', #61855, #11964, #16316 ) ;
#53471 = CARTESIAN_POINT ( 'NONE',  ( -35.00000000000000000, 0.3025107581132838175, -11.74226168163341377 ) ) ;
#53472 = EDGE_CURVE ( 'NONE', #7657, #55501, #7036, .T. ) ;
#53473 = CARTESIAN_POINT ( 'NONE',  ( 0.2869720083484368911, -11.58405933820304234, 3.994435966590022424 ) ) ;
#53474 = AXIS2_PLACEMENT_3D ( 'NONE', #21223, #16247, #36531 ) ;
#53475 = VERTEX_POINT ( 'NONE', #52915 ) ;
#53476 = FACE_OUTER_BOUND ( 'NONE', #60272, .T. ) ;
#53477 = ORIENTED_EDGE ( 'NONE', *, *, #24483, .T. ) ;
#53478 = CARTESIAN_POINT ( 'NONE',  ( 5.520433897694421610, -0.01432141647227114754, -0.004666464468078277902 ) ) ;
#53480 = AXIS2_PLACEMENT_3D ( 'NONE', #60323, #46033, #65620 ) ;
#53479 = DIRECTION ( 'NONE',  ( 0.000000000000000000, -0.01356324068817998940, 0.9999080150203990547 ) ) ;
#53481 = CARTESIAN_POINT ( 'NONE',  ( 35.00000000000000000, -11.61976888909157246, -3.827969819614423841 ) ) ;
#53482 = DIRECTION ( 'NONE',  ( -1.000000000000000000, 0.000000000000000000, 0.000000000000000000 ) ) ;
#53483 = LINE ( 'NONE', #34481, #32214 ) ;
#53484 = AXIS2_PLACEMENT_3D ( 'NONE', #44554, #38940, #4021 ) ;
#53485 = CARTESIAN_POINT ( 'NONE',  ( 2.284126774969136076, 5.756079777200249659, 5.036818232553848418 ) ) ;
#53486 = FACE_OUTER_BOUND ( 'NONE', #21311, .T. ) ;
#53487 = ORIENTED_EDGE ( 'NONE', *, *, #22925, .T. ) ;
#53488 = VERTEX_POINT ( 'NONE', #62233 ) ;
#53489 = DIRECTION ( 'NONE',  ( -1.000000000000000000, 0.000000000000000000, 0.000000000000000000 ) ) ;
#53490 = ORIENTED_EDGE ( 'NONE', *, *, #41921, .T. ) ;
#53491 = EDGE_CURVE ( 'NONE', #17535, #39390, #1412, .T. ) ;
#53492 = CARTESIAN_POINT ( 'NONE',  ( 1.719304012338836563, -3.626341562670527985, 12.20344780066003487 ) ) ;
#53493 = LINE ( 'NONE', #12904, #27951 ) ;
#53494 = VECTOR ( 'NONE', #2643, 1000.000000000000000 ) ;
#53495 = EDGE_CURVE ( 'NONE', #26254, #22685, #57658, .T. ) ;
#53496 = DIRECTION ( 'NONE',  ( -1.000000000000000000, 0.000000000000000000, -0.000000000000000000 ) ) ;
#53497 = ORIENTED_EDGE ( 'NONE', *, *, #5702, .T. ) ;
#53498 = CARTESIAN_POINT ( 'NONE',  ( -35.04660725145885891, 0.009947898977325340605, -0.007231372203147071014 ) ) ;
#53499 = CARTESIAN_POINT ( 'NONE',  ( 2.507146904658099196, 1.553587269793159642, -7.565123178000298765 ) ) ;
#53500 = DIRECTION ( 'NONE',  ( -1.000000000000000000, 0.000000000000000000, 0.000000000000000000 ) ) ;
#53501 = VERTEX_POINT ( 'NONE', #27984 ) ;
#53502 = ORIENTED_EDGE ( 'NONE', *, *, #12662, .F. ) ;
#53503 = EDGE_CURVE ( 'NONE', #15336, #49701, #31961, .T. ) ;
#53504 = CARTESIAN_POINT ( 'NONE',  ( 37.00000000000000711, -9.493370459201747380, -6.917234959366797220 ) ) ;
#53505 = ORIENTED_EDGE ( 'NONE', *, *, #2861, .F. ) ;
#53507 = CYLINDRICAL_SURFACE ( 'NONE', #59909, 13.50000000000000178 ) ;
#53506 = CIRCLE ( 'NONE', #54544, 12.74999999999999822 ) ;
#53508 = AXIS2_PLACEMENT_3D ( 'NONE', #39738, #40370, #56331 ) ;
#53509 = ORIENTED_EDGE ( 'NONE', *, *, #56022, .F. ) ;
#53510 = VERTEX_POINT ( 'NONE', #32942 ) ;
#53511 = CARTESIAN_POINT ( 'NONE',  ( 35.00000000000000000, 4.705694406421931860E-17, -3.469127814946512892E-15 ) ) ;
#53512 = CARTESIAN_POINT ( 'NONE',  ( -27.09229696323388126, -1.607344345646396278, 1.666734935102338833 ) ) ;
#53513 = CIRCLE ( 'NONE', #34358, 6.936499999999989896 ) ;
#53514 = CARTESIAN_POINT ( 'NONE',  ( -35.00000000000000000, -4.986700593229626222, -10.63508530065527147 ) ) ;
#53515 = CARTESIAN_POINT ( 'NONE',  ( 0.3053067050349185796, 8.055646999028132527, -9.241336250185277379 ) ) ;
#53516 = DIRECTION ( 'NONE',  ( -1.000000000000000000, 0.000000000000000000, -0.000000000000000000 ) ) ;
#53517 = EDGE_CURVE ( 'NONE', #13636, #24509, #26998, .T. ) ;
#53518 = CARTESIAN_POINT ( 'NONE',  ( 2.350038591458112780, 6.324706260080001030, 8.533611140765424707 ) ) ;
#53519 = ORIENTED_EDGE ( 'NONE', *, *, #4053, .F. ) ;
#53520 = VECTOR ( 'NONE', #58442, 1000.000000000000000 ) ;
#53521 = DIRECTION ( 'NONE',  ( 0.000000000000000000, -0.01356324068817998940, 0.9999080150203990547 ) ) ;
#53523 = CARTESIAN_POINT ( 'NONE',  ( 3.100650473569697585, 4.737096019059274354, 6.348250400753886247 ) ) ;
#53522 = AXIS2_PLACEMENT_3D ( 'NONE', #26275, #61505, #52216 ) ;
#53524 = CARTESIAN_POINT ( 'NONE',  ( 2.251152103364156609, 3.709836606812680682, -6.676162264141248137 ) ) ;
#53525 = CARTESIAN_POINT ( 'NONE',  ( -35.04834644901396956, -0.01211993185718040697, -0.006670072992065173914 ) ) ;
#53526 = DIRECTION ( 'NONE',  ( 0.000000000000000000, -1.000000000000000000, 0.000000000000000000 ) ) ;
#53527 = AXIS2_PLACEMENT_3D ( 'NONE', #46308, #21007, #61914 ) ;
#53528 = CARTESIAN_POINT ( 'NONE',  ( -35.00000000000000000, 10.14408668126213442, 5.921969905510389154 ) ) ;
#53529 = CARTESIAN_POINT ( 'NONE',  ( 2.305787727787084407, -0.1666591538753222634, 7.654065630109506024 ) ) ;
#53530 = CARTESIAN_POINT ( 'NONE',  ( -7.181456785175555524, 25.00000000000000000, -10.45493698471458188 ) ) ;
#53531 = CIRCLE ( 'NONE', #33328, 12.74999999999999822 ) ;
#53532 = ORIENTED_EDGE ( 'NONE', *, *, #20528, .F. ) ;
#53533 = CYLINDRICAL_SURFACE ( 'NONE', #13146, 4.999999999999999112 ) ;
#53534 = ADVANCED_FACE ( 'NONE', ( #47604 ), #58764, .T. ) ;
#53535 = ORIENTED_EDGE ( 'NONE', *, *, #27381, .T. ) ;
#53536 = DIRECTION ( 'NONE',  ( 1.000000000000000000, 0.000000000000000000, 0.000000000000000000 ) ) ;
#53537 = CARTESIAN_POINT ( 'NONE',  ( 0.3537226245948373315, -0.2609894354290372975, 12.27287980220284602 ) ) ;
#53538 = AXIS2_PLACEMENT_3D ( 'NONE', #18260, #33848, #33207 ) ;
#53539 = CARTESIAN_POINT ( 'NONE',  ( 3.152665057734036491, 7.923639299009025194, 0.4801242025592407647 ) ) ;
#53540 = CARTESIAN_POINT ( 'NONE',  ( -10.90165637462999904, -7.508992741355384304, 11.21895841913464587 ) ) ;
#53541 = CARTESIAN_POINT ( 'NONE',  ( 2.931247277082684288, -4.765826751677395556, -6.255823895767015586 ) ) ;
#53542 = ORIENTED_EDGE ( 'NONE', *, *, #12043, .T. ) ;
#53543 = CARTESIAN_POINT ( 'NONE',  ( 0.000000000000000000, 6.767909380267608022, -0.7805499053121014441 ) ) ;
#53544 = CARTESIAN_POINT ( 'NONE',  ( -37.00000000000000711, 7.376655759825023750, -9.700295462048581285 ) ) ;
#53545 = EDGE_CURVE ( 'NONE', #46888, #7394, #37464, .T. ) ;
#53546 = CARTESIAN_POINT ( 'NONE',  ( -18.11311222685468891, -13.11907746847522205, 3.257880281090000718 ) ) ;
#53547 = CARTESIAN_POINT ( 'NONE',  ( 1.836544102188037542, -30.58412608844215796, -15.25442441212476652 ) ) ;
#53548 = CIRCLE ( 'NONE', #3671, 6.936499999999989896 ) ;
#53549 = CYLINDRICAL_SURFACE ( 'NONE', #32910, 7.499999999999988454 ) ;
#53550 = VERTEX_POINT ( 'NONE', #1733 ) ;
#53551 = CARTESIAN_POINT ( 'NONE',  ( 1.014383007554949589, -8.367379244277062256, -9.280879504741022856 ) ) ;
#53552 = ADVANCED_FACE ( 'NONE', ( #42582 ), #17684, .T. ) ;
#53553 = EDGE_CURVE ( 'NONE', #60601, #32845, #52612, .T. ) ;
#53554 = AXIS2_PLACEMENT_3D ( 'NONE', #46562, #59120, #64397 ) ;
#53555 = EDGE_CURVE ( 'NONE', #16089, #12285, #62884, .T. ) ;
#53556 = ORIENTED_EDGE ( 'NONE', *, *, #11035, .F. ) ;
#53557 = DIRECTION ( 'NONE',  ( -1.000000000000000000, 0.000000000000000000, 0.000000000000000000 ) ) ;
#53558 = ORIENTED_EDGE ( 'NONE', *, *, #28053, .F. ) ;
#53559 = CARTESIAN_POINT ( 'NONE',  ( -35.00000000000000000, 1.591260454995410578, -12.08216339958899077 ) ) ;
#53560 = CARTESIAN_POINT ( 'NONE',  ( 3.100650473569578569, -3.562766772868545484, -7.074394303868158040 ) ) ;
#53561 = DIRECTION ( 'NONE',  ( 0.000000000000000000, 0.01356324068817998940, -0.9999080150203990547 ) ) ;
#53562 = CARTESIAN_POINT ( 'NONE',  ( 5.536195898058073439, -0.0002547682446684437600, -0.008496323383586771791 ) ) ;
#53563 = CARTESIAN_POINT ( 'NONE',  ( -22.28506771379528573, -2.081613609299067580, -3.091577134491938050 ) ) ;
#53564 = ORIENTED_EDGE ( 'NONE', *, *, #56528, .F. ) ;
#53566 = VERTEX_POINT ( 'NONE', #22671 ) ;
#53565 = B_SPLINE_CURVE_WITH_KNOTS ( 'NONE', 3,
 ( #41996, #2097, #47343, #57649, #11729, #21054, #12066, #22368, #56668, #1121, #36362, #15731, #36011, #21402, #36689, #56309 ),
 .UNSPECIFIED., .F., .F.,
 ( 4, 3, 3, 3, 3, 4 ),
 ( 0.000000000000000000, 6.991367980366407805E-05, 0.0001398269368981363962, 0.0002097400188389097965, 0.0002811534801551364318, 0.0003526297678872492578 ),
 .UNSPECIFIED. ) ;
#53567 = ORIENTED_EDGE ( 'NONE', *, *, #22612, .T. ) ;
#53568 = CARTESIAN_POINT ( 'NONE',  ( 2.258463476536645143, 7.224688073723641857, -2.484972401833173805 ) ) ;
#53569 = EDGE_CURVE ( 'NONE', #7570, #49200, #30050, .T. ) ;
#53570 = AXIS2_PLACEMENT_3D ( 'NONE', #34635, #49952, #24681 ) ;
#53571 = DIRECTION ( 'NONE',  ( 0.000000000000000000, 0.01356324068817998940, -0.9999080150203990547 ) ) ;
#53572 = ORIENTED_EDGE ( 'NONE', *, *, #46854, .T. ) ;
#53573 = FACE_OUTER_BOUND ( 'NONE', #55299, .T. ) ;
#53574 = CARTESIAN_POINT ( 'NONE',  ( 2.262775599886257982, -7.548684916004836154, 1.187656132455246150 ) ) ;
#53575 = ORIENTED_EDGE ( 'NONE', *, *, #1058, .F. ) ;
#53576 = CARTESIAN_POINT ( 'NONE',  ( -24.42101984568203932, 2.451666775035126644, -3.522366633939671310 ) ) ;
#53577 = CIRCLE ( 'NONE', #10031, 5.000000000000000000 ) ;
#53578 = CARTESIAN_POINT ( 'NONE',  ( 2.280717697723838366, -2.762096098144292800, -7.131299706077053990 ) ) ;
#53579 = CARTESIAN_POINT ( 'NONE',  ( 20.00005080000000035, 3.872983346207417021, -1.000000000000000000 ) ) ;
#53580 = ORIENTED_EDGE ( 'NONE', *, *, #42539, .F. ) ;
#53581 = VERTEX_POINT ( 'NONE', #57596 ) ;
#53582 = CARTESIAN_POINT ( 'NONE',  ( -1.734723475976807094E-15, -3.469446951953614189E-15, 12.00000000000000178 ) ) ;
#53583 = EDGE_LOOP ( 'NONE', ( #35463, #41659, #23001, #14693 ) ) ;
#53584 = FILL_AREA_STYLE_COLOUR ( '', #54036 ) ;
#53585 = ORIENTED_EDGE ( 'NONE', *, *, #23596, .T. ) ;
#53586 = VECTOR ( 'NONE', #42437, 1000.000000000000000 ) ;
#53587 = CARTESIAN_POINT ( 'NONE',  ( 2.827825597296797167, 7.250702617666076932, -5.372687261161209094 ) ) ;
#53588 = CARTESIAN_POINT ( 'NONE',  ( -35.00000000000000000, -11.59095880812009582, 1.903127969211145132 ) ) ;
#53589 = CARTESIAN_POINT ( 'NONE',  ( -22.27384469013076185, 0.9224151068931638608, 3.564715702084478632 ) ) ;
#53590 = AXIS2_PLACEMENT_3D ( 'NONE', #14865, #64761, #35153 ) ;
#53591 = LINE ( 'NONE', #28300, #49748 ) ;
#53592 = LINE ( 'NONE', #17996, #27680 ) ;
#53593 = CARTESIAN_POINT ( 'NONE',  ( -35.00000000000000000, 7.215058775251398160, -9.821084925794490772 ) ) ;
#53594 = CARTESIAN_POINT ( 'NONE',  ( 6.548939983325835712, -7.784018732717215450, -9.141476843261248320 ) ) ;
#53595 = ORIENTED_EDGE ( 'NONE', *, *, #4484, .F. ) ;
#53596 = CARTESIAN_POINT ( 'NONE',  ( 1.372161826075801505, 11.20801830616751893, 5.789954543171472956 ) ) ;
#53597 = ORIENTED_EDGE ( 'NONE', *, *, #5905, .F. ) ;
#53598 = CARTESIAN_POINT ( 'NONE',  ( 2.259830038564998311, -2.742210045659230211, 7.131511317046845377 ) ) ;
#53599 = DIRECTION ( 'NONE',  ( 0.000000000000000000, -0.01356324068817992175, 0.9999080150203990547 ) ) ;
#53600 = CIRCLE ( 'NONE', #36590, 12.18650000000000233 ) ;
#53601 = ORIENTED_EDGE ( 'NONE', *, *, #60332, .F. ) ;
#53603 = AXIS2_PLACEMENT_3D ( 'NONE', #9502, #34467, #40775 ) ;
#53602 = CARTESIAN_POINT ( 'NONE',  ( 5.515188684475870851, 0.005140903460551586937, 0.001485678338381530954 ) ) ;
#53604 = CARTESIAN_POINT ( 'NONE',  ( 0.3341166715381294616, 12.03629799686217972, -2.378838837788969762 ) ) ;
#53605 = CARTESIAN_POINT ( 'NONE',  ( 0.2671309869109482205, -2.286013846429945762, -12.03155065772887689 ) ) ;
#53606 = ORIENTED_EDGE ( 'NONE', *, *, #15066, .F. ) ;
#53607 = ORIENTED_EDGE ( 'NONE', *, *, #12940, .F. ) ;
#53608 = DIRECTION ( 'NONE',  ( -1.000000000000000000, -0.000000000000000000, 0.000000000000000000 ) ) ;
#53609 = EDGE_CURVE ( 'NONE', #24621, #30317, #8801, .T. ) ;
#53610 = ORIENTED_EDGE ( 'NONE', *, *, #3077, .T. ) ;
#53611 = CARTESIAN_POINT ( 'NONE',  ( -28.85619398320021745, 3.750539801530000439, 12.96855624952675612 ) ) ;
#53612 =( LENGTH_UNIT ( ) NAMED_UNIT ( * ) SI_UNIT ( .MILLI., .METRE. ) );
#53613 = CARTESIAN_POINT ( 'NONE',  ( 2.241536586108914264, -1.331908602351589144, -7.517390684805882906 ) ) ;
#53614 = CARTESIAN_POINT ( 'NONE',  ( 0.2648321136542700072, -9.289286523730366341, -7.979621084888208316 ) ) ;
#53615 = CARTESIAN_POINT ( 'NONE',  ( -17.65546883943164147, -7.074198755462914434, 9.697947387155558374 ) ) ;
#53616 = AXIS2_PLACEMENT_3D ( 'NONE', #29591, #9987, #61181 ) ;
#53617 = ORIENTED_EDGE ( 'NONE', *, *, #15079, .F. ) ;
#53618 = FACE_OUTER_BOUND ( 'NONE', #60572, .T. ) ;
#53619 = CIRCLE ( 'NONE', #13258, 2.899999999999994582 ) ;
#53620 = ADVANCED_FACE ( 'NONE', ( #37629 ), #57926, .T. ) ;
#53621 = CARTESIAN_POINT ( 'NONE',  ( 2.705197763288547108, -7.617149697727731095, -1.627208841526538663 ) ) ;
#53622 =( BOUNDED_SURFACE ( )  B_SPLINE_SURFACE ( 3, 1, ( 
 ( #36715, #62301 ),
 ( #7107, #47366 ),
 ( #17427, #6464 ),
 ( #57997, #48360 ) ),
 .UNSPECIFIED., .F., .F., .F. ) 
 B_SPLINE_SURFACE_WITH_KNOTS ( ( 4, 4 ),
 ( 2, 2 ),
 ( 0.000000000000000000, 1.000000000000000000 ),
 ( 0.000000000000000000, 1.000000000000000000 ),
 .UNSPECIFIED. ) 
 GEOMETRIC_REPRESENTATION_ITEM ( )  RATIONAL_B_SPLINE_SURFACE ( (
 ( 1.000000000000000000, 1.000000000000000000),
 ( 0.9942764183789327692, 0.8450855930916585379),
 ( 0.9942764183789327692, 0.8450855930916585379),
 ( 1.000000000000000000, 1.000000000000000000) ) ) 
 REPRESENTATION_ITEM ( '' )  SURFACE ( )  );
#53623 = CARTESIAN_POINT ( 'NONE',  ( 0.3665391374699467075, 4.447929964103001232, -11.44911061034382094 ) ) ;
#53624 = CARTESIAN_POINT ( 'NONE',  ( -27.08417568107324058, -0.8117865859100323878, 2.142502990753197611 ) ) ;
#53625 = CARTESIAN_POINT ( 'NONE',  ( 0.2653141617321028711, 7.837919552760726383, 9.409385893408531487 ) ) ;
#53626 = ADVANCED_FACE ( 'NONE', ( #21342 ), #55134, .F. ) ;
#53627 = CARTESIAN_POINT ( 'NONE',  ( 4.364872672758343342, -10.79984456430371864, -5.233809610475972818 ) ) ;
#53628 = CARTESIAN_POINT ( 'NONE',  ( -22.27706485742869091, -2.580541389029911148, -2.625261754997698205 ) ) ;
#53629 = AXIS2_PLACEMENT_3D ( 'NONE', #51646, #46973, #1750 ) ;
#53630 = VERTEX_POINT ( 'NONE', #28624 ) ;
#53631 = CARTESIAN_POINT ( 'NONE',  ( 12.86999076135267117, -11.06020008475422145, -4.659701079214955577 ) ) ;
#53632 = ORIENTED_EDGE ( 'NONE', *, *, #12744, .T. ) ;
#53633 = CARTESIAN_POINT ( 'NONE',  ( 0.3223008802179228027, 1.888629463821845489, -12.11889957318022404 ) ) ;
#53634 = CARTESIAN_POINT ( 'NONE',  ( -22.29479313954897890, 3.724550806388644109, -0.2707859422896706780 ) ) ;
#53635 = DIRECTION ( 'NONE',  ( -1.000000000000000000, 0.000000000000000000, 0.000000000000000000 ) ) ;
#53636 = EDGE_LOOP ( 'NONE', ( #3116, #56596, #64936, #29092 ) ) ;
#53637 = CARTESIAN_POINT ( 'NONE',  ( -35.00000000000000000, 11.32068061209295529, 5.865551165831117686 ) ) ;
#53638 = DIRECTION ( 'NONE',  ( 0.000000000000000000, -0.01356324068817991828, 0.9999080150203990547 ) ) ;
#53639 = ORIENTED_EDGE ( 'NONE', *, *, #26515, .T. ) ;
#53640 = CIRCLE ( 'NONE', #19655, 5.000000000000000000 ) ;
#53641 = ORIENTED_EDGE ( 'NONE', *, *, #14804, .T. ) ;
#53642 = ORIENTED_EDGE ( 'NONE', *, *, #379, .T. ) ;
#53643 = CARTESIAN_POINT ( 'NONE',  ( 0.2833330754217395220, -7.719627479384596036, -9.514385791198174402 ) ) ;
#53644 = CARTESIAN_POINT ( 'NONE',  ( 0.3401186441510245517, -12.03768714635923764, -2.382124782498485693 ) ) ;
#53645 = ORIENTED_EDGE ( 'NONE', *, *, #23658, .F. ) ;
#53646 = CARTESIAN_POINT ( 'NONE',  ( 35.00000000000000000, -4.018060380616318206, 11.50504120060946533 ) ) ;
#53647 = CARTESIAN_POINT ( 'NONE',  ( 2.665405856346676927, 9.549966053095770846, 0.5773576323838272017 ) ) ;
#53648 = DIRECTION ( 'NONE',  ( -1.000000000000000000, -0.000000000000000000, 0.000000000000000000 ) ) ;
#53649 = CARTESIAN_POINT ( 'NONE',  ( -37.00000000000000711, -5.015831474386382105, 10.62137734850266391 ) ) ;
#53650 = ORIENTED_EDGE ( 'NONE', *, *, #64184, .F. ) ;
#53651 = AXIS2_PLACEMENT_3D ( 'NONE', #61514, #56553, #21284 ) ;
#53652 = CARTESIAN_POINT ( 'NONE',  ( 0.2834382757447978518, -7.719209397492048375, 9.514772331577404429 ) ) ;
#53653 = DIRECTION ( 'NONE',  ( 0.000000000000000000, -0.01356324068817991828, 0.9999080150203990547 ) ) ;
#53654 = CYLINDRICAL_SURFACE ( 'NONE', #27109, 5.000000000000000888 ) ;
#53656 = ORIENTED_EDGE ( 'NONE', *, *, #4136, .F. ) ;
#53655 = CARTESIAN_POINT ( 'NONE',  ( -24.35981274529309815, 7.722558591804820516, 9.187561872115383110 ) ) ;
#53657 = CARTESIAN_POINT ( 'NONE',  ( 0.2646305136544065406, -12.08286001766536621, 1.996350543472954264 ) ) ;
#53658 = EDGE_LOOP ( 'NONE', ( #33679, #51320, #51894, #33423 ) ) ;
#53660 = EDGE_CURVE ( 'NONE', #31648, #51996, #55609, .T. ) ;
#53659 = DIRECTION ( 'NONE',  ( 0.000000000000000000, 0.5472293298355215274, -0.8369827122275381726 ) ) ;
#53661 = ORIENTED_EDGE ( 'NONE', *, *, #1605, .F. ) ;
#53662 = DIRECTION ( 'NONE',  ( -1.000000000000000000, 0.000000000000000000, -0.000000000000000000 ) ) ;
#53663 = DIRECTION ( 'NONE',  ( 0.000000000000000000, -0.01356324068817998940, 0.9999080150203990547 ) ) ;
#53664 = CIRCLE ( 'NONE', #24986, 5.000000000000000888 ) ;
#53665 = CARTESIAN_POINT ( 'NONE',  ( 47.00000000000000711, 4.705694406421931860E-17, -3.469127814946512892E-15 ) ) ;
#53666 = DIRECTION ( 'NONE',  ( 0.000000000000000000, -0.9718671068226485410, 0.2355298848897412756 ) ) ;
#53667 = EDGE_CURVE ( 'NONE', #31565, #51364, #41823, .T. ) ;
#53668 = CARTESIAN_POINT ( 'NONE',  ( 35.00000000000000000, 11.47758908105697806, 2.497432891016712286 ) ) ;
#53669 = CARTESIAN_POINT ( 'NONE',  ( -9.813495697803759299, -4.010685208788737022, -12.89544212305399462 ) ) ;
#53670 = CARTESIAN_POINT ( 'NONE',  ( -22.29570301036918423, -3.629130197778195122, -0.8918611685731365757 ) ) ;
#53671 = EDGE_LOOP ( 'NONE', ( #15835, #23291, #27637, #60561, #6577, #15606, #15347, #38300, #51199, #3693, #3054, #54417, #53610, #18250, #11033, #12950, #60153, #58280, #9988, #7685, #55141, #35304, #22978, #34512, #43026, #7276, #52305, #64907, #63750, #49856, #30630, #27925, #51668, #99, #7950, #17597, #952, #8095, #13602, #15105, #19377, #49002, #28417, #58685, #34699, #37460, #30143, #50016, #43391, #4501, #15132, #32022, #46491, #27388, #25307, #34980, #60069, #5902, #18406, #10051, #1866, #8231, #47024, #61702, #47719, #8479, #36473, #54902, #21070, #49483, #24875, #53673, #21050, #49145, #13255, #55437, #5487, #10600, #50740, #22177, #47730, #53497, #26675, #32924, #10151, #41553, #30031, #27413, #22514, #38498, #1912, #29885, #29945, #28383, #19297, #4675, #36844, #6354, #27916, #47895, #2781, #53873, #7946, #41524, #65227, #46855, #35022, #3516, #65000, #61969, #18462, #16921, #5129, #44489, #24440, #4749, #50550, #39570, #1152, #55709, #38620, #28812, #59898, #3659, #43088, #51772, #20943, #9975, #42214, #6598, #43564, #30226, #43134, #30392, #53386, #39623, #24607, #13382, #52999, #53071, #19948, #61152, #54661, #43858, #15220, #44544, #1219, #15687, #64888, #25921, #38932, #61225, #11987, #11832, #6206, #25892, #18893, #27634, #23654, #8320, #33267, #61359, #54716, #4592, #3692, #7195, #36673, #54981, #21665, #2196, #55045, #28949, #51552, #47210, #47787, #45310, #22213, #60001, #42581, #38472, #32369, #21886, #56301, #64250, #22290, #54204, #42969, #16728, #24827, #28966, #31969, #32343, #9215, #22072, #3133, #8173, #11515, #28274, #7650, #4745, #17135, #48104, #33135, #55376, #38754, #27213, #23224, #47683, #20231, #5697, #46124, #55645, #802, #42290, #63427, #61099, #40522, #41307, #3947, #56751, #17409, #29930, #5742, #15106, #20100, #8441, #4517, #36428, #17071, #37892, #21709, #55834, #12571, #6483, #33518, #50682, #49713, #10271, #30763, #60465, #16818, #7416, #13439, #41015, #16938, #33507, #14186, #6742, #19709, #13874, #48004, #24323, #33095, #47581, #46422, #41927, #11601, #5090, #19559, #1333, #14114, #18683, #56297, #18700, #26497, #19867, #23381, #20089, #22724, #17207, #55216, #4095, #30858, #18716, #6137, #27542, #62217, #20127, #50840, #8729, #8810, #61787, #49227, #28310, #12228, #10524, #62552, #59095, #37370, #59216, #50977, #6664, #37846, #43538, #30729, #57563, #60687, #9910, #6997, #20020, #64672, #13633, #32839, #35864, #1857, #50226, #48069, #53746, #14608, #54294, #55850, #8568, #39851, #28935, #41864, #52877, #1700, #37133, #47592, #22833, #54825, #49082, #63093, #4367, #6685, #4001, #29577, #8990, #20142, #27317, #48538, #43459, #26060, #38260, #8750, #42597, #56552, #55412, #9183, #21614, #31616, #46709, #30813, #54805, #65, #48678, #6565, #15256, #38058, #35851, #43016, #2116, #50625, #36217, #30909, #55824, #28977, #44694, #6096, #16081, #30069, #51057, #17028, #55706, #25413, #11472, #8588, #40043, #53490, #6280, #14074, #57507, #55321, #16435, #1996, #20671, #7674, #60944, #46688, #59325, #53572, #11540, #20574, #19552, #41291, #25651, #65470, #717, #13012, #2694, #17716, #61014, #46771, #52095, #37596, #53674, #13919, #31299, #22987, #46469, #30058, #15351, #12483, #7600, #5049 ) ) ;
#53672 = DIRECTION ( 'NONE',  ( 0.000000000000000000, 0.01356324068817998940, -0.9999080150203989437 ) ) ;
#53673 = ORIENTED_EDGE ( 'NONE', *, *, #7991, .T. ) ;
#53674 = ORIENTED_EDGE ( 'NONE', *, *, #15300, .T. ) ;
#53675 = CARTESIAN_POINT ( 'NONE',  ( 0.6473888112830243902, 1.823007254467119198, -12.23851338376146991 ) ) ;
#53676 = DIRECTION ( 'NONE',  ( 1.000000000000000000, 0.000000000000000000, 0.000000000000000000 ) ) ;
#53677 = CARTESIAN_POINT ( 'NONE',  ( 0.3665391374699465965, -2.392238720110376970, -12.04754782681759728 ) ) ;
#53678 = CARTESIAN_POINT ( 'NONE',  ( -22.27710395300133683, 0.9291085174899564869, 3.562137928983401203 ) ) ;
#53679 = CARTESIAN_POINT ( 'NONE',  ( 29.51976981715666781, 25.00000000000000000, 11.09513982864076276 ) ) ;
#53680 = DIRECTION ( 'NONE',  ( 1.000000000000000000, 0.000000000000000000, 0.000000000000000000 ) ) ;
#53681 = AXIS2_PLACEMENT_3D ( 'NONE', #54258, #38627, #58940 ) ;
#53682 = EDGE_CURVE ( 'NONE', #52961, #37153, #62994, .T. ) ;
#53683 = FACE_OUTER_BOUND ( 'NONE', #27514, .T. ) ;
#53684 = ADVANCED_FACE ( 'NONE', ( #43578 ), #33292, .T. ) ;
#53685 = ORIENTED_EDGE ( 'NONE', *, *, #29967, .F. ) ;
#53686 = CARTESIAN_POINT ( 'NONE',  ( 2.990245332647680332, -6.155689586375244104, -5.834301250882039547 ) ) ;
#53687 = DIRECTION ( 'NONE',  ( 0.000000000000000000, 0.9999080150203989437, 0.01356324068818348313 ) ) ;
#53688 = EDGE_CURVE ( 'NONE', #39957, #57971, #17352, .T. ) ;
#53689 = CARTESIAN_POINT ( 'NONE',  ( -35.00000000000000000, 0.000000000000000000, 0.000000000000000000 ) ) ;
#53690 = FACE_OUTER_BOUND ( 'NONE', #46005, .T. ) ;
#53691 = DIRECTION ( 'NONE',  ( 1.000000000000000000, -0.000000000000000000, 0.000000000000000000 ) ) ;
#53692 = ADVANCED_FACE ( 'NONE', ( #13649 ), #43253, .T. ) ;
#53693 = VECTOR ( 'NONE', #31107, 1000.000000000000000 ) ;
#53694 = CARTESIAN_POINT ( 'NONE',  ( 26.65194590272820108, -3.631858188236756657, -25.00000000000000711 ) ) ;
#53695 = EDGE_CURVE ( 'NONE', #8085, #31867, #53909, .T. ) ;
#53696 = CARTESIAN_POINT ( 'NONE',  ( 9.769972995331128729, 2.020868073575773138, -11.83009605721721158 ) ) ;
#53697 = ORIENTED_EDGE ( 'NONE', *, *, #60046, .T. ) ;
#53698 = CARTESIAN_POINT ( 'NONE',  ( 37.00000000000000711, 2.627174906297071733, 11.44858830469737221 ) ) ;
#53699 = LINE ( 'NONE', #13117, #47383 ) ;
#53700 = CYLINDRICAL_SURFACE ( 'NONE', #12041, 12.74999999999999822 ) ;
#53701 = VECTOR ( 'NONE', #50865, 1000.000000000000000 ) ;
#53702 = EDGE_CURVE ( 'NONE', #16286, #57171, #33296, .T. ) ;
#53703 = CARTESIAN_POINT ( 'NONE',  ( -35.00000000000000000, 1.488153103997124971, -11.65150730582933036 ) ) ;
#53704 = CARTESIAN_POINT ( 'NONE',  ( 35.00000000000000000, 12.31350058095522826, -3.307597835713290024 ) ) ;
#53705 = ORIENTED_EDGE ( 'NONE', *, *, #28219, .T. ) ;
#53706 = CARTESIAN_POINT ( 'NONE',  ( -18.08686583997218733, 5.151216734910788908, 12.47858029384653733 ) ) ;
#53707 = CARTESIAN_POINT ( 'NONE',  ( 2.251139882113691648, -4.813633939919740534, -5.929826121558939178 ) ) ;
#53708 = CARTESIAN_POINT ( 'NONE',  ( 35.00000000000000000, -11.86701198550353986, 2.772148766916240348 ) ) ;
#53709 = ORIENTED_EDGE ( 'NONE', *, *, #38405, .T. ) ;
#53710 = B_SPLINE_CURVE_WITH_KNOTS ( 'NONE', 3,
 ( #22034, #42288, #17390, #17045, #37324, #12054, #62926, #32641, #7385, #47976, #22710, #64167, #18638, #51666, #38900, #6109, #26368, #54844, #64475, #13927, #9265, #4964 ),
 .UNSPECIFIED., .F., .F.,
 ( 4, 2, 2, 2, 2, 2, 2, 2, 2, 2, 4 ),
 ( 3.903127820947815962E-18, 0.001139938506664698757, 0.001709907759997047159, 0.002279877013329395779, 0.003419815519994091283, 0.004559754026658787221, 0.005129723279991135407, 0.005699692533323483593, 0.006839631039988181699, 0.007979569546652876336, 0.009119508053317574442 ),
 .UNSPECIFIED. ) ;
#53711 = CARTESIAN_POINT ( 'NONE',  ( 37.00000000000000711, 4.705694406421931860E-17, -3.469127814946512892E-15 ) ) ;
#53712 = FACE_OUTER_BOUND ( 'NONE', #25081, .T. ) ;
#53713 = ORIENTED_EDGE ( 'NONE', *, *, #16052, .F. ) ;
#53714 = VERTEX_POINT ( 'NONE', #3053 ) ;
#53715 = CARTESIAN_POINT ( 'NONE',  ( 0.000000000000000000, -1.693411908627245221, 7.306323022404576761 ) ) ;
#53716 = CIRCLE ( 'NONE', #10167, 4.999999999999999112 ) ;
#53717 = VERTEX_POINT ( 'NONE', #8678 ) ;
#53718 = DIRECTION ( 'NONE',  ( 0.000000000000000000, 0.2006870767258819854, -0.9796553971857756560 ) ) ;
#53719 = DIRECTION ( 'NONE',  ( 0.9606638835031803270, -0.2535400141108140604, -0.1133241553124317708 ) ) ;
#53720 = DIRECTION ( 'NONE',  ( -1.000000000000000000, 0.000000000000000000, 0.000000000000000000 ) ) ;
#53721 = DIRECTION ( 'NONE',  ( 0.000000000000000000, -0.5243256840888622650, -0.8515178078024832065 ) ) ;
#53722 = FACE_OUTER_BOUND ( 'NONE', #38755, .T. ) ;
#53723 = CARTESIAN_POINT ( 'NONE',  ( 0.9232058338315048962, -7.723624854284649288, -9.791640253608225208 ) ) ;
#53725 = ORIENTED_EDGE ( 'NONE', *, *, #1642, .F. ) ;
#53724 = DIRECTION ( 'NONE',  ( -1.000000000000000000, 0.000000000000000000, 0.000000000000000000 ) ) ;
#53726 = CARTESIAN_POINT ( 'NONE',  ( -22.27718112499583469, 2.265557025479522757, 2.901898111564422678 ) ) ;
#53727 = EDGE_LOOP ( 'NONE', ( #31869, #43830, #35477, #5992 ) ) ;
#53728 = DIRECTION ( 'NONE',  ( 1.000000000000000000, 0.000000000000000000, 0.000000000000000000 ) ) ;
#53729 = ORIENTED_EDGE ( 'NONE', *, *, #55116, .T. ) ;
#53730 = ORIENTED_EDGE ( 'NONE', *, *, #20552, .F. ) ;
#53731 = CARTESIAN_POINT ( 'NONE',  ( -18.35026244561209552, 6.405804631758845069, 11.88625230963459067 ) ) ;
#53732 = CARTESIAN_POINT ( 'NONE',  ( -10.20982488791560883, -27.71818678970603500, 14.28592212877897438 ) ) ;
#53733 = DIRECTION ( 'NONE',  ( -0.8867529933577791290, 0.000000000000000000, -0.4622435816439406930 ) ) ;
#53734 = EDGE_CURVE ( 'NONE', #44729, #60783, #59264, .T. ) ;
#53735 = CARTESIAN_POINT ( 'NONE',  ( 2.305787727787083519, -2.774453000917102230, -7.135468203930011910 ) ) ;
#53736 = VECTOR ( 'NONE', #12736, 1000.000000000000000 ) ;
#53737 = DIRECTION ( 'NONE',  ( -1.000000000000000000, 0.000000000000000000, -0.000000000000000000 ) ) ;
#53738 = DIRECTION ( 'NONE',  ( 1.000000000000000000, -0.000000000000000000, -0.000000000000000000 ) ) ;
#53739 = ORIENTED_EDGE ( 'NONE', *, *, #52547, .T. ) ;
#53740 = CIRCLE ( 'NONE', #44182, 12.18650000000000055 ) ;
#53741 = CARTESIAN_POINT ( 'NONE',  ( -37.00000000000000711, -2.497432891016921008, 11.47758908105693720 ) ) ;
#53742 = CARTESIAN_POINT ( 'NONE',  ( 1.104777566491145890, -3.832109395972729260, 11.92547689818820800 ) ) ;
#53743 = DIRECTION ( 'NONE',  ( -1.000000000000000000, 0.000000000000000000, 0.000000000000000000 ) ) ;
#53744 = ORIENTED_EDGE ( 'NONE', *, *, #54129, .F. ) ;
#53745 = DIRECTION ( 'NONE',  ( -1.000000000000000000, 0.000000000000000000, 0.000000000000000000 ) ) ;
#53746 = ORIENTED_EDGE ( 'NONE', *, *, #23337, .T. ) ;
#53747 = DIRECTION ( 'NONE',  ( 1.000000000000000000, -0.000000000000000000, 0.000000000000000000 ) ) ;
#53748 = CARTESIAN_POINT ( 'NONE',  ( 0.3278977287071214719, -10.49733767381177607, -6.347150352417415320 ) ) ;
#53749 = DIRECTION ( 'NONE',  ( -1.000000000000000000, -0.000000000000000000, -0.000000000000000000 ) ) ;
#53750 = CIRCLE ( 'NONE', #36740, 2.899999999999995026 ) ;
#53751 = CYLINDRICAL_SURFACE ( 'NONE', #33719, 4.999999999999999112 ) ;
#53752 = CARTESIAN_POINT ( 'NONE',  ( 0.9232058338315058954, 3.908895078357680131, -11.84276737136196900 ) ) ;
#53753 = CARTESIAN_POINT ( 'NONE',  ( -27.10422407540562162, -1.954655484501055085, 1.306850885988407596 ) ) ;
#53754 = EDGE_CURVE ( 'NONE', #62148, #15452, #22033, .T. ) ;
#53755 = LINE ( 'NONE', #8190, #49273 ) ;
#53756 = ORIENTED_EDGE ( 'NONE', *, *, #37083, .T. ) ;
#53757 = DIRECTION ( 'NONE',  ( 0.000000000000000000, 0.01356324068817998940, -0.9999080150203990547 ) ) ;
#53758 = EDGE_CURVE ( 'NONE', #50610, #58860, #35238, .T. ) ;
#53759 = ORIENTED_EDGE ( 'NONE', *, *, #13436, .F. ) ;
#53760 = EDGE_CURVE ( 'NONE', #8369, #49125, #14147, .T. ) ;
#53761 = DIRECTION ( 'NONE',  ( -0.000000000000000000, -0.000000000000000000, -1.000000000000000000 ) ) ;
#53762 = CARTESIAN_POINT ( 'NONE',  ( 2.653899356900333739, 4.792827201941057602, -6.118160465319149033 ) ) ;
#53763 = CARTESIAN_POINT ( 'NONE',  ( 37.00000000000000711, 1.286231064351313735, -12.68495603654572257 ) ) ;
#53764 = CARTESIAN_POINT ( 'NONE',  ( 2.034671305879536263, -1.331347915349381683, -11.60021725667554193 ) ) ;
#53765 = CARTESIAN_POINT ( 'NONE',  ( -28.19149199850170717, 12.81122912241742995, -4.268081906603431896 ) ) ;
#53766 = EDGE_LOOP ( 'NONE', ( #6791, #12073, #21102, #5969 ) ) ;
#53767 = CARTESIAN_POINT ( 'NONE',  ( 6.593984040184932560, -8.829533010771809742, -10.21404802089835151 ) ) ;
#53768 = EDGE_CURVE ( 'NONE', #8663, #13128, #15299, .T. ) ;
#53769 = CARTESIAN_POINT ( 'NONE',  ( 5.516018279890452902, -0.001397286410094361001, 0.006629829924290971295 ) ) ;
#53770 = CARTESIAN_POINT ( 'NONE',  ( -27.08429572838383947, -2.089332284968714593, -0.9410937941434025511 ) ) ;
#53771 = FACE_OUTER_BOUND ( 'NONE', #38222, .T. ) ;
#53772 = EDGE_CURVE ( 'NONE', #17578, #52527, #41208, .T. ) ;
#53773 = ORIENTED_EDGE ( 'NONE', *, *, #54622, .F. ) ;
#53774 = CARTESIAN_POINT ( 'NONE',  ( 0.2653141617321010393, 12.05243138604825859, 2.169890202573236060 ) ) ;
#53775 = CARTESIAN_POINT ( 'NONE',  ( -22.27710395300133328, -2.620347679538745034, 2.585700543510492277 ) ) ;
#53776 = DIRECTION ( 'NONE',  ( 0.000000000000000000, 0.01356324068817998940, -0.9999080150203989437 ) ) ;
#53777 = DIRECTION ( 'NONE',  ( 0.000000000000000000, 1.000000000000000000, 0.000000000000000000 ) ) ;
#53778 = ADVANCED_FACE ( 'NONE', ( #30906 ), #14948, .T. ) ;
#53779 = CIRCLE ( 'NONE', #45267, 2.899999999999994582 ) ;
#53780 = EDGE_CURVE ( 'NONE', #807, #43133, #48906, .T. ) ;
#53781 = CARTESIAN_POINT ( 'NONE',  ( 3.092491956585452506, -3.565393530441456349, 7.070043156103451132 ) ) ;
#53782 = CARTESIAN_POINT ( 'NONE',  ( -28.25057532999396059, -10.95459410115464216, -4.908922407349892936 ) ) ;
#53783 = AXIS2_PLACEMENT_3D ( 'NONE', #29077, #9107, #33403 ) ;
#53784 = VERTEX_POINT ( 'NONE', #20629 ) ;
#53785 = CARTESIAN_POINT ( 'NONE',  ( -35.04582288351658548, 0.01196488372921770960, -0.004274985098085598047 ) ) ;
#53787 = EDGE_CURVE ( 'NONE', #15089, #18204, #35414, .T. ) ;
#53786 = CARTESIAN_POINT ( 'NONE',  ( 3.448218607682480563, -27.97504209442909939, -12.21548802405080991 ) ) ;
#53788 = ORIENTED_EDGE ( 'NONE', *, *, #32069, .F. ) ;
#53789 = CARTESIAN_POINT ( 'NONE',  ( 5.514970785353741078, -0.003415090918276209378, -0.003262412238248218153 ) ) ;
#53790 = DIRECTION ( 'NONE',  ( 1.000000000000000000, 0.000000000000000000, 0.000000000000000000 ) ) ;
#53791 = DIRECTION ( 'NONE',  ( -1.000000000000000000, -0.000000000000000000, 0.000000000000000000 ) ) ;
#53792 = CARTESIAN_POINT ( 'NONE',  ( -35.00000000000000000, 0.000000000000000000, 0.000000000000000000 ) ) ;
#53793 = CARTESIAN_POINT ( 'NONE',  ( 0.2676618633000466541, -11.56235835488943131, 4.037335446657195348 ) ) ;
#53794 = ORIENTED_EDGE ( 'NONE', *, *, #54229, .F. ) ;
#53795 = CARTESIAN_POINT ( 'NONE',  ( 5.536195898058073439, -0.003145317580921205142, 0.007896796515810326073 ) ) ;
#53796 = ORIENTED_EDGE ( 'NONE', *, *, #17577, .T. ) ;
#53797 = CARTESIAN_POINT ( 'NONE',  ( 2.241311220309555541, -7.205198716057802599, 2.523702734785320700 ) ) ;
#53799 = CARTESIAN_POINT ( 'NONE',  ( -35.00000000000000000, -0.06441628369844946966, 12.18632975068352842 ) ) ;
#53798 =( BOUNDED_CURVE ( )  B_SPLINE_CURVE ( 3, ( #41788, #41120, #56092, #62083 ),
 .UNSPECIFIED., .F., .F. ) 
 B_SPLINE_CURVE_WITH_KNOTS ( ( 4, 4 ),
 ( 1.491236873172884225, 1.527413679725934559 ),
 .UNSPECIFIED. ) 
 CURVE ( )  GEOMETRIC_REPRESENTATION_ITEM ( )  RATIONAL_B_SPLINE_CURVE ( ( 1.000000000000000000, 0.9998909395293115177, 0.9998909395293115177, 1.000000000000000000 ) ) 
 REPRESENTATION_ITEM ( '' )  );
#53800 = CARTESIAN_POINT ( 'NONE',  ( 2.034671305879990566, -9.380408876023713205, 6.953089744304931763 ) ) ;
#53801 = DIRECTION ( 'NONE',  ( 0.000000000000000000, 0.000000000000000000, 1.000000000000000000 ) ) ;
#53802 = CYLINDRICAL_SURFACE ( 'NONE', #61839, 4.999999999999999112 ) ;
#53803 = CARTESIAN_POINT ( 'NONE',  ( 35.00000000000000000, 5.672855678558685888, -10.28547182238010116 ) ) ;
#53804 = DIRECTION ( 'NONE',  ( 0.000000000000000000, 0.000000000000000000, 1.000000000000000000 ) ) ;
#53805 = VERTEX_POINT ( 'NONE', #25269 ) ;
#53806 = ORIENTED_EDGE ( 'NONE', *, *, #56212, .T. ) ;
#53807 = CARTESIAN_POINT ( 'NONE',  ( -17.63946288578489430, -7.321399697264532769, -9.512743050931277367 ) ) ;
#53808 = ORIENTED_EDGE ( 'NONE', *, *, #58503, .T. ) ;
#53809 =( LENGTH_UNIT ( ) NAMED_UNIT ( * ) SI_UNIT ( .MILLI., .METRE. ) );
#53810 = CARTESIAN_POINT ( 'NONE',  ( -22.29770266787582500, 2.588315884842656178, -2.703976473263633995 ) ) ;
#53811 = CARTESIAN_POINT ( 'NONE',  ( -27.15511094194037511, -0.1446243978645335992, -2.499833641087599201 ) ) ;
#53812 = EDGE_CURVE ( 'NONE', #22263, #26214, #48176, .T. ) ;
#53813 = CARTESIAN_POINT ( 'NONE',  ( 35.00000000000000000, 7.817492529713852889, -9.348667969174437431 ) ) ;
#53814 = ORIENTED_EDGE ( 'NONE', *, *, #24570, .F. ) ;
#53815 = CARTESIAN_POINT ( 'NONE',  ( 0.3057689695767493721, 5.928746590069732036, -10.73077184758785663 ) ) ;
#53816 = CARTESIAN_POINT ( 'NONE',  ( 2.241317068080793451, 6.565357088387198559, -3.896159243838468900 ) ) ;
#53817 = CARTESIAN_POINT ( 'NONE',  ( 18.00005080000000035, 0.000000000000000000, 1.499999999999997780 ) ) ;
#53818 = ORIENTED_EDGE ( 'NONE', *, *, #65123, .F. ) ;
#53819 = VERTEX_POINT ( 'NONE', #61184 ) ;
#53820 = CARTESIAN_POINT ( 'NONE',  ( -37.00000000000000711, 4.545979934229579023, -11.30684963584384306 ) ) ;
#53821 = EDGE_LOOP ( 'NONE', ( #9132, #53542, #45691, #45806 ) ) ;
#53822 = CARTESIAN_POINT ( 'NONE',  ( 37.00000000000000711, 4.705694406421931860E-17, -3.469127814946512892E-15 ) ) ;
#53823 = EDGE_CURVE ( 'NONE', #33456, #10138, #9934, .T. ) ;
#53824 = VERTEX_POINT ( 'NONE', #56182 ) ;
#53825 = VECTOR ( 'NONE', #41614, 1000.000000000000000 ) ;
#53826 = VERTEX_POINT ( 'NONE', #49899 ) ;
#53827 = CARTESIAN_POINT ( 'NONE',  ( 5.514624014163232779, 0.002789935220458468652, 0.003060352188290557749 ) ) ;
#53828 = DIRECTION ( 'NONE',  ( 0.000000000000000000, -0.01356324068817992175, 0.9999080150203990547 ) ) ;
#53829 = CARTESIAN_POINT ( 'NONE',  ( -27.08430418657511041, -2.280643121250624628, 0.2231435303617014532 ) ) ;
#53830 = CARTESIAN_POINT ( 'NONE',  ( -47.00000000000000711, 0.000000000000000000, 0.000000000000000000 ) ) ;
#53831 = LINE ( 'NONE', #8266, #36974 ) ;
#53832 = EDGE_CURVE ( 'NONE', #24551, #43237, #60919, .T. ) ;
#53833 = AXIS2_PLACEMENT_3D ( 'NONE', #17327, #32915, #32583 ) ;
#53834 = DIRECTION ( 'NONE',  ( 0.000000000000000000, -0.5987040770935737610, 0.8009703041134123014 ) ) ;
#53835 = EDGE_LOOP ( 'NONE', ( #58309, #32497 ) ) ;
#53836 = CARTESIAN_POINT ( 'NONE',  ( -37.00000000000000711, -12.49688848680886011, 2.527899948230591942 ) ) ;
#53837 = CYLINDRICAL_SURFACE ( 'NONE', #8932, 5.000000000000000888 ) ;
#53838 = DIRECTION ( 'NONE',  ( 1.000000000000000000, 0.000000000000000000, 0.000000000000000000 ) ) ;
#53839 = EDGE_CURVE ( 'NONE', #8090, #10925, #7808, .T. ) ;
#53840 = DIRECTION ( 'NONE',  ( -1.000000000000000000, 0.000000000000000000, 0.000000000000000000 ) ) ;
#53841 = DIRECTION ( 'NONE',  ( 1.000000000000000000, 0.000000000000000000, 0.000000000000000000 ) ) ;
#53842 = CARTESIAN_POINT ( 'NONE',  ( -27.09125059358711951, 1.607567221344183173, -1.662156772100930935 ) ) ;
#53843 = DIRECTION ( 'NONE',  ( -1.000000000000000000, 0.000000000000000000, 0.000000000000000000 ) ) ;
#53844 = CARTESIAN_POINT ( 'NONE',  ( 2.000000000000001776, 0.7281529553922108100, 7.464569195442779304 ) ) ;
#53845 = DIRECTION ( 'NONE',  ( 1.000000000000000000, 0.000000000000000000, 0.000000000000000000 ) ) ;
#53846 = ORIENTED_EDGE ( 'NONE', *, *, #38489, .T. ) ;
#53847 = CARTESIAN_POINT ( 'NONE',  ( 2.440552418640495880, -7.166505277347703817, -2.818488640081646679 ) ) ;
#53848 = ORIENTED_EDGE ( 'NONE', *, *, #35444, .T. ) ;
#53849 = CARTESIAN_POINT ( 'NONE',  ( 35.00000000000000000, -11.74226168163341555, -0.3025107581130825896 ) ) ;
#53850 = CARTESIAN_POINT ( 'NONE',  ( 0.3401186441510243297, -0.2556125181570694238, 12.26845925752606981 ) ) ;
#53851 = DIRECTION ( 'NONE',  ( 0.000000000000000000, 0.01356324068817998940, -0.9999080150203989437 ) ) ;
#53852 = CARTESIAN_POINT ( 'NONE',  ( 0.2653519991613832452, 9.366979519113348474, 7.888569541500555893 ) ) ;
#53853 = CARTESIAN_POINT ( 'NONE',  ( 3.092491956585984525, 5.424230976134757576, 5.768471164322518163 ) ) ;
#53854 = VERTEX_POINT ( 'NONE', #50239 ) ;
#53855 = DIRECTION ( 'NONE',  ( 0.000000000000000000, -0.01356324068817992175, 0.9999080150203990547 ) ) ;
#53856 = CARTESIAN_POINT ( 'NONE',  ( -22.27384469013076185, 3.564715702084495952, -0.9224151068931343289 ) ) ;
#53857 = DIRECTION ( 'NONE',  ( 1.000000000000000000, 0.000000000000000000, -0.000000000000000000 ) ) ;
#53858 = CARTESIAN_POINT ( 'NONE',  ( 0.3675815128205894289, 2.391755495700603973, 12.04510820461660003 ) ) ;
#53859 = EDGE_CURVE ( 'NONE', #37516, #23486, #19489, .T. ) ;
#53860 = EDGE_CURVE ( 'NONE', #22226, #41515, #31566, .T. ) ;
#53861 = CARTESIAN_POINT ( 'NONE',  ( 0.000000000000000000, -6.338823199656690832, 2.816798305433647620 ) ) ;
#53862 = CIRCLE ( 'NONE', #25172, 5.000000000000000888 ) ;
#53863 = VERTEX_POINT ( 'NONE', #62471 ) ;
#53865 = EDGE_CURVE ( 'NONE', #3409, #26770, #26920, .T. ) ;
#53864 = CARTESIAN_POINT ( 'NONE',  ( 0.2646305136544072623, -6.008537389229492653, 10.67138229758227652 ) ) ;
#53866 = CARTESIAN_POINT ( 'NONE',  ( 0.7400311444011713480, -8.241979373543594889, -9.270387619166411852 ) ) ;
#53867 = CARTESIAN_POINT ( 'NONE',  ( -16.98800322446194855, 2.922502605998049674, 25.00000000000000000 ) ) ;
#53868 = CIRCLE ( 'NONE', #26237, 5.000000000000000000 ) ;
#53869 = ORIENTED_EDGE ( 'NONE', *, *, #29896, .T. ) ;
#53870 = CIRCLE ( 'NONE', #19916, 5.000000000000000000 ) ;
#53871 = ORIENTED_EDGE ( 'NONE', *, *, #46571, .T. ) ;
#53872 = DIRECTION ( 'NONE',  ( -0.000000000000000000, -0.000000000000000000, -1.000000000000000000 ) ) ;
#53873 = ORIENTED_EDGE ( 'NONE', *, *, #58267, .T. ) ;
#53874 = DIRECTION ( 'NONE',  ( 1.000000000000000000, 0.000000000000000000, 0.000000000000000000 ) ) ;
#53875 = CARTESIAN_POINT ( 'NONE',  ( 37.00000000000000711, 11.16627499335655216, 3.645068577060061266 ) ) ;
#53876 = CARTESIAN_POINT ( 'NONE',  ( -27.10113028276028757, -1.697941299265485426, -1.613062633975405280 ) ) ;
#53877 = CARTESIAN_POINT ( 'NONE',  ( 0.2671309869109512181, 9.276621593297619484, -7.995521393275721422 ) ) ;
#53878 = FACE_OUTER_BOUND ( 'NONE', #30055, .T. ) ;
#53879 = VERTEX_POINT ( 'NONE', #21933 ) ;
#53880 = VERTEX_POINT ( 'NONE', #17608 ) ;
#53881 = VERTEX_POINT ( 'NONE', #52202 ) ;
#53882 = B_SPLINE_CURVE_WITH_KNOTS ( 'NONE', 3,
 ( #24315, #5036, #28, #44580, #4727, #64866, #14334, #24006, #9331, #29618, #49926, #24655, #45579, #13678, #24988, #45261, #65518, #10016, #54270, #8710, #30296, #28989 ),
 .UNSPECIFIED., .F., .F.,
 ( 4, 3, 3, 3, 3, 3, 3, 4 ),
 ( 1.318988870012550679E-18, 4.449119708436909988E-05, 6.626296329540551637E-05, 8.803456484962757917E-05, 0.0001098060367612809348, 0.0001315774408628539991, 0.0001760698110411219549, 0.0001829697163287831582 ),
 .UNSPECIFIED. ) ;
#53883 = CARTESIAN_POINT ( 'NONE',  ( 2.247206125382828379, 7.214589497757620151, -2.502718378778734376 ) ) ;
#53884 = CARTESIAN_POINT ( 'NONE',  ( 35.00000000000000000, 12.14284015767851166, 1.030638227056429157 ) ) ;
#53885 = ADVANCED_FACE ( 'NONE', ( #16937 ), #57518, .T. ) ;
#53886 = ORIENTED_EDGE ( 'NONE', *, *, #24188, .F. ) ;
#53887 = DIRECTION ( 'NONE',  ( 0.000000000000000000, -0.01356324068817999287, 0.9999080150203990547 ) ) ;
#53888 = CARTESIAN_POINT ( 'NONE',  ( -22.28121537037576871, -0.3168735205819631640, -3.680034389105507842 ) ) ;
#53889 = EDGE_CURVE ( 'NONE', #26353, #5798, #40741, .T. ) ;
#53890 = VERTEX_POINT ( 'NONE', #26263 ) ;
#53891 = CARTESIAN_POINT ( 'NONE',  ( 2.994568964204213035, 7.263701055179730304, 3.069094401380807025 ) ) ;
#53892 = CARTESIAN_POINT ( 'NONE',  ( 0.000000000000000000, -3.230174184210094168, 5.998318953995296354 ) ) ;
#53893 = DIRECTION ( 'NONE',  ( 1.000000000000000000, -0.000000000000000000, -0.000000000000000000 ) ) ;
#53894 = ORIENTED_EDGE ( 'NONE', *, *, #34854, .T. ) ;
#53895 = ORIENTED_EDGE ( 'NONE', *, *, #18166, .T. ) ;
#53896 = DIRECTION ( 'NONE',  ( 1.000000000000000000, 0.000000000000000000, -0.000000000000000000 ) ) ;
#53897 = VERTEX_POINT ( 'NONE', #31884 ) ;
#53898 = SURFACE_STYLE_USAGE ( .BOTH. , #23974 ) ;
#53899 = VERTEX_POINT ( 'NONE', #46538 ) ;
#53900 = EDGE_CURVE ( 'NONE', #49500, #43816, #12268, .T. ) ;
#53901 = CARTESIAN_POINT ( 'NONE',  ( 5.514970785353741078, 0.002619824551223704900, 0.003929719953530115030 ) ) ;
#53902 = DIRECTION ( 'NONE',  ( 0.3939253465568943735, 0.9034404741085543256, 0.1691689424289857246 ) ) ;
#53904 = AXIS2_PLACEMENT_3D ( 'NONE', #57583, #12004, #2037 ) ;
#53903 = DIRECTION ( 'NONE',  ( -1.000000000000000000, 0.000000000000000000, 0.000000000000000000 ) ) ;
#53905 = CARTESIAN_POINT ( 'NONE',  ( -35.00000000000000000, -11.53507381115581687, -2.216820770815207897 ) ) ;
#53906 = CARTESIAN_POINT ( 'NONE',  ( 0.4613984246114872789, 11.46927345719242552, -4.475519447653872440 ) ) ;
#53907 = DIRECTION ( 'NONE',  ( 0.000000000000000000, -0.01356324068817991828, 0.9999080150203990547 ) ) ;
#53908 = EDGE_LOOP ( 'NONE', ( #4499, #64457, #41961, #60668 ) ) ;
#53909 = LINE ( 'NONE', #13335, #42821 ) ;
#53910 = EDGE_LOOP ( 'NONE', ( #60979, #60579, #34644, #53193 ) ) ;
#53911 = DIRECTION ( 'NONE',  ( 0.3771207168306929813, -0.000000000000000000, 0.9261641133930337277 ) ) ;
#53912 = CARTESIAN_POINT ( 'NONE',  ( 0.9232058338315058954, -12.21058493388775013, 2.536181247095325109 ) ) ;
#53913 = EDGE_CURVE ( 'NONE', #12705, #39365, #63141, .T. ) ;
#53914 = ORIENTED_EDGE ( 'NONE', *, *, #25476, .F. ) ;
#53915 = DIRECTION ( 'NONE',  ( 0.000000000000000000, 0.000000000000000000, 1.000000000000000000 ) ) ;
#53916 = CARTESIAN_POINT ( 'NONE',  ( 0.2739690278137266732, 12.02985305092653334, -2.307031017960325503 ) ) ;
#53917 = B_SPLINE_CURVE_WITH_KNOTS ( 'NONE', 3,
 ( #48244, #2695, #42212, #58878, #47252, #22624, #12960, #33243, #52237, #57550, #63174, #17955, #13292, #23267, #1696, #27269 ),
 .UNSPECIFIED., .F., .F.,
 ( 4, 3, 3, 3, 3, 4 ),
 ( 1.908037674429563007E-15, 0.0002126834539180016254, 0.0004253519300366894536, 0.0006380165497225117992, 0.0007442707582429362130, 0.0009453531351410612241 ),
 .UNSPECIFIED. ) ;
#53918 = CARTESIAN_POINT ( 'NONE',  ( 0.3474126878361887827, -2.385599230261960635, -12.03947592323248905 ) ) ;
#53919 = VECTOR ( 'NONE', #56091, 1000.000000000000000 ) ;
#53920 = EDGE_CURVE ( 'NONE', #32028, #43145, #39797, .T. ) ;
#53921 = ORIENTED_EDGE ( 'NONE', *, *, #49517, .F. ) ;
#53922 = VERTEX_POINT ( 'NONE', #6967 ) ;
#53923 = AXIS2_PLACEMENT_3D ( 'NONE', #4423, #34964, #49965 ) ;
#53924 = FACE_OUTER_BOUND ( 'NONE', #36202, .T. ) ;
#53925 = VERTEX_POINT ( 'NONE', #21613 ) ;
#53926 = LINE ( 'NONE', #19000, #35950 ) ;
#53927 = DIRECTION ( 'NONE',  ( -1.000000000000000000, 0.000000000000000000, 0.000000000000000000 ) ) ;
#53928 = FACE_OUTER_BOUND ( 'NONE', #38819, .T. ) ;
#53929 = CARTESIAN_POINT ( 'NONE',  ( -35.00000000000000000, 6.711949091238296639, -10.84030624090599559 ) ) ;
#53930 = DIRECTION ( 'NONE',  ( 0.000000000000000000, 0.2355298848897516562, 0.9718671068226459875 ) ) ;
#53931 = VERTEX_POINT ( 'NONE', #6317 ) ;
#53932 = CYLINDRICAL_SURFACE ( 'NONE', #24267, 12.18649999999999878 ) ;
#53933 = EDGE_CURVE ( 'NONE', #16541, #24026, #21631, .T. ) ;
#53934 = EDGE_CURVE ( 'NONE', #41081, #58777, #7273, .T. ) ;
#53935 = CARTESIAN_POINT ( 'NONE',  ( 2.440552418640498544, -7.547055375260043775, -1.531218882877369847 ) ) ;
#53936 = B_SPLINE_CURVE_WITH_KNOTS ( 'NONE', 3,
 ( #8981, #60168, #29262, #49559, #3998, #19289, #15909 ),
 .UNSPECIFIED., .F., .F.,
 ( 4, 3, 4 ),
 ( 3.582791971490861909E-18, 0.002398160485434292465, 0.005002426799376466851 ),
 .UNSPECIFIED. ) ;
#53937 = DIRECTION ( 'NONE',  ( -1.000000000000000000, -0.000000000000000000, 0.000000000000000000 ) ) ;
#53938 = DIRECTION ( 'NONE',  ( -1.000000000000000000, -1.836970198721029688E-16, -0.000000000000000000 ) ) ;
#53939 = CARTESIAN_POINT ( 'NONE',  ( 2.000000000000001776, 2.480520636974283821, -6.345145617221223944 ) ) ;
#53940 = CARTESIAN_POINT ( 'NONE',  ( 3.663374565622874890, -11.05180360393428884, -4.676830153586281291 ) ) ;
#53941 = CARTESIAN_POINT ( 'NONE',  ( -22.30398854582847790, -2.724439933030904815, -2.594196582747015256 ) ) ;
#53942 = AXIS2_PLACEMENT_3D ( 'NONE', #41525, #16606, #22828 ) ;
#53943 = VERTEX_POINT ( 'NONE', #62165 ) ;
#53944 = CARTESIAN_POINT ( 'NONE',  ( 12.91062684683197936, -10.80902803636823251, -5.215964072882972147 ) ) ;
#53945 = CIRCLE ( 'NONE', #27399, 4.999999999999999112 ) ;
#53946 = ORIENTED_EDGE ( 'NONE', *, *, #56721, .F. ) ;
#53947 = CARTESIAN_POINT ( 'NONE',  ( 0.3654063281920728601, 1.872466061177246344, -12.13594617907220652 ) ) ;
#53948 = DIRECTION ( 'NONE',  ( -0.3865475372811021382, 0.9046932595863073079, -0.1791957239473569996 ) ) ;
#53949 = CARTESIAN_POINT ( 'NONE',  ( 0.2653141334712570965, 6.161213243425262220, 10.58342934917114420 ) ) ;
#53950 = ORIENTED_EDGE ( 'NONE', *, *, #3815, .F. ) ;
#53951 = AXIS2_PLACEMENT_3D ( 'NONE', #14060, #53338, #9081 ) ;
#53952 = CARTESIAN_POINT ( 'NONE',  ( 22.78386511336923093, 3.290201280387628824, -13.09362067330721757 ) ) ;
#53953 = VERTEX_POINT ( 'NONE', #16618 ) ;
#53954 = VERTEX_POINT ( 'NONE', #17271 ) ;
#53955 = VERTEX_POINT ( 'NONE', #42506 ) ;
#53956 = CARTESIAN_POINT ( 'NONE',  ( 29.71064890353178711, -9.099148391133041969, 9.982812328254121681 ) ) ;
#53957 = CARTESIAN_POINT ( 'NONE',  ( -22.59983133926800036, -0.06110861519530256386, 4.650609684383217868 ) ) ;
#53958 = ORIENTED_EDGE ( 'NONE', *, *, #8774, .F. ) ;
#53959 = DIRECTION ( 'NONE',  ( -1.000000000000000000, 0.000000000000000000, 0.000000000000000000 ) ) ;
#53960 = CARTESIAN_POINT ( 'NONE',  ( 3.916028893512121467, 5.727067861402937332, 12.22698748357986531 ) ) ;
#53961 = CARTESIAN_POINT ( 'NONE',  ( 35.00000000000000000, -8.295159312811920316, -8.927548052240867449 ) ) ;
#53962 = CARTESIAN_POINT ( 'NONE',  ( 0.2655924914740778742, -11.49267051747971280, 4.229867354073519436 ) ) ;
#53963 = EDGE_CURVE ( 'NONE', #44463, #13725, #21264, .T. ) ;
#53964 = ORIENTED_EDGE ( 'NONE', *, *, #41196, .F. ) ;
#53965 = DIRECTION ( 'NONE',  ( 0.000000000000000000, -0.6478160128811839558, 0.7617968321374970486 ) ) ;
#53966 = CARTESIAN_POINT ( 'NONE',  ( 15.04222346523121168, -34.74354600359600909, 6.996510958921167145 ) ) ;
#53967 = CARTESIAN_POINT ( 'NONE',  ( 2.280717697723837922, -1.481796453660269464, -7.502592193582068525 ) ) ;
#53969 = ORIENTED_EDGE ( 'NONE', *, *, #6342, .T. ) ;
#53968 = LINE ( 'NONE', #28684, #5439 ) ;
#53970 = CARTESIAN_POINT ( 'NONE',  ( 2.241352910868908310, 0.08337961031704246850, 7.633946224498473931 ) ) ;
#53971 = ORIENTED_EDGE ( 'NONE', *, *, #40149, .T. ) ;
#53972 = DIRECTION ( 'NONE',  ( 0.000000000000000000, -0.8696919319575238116, -0.4935949184179166949 ) ) ;
#53973 = ORIENTED_EDGE ( 'NONE', *, *, #7077, .F. ) ;
#53974 = DIRECTION ( 'NONE',  ( 0.000000000000000000, -0.01356324068817999114, 0.9999080150203989437 ) ) ;
#53975 = DIRECTION ( 'NONE',  ( 0.000000000000000000, -0.9105187689795998240, 0.4134677391718418193 ) ) ;
#53976 = DIRECTION ( 'NONE',  ( 1.000000000000000000, 0.000000000000000000, 0.000000000000000000 ) ) ;
#53977 = CARTESIAN_POINT ( 'NONE',  ( 3.152665057734120868, 6.378477742800529704, -4.725420687650643714 ) ) ;
#53978 = EDGE_CURVE ( 'NONE', #23142, #43264, #10990, .T. ) ;
#53979 = CARTESIAN_POINT ( 'NONE',  ( 0.2767916011545393240, 9.504925141026355107, 7.727819755721503370 ) ) ;
#53980 = CARTESIAN_POINT ( 'NONE',  ( -37.00000000000000711, 11.70009620280411688, 1.039216533672945753 ) ) ;
#53981 = CARTESIAN_POINT ( 'NONE',  ( -27.28563798457901513, -2.528380693767725340, 1.413023339712126569 ) ) ;
#53982 = ORIENTED_EDGE ( 'NONE', *, *, #52599, .F. ) ;
#53983 = AXIS2_PLACEMENT_3D ( 'NONE', #55780, #41115, #58078 ) ;
#53984 = DIRECTION ( 'NONE',  ( 1.000000000000000000, 0.000000000000000000, 0.000000000000000000 ) ) ;
#53985 = ORIENTED_EDGE ( 'NONE', *, *, #37196, .F. ) ;
#53986 = EDGE_CURVE ( 'NONE', #22284, #6123, #6008, .T. ) ;
#53987 = ORIENTED_EDGE ( 'NONE', *, *, #46259, .F. ) ;
#53988 = DIRECTION ( 'NONE',  ( 0.000000000000000000, 0.000000000000000000, 1.000000000000000000 ) ) ;
#53989 = FACE_OUTER_BOUND ( 'NONE', #23898, .T. ) ;
#53990 = CARTESIAN_POINT ( 'NONE',  ( -35.00000000000000000, -12.60630747491664572, 1.908798535168333643 ) ) ;
#53991 = CARTESIAN_POINT ( 'NONE',  ( 0.2767916011545364374, -10.51265105824867696, 6.288637995698077354 ) ) ;
#53992 = CARTESIAN_POINT ( 'NONE',  ( 5.516018279890452902, 0.0002248006052448508899, 0.006771744149385265123 ) ) ;
#53993 = EDGE_CURVE ( 'NONE', #40032, #22062, #24801, .T. ) ;
#53994 = AXIS2_PLACEMENT_3D ( 'NONE', #46147, #47130, #26181 ) ;
#53995 = DIRECTION ( 'NONE',  ( -1.000000000000000000, -0.000000000000000000, 0.000000000000000000 ) ) ;
#53996 = LINE ( 'NONE', #49027, #31247 ) ;
#53997 = VECTOR ( 'NONE', #51163, 1000.000000000000000 ) ;
#53998 = VECTOR ( 'NONE', #54714, 1000.000000000000000 ) ;
#53999 =( BOUNDED_CURVE ( )  B_SPLINE_CURVE ( 3, ( #29338, #34953, #8743, #13705 ),
 .UNSPECIFIED., .F., .F. ) 
 B_SPLINE_CURVE_WITH_KNOTS ( ( 4, 4 ),
 ( 5.154908875633210208, 5.200862432538539082 ),
 .UNSPECIFIED. ) 
 CURVE ( )  GEOMETRIC_REPRESENTATION_ITEM ( )  RATIONAL_B_SPLINE_CURVE ( ( 1.000000000000000000, 0.9998240302925252010, 0.9998240302925252010, 1.000000000000000000 ) ) 
 REPRESENTATION_ITEM ( '' )  );
#54000 = ORIENTED_EDGE ( 'NONE', *, *, #9742, .F. ) ;
#54001 = CARTESIAN_POINT ( 'NONE',  ( 37.00000000000000711, 2.544412758415841136, -11.91791701451267471 ) ) ;
#54002 = CARTESIAN_POINT ( 'NONE',  ( -27.08417473062937120, -1.503027223283682101, -1.729223128152646671 ) ) ;
#54003 = AXIS2_PLACEMENT_3D ( 'NONE', #29289, #45549, #29595 ) ;
#54004 = CARTESIAN_POINT ( 'NONE',  ( 0.2653519890538380555, 6.776488011961817416E-18, -12.24619734961521722 ) ) ;
#54005 = CIRCLE ( 'NONE', #20005, 5.000000000000000888 ) ;
#54006 = EDGE_CURVE ( 'NONE', #2871, #57207, #56659, .T. ) ;
#54007 = CARTESIAN_POINT ( 'NONE',  ( -17.71317172853720479, -11.35466418304648251, 3.882258812239222312 ) ) ;
#54008 = CARTESIAN_POINT ( 'NONE',  ( 1.372161826076962576, 5.789954543171331736, -11.20801830616803940 ) ) ;
#54009 = DIRECTION ( 'NONE',  ( -1.000000000000000000, 0.000000000000000000, 0.000000000000000000 ) ) ;
#54010 = CARTESIAN_POINT ( 'NONE',  ( -8.245440395195840821, -2.472445095731639508, 13.27222751525900435 ) ) ;
#54011 = ORIENTED_EDGE ( 'NONE', *, *, #59895, .T. ) ;
#54012 = CARTESIAN_POINT ( 'NONE',  ( -37.00000000000000711, 6.018036132182325026, -11.24036214326513949 ) ) ;
#54013 = FACE_OUTER_BOUND ( 'NONE', #20129, .T. ) ;
#54014 = DIRECTION ( 'NONE',  ( 0.000000000000000000, -0.01356324068817992175, 0.9999080150203990547 ) ) ;
#54015 = ADVANCED_FACE ( 'NONE', ( #48846 ), #8587, .T. ) ;
#54016 = AXIS2_PLACEMENT_3D ( 'NONE', #16386, #62249, #58255 ) ;
#54017 = CARTESIAN_POINT ( 'NONE',  ( -27.45775109278350712, 13.35262336282554152, -1.989333891161978674 ) ) ;
#54018 = CARTESIAN_POINT ( 'NONE',  ( 0.000000000000000000, 0.000000000000000000, 0.000000000000000000 ) ) ;
#54019 = VERTEX_POINT ( 'NONE', #58162 ) ;
#54020 = AXIS2_PLACEMENT_3D ( 'NONE', #1156, #1504, #52366 ) ;
#54021 = CARTESIAN_POINT ( 'NONE',  ( -17.16525335255839835, 3.058555645758342934, 13.14970181877596822 ) ) ;
#54022 = CYLINDRICAL_SURFACE ( 'NONE', #25781, 4.999999999999999112 ) ;
#54023 = CARTESIAN_POINT ( 'NONE',  ( 35.00000000000000000, 6.946017217730082294, 10.01317267707878500 ) ) ;
#54024 = EDGE_LOOP ( 'NONE', ( #21499, #29211, #10620, #37748 ) ) ;
#54025 = CARTESIAN_POINT ( 'NONE',  ( 0.3223008802179250232, 2.370176598416333213, 12.03398982086834934 ) ) ;
#54026 = CARTESIAN_POINT ( 'NONE',  ( 0.2652384770603657405, -4.126289928142327312, -11.53005438969048413 ) ) ;
#54027 = VERTEX_POINT ( 'NONE', #29210 ) ;
#54028 = ORIENTED_EDGE ( 'NONE', *, *, #18704, .F. ) ;
#54029 = FACE_OUTER_BOUND ( 'NONE', #50549, .T. ) ;
#54030 = CIRCLE ( 'NONE', #39161, 5.000000000000001776 ) ;
#54031 = ORIENTED_EDGE ( 'NONE', *, *, #1671, .F. ) ;
#54032 = DIRECTION ( 'NONE',  ( -0.000000000000000000, -1.000000000000000000, -0.000000000000000000 ) ) ;
#54033 = DIRECTION ( 'NONE',  ( 0.000000000000000000, -0.5155538571770110767, -0.8568571761675956022 ) ) ;
#54034 = VECTOR ( 'NONE', #63557, 1000.000000000000000 ) ;
#54035 = CARTESIAN_POINT ( 'NONE',  ( 2.241536586108912044, 7.517390684805887346, -1.331908602351562942 ) ) ;
#54036 = COLOUR_RGB ( '', 0.72549020, 0.75294118, 0.79215686) ;
#54037 = CARTESIAN_POINT ( 'NONE',  ( 2.247112776671466694, -7.539676020705987192, -1.211104213045449018 ) ) ;
#54038 = EDGE_CURVE ( 'NONE', #2298, #28421, #12928, .T. ) ;
#54039 = CARTESIAN_POINT ( 'NONE',  ( 0.000000000000000000, 2.664846396702499121, 6.404188155572998475 ) ) ;
#54041 = ORIENTED_EDGE ( 'NONE', *, *, #5047, .F. ) ;
#54040 = CARTESIAN_POINT ( 'NONE',  ( -18.08686583997218378, 5.151216734910788908, 25.00000000000000000 ) ) ;
#54042 = AXIS2_PLACEMENT_3D ( 'NONE', #58498, #12930, #53521 ) ;
#54043 = PRODUCT ( 'straight bevel gear_iso_ISO - Straight bevel gear 0.7M 36GT 12PT 20PA 5FW ---36O12H20MD8.0S1', 'straight bevel gear_iso_ISO - Straight bevel gear 0.7M 36GT 12PT 20PA 5FW ---36O12H20MD8.0S1', '', ( #37099 ) ) ;
#54044 = EDGE_CURVE ( 'NONE', #24896, #3865, #16309, .T. ) ;
#54045 = DIRECTION ( 'NONE',  ( -1.000000000000000000, 0.000000000000000000, -0.000000000000000000 ) ) ;
#54046 = EDGE_LOOP ( 'NONE', ( #23553, #37295, #21245, #53106 ) ) ;
#54047 = CARTESIAN_POINT ( 'NONE',  ( -22.71097035706202405, 0.4203397252017515573, -4.965150228107761521 ) ) ;
#54048 = ORIENTED_EDGE ( 'NONE', *, *, #46062, .F. ) ;
#54049 = VECTOR ( 'NONE', #15466, 1000.000000000000000 ) ;
#54050 = ORIENTED_EDGE ( 'NONE', *, *, #50377, .F. ) ;
#54051 = CARTESIAN_POINT ( 'NONE',  ( 37.00000000000000711, -2.627174906296994905, -11.44858830469739530 ) ) ;
#54052 = CARTESIAN_POINT ( 'NONE',  ( -7.103478058730853917, -31.43429545818073834, 14.15162322622613544 ) ) ;
#54053 = LINE ( 'NONE', #44072, #10960 ) ;
#54054 = EDGE_CURVE ( 'NONE', #37251, #15685, #38860, .T. ) ;
#54055 = CARTESIAN_POINT ( 'NONE',  ( 23.76437454561591522, 1.692121138565719107, 11.88453119584711182 ) ) ;
#54056 = CARTESIAN_POINT ( 'NONE',  ( 35.00000000000000000, 4.705694406421931860E-17, -3.469127814946512892E-15 ) ) ;
#54057 = DIRECTION ( 'NONE',  ( 0.000000000000000000, 0.1740410799127543318, 0.9847383929261630531 ) ) ;
#54058 = ORIENTED_EDGE ( 'NONE', *, *, #28208, .F. ) ;
#54059 = DIRECTION ( 'NONE',  ( 0.000000000000000000, 0.01356324068817992175, -0.9999080150203990547 ) ) ;
#54060 = CARTESIAN_POINT ( 'NONE',  ( 2.260457164927188511, 5.763213574030923603, -5.016645293558149810 ) ) ;
#54061 = LINE ( 'NONE', #8834, #16768 ) ;
#54062 = CARTESIAN_POINT ( 'NONE',  ( 35.00000000000000000, 4.705694406421931860E-17, -3.469127814946512892E-15 ) ) ;
#54063 = B_SPLINE_CURVE_WITH_KNOTS ( 'NONE', 3,
 ( #56712, #52691, #7119, #31415, #22406, #62314, #57342, #42672, #16460, #36727, #57026, #11447, #53346, #48683, #49363, #13099, #2485, #58331, #33700, #53678, #29055, #18756 ),
 .UNSPECIFIED., .F., .F.,
 ( 4, 3, 3, 3, 3, 3, 3, 4 ),
 ( 0.000000000000000000, 4.455945684386588987E-05, 6.636307477203692504E-05, 8.816671873158415896E-05, 0.0001099660380492575759, 0.0001317545563165277965, 0.0001762613022895024694, 0.0001867992666138357434 ),
 .UNSPECIFIED. ) ;
#54064 = EDGE_CURVE ( 'NONE', #21980, #11179, #1457, .T. ) ;
#54065 = EDGE_LOOP ( 'NONE', ( #15200, #13369, #30971, #16355 ) ) ;
#54066 = DIRECTION ( 'NONE',  ( 0.000000000000000000, 0.01356324068817998940, -0.9999080150203990547 ) ) ;
#54067 = FACE_OUTER_BOUND ( 'NONE', #4403, .T. ) ;
#54068 = CARTESIAN_POINT ( 'NONE',  ( 0.2646305136544065406, 12.24595685781654453, -0.1321451301298282588 ) ) ;
#54069 = CARTESIAN_POINT ( 'NONE',  ( 29.19808783025697352, 7.805332973316867040, 11.01506521398891891 ) ) ;
#54070 = DIRECTION ( 'NONE',  ( -1.000000000000000000, 0.000000000000000000, -0.000000000000000000 ) ) ;
#54071 = FACE_OUTER_BOUND ( 'NONE', #28731, .T. ) ;
#54072 = CIRCLE ( 'NONE', #40236, 12.18650000000000055 ) ;
#54073 = EDGE_CURVE ( 'NONE', #4699, #416, #38613, .T. ) ;
#54074 = LINE ( 'NONE', #48447, #30153 ) ;
#54075 = ORIENTED_EDGE ( 'NONE', *, *, #42094, .F. ) ;
#54076 = ORIENTED_EDGE ( 'NONE', *, *, #10824, .T. ) ;
#54077 = CARTESIAN_POINT ( 'NONE',  ( 1.719304012338831678, -5.066286238785654206, 11.67935079956403044 ) ) ;
#54078 = CARTESIAN_POINT ( 'NONE',  ( -37.00000000000000711, 0.000000000000000000, 0.000000000000000000 ) ) ;
#54079 = DIRECTION ( 'NONE',  ( -1.000000000000000000, -0.000000000000000000, 0.000000000000000000 ) ) ;
#54080 = VECTOR ( 'NONE', #13523, 1000.000000000000000 ) ;
#54081 = CARTESIAN_POINT ( 'NONE',  ( 2.827825597296801163, -1.027532345921625678, -8.965636292765733373 ) ) ;
#54082 = DIRECTION ( 'NONE',  ( -1.000000000000000000, 0.000000000000000000, 0.000000000000000000 ) ) ;
#54083 = VECTOR ( 'NONE', #42535, 1000.000000000000000 ) ;
#54084 = CARTESIAN_POINT ( 'NONE',  ( 4.231238796982053962, -10.86860989014256518, -8.012325656740021174 ) ) ;
#54085 = FACE_OUTER_BOUND ( 'NONE', #46343, .T. ) ;
#54086 = CARTESIAN_POINT ( 'NONE',  ( 2.257661810676419023, 1.459225434025981594, 7.499185766072595349 ) ) ;
#54087 = DIRECTION ( 'NONE',  ( 0.000000000000000000, 0.01356324068817998940, -0.9999080150203990547 ) ) ;
#54088 = VERTEX_POINT ( 'NONE', #13565 ) ;
#54089 = CARTESIAN_POINT ( 'NONE',  ( 0.2652384770603652409, 12.04846497255942772, 2.191555293694015916 ) ) ;
#54090 = CARTESIAN_POINT ( 'NONE',  ( -22.27878402819508352, -2.600576127690917172, 2.612733676624896972 ) ) ;
#54091 = FACE_OUTER_BOUND ( 'NONE', #28668, .T. ) ;
#54092 = VECTOR ( 'NONE', #56505, 1000.000000000000000 ) ;
#54093 = EDGE_CURVE ( 'NONE', #34672, #35595, #40689, .T. ) ;
#54094 = CARTESIAN_POINT ( 'NONE',  ( 41.00000000000000711, 1.820029539775944174E-16, -1.500000000000000222 ) ) ;
#54095 = CARTESIAN_POINT ( 'NONE',  ( -17.71314213125380377, -12.92974920937838057, 3.882255733911256890 ) ) ;
#54096 = VERTEX_POINT ( 'NONE', #43843 ) ;
#54097 = FACE_OUTER_BOUND ( 'NONE', #19744, .T. ) ;
#54098 = CYLINDRICAL_SURFACE ( 'NONE', #29057, 4.999999999999999112 ) ;
#54099 = CARTESIAN_POINT ( 'NONE',  ( -9.081998980629425233, -32.61802400030150295, -12.41144404786857081 ) ) ;
#54100 = VERTEX_POINT ( 'NONE', #64125 ) ;
#54101 = FACE_OUTER_BOUND ( 'NONE', #12503, .T. ) ;
#54102 = LINE ( 'NONE', #8541, #10822 ) ;
#54103 = CYLINDRICAL_SURFACE ( 'NONE', #25399, 6.342778212674966554 ) ;
#54104 = CARTESIAN_POINT ( 'NONE',  ( 1.109979610368937442, 12.51859925746076208, 0.4797593171722376870 ) ) ;
#54105 = CARTESIAN_POINT ( 'NONE',  ( -14.29135464769095520, 7.782112657557433089, 9.134479874907178498 ) ) ;
#54106 = CIRCLE ( 'NONE', #17994, 5.000000000000001776 ) ;
#54107 = ADVANCED_FACE ( 'NONE', ( #54488 ), #18903, .T. ) ;
#54108 = DIRECTION ( 'NONE',  ( 0.000000000000000000, 0.01356324068818000328, -0.9999080150203990547 ) ) ;
#54109 = VERTEX_POINT ( 'NONE', #49183 ) ;
#54110 = CARTESIAN_POINT ( 'NONE',  ( 2.249013661412228249, -7.216565855998267942, 2.498855301843061483 ) ) ;
#54111 = CARTESIAN_POINT ( 'NONE',  ( 0.3164563675027645129, -9.546944054903041987, -7.696930404785138791 ) ) ;
#54112 = DIRECTION ( 'NONE',  ( -1.000000000000000000, 0.000000000000000000, 0.000000000000000000 ) ) ;
#54113 = CARTESIAN_POINT ( 'NONE',  ( 2.305787727787085295, 7.566723232958088019, -1.164987321564654676 ) ) ;
#54115 = CARTESIAN_POINT ( 'NONE',  ( 2.241526690369557429, -3.802233103835215733, 6.620271521148420213 ) ) ;
#54114 = AXIS2_PLACEMENT_3D ( 'NONE', #23410, #29685, #54342 ) ;
#54116 = EDGE_CURVE ( 'NONE', #32831, #32332, #64751, .T. ) ;
#54117 = DIRECTION ( 'NONE',  ( 0.000000000000000000, 0.9970832820307041766, 0.07632122047556146038 ) ) ;
#54118 = DIRECTION ( 'NONE',  ( 0.000000000000000000, 0.01356324068817998940, -0.9999080150203990547 ) ) ;
#54119 = ORIENTED_EDGE ( 'NONE', *, *, #61119, .F. ) ;
#54120 = EDGE_CURVE ( 'NONE', #32235, #39817, #3643, .T. ) ;
#54121 = ORIENTED_EDGE ( 'NONE', *, *, #15182, .F. ) ;
#54122 = CARTESIAN_POINT ( 'NONE',  ( 2.000000000000001776, -6.935703035393428806, -0.1051458740708305362 ) ) ;
#54123 = EDGE_LOOP ( 'NONE', ( #12320, #50727, #18302, #26512 ) ) ;
#54124 = B_SPLINE_CURVE_WITH_KNOTS ( 'NONE', 3,
 ( #60957, #40991, #40004, #10723, #51321, #50658, #9739, #35664, #5772, #761, #26038, #46320, #40661, #20382, #21022, #30027 ),
 .UNSPECIFIED., .F., .F.,
 ( 4, 3, 3, 3, 3, 4 ),
 ( 2.285843118747037940E-15, 0.0002126834539180153677, 0.0004253519300367159623, 0.0006380165497225516978, 0.0007442707582429830505, 0.0009453531351407891978 ),
 .UNSPECIFIED. ) ;
#54125 = SURFACE_STYLE_FILL_AREA ( #64410 ) ;
#54126 = CARTESIAN_POINT ( 'NONE',  ( -37.00000000000000711, -11.13736569743278082, 4.946702696913133579 ) ) ;
#54127 = AXIS2_PLACEMENT_3D ( 'NONE', #29560, #49867, #60482 ) ;
#54128 = CARTESIAN_POINT ( 'NONE',  ( -27.20164183316781248, -0.1019800881472461007, -2.642567708136698279 ) ) ;
#54129 = EDGE_CURVE ( 'NONE', #6208, #64016, #36142, .T. ) ;
#54130 = CARTESIAN_POINT ( 'NONE',  ( -22.28776923226071460, -1.601293944844114359, 3.350304995653723417 ) ) ;
#54132 = VERTEX_POINT ( 'NONE', #53171 ) ;
#54131 = AXIS2_PLACEMENT_3D ( 'NONE', #60640, #65608, #25391 ) ;
#54133 = CARTESIAN_POINT ( 'NONE',  ( -35.00000000000000000, 0.000000000000000000, 0.000000000000000000 ) ) ;
#54134 = CARTESIAN_POINT ( 'NONE',  ( 2.573738926104375047, 1.575954828885357095, -7.583190312075753781 ) ) ;
#54136 = EDGE_CURVE ( 'NONE', #9776, #19326, #7675, .T. ) ;
#54135 = CARTESIAN_POINT ( 'NONE',  ( 2.259025283528624417, -5.014999102876465997, -5.764013728791902658 ) ) ;
#54137 = VERTEX_POINT ( 'NONE', #45150 ) ;
#54138 = ORIENTED_EDGE ( 'NONE', *, *, #45922, .T. ) ;
#54139 = CARTESIAN_POINT ( 'NONE',  ( -37.00000000000000711, -11.72195762423409349, -0.7536123767499773862 ) ) ;
#54140 = DIRECTION ( 'NONE',  ( 0.000000000000000000, -0.01356324068817991828, 0.9999080150203990547 ) ) ;
#54141 = ORIENTED_EDGE ( 'NONE', *, *, #18085, .T. ) ;
#54142 = AXIS2_PLACEMENT_3D ( 'NONE', #48912, #63843, #33606 ) ;
#54143 = ORIENTED_EDGE ( 'NONE', *, *, #33394, .F. ) ;
#54144 = DIRECTION ( 'NONE',  ( 0.000000000000000000, -0.01356324068817991828, 0.9999080150203990547 ) ) ;
#54145 = DIRECTION ( 'NONE',  ( 1.000000000000000000, 0.000000000000000000, -0.000000000000000000 ) ) ;
#54146 = CARTESIAN_POINT ( 'NONE',  ( -27.09861164373156228, -2.328930759213684976, 0.1603819633258212751 ) ) ;
#54147 = DIRECTION ( 'NONE',  ( -1.000000000000000000, -0.000000000000000000, 0.000000000000000000 ) ) ;
#54148 = FACE_OUTER_BOUND ( 'NONE', #62211, .T. ) ;
#54149 = ADVANCED_FACE ( 'NONE', ( #49814 ), #4263, .T. ) ;
#54150 = DIRECTION ( 'NONE',  ( 0.000000000000000000, 0.8276889981568920085, -0.5611870653623801664 ) ) ;
#54151 = VERTEX_POINT ( 'NONE', #20538 ) ;
#54152 = DIRECTION ( 'NONE',  ( 0.2475719085175094314, 0.000000000000000000, -0.9688695217174487784 ) ) ;
#54153 = CARTESIAN_POINT ( 'NONE',  ( 0.2650492433740053166, 7.786978278830098077, -9.451472485870480611 ) ) ;
#54154 = EDGE_CURVE ( 'NONE', #27489, #61832, #35460, .T. ) ;
#54155 = B_SPLINE_CURVE_WITH_KNOTS ( 'NONE', 3,
 ( #40299, #60592, #49093, #50636, #60933, #55938, #16364, #51943, #36636, #1408, #26015, #16677, #12337, #12012, #32602, #5749, #16010, #26654 ),
 .UNSPECIFIED., .F., .F.,
 ( 4, 2, 2, 2, 2, 2, 2, 2, 4 ),
 ( 4.168589959160076653E-21, 0.0008349329933307835482, 0.001669865986661567096, 0.002504798979992350644, 0.003339731973323134193, 0.004174664966653918174, 0.005009597959984701289, 0.005844530953315485271, 0.006679463946646270120 ),
 .UNSPECIFIED. ) ;
#54156 = CARTESIAN_POINT ( 'NONE',  ( 35.00000000000000000, 0.7214809346830272085, 11.72397916322010936 ) ) ;
#54157 = CARTESIAN_POINT ( 'NONE',  ( -17.83419946441818027, -9.720786832536937538, 25.00000000000000000 ) ) ;
#54158 = DIRECTION ( 'NONE',  ( 0.000000000000000000, 0.01356324068817998940, -0.9999080150203990547 ) ) ;
#54159 = CARTESIAN_POINT ( 'NONE',  ( -47.00000000000000711, 0.000000000000000000, 0.000000000000000000 ) ) ;
#54160 = DIRECTION ( 'NONE',  ( -1.000000000000000000, 0.000000000000000000, 0.000000000000000000 ) ) ;
#54161 = DIRECTION ( 'NONE',  ( -1.000000000000000000, 0.000000000000000000, 0.000000000000000000 ) ) ;
#54162 = CARTESIAN_POINT ( 'NONE',  ( -4.984431264850669230, -1.083143072858139710, 11.95218935805936056 ) ) ;
#54163 = VECTOR ( 'NONE', #47963, 1000.000000000000227 ) ;
#54164 = VECTOR ( 'NONE', #17279, 1000.000000000000000 ) ;
#54165 = ORIENTED_EDGE ( 'NONE', *, *, #34680, .T. ) ;
#54166 = CARTESIAN_POINT ( 'NONE',  ( -18.35310563997612476, 6.398290920003422144, -10.15549306850661004 ) ) ;
#54167 = VERTEX_POINT ( 'NONE', #54811 ) ;
#54168 = LINE ( 'NONE', #7979, #13660 ) ;
#54169 = CARTESIAN_POINT ( 'NONE',  ( 0.2648978790185593790, -0.1321385342563263510, 12.24533305150758089 ) ) ;
#54170 = CARTESIAN_POINT ( 'NONE',  ( 3.152665057735747567, 7.886634106564638813, 0.9030954876722160352 ) ) ;
#54171 = CARTESIAN_POINT ( 'NONE',  ( 0.2648978790185593790, 9.295532325666449935, 7.972372351883061370 ) ) ;
#54172 = CARTESIAN_POINT ( 'NONE',  ( 2.717984159220115714, 5.223388265380211948, 5.783767685176838036 ) ) ;
#54173 = ORIENTED_EDGE ( 'NONE', *, *, #206, .F. ) ;
#54174 = DIRECTION ( 'NONE',  ( 1.000000000000000000, 0.000000000000000000, 0.000000000000000000 ) ) ;
#54175 = CARTESIAN_POINT ( 'NONE',  ( -35.00000000000000000, 0.000000000000000000, 0.000000000000000000 ) ) ;
#54176 = CARTESIAN_POINT ( 'NONE',  ( 0.000000000000000000, 1.058508696394974358, 6.730038252034905355 ) ) ;
#54177 = CARTESIAN_POINT ( 'NONE',  ( 1.719304012338834786, 2.961219984257995819, 12.38166659046419227 ) ) ;
#54178 = EDGE_CURVE ( 'NONE', #11339, #23831, #14225, .T. ) ;
#54179 = EDGE_CURVE ( 'NONE', #60445, #153, #21559, .T. ) ;
#54180 = AXIS2_PLACEMENT_3D ( 'NONE', #21574, #46191, #20894 ) ;
#54181 = CARTESIAN_POINT ( 'NONE',  ( -41.00000000000000711, -25.03188948156373783, 4.499999999999997335 ) ) ;
#54182 =( BOUNDED_SURFACE ( )  B_SPLINE_SURFACE ( 3, 1, ( 
 ( #27128, #11492 ),
 ( #22462, #37420 ),
 ( #57731, #52415 ),
 ( #41414, #11181 ) ),
 .UNSPECIFIED., .F., .F., .F. ) 
 B_SPLINE_SURFACE_WITH_KNOTS ( ( 4, 4 ),
 ( 2, 2 ),
 ( 0.000000000000000000, 1.000000000000000000 ),
 ( 0.000000000000000000, 1.000000000000000000 ),
 .UNSPECIFIED. ) 
 GEOMETRIC_REPRESENTATION_ITEM ( )  RATIONAL_B_SPLINE_SURFACE ( (
 ( 1.000000000000000000, 1.000000000000000000),
 ( 0.9942764183789327692, 0.8450855930916585379),
 ( 0.9942764183789327692, 0.8450855930916585379),
 ( 1.000000000000000000, 1.000000000000000000) ) ) 
 REPRESENTATION_ITEM ( '' )  SURFACE ( )  );
#54183 = ORIENTED_EDGE ( 'NONE', *, *, #47064, .T. ) ;
#54184 = DIRECTION ( 'NONE',  ( 0.000000000000000000, 0.9105187689795969375, -0.4134677391718481476 ) ) ;
#54185 = VERTEX_POINT ( 'NONE', #44811 ) ;
#54186 = CARTESIAN_POINT ( 'NONE',  ( -37.00000000000000711, 0.000000000000000000, 0.000000000000000000 ) ) ;
#54187 = CARTESIAN_POINT ( 'NONE',  ( 3.455388140186510970, 8.284410676190361755, -8.681632586536968788 ) ) ;
#54188 = EDGE_CURVE ( 'NONE', #14567, #40113, #55117, .T. ) ;
#54189 = AXIS2_PLACEMENT_3D ( 'NONE', #51775, #47118, #6219 ) ;
#54190 = DIRECTION ( 'NONE',  ( 1.000000000000000000, -0.000000000000000000, 0.000000000000000000 ) ) ;
#54191 = DIRECTION ( 'NONE',  ( -1.000000000000000000, 0.000000000000000000, 0.000000000000000000 ) ) ;
#54192 = EDGE_CURVE ( 'NONE', #42378, #7123, #50793, .T. ) ;
#54193 = ORIENTED_EDGE ( 'NONE', *, *, #23587, .T. ) ;
#54194 = EDGE_LOOP ( 'NONE', ( #24046, #60405, #61687, #44368 ) ) ;
#54195 = CARTESIAN_POINT ( 'NONE',  ( -37.00000000000000711, 12.08151691381195825, -4.074242145635881052 ) ) ;
#54196 = CIRCLE ( 'NONE', #19319, 12.74999999999999822 ) ;
#54197 = CARTESIAN_POINT ( 'NONE',  ( 0.3665391374699464300, 4.447929964103003009, -11.44911061034381916 ) ) ;
#54198 = CARTESIAN_POINT ( 'NONE',  ( 2.241509619876138171, -5.823675573301041908, -4.936617871859563245 ) ) ;
#54199 = CARTESIAN_POINT ( 'NONE',  ( 0.2648321136542701182, 12.24520788540325711, 0.1417061099915184474 ) ) ;
#54200 = CARTESIAN_POINT ( 'NONE',  ( 0.2648978790185610999, 9.295532325666560070, -7.972372351882934360 ) ) ;
#54201 = CARTESIAN_POINT ( 'NONE',  ( -22.29115169517546136, -2.098196790595522998, -3.075985640626811790 ) ) ;
#54202 = VERTEX_POINT ( 'NONE', #55454 ) ;
#54203 = EDGE_CURVE ( 'NONE', #27200, #51547, #10218, .T. ) ;
#54204 = ORIENTED_EDGE ( 'NONE', *, *, #23895, .T. ) ;
#54205 = EDGE_LOOP ( 'NONE', ( #65013, #26564, #60471, #29527 ) ) ;
#54206 = DIRECTION ( 'NONE',  ( -1.000000000000000000, -0.000000000000000000, 0.000000000000000000 ) ) ;
#54208 = DIRECTION ( 'NONE',  ( -1.000000000000000000, -1.685093406416449860E-16, 1.011030131491573426E-17 ) ) ;
#54207 = VECTOR ( 'NONE', #5621, 1000.000000000000000 ) ;
#54209 = AXIS2_PLACEMENT_3D ( 'NONE', #52380, #43269, #28641 ) ;
#54210 = AXIS2_PLACEMENT_3D ( 'NONE', #1079, #62241, #61577 ) ;
#54211 = CIRCLE ( 'NONE', #29778, 5.000000000000000888 ) ;
#54212 = ORIENTED_EDGE ( 'NONE', *, *, #51401, .F. ) ;
#54213 = DIRECTION ( 'NONE',  ( 0.000000000000000000, -0.01356324068817991828, 0.9999080150203990547 ) ) ;
#54214 = CARTESIAN_POINT ( 'NONE',  ( 2.241311220309555097, -7.533971938435851001, 1.234192392743148847 ) ) ;
#54215 = ORIENTED_EDGE ( 'NONE', *, *, #27654, .T. ) ;
#54216 = CARTESIAN_POINT ( 'NONE',  ( -26.43258404273187523, 1.987083010659177251, -2.854888342447755800 ) ) ;
#54218 = EDGE_CURVE ( 'NONE', #37684, #22078, #56094, .T. ) ;
#54217 = LINE ( 'NONE', #37610, #60486 ) ;
#54219 = DIRECTION ( 'NONE',  ( 0.000000000000000000, 0.04924826701373889726, 0.9987865678893281807 ) ) ;
#54220 = ORIENTED_EDGE ( 'NONE', *, *, #53241, .T. ) ;
#54221 = ORIENTED_EDGE ( 'NONE', *, *, #24878, .F. ) ;
#54222 = CARTESIAN_POINT ( 'NONE',  ( 2.305787727787083519, 2.461236246751071555, 7.249469779319919205 ) ) ;
#54224 = VERTEX_POINT ( 'NONE', #9544 ) ;
#54223 = EDGE_CURVE ( 'NONE', #42938, #7910, #26981, .T. ) ;
#54225 = FILL_AREA_STYLE ('',( #53584 ) ) ;
#54226 = ORIENTED_EDGE ( 'NONE', *, *, #5069, .F. ) ;
#54227 = VERTEX_POINT ( 'NONE', #46148 ) ;
#54229 = EDGE_CURVE ( 'NONE', #38939, #32577, #30180, .T. ) ;
#54228 = ORIENTED_EDGE ( 'NONE', *, *, #48984, .T. ) ;
#54230 = CARTESIAN_POINT ( 'NONE',  ( 2.000000000000001776, 0.000000000000000000, 0.000000000000000000 ) ) ;
#54231 = CARTESIAN_POINT ( 'NONE',  ( -37.00000000000000711, -9.240395740215685549, 7.251710744571544964 ) ) ;
#54232 = DIRECTION ( 'NONE',  ( 1.000000000000000000, 0.000000000000000000, 0.000000000000000000 ) ) ;
#54233 = DIRECTION ( 'NONE',  ( 0.000000000000000000, 0.000000000000000000, -1.000000000000000000 ) ) ;
#54234 = CARTESIAN_POINT ( 'NONE',  ( -22.38932658256919694, -0.2254938976656423455, -4.011828264158265434 ) ) ;
#54235 = ORIENTED_EDGE ( 'NONE', *, *, #3879, .F. ) ;
#54236 = EDGE_CURVE ( 'NONE', #21790, #28847, #50350, .T. ) ;
#54237 = CIRCLE ( 'NONE', #3259, 12.75000000000000178 ) ;
#54238 = CARTESIAN_POINT ( 'NONE',  ( 2.242819959140643693, -7.138786956204143053, -2.707278038035143553 ) ) ;
#54239 = VECTOR ( 'NONE', #49467, 1000.000000000000000 ) ;
#54240 = ORIENTED_EDGE ( 'NONE', *, *, #63899, .T. ) ;
#54241 = CARTESIAN_POINT ( 'NONE',  ( 22.36482863261543486, 25.00000000000000000, -0.9234811557364158707 ) ) ;
#54242 = CARTESIAN_POINT ( 'NONE',  ( 35.00000000000000000, 4.705694406421931860E-17, -3.469127814946512892E-15 ) ) ;
#54243 = CIRCLE ( 'NONE', #24502, 12.18649999999999878 ) ;
#54244 = EDGE_CURVE ( 'NONE', #44838, #4743, #21082, .T. ) ;
#54245 = VERTEX_POINT ( 'NONE', #15207 ) ;
#54246 = B_SPLINE_CURVE_WITH_KNOTS ( 'NONE', 3,
 ( #17865, #53781, #53458, #43119, #38129, #14169, #2605, #33148, #28179, #48469, #29162, #48790, #49458, #64068, #3896, #3243 ),
 .UNSPECIFIED., .F., .F.,
 ( 4, 3, 3, 3, 3, 4 ),
 ( 2.486702240418149477E-15, 0.0002126834539179916508, 0.0004253519300366688538, 0.0006380165497224804657, 0.0007442707582428997838, 0.0009453531351413591629 ),
 .UNSPECIFIED. ) ;
#54247 = CARTESIAN_POINT ( 'NONE',  ( -15.08738464654653733, 8.458522730116888155, 8.511980925729206504 ) ) ;
#54248 = CARTESIAN_POINT ( 'NONE',  ( 0.3537226245948359438, 3.952322262392388375, 11.62199823003435384 ) ) ;
#54249 = AXIS2_PLACEMENT_3D ( 'NONE', #19954, #30574, #20282 ) ;
#54250 = CARTESIAN_POINT ( 'NONE',  ( 2.524535260911930923, -7.569872524928807245, 1.559291270914333394 ) ) ;
#54251 = ORIENTED_EDGE ( 'NONE', *, *, #56588, .F. ) ;
#54252 = VERTEX_POINT ( 'NONE', #45460 ) ;
#54253 = LINE ( 'NONE', #45246, #27968 ) ;
#54254 = CIRCLE ( 'NONE', #44628, 6.936499999999990784 ) ;
#54255 = EDGE_LOOP ( 'NONE', ( #9957, #14710, #25834, #58469 ) ) ;
#54256 = DIRECTION ( 'NONE',  ( -0.000000000000000000, -1.000000000000000000, -0.000000000000000000 ) ) ;
#54257 = CARTESIAN_POINT ( 'NONE',  ( 0.8320506296491635423, 9.767350172724423629, 7.696193170530645666 ) ) ;
#54258 = CARTESIAN_POINT ( 'NONE',  ( 0.000000000000000000, -33.00000000000000000, 0.000000000000000000 ) ) ;
#54260 = AXIS2_PLACEMENT_3D ( 'NONE', #15817, #51445, #50765 ) ;
#54259 = CARTESIAN_POINT ( 'NONE',  ( 3.152665057735899001, -7.886634106564667235, -0.9030954876721221103 ) ) ;
#54261 = CARTESIAN_POINT ( 'NONE',  ( 12.33930588725807631, 11.79251860674097685, -2.229502300750831889 ) ) ;
#54262 = ORIENTED_EDGE ( 'NONE', *, *, #43619, .F. ) ;
#54263 = CARTESIAN_POINT ( 'NONE',  ( 2.241352910868909643, 3.744764251557084922, -6.652881166698471738 ) ) ;
#54264 = CARTESIAN_POINT ( 'NONE',  ( 35.00000000000000000, 4.705694406421931860E-17, -3.469127814946512892E-15 ) ) ;
#54265 = CIRCLE ( 'NONE', #59572, 4.999999999999999112 ) ;
#54266 = EDGE_CURVE ( 'NONE', #47209, #12414, #54581, .T. ) ;
#54267 = AXIS2_PLACEMENT_3D ( 'NONE', #11546, #25204, #45824 ) ;
#54268 = AXIS2_PLACEMENT_3D ( 'NONE', #50114, #56063, #4571 ) ;
#54269 = EDGE_CURVE ( 'NONE', #41991, #62732, #30497, .T. ) ;
#54270 = CARTESIAN_POINT ( 'NONE',  ( 0.3610902822527252698, -12.13436647668549462, -1.873269382026117924 ) ) ;
#54271 = CIRCLE ( 'NONE', #58546, 11.99999999999998757 ) ;
#54272 = CARTESIAN_POINT ( 'NONE',  ( -17.22530951443547309, -6.628480137379963999, 10.00470364405594204 ) ) ;
#54273 = CYLINDRICAL_SURFACE ( 'NONE', #56159, 5.000000000000000888 ) ;
#54274 = CARTESIAN_POINT ( 'NONE',  ( 0.000000000000000000, 0.000000000000000000, 0.000000000000000000 ) ) ;
#54275 = CARTESIAN_POINT ( 'NONE',  ( 37.00000000000000711, -7.745827850123079727, -10.12742074351894317 ) ) ;
#54276 = CARTESIAN_POINT ( 'NONE',  ( 36.00000000000000711, 0.6593684648220483613, -12.73293890771483738 ) ) ;
#54277 = EDGE_CURVE ( 'NONE', #46044, #10053, #47132, .T. ) ;
#54278 = AXIS2_PLACEMENT_3D ( 'NONE', #54793, #30161, #9209 ) ;
#54279 = AXIS2_PLACEMENT_3D ( 'NONE', #60520, #39254, #65494 ) ;
#54280 = ORIENTED_EDGE ( 'NONE', *, *, #4909, .F. ) ;
#54281 = DIRECTION ( 'NONE',  ( -1.000000000000000000, 0.000000000000000000, 0.000000000000000000 ) ) ;
#54282 = CIRCLE ( 'NONE', #34034, 12.75000000000000178 ) ;
#54283 = ORIENTED_EDGE ( 'NONE', *, *, #29457, .T. ) ;
#54284 = DIRECTION ( 'NONE',  ( -1.000000000000000000, 0.000000000000000000, 0.000000000000000000 ) ) ;
#54285 = CARTESIAN_POINT ( 'NONE',  ( -22.27719412087655471, -3.642699606241631471, 0.5341638063191882502 ) ) ;
#54286 = CARTESIAN_POINT ( 'NONE',  ( 2.000000000000001776, -0.8935325819929111901, 7.446583077151331942 ) ) ;
#54287 = CIRCLE ( 'NONE', #56401, 4.999999999999999112 ) ;
#54288 = B_SPLINE_CURVE_WITH_KNOTS ( 'NONE', 3,
 ( #16124, #16774, #36408, #6484, #11149, #58018, #61667, #51720, #17110, #6165, #26760, #57352, #42683, #32699, #32060, #52379, #6823, #57693, #12114, #52701, #7125, #27403 ),
 .UNSPECIFIED., .F., .F.,
 ( 4, 3, 3, 3, 3, 3, 3, 4 ),
 ( 0.000000000000000000, 4.447697177976088099E-05, 6.624143997790994502E-05, 8.800576886943949225E-05, 0.0001097699864780839652, 0.0001315341395364316897, 0.0001760120188223209209, 0.0001867971373174606459 ),
 .UNSPECIFIED. ) ;
#54289 = CARTESIAN_POINT ( 'NONE',  ( 0.2653519789438759657, -12.24619733037255997, 0.02203059356484748585 ) ) ;
#54290 = ORIENTED_EDGE ( 'NONE', *, *, #65188, .T. ) ;
#54291 = EDGE_CURVE ( 'NONE', #60108, #39829, #36806, .T. ) ;
#54292 = CIRCLE ( 'NONE', #24561, 5.000000000000000000 ) ;
#54293 = ORIENTED_EDGE ( 'NONE', *, *, #56996, .T. ) ;
#54294 = ORIENTED_EDGE ( 'NONE', *, *, #42607, .T. ) ;
#54295 = CARTESIAN_POINT ( 'NONE',  ( 0.2648321136542706178, -7.762514728658031160, -9.471460387169347683 ) ) ;
#54296 = EDGE_CURVE ( 'NONE', #42715, #58005, #44877, .T. ) ;
#54297 = ORIENTED_EDGE ( 'NONE', *, *, #48799, .T. ) ;
#54298 = CARTESIAN_POINT ( 'NONE',  ( -22.27718112499583469, -2.265557025479512099, -2.901898111564459093 ) ) ;
#54299 = DIRECTION ( 'NONE',  ( -1.000000000000000000, -0.000000000000000000, -0.000000000000000000 ) ) ;
#54300 = CARTESIAN_POINT ( 'NONE',  ( 5.516018279890452902, 0.0009545156522407046611, 0.006707902355169304519 ) ) ;
#54301 = AXIS2_PLACEMENT_3D ( 'NONE', #49261, #60185, #8672 ) ;
#54302 = DIRECTION ( 'NONE',  ( -1.000000000000000000, 0.000000000000000000, 0.000000000000000000 ) ) ;
#54303 = ORIENTED_EDGE ( 'NONE', *, *, #16731, .F. ) ;
#54304 = DIRECTION ( 'NONE',  ( 0.000000000000000000, 0.000000000000000000, 1.000000000000000000 ) ) ;
#54305 = DIRECTION ( 'NONE',  ( 1.000000000000000000, -0.000000000000000000, -0.000000000000000000 ) ) ;
#54306 = CYLINDRICAL_SURFACE ( 'NONE', #37700, 4.999999999999999112 ) ;
#54308 = VERTEX_POINT ( 'NONE', #31489 ) ;
#54307 = CARTESIAN_POINT ( 'NONE',  ( 42.50000000000000000, -2.710505431213761085E-17, 1.201363017033314212E-18 ) ) ;
#54310 = CIRCLE ( 'NONE', #4372, 6.936499999999990784 ) ;
#54309 = CARTESIAN_POINT ( 'NONE',  ( 0.2638984909335720941, 5.950360275955205225, -10.70468911391657940 ) ) ;
#54311 = ORIENTED_EDGE ( 'NONE', *, *, #12080, .F. ) ;
#54312 = CARTESIAN_POINT ( 'NONE',  ( 0.2739690278137258961, -6.282352088166191173, -10.51531306167493085 ) ) ;
#54313 = ORIENTED_EDGE ( 'NONE', *, *, #10788, .T. ) ;
#54314 = DIRECTION ( 'NONE',  ( 0.000000000000000000, 0.000000000000000000, -1.000000000000000000 ) ) ;
#54315 = CARTESIAN_POINT ( 'NONE',  ( 0.2671309869109484980, 4.036029264453140364, -11.56263543972754704 ) ) ;
#54316 = EDGE_CURVE ( 'NONE', #30274, #136, #51789, .T. ) ;
#54317 = CARTESIAN_POINT ( 'NONE',  ( -35.00000000000000000, 9.700295462048664774, 7.376655759824919834 ) ) ;
#54318 = CARTESIAN_POINT ( 'NONE',  ( -35.00000000000000000, 0.000000000000000000, 0.000000000000000000 ) ) ;
#54319 = AXIS2_PLACEMENT_3D ( 'NONE', #14572, #64791, #44856 ) ;
#54320 = VECTOR ( 'NONE', #25375, 1000.000000000000000 ) ;
#54321 = CARTESIAN_POINT ( 'NONE',  ( 0.2651627682582921586, -11.47719223137562850, 4.271106202749230363 ) ) ;
#54322 = CARTESIAN_POINT ( 'NONE',  ( -9.169765030952540030, -3.248313620670495006, -13.10426324017876887 ) ) ;
#54323 = CARTESIAN_POINT ( 'NONE',  ( 10.74559270775345432, 13.46648889917082847, -0.9568044215894803139 ) ) ;
#54324 = EDGE_CURVE ( 'NONE', #35667, #60506, #46455, .T. ) ;
#54325 = ORIENTED_EDGE ( 'NONE', *, *, #60242, .F. ) ;
#54326 = DIRECTION ( 'NONE',  ( 1.000000000000000000, 0.000000000000000000, 0.000000000000000000 ) ) ;
#54327 = VERTEX_POINT ( 'NONE', #6889 ) ;
#54328 = B_SPLINE_CURVE_WITH_KNOTS ( 'NONE', 3,
 ( #42612, #12046, #32324, #3417, #23686, #47629, #62571 ),
 .UNSPECIFIED., .F., .F.,
 ( 4, 3, 4 ),
 ( 4.934630583344367301E-15, 0.002398160485434615557, 0.005002426799381651940 ),
 .UNSPECIFIED. ) ;
#54329 = EDGE_CURVE ( 'NONE', #55598, #3201, #16538, .T. ) ;
#54330 = ORIENTED_EDGE ( 'NONE', *, *, #30602, .F. ) ;
#54331 = CARTESIAN_POINT ( 'NONE',  ( 22.88594695219327235, -4.822122601967141264, -12.60940655271284427 ) ) ;
#54332 = CARTESIAN_POINT ( 'NONE',  ( 1.719304012338199517, 1.559079228025238604E-15, 12.73084802173761787 ) ) ;
#54333 = CYLINDRICAL_SURFACE ( 'NONE', #19594, 7.499999999999988454 ) ;
#54334 = CARTESIAN_POINT ( 'NONE',  ( -22.30986928587821794, 2.105440358094968545, 3.138878161034310388 ) ) ;
#54336 = CIRCLE ( 'NONE', #10778, 5.000000000000000000 ) ;
#54335 = CARTESIAN_POINT ( 'NONE',  ( 35.00000000000000000, -10.14433819232439049, -6.753013023069681431 ) ) ;
#54337 = AXIS2_PLACEMENT_3D ( 'NONE', #20071, #60628, #5451 ) ;
#54338 = CARTESIAN_POINT ( 'NONE',  ( 0.2911222467163553929, 10.71854909364326325, -5.940753417478811471 ) ) ;
#54339 = CARTESIAN_POINT ( 'NONE',  ( 1.000000000000000888, -3.937687286050771895, -6.383151168292510391 ) ) ;
#54340 = AXIS2_PLACEMENT_3D ( 'NONE', #29861, #19585, #50171 ) ;
#54341 = ORIENTED_EDGE ( 'NONE', *, *, #30829, .T. ) ;
#54342 = DIRECTION ( 'NONE',  ( 0.000000000000000000, -0.01356324068817998940, 0.9999080150203990547 ) ) ;
#54343 = CIRCLE ( 'NONE', #14995, 7.499999999999988454 ) ;
#54344 = DIRECTION ( 'NONE',  ( -1.000000000000000000, 0.000000000000000000, 0.000000000000000000 ) ) ;
#54345 = DIRECTION ( 'NONE',  ( 0.000000000000000000, -0.8515178078024813191, 0.5243256840888652626 ) ) ;
#54346 = ORIENTED_EDGE ( 'NONE', *, *, #27468, .T. ) ;
#54347 = AXIS2_PLACEMENT_3D ( 'NONE', #11144, #25438, #42036 ) ;
#54348 = ADVANCED_FACE ( 'NONE', ( #6232 ), #21857, .T. ) ;
#54349 = CARTESIAN_POINT ( 'NONE',  ( -11.40165637463000259, -7.324853138339117109, 11.34220541683159489 ) ) ;
#54350 = CYLINDRICAL_SURFACE ( 'NONE', #24652, 6.936499999999988120 ) ;
#54351 = AXIS2_PLACEMENT_3D ( 'NONE', #24037, #23719, #53965 ) ;
#54352 = CIRCLE ( 'NONE', #38379, 12.18649999999999878 ) ;
#54353 = ORIENTED_EDGE ( 'NONE', *, *, #35342, .F. ) ;
#54354 = DIRECTION ( 'NONE',  ( 0.000000000000000000, -0.01356324068818001369, 0.9999080150203990547 ) ) ;
#54355 = DIRECTION ( 'NONE',  ( -1.000000000000000000, 0.000000000000000000, 0.000000000000000000 ) ) ;
#54356 = DIRECTION ( 'NONE',  ( 0.000000000000000000, -0.9635499925192201331, -0.2675283385292311356 ) ) ;
#54357 = AXIS2_PLACEMENT_3D ( 'NONE', #31124, #61063, #45758 ) ;
#54358 = VECTOR ( 'NONE', #20120, 1000.000000000000000 ) ;
#54359 = AXIS2_PLACEMENT_3D ( 'NONE', #16055, #32333, #37323 ) ;
#54360 = CARTESIAN_POINT ( 'NONE',  ( -25.54435311314727386, 5.747082554913779617, 10.54001105275434291 ) ) ;
#54361 = DIRECTION ( 'NONE',  ( 0.000000000000000000, -0.9346839223284579834, 0.3554799084908866202 ) ) ;
#54362 = ORIENTED_EDGE ( 'NONE', *, *, #962, .T. ) ;
#54363 = CARTESIAN_POINT ( 'NONE',  ( 19.28625800530496903, 1.699513388191793428, 11.87904264843580471 ) ) ;
#54364 = CARTESIAN_POINT ( 'NONE',  ( -9.838098675710270413, -10.18811004032726686, -6.355130291591023273 ) ) ;
#54365 = LINE ( 'NONE', #44672, #45627 ) ;
#54366 = VERTEX_POINT ( 'NONE', #26182 ) ;
#54367 = CARTESIAN_POINT ( 'NONE',  ( 21.44353899438906907, 13.23503942470536643, -2.693104912682990015 ) ) ;
#54368 = DIRECTION ( 'NONE',  ( 1.000000000000000000, 0.000000000000000000, 0.000000000000000000 ) ) ;
#54369 = ORIENTED_EDGE ( 'NONE', *, *, #20482, .F. ) ;
#54370 = EDGE_CURVE ( 'NONE', #37836, #64097, #6822, .T. ) ;
#54371 = ORIENTED_EDGE ( 'NONE', *, *, #55728, .T. ) ;
#54372 = DIRECTION ( 'NONE',  ( -1.000000000000000000, 0.000000000000000000, 0.000000000000000000 ) ) ;
#54373 = AXIS2_PLACEMENT_3D ( 'NONE', #8964, #14267, #54530 ) ;
#54374 = EDGE_CURVE ( 'NONE', #11657, #33165, #32458, .T. ) ;
#54375 = VECTOR ( 'NONE', #19267, 1000.000000000000000 ) ;
#54376 = VERTEX_POINT ( 'NONE', #61741 ) ;
#54377 = AXIS2_PLACEMENT_3D ( 'NONE', #22024, #56286, #42278 ) ;
#54378 = DIRECTION ( 'NONE',  ( 0.000000000000000000, -0.01356324068817998940, 0.9999080150203990547 ) ) ;
#54379 = CARTESIAN_POINT ( 'NONE',  ( 0.2653141617321040924, 6.161204121352837682, -10.58343467791289072 ) ) ;
#54381 = CYLINDRICAL_SURFACE ( 'NONE', #4693, 12.75000000000000178 ) ;
#54380 =( BOUNDED_SURFACE ( )  B_SPLINE_SURFACE ( 3, 1, ( 
 ( #56757, #20825 ),
 ( #26150, #6198 ),
 ( #15496, #31455 ),
 ( #46423, #868 ) ),
 .UNSPECIFIED., .F., .F., .F. ) 
 B_SPLINE_SURFACE_WITH_KNOTS ( ( 4, 4 ),
 ( 2, 2 ),
 ( 0.000000000000000000, 1.000000000000000000 ),
 ( 0.000000000000000000, 1.000000000000000000 ),
 .UNSPECIFIED. ) 
 GEOMETRIC_REPRESENTATION_ITEM ( )  RATIONAL_B_SPLINE_SURFACE ( (
 ( 1.000000000000000000, 1.000000000000000000),
 ( 0.8716676215708681896, 0.8964445200148167814),
 ( 0.8716676215708681896, 0.8964445200148167814),
 ( 1.000000000000000000, 1.000000000000000000) ) ) 
 REPRESENTATION_ITEM ( '' )  SURFACE ( )  );
#54382 = CARTESIAN_POINT ( 'NONE',  ( 2.263328370261528555, -7.548992860189814635, -1.186889399881268181 ) ) ;
#54383 = FACE_OUTER_BOUND ( 'NONE', #13704, .T. ) ;
#54385 = ORIENTED_EDGE ( 'NONE', *, *, #57172, .T. ) ;
#54384 = DIRECTION ( 'NONE',  ( -1.000000000000000000, 0.000000000000000000, 0.000000000000000000 ) ) ;
#54386 = CARTESIAN_POINT ( 'NONE',  ( -35.00000000000000000, 8.699265615722982403, 8.534258022646129760 ) ) ;
#54387 = ORIENTED_EDGE ( 'NONE', *, *, #29435, .F. ) ;
#54388 = DIRECTION ( 'NONE',  ( 1.000000000000000000, 0.000000000000000000, -0.000000000000000000 ) ) ;
#54389 = AXIS2_PLACEMENT_3D ( 'NONE', #1084, #55641, #35972 ) ;
#54390 = EDGE_LOOP ( 'NONE', ( #24800, #37707, #35095, #48576 ) ) ;
#54391 = ORIENTED_EDGE ( 'NONE', *, *, #9524, .F. ) ;
#54392 = CARTESIAN_POINT ( 'NONE',  ( -15.91316379733282282, 8.402199048040264628, 10.56663549368182942 ) ) ;
#54393 = CARTESIAN_POINT ( 'NONE',  ( -2.287538219536366935, -28.18941229671508708, 13.77533426008843165 ) ) ;
#54394 = ADVANCED_FACE ( 'NONE', ( #57421 ), #21525, .T. ) ;
#54395 = DIRECTION ( 'NONE',  ( 0.000000000000000000, 0.000000000000000000, 1.000000000000000000 ) ) ;
#54396 = DIRECTION ( 'NONE',  ( 0.000000000000000000, 0.000000000000000000, 1.000000000000000000 ) ) ;
#54397 = FACE_OUTER_BOUND ( 'NONE', #51454, .T. ) ;
#54398 = CARTESIAN_POINT ( 'NONE',  ( 2.242418902651536428, 5.912154560269232917, 4.830735119002372180 ) ) ;
#54399 = ORIENTED_EDGE ( 'NONE', *, *, #16611, .F. ) ;
#54400 = AXIS2_PLACEMENT_3D ( 'NONE', #4851, #61334, #39750 ) ;
#54401 =( BOUNDED_SURFACE ( )  B_SPLINE_SURFACE ( 3, 1, ( 
 ( #40751, #50737 ),
 ( #46717, #21456 ),
 ( #9825, #21109 ),
 ( #41727, #46083 ) ),
 .UNSPECIFIED., .F., .F., .F. ) 
 B_SPLINE_SURFACE_WITH_KNOTS ( ( 4, 4 ),
 ( 2, 2 ),
 ( 0.000000000000000000, 1.000000000000000000 ),
 ( 0.000000000000000000, 1.000000000000000000 ),
 .UNSPECIFIED. ) 
 GEOMETRIC_REPRESENTATION_ITEM ( )  RATIONAL_B_SPLINE_SURFACE ( (
 ( 1.000000000000000000, 1.000000000000000000),
 ( 0.9942764183789327692, 0.8450855930916580938),
 ( 0.9942764183789327692, 0.8450855930916580938),
 ( 1.000000000000000000, 1.000000000000000000) ) ) 
 REPRESENTATION_ITEM ( '' )  SURFACE ( )  );
#54402 = ORIENTED_EDGE ( 'NONE', *, *, #10077, .F. ) ;
#54403 = B_SPLINE_CURVE_WITH_KNOTS ( 'NONE', 3,
 ( #24161, #10175, #29787, #50104, #35096, #59748, #30456, #14811, #14493, #14177, #60388, #35753, #24828, #54770, #3904, #15487 ),
 .UNSPECIFIED., .F., .F.,
 ( 4, 3, 3, 3, 3, 4 ),
 ( 0.000000000000000000, 0.0002999043160757219450, 0.0005998071753050750882, 0.0008997092107374163967, 0.001204458948194988069, 0.001510329163475231757 ),
 .UNSPECIFIED. ) ;
#54404 = CARTESIAN_POINT ( 'NONE',  ( 35.00000000000000000, 0.9416912585476243658, 12.71517666308946204 ) ) ;
#54405 = CARTESIAN_POINT ( 'NONE',  ( -35.00000000000000000, -11.02904044024211849, 4.041347439435823752 ) ) ;
#54406 = ORIENTED_EDGE ( 'NONE', *, *, #64229, .F. ) ;
#54408 = CIRCLE ( 'NONE', #59709, 4.999999999999999112 ) ;
#54407 = CYLINDRICAL_SURFACE ( 'NONE', #11473, 4.999999999999999112 ) ;
#54409 = CARTESIAN_POINT ( 'NONE',  ( 0.3537226245948383863, 0.2609894354291231178, -12.27287980220284425 ) ) ;
#54410 = DIRECTION ( 'NONE',  ( 0.000000000000000000, 0.000000000000000000, 1.000000000000000000 ) ) ;
#54411 = CARTESIAN_POINT ( 'NONE',  ( -22.30527770659433173, 3.125767038151207267, -2.100259071719456028 ) ) ;
#54412 = EDGE_CURVE ( 'NONE', #21947, #18329, #11853, .T. ) ;
#54413 = AXIS2_PLACEMENT_3D ( 'NONE', #12789, #33078, #28112 ) ;
#54414 = CARTESIAN_POINT ( 'NONE',  ( -37.00000000000000711, 0.000000000000000000, 0.000000000000000000 ) ) ;
#54415 = CIRCLE ( 'NONE', #63976, 4.999999999999999112 ) ;
#54416 = CARTESIAN_POINT ( 'NONE',  ( 2.255723233588950105, 3.933511348457526591, -6.548644987607518786 ) ) ;
#54417 = ORIENTED_EDGE ( 'NONE', *, *, #42991, .T. ) ;
#54418 = VERTEX_POINT ( 'NONE', #27160 ) ;
#54419 = CARTESIAN_POINT ( 'NONE',  ( -27.20164183316779827, 1.409601201084051514, 2.237540722393148940 ) ) ;
#54420 = CARTESIAN_POINT ( 'NONE',  ( 3.092491956585849522, 4.738927301402013903, -6.343509225035191434 ) ) ;
#54421 = CARTESIAN_POINT ( 'NONE',  ( -14.47334165536100059, 5.400000000000000355, 0.000000000000000000 ) ) ;
#54422 = VECTOR ( 'NONE', #46123, 1000.000000000000000 ) ;
#54423 = AXIS2_PLACEMENT_3D ( 'NONE', #18560, #38812, #59111 ) ;
#54424 = CYLINDRICAL_SURFACE ( 'NONE', #44041, 5.000000000000000888 ) ;
#54425 = CARTESIAN_POINT ( 'NONE',  ( 35.00000000000000000, 4.705694406421931860E-17, -3.469127814946512892E-15 ) ) ;
#54426 = EDGE_CURVE ( 'NONE', #50839, #21538, #57758, .T. ) ;
#54427 = DIRECTION ( 'NONE',  ( -1.000000000000000000, 0.000000000000000000, -0.000000000000000000 ) ) ;
#54428 = LINE ( 'NONE', #9485, #39610 ) ;
#54429 = AXIS2_PLACEMENT_3D ( 'NONE', #44157, #39154, #19866 ) ;
#54430 = DIRECTION ( 'NONE',  ( 0.000000000000000000, -0.5767582926624851281, -0.8169148498130359703 ) ) ;
#54431 = EDGE_CURVE ( 'NONE', #8244, #31482, #8893, .T. ) ;
#54432 = CARTESIAN_POINT ( 'NONE',  ( 3.291290029914074378, 8.250315036047103590, 25.00000000000000000 ) ) ;
#54433 = ORIENTED_EDGE ( 'NONE', *, *, #52579, .F. ) ;
#54434 = DIRECTION ( 'NONE',  ( 1.000000000000000000, 0.000000000000000000, 0.000000000000000000 ) ) ;
#54435 = CARTESIAN_POINT ( 'NONE',  ( 35.00000000000000000, 12.74068829017553739, 0.4871980014161889083 ) ) ;
#54436 = EDGE_CURVE ( 'NONE', #34943, #2113, #36889, .T. ) ;
#54437 = DIRECTION ( 'NONE',  ( -1.000000000000000000, -0.000000000000000000, -0.000000000000000000 ) ) ;
#54438 = CIRCLE ( 'NONE', #25765, 12.18650000000000055 ) ;
#54439 = CARTESIAN_POINT ( 'NONE',  ( 3.618261583105314649, 8.318251859915346103, 10.63289868894575463 ) ) ;
#54440 = ORIENTED_EDGE ( 'NONE', *, *, #35495, .F. ) ;
#54441 = CARTESIAN_POINT ( 'NONE',  ( 2.288423627607476973, -2.464337058688807147, 7.242304196986142806 ) ) ;
#54442 = CARTESIAN_POINT ( 'NONE',  ( 1.452237505248552996, -0.5922625322517893753, 12.64182585313125884 ) ) ;
#54443 = CARTESIAN_POINT ( 'NONE',  ( 5.786001662380198418, -26.09353282112645189, -15.10027383179532023 ) ) ;
#54444 = VERTEX_POINT ( 'NONE', #18827 ) ;
#54445 = LINE ( 'NONE', #37827, #36591 ) ;
#54446 = CARTESIAN_POINT ( 'NONE',  ( -22.35190811654613086, 3.898012445334707365, -0.2457675311904780890 ) ) ;
#54447 = DIRECTION ( 'NONE',  ( -1.000000000000000000, 0.000000000000000000, -0.000000000000000000 ) ) ;
#54448 = EDGE_CURVE ( 'NONE', #3635, #63404, #58865, .T. ) ;
#54449 = CIRCLE ( 'NONE', #17422, 7.499999999999988454 ) ;
#54450 = AXIS2_PLACEMENT_3D ( 'NONE', #13947, #34239, #19627 ) ;
#54451 = CARTESIAN_POINT ( 'NONE',  ( 0.2676618633000448777, -7.994628339664874517, 9.277614237849251211 ) ) ;
#54452 = CARTESIAN_POINT ( 'NONE',  ( 25.00000000000000355, -28.99999999999999645, 5.000000000000000888 ) ) ;
#54453 = AXIS2_PLACEMENT_3D ( 'NONE', #65119, #11879, #41147 ) ;
#54454 = CIRCLE ( 'NONE', #1387, 12.74999999999999822 ) ;
#54455 = CARTESIAN_POINT ( 'NONE',  ( 0.4613984246114871679, 12.07219521825823527, -2.415907815801280556 ) ) ;
#54456 = ORIENTED_EDGE ( 'NONE', *, *, #10306, .T. ) ;
#54457 = FACE_OUTER_BOUND ( 'NONE', #62330, .T. ) ;
#54458 = DIRECTION ( 'NONE',  ( 0.000000000000000000, 0.9847383929261623869, -0.1740410799127578845 ) ) ;
#54459 = DIRECTION ( 'NONE',  ( 0.000000000000000000, 0.000000000000000000, 1.000000000000000000 ) ) ;
#54460 = CARTESIAN_POINT ( 'NONE',  ( -27.10719052120871098, 0.5475695427849553987, -2.295785794152566339 ) ) ;
#54461 = DIRECTION ( 'NONE',  ( 1.000000000000000000, 0.000000000000000000, 0.000000000000000000 ) ) ;
#54462 = DIRECTION ( 'NONE',  ( -1.000000000000000000, 0.000000000000000000, 0.000000000000000000 ) ) ;
#54463 = CARTESIAN_POINT ( 'NONE',  ( -26.74023318801843985, 2.752802096869884529, 1.916028097164389932 ) ) ;
#54464 = DIRECTION ( 'NONE',  ( 0.000000000000000000, -0.8989688749565110104, -0.4380125133594070519 ) ) ;
#54465 = ORIENTED_EDGE ( 'NONE', *, *, #59118, .T. ) ;
#54466 = ORIENTED_EDGE ( 'NONE', *, *, #39087, .T. ) ;
#54467 = VERTEX_POINT ( 'NONE', #8845 ) ;
#54468 = AXIS2_PLACEMENT_3D ( 'NONE', #53875, #65773, #4311 ) ;
#54469 = DIRECTION ( 'NONE',  ( 0.000000000000000000, -0.01356324068817992175, 0.9999080150203990547 ) ) ;
#54470 = CARTESIAN_POINT ( 'NONE',  ( 1.937114397841932290, 3.531416430611295620, 12.33981801388259036 ) ) ;
#54471 = ORIENTED_EDGE ( 'NONE', *, *, #5650, .T. ) ;
#54472 = DIRECTION ( 'NONE',  ( -1.000000000000000000, 0.000000000000000000, 0.000000000000000000 ) ) ;
#54473 = CARTESIAN_POINT ( 'NONE',  ( -37.00000000000000711, -12.16632754454237464, 0.7008968033238341944 ) ) ;
#54474 = CARTESIAN_POINT ( 'NONE',  ( 24.85771399857551600, 0.06729695006813952995, 13.50545047877942650 ) ) ;
#54475 = ORIENTED_EDGE ( 'NONE', *, *, #20480, .F. ) ;
#54476 = CIRCLE ( 'NONE', #60823, 6.936499999999992561 ) ;
#54477 = ORIENTED_EDGE ( 'NONE', *, *, #39224, .T. ) ;
#54478 = CARTESIAN_POINT ( 'NONE',  ( 3.152665057734040488, 0.000000000000000000, 0.000000000000000000 ) ) ;
#54479 = FACE_OUTER_BOUND ( 'NONE', #35337, .T. ) ;
#54480 = EDGE_CURVE ( 'NONE', #46064, #55188, #38781, .T. ) ;
#54481 = ORIENTED_EDGE ( 'NONE', *, *, #45906, .F. ) ;
#54482 = ORIENTED_EDGE ( 'NONE', *, *, #58278, .T. ) ;
#54483 = CARTESIAN_POINT ( 'NONE',  ( -37.00000000000000711, 0.000000000000000000, 0.000000000000000000 ) ) ;
#54484 = EDGE_CURVE ( 'NONE', #28605, #50714, #767, .T. ) ;
#54485 = CARTESIAN_POINT ( 'NONE',  ( 0.2958664285830415741, 10.50235171906349585, -6.318165763623519560 ) ) ;
#54486 = LINE ( 'NONE', #24530, #61715 ) ;
#54487 = DIRECTION ( 'NONE',  ( 0.000000000000000000, -0.01356324068817998940, 0.9999080150203990547 ) ) ;
#54488 = FACE_OUTER_BOUND ( 'NONE', #50111, .T. ) ;
#54489 = ORIENTED_EDGE ( 'NONE', *, *, #26381, .T. ) ;
#54490 = CARTESIAN_POINT ( 'NONE',  ( 2.034671305879988346, -2.716450156984129283, 11.35598636043403609 ) ) ;
#54491 = DIRECTION ( 'NONE',  ( -1.000000000000000000, 0.000000000000000000, 0.000000000000000000 ) ) ;
#54492 = CARTESIAN_POINT ( 'NONE',  ( 0.2653519991613819684, -9.395283368383228861, 7.854838327448937285 ) ) ;
#54493 = CARTESIAN_POINT ( 'NONE',  ( 2.941278708680199916, -2.952340773940147045, 5.383216837018931500 ) ) ;
#54494 = CARTESIAN_POINT ( 'NONE',  ( 29.40624810938076905, 9.599151068884586024, 7.217545767187523609 ) ) ;
#54495 = CARTESIAN_POINT ( 'NONE',  ( 0.4626703367448398718, 0.2831487465615306620, -12.30872794628584188 ) ) ;
#54496 = CARTESIAN_POINT ( 'NONE',  ( 2.717984159219702267, -4.139692542159338018, -6.602931111513714590 ) ) ;
#54497 = DIRECTION ( 'NONE',  ( 1.000000000000000000, 0.000000000000000000, 0.000000000000000000 ) ) ;
#54498 = CARTESIAN_POINT ( 'NONE',  ( 1.948354844646999817, -11.94326855455517489, 0.7204626209692002181 ) ) ;
#54499 = CIRCLE ( 'NONE', #9909, 12.74999999999999822 ) ;
#54500 = EDGE_CURVE ( 'NONE', #43254, #20748, #17085, .T. ) ;
#54501 = ORIENTED_EDGE ( 'NONE', *, *, #62641, .F. ) ;
#54502 = CARTESIAN_POINT ( 'NONE',  ( -16.08965205424928868, 8.362593759199420163, -8.606399676289541389 ) ) ;
#54503 = EDGE_CURVE ( 'NONE', #63220, #36458, #54074, .T. ) ;
#54504 = ORIENTED_EDGE ( 'NONE', *, *, #41608, .F. ) ;
#54505 = EDGE_CURVE ( 'NONE', #51431, #21573, #37570, .T. ) ;
#54506 = CARTESIAN_POINT ( 'NONE',  ( 2.990245332647743393, 7.075286609974440033, 4.676740826320128441 ) ) ;
#54507 = CARTESIAN_POINT ( 'NONE',  ( 2.242819959140646802, -7.500446639314762187, -1.426511055719384302 ) ) ;
#54508 = CARTESIAN_POINT ( 'NONE',  ( 0.3665391374699465965, 1.872534962004961834, -12.13918562134716694 ) ) ;
#54509 = CIRCLE ( 'NONE', #26865, 12.18650000000000055 ) ;
#54510 = DIRECTION ( 'NONE',  ( -1.000000000000000000, 0.000000000000000000, 0.000000000000000000 ) ) ;
#54511 = ADVANCED_FACE ( 'NONE', ( #8506 ), #33466, .T. ) ;
#54512 = CARTESIAN_POINT ( 'NONE',  ( 2.000000000000001776, 0.000000000000000000, 0.000000000000000000 ) ) ;
#54513 = ORIENTED_EDGE ( 'NONE', *, *, #56223, .F. ) ;
#54514 = CIRCLE ( 'NONE', #18453, 12.18650000000000233 ) ;
#54515 = CARTESIAN_POINT ( 'NONE',  ( 5.514970785353741078, -0.004532877335078326457, 0.001326349372336564462 ) ) ;
#54516 = DIRECTION ( 'NONE',  ( -1.000000000000000000, 0.000000000000000000, 0.000000000000000000 ) ) ;
#54517 = DIRECTION ( 'NONE',  ( 0.000000000000000000, 0.01356324068817992175, -0.9999080150203990547 ) ) ;
#54518 = DIRECTION ( 'NONE',  ( -1.000000000000000000, 0.000000000000000000, 0.000000000000000000 ) ) ;
#54519 = CIRCLE ( 'NONE', #25838, 2.899999999999996358 ) ;
#54520 = EDGE_CURVE ( 'NONE', #39152, #50397, #3215, .T. ) ;
#54521 = DIRECTION ( 'NONE',  ( -1.000000000000000000, 0.000000000000000000, 0.000000000000000000 ) ) ;
#54522 = CIRCLE ( 'NONE', #10986, 2.899999999999996358 ) ;
#54523 = ORIENTED_EDGE ( 'NONE', *, *, #8657, .T. ) ;
#54524 = EDGE_CURVE ( 'NONE', #35057, #58885, #53755, .T. ) ;
#54525 = AXIS2_PLACEMENT_3D ( 'NONE', #30577, #4698, #9989 ) ;
#54526 = DIRECTION ( 'NONE',  ( 0.000000000000000000, -0.01356324068817999114, 0.9999080150203989437 ) ) ;
#54527 = EDGE_LOOP ( 'NONE', ( #21603, #18294, #41179, #26630 ) ) ;
#54528 = CARTESIAN_POINT ( 'NONE',  ( 2.430348790456849262, 5.769383131055064950, -5.095533593439648179 ) ) ;
#54529 = DIRECTION ( 'NONE',  ( 1.000000000000000000, -0.000000000000000000, 0.000000000000000000 ) ) ;
#54530 = DIRECTION ( 'NONE',  ( 0.000000000000000000, 0.01356324068817998940, -0.9999080150203990547 ) ) ;
#54531 = CARTESIAN_POINT ( 'NONE',  ( 2.889800649504073782, -3.882893708502015429, -4.732281052280351119 ) ) ;
#54532 = VECTOR ( 'NONE', #32277, 1000.000000000000000 ) ;
#54533 = ORIENTED_EDGE ( 'NONE', *, *, #51046, .F. ) ;
#54534 = EDGE_LOOP ( 'NONE', ( #21312, #30373, #8727, #18313 ) ) ;
#54536 = EDGE_CURVE ( 'NONE', #55528, #47834, #62014, .T. ) ;
#54535 = CARTESIAN_POINT ( 'NONE',  ( 0.000000000000000000, -5.888698556700776798, 3.665823448873372747 ) ) ;
#54537 = CARTESIAN_POINT ( 'NONE',  ( 2.288423627607356625, 5.039850887180204353, 5.755330594804989097 ) ) ;
#54538 = DIRECTION ( 'NONE',  ( 1.000000000000000000, 0.000000000000000000, 0.000000000000000000 ) ) ;
#54539 = CARTESIAN_POINT ( 'NONE',  ( -37.00000000000000711, -9.700295462048607931, -7.376655759824990000 ) ) ;
#54540 = CARTESIAN_POINT ( 'NONE',  ( 1.937114397841932290, -11.72279974487460130, -5.226660192101706848 ) ) ;
#54541 = LINE ( 'NONE', #44523, #27483 ) ;
#54542 = CARTESIAN_POINT ( 'NONE',  ( 0.3675815128205912052, -12.27743992903065973, -0.2638082659429707988 ) ) ;
#54543 = ORIENTED_EDGE ( 'NONE', *, *, #18987, .T. ) ;
#54544 = AXIS2_PLACEMENT_3D ( 'NONE', #28842, #43811, #24500 ) ;
#54545 = AXIS2_PLACEMENT_3D ( 'NONE', #57994, #1143, #26403 ) ;
#54546 = ORIENTED_EDGE ( 'NONE', *, *, #41598, .F. ) ;
#54547 = ORIENTED_EDGE ( 'NONE', *, *, #63485, .T. ) ;
#54548 = CARTESIAN_POINT ( 'NONE',  ( 0.8320506296491578802, -2.535206712041371713, -12.17395768195219397 ) ) ;
#54549 = AXIS2_PLACEMENT_3D ( 'NONE', #50272, #4731, #55580 ) ;
#54551 = AXIS2_PLACEMENT_3D ( 'NONE', #4899, #65059, #5559 ) ;
#54550 = CARTESIAN_POINT ( 'NONE',  ( -37.00000000000000711, 11.29812557209476864, 3.213188559034282132 ) ) ;
#54552 = ORIENTED_EDGE ( 'NONE', *, *, #26494, .T. ) ;
#54553 = CARTESIAN_POINT ( 'NONE',  ( -37.00000000000000711, -11.96656215839366055, -4.400442035671074947 ) ) ;
#54554 = FACE_BOUND ( 'NONE', #64305, .T. ) ;
#54555 = ORIENTED_EDGE ( 'NONE', *, *, #41634, .F. ) ;
#54556 = LINE ( 'NONE', #23965, #26946 ) ;
#54557 = DIRECTION ( 'NONE',  ( 0.000000000000000000, -0.3193015301359669600, -0.9476531711828067861 ) ) ;
#54558 = CARTESIAN_POINT ( 'NONE',  ( 2.000000000000001776, 0.000000000000000000, 0.000000000000000000 ) ) ;
#54559 = ORIENTED_EDGE ( 'NONE', *, *, #46297, .T. ) ;
#54560 = AXIS2_PLACEMENT_3D ( 'NONE', #51150, #30197, #10230 ) ;
#54561 = ORIENTED_EDGE ( 'NONE', *, *, #11869, .F. ) ;
#54562 = CARTESIAN_POINT ( 'NONE',  ( -37.00000000000000711, 5.130401251914730842, 11.05394794832831629 ) ) ;
#54563 = ORIENTED_EDGE ( 'NONE', *, *, #64112, .F. ) ;
#54564 = DIRECTION ( 'NONE',  ( -0.000000000000000000, -0.000000000000000000, -1.000000000000000000 ) ) ;
#54565 = ORIENTED_EDGE ( 'NONE', *, *, #58899, .F. ) ;
#54566 = VECTOR ( 'NONE', #31109, 1000.000000000000000 ) ;
#54567 = ORIENTED_EDGE ( 'NONE', *, *, #52565, .F. ) ;
#54568 = VERTEX_POINT ( 'NONE', #12499 ) ;
#54569 = DIRECTION ( 'NONE',  ( -0.000000000000000000, -1.000000000000000000, -0.000000000000000000 ) ) ;
#54570 = AXIS2_PLACEMENT_3D ( 'NONE', #7838, #12153, #27774 ) ;
#54571 = DIRECTION ( 'NONE',  ( 0.000000000000000000, 0.8169148498130297531, -0.5767582926624940098 ) ) ;
#54572 = EDGE_CURVE ( 'NONE', #58025, #29486, #53084, .T. ) ;
#54573 = FACE_OUTER_BOUND ( 'NONE', #20670, .T. ) ;
#54574 = DIRECTION ( 'NONE',  ( 0.000000000000000000, 0.01356324068817998940, -0.9999080150203990547 ) ) ;
#54575 = DIRECTION ( 'NONE',  ( -1.000000000000000000, -1.836970198721029688E-16, 0.000000000000000000 ) ) ;
#54576 = ORIENTED_EDGE ( 'NONE', *, *, #63549, .T. ) ;
#54577 = CARTESIAN_POINT ( 'NONE',  ( 2.305787727787083519, -7.135468203929965725, -2.774453000917220802 ) ) ;
#54578 = CIRCLE ( 'NONE', #37566, 5.000000000000000888 ) ;
#54579 = EDGE_LOOP ( 'NONE', ( #60926, #13152, #573, #65589 ) ) ;
#54580 = DIRECTION ( 'NONE',  ( 0.000000000000000000, -1.000000000000000000, 0.000000000000000000 ) ) ;
#54581 = CIRCLE ( 'NONE', #56718, 7.938172270156617749 ) ;
#54582 = FACE_OUTER_BOUND ( 'NONE', #36963, .T. ) ;
#54583 = VERTEX_POINT ( 'NONE', #48117 ) ;
#54584 = EDGE_CURVE ( 'NONE', #12670, #10959, #2573, .T. ) ;
#54585 = CARTESIAN_POINT ( 'NONE',  ( -15.23449087116190093, 8.463651061413711929, 8.506858964723610583 ) ) ;
#54586 = CARTESIAN_POINT ( 'NONE',  ( 5.514970785353741078, 0.003415090918276187260, 0.003262412238248241138 ) ) ;
#54587 = DIRECTION ( 'NONE',  ( 0.000000000000000000, -0.01356324068817998940, 0.9999080150203990547 ) ) ;
#54588 = ORIENTED_EDGE ( 'NONE', *, *, #35425, .T. ) ;
#54589 = CIRCLE ( 'NONE', #25900, 5.000000000000000888 ) ;
#54590 = ADVANCED_FACE ( 'NONE', ( #35409 ), #5174, .T. ) ;
#54591 = ORIENTED_EDGE ( 'NONE', *, *, #29620, .T. ) ;
#54592 = CARTESIAN_POINT ( 'NONE',  ( -22.28506771379528573, 1.636577531579587630, -3.348518833762368807 ) ) ;
#54593 =( BOUNDED_SURFACE ( )  B_SPLINE_SURFACE ( 3, 1, ( 
 ( #46570, #40932 ),
 ( #61212, #15640 ),
 ( #20960, #61863 ),
 ( #1027, #21293 ) ),
 .UNSPECIFIED., .F., .F., .F. ) 
 B_SPLINE_SURFACE_WITH_KNOTS ( ( 4, 4 ),
 ( 2, 2 ),
 ( 0.000000000000000000, 1.000000000000000000 ),
 ( 0.000000000000000000, 1.000000000000000000 ),
 .UNSPECIFIED. ) 
 GEOMETRIC_REPRESENTATION_ITEM ( )  RATIONAL_B_SPLINE_SURFACE ( (
 ( 1.000000000000000000, 1.000000000000000000),
 ( 0.6933888150995267674, 0.9895912004443193632),
 ( 0.6933888150995267674, 0.9895912004443193632),
 ( 1.000000000000000000, 1.000000000000000000) ) ) 
 REPRESENTATION_ITEM ( '' )  SURFACE ( )  );
#54594 = ORIENTED_EDGE ( 'NONE', *, *, #34360, .F. ) ;
#54595 = EDGE_CURVE ( 'NONE', #59201, #25850, #34374, .T. ) ;
#54596 = FACE_OUTER_BOUND ( 'NONE', #19775, .T. ) ;
#54597 = CARTESIAN_POINT ( 'NONE',  ( 35.00000000000000000, -8.624332853795991127, 9.390600770288079602 ) ) ;
#54598 = CARTESIAN_POINT ( 'NONE',  ( 0.2869720083484378348, -9.251312689958709257, -8.034871682535190018 ) ) ;
#54599 = ADVANCED_FACE ( 'NONE', ( #14782 ), #49436, .T. ) ;
#54600 = CARTESIAN_POINT ( 'NONE',  ( -19.62351202312758502, -4.052328796303131142, -12.87840960595547557 ) ) ;
#54601 = VERTEX_POINT ( 'NONE', #59717 ) ;
#54602 = CIRCLE ( 'NONE', #9956, 12.18650000000000055 ) ;
#54603 = B_SPLINE_CURVE_WITH_KNOTS ( 'NONE', 3,
 ( #21558, #62114, #60803, #15240, #15561, #35822 ),
 .UNSPECIFIED., .F., .F.,
 ( 4, 2, 4 ),
 ( 0.000000000000000000, 0.0004528561986909333511, 0.0009057123973818667021 ),
 .UNSPECIFIED. ) ;
#54604 = CARTESIAN_POINT ( 'NONE',  ( 2.903928887688894012, -2.041797854846922000, -8.528865300110647141 ) ) ;
#54605 = CARTESIAN_POINT ( 'NONE',  ( -37.00000000000000711, 1.738225594539996477, 12.63095688309029718 ) ) ;
#54606 = AXIS2_PLACEMENT_3D ( 'NONE', #47641, #17720, #63910 ) ;
#54607 = CARTESIAN_POINT ( 'NONE',  ( -17.14901781563217398, -29.51442629269803319, -9.398967198486927188 ) ) ;
#54608 = CONICAL_SURFACE ( 'NONE', #39723, 7.938172270156617749, 1.280189991382167047 ) ;
#54609 = EDGE_CURVE ( 'NONE', #46591, #35774, #25801, .T. ) ;
#54610 = VECTOR ( 'NONE', #64370, 1000.000000000000000 ) ;
#54611 = CARTESIAN_POINT ( 'NONE',  ( 2.639814597422736497, -5.186391178752170816, 5.782006333156054723 ) ) ;
#54612 = PRODUCT ( 'tweezer drum assembly', 'tweezer drum assembly', '', ( #57746 ) ) ;
#54613 = ADVANCED_FACE ( 'NONE', ( #65345 ), #55373, .T. ) ;
#54614 = CARTESIAN_POINT ( 'NONE',  ( 37.00000000000000711, 4.705694406421931860E-17, -3.469127814946512892E-15 ) ) ;
#54615 = DIRECTION ( 'NONE',  ( 0.000000000000000000, 0.2355298848897446895, 0.9718671068226476528 ) ) ;
#54616 = DIRECTION ( 'NONE',  ( -0.000000000000000000, -1.000000000000000000, -0.000000000000000000 ) ) ;
#54617 = CIRCLE ( 'NONE', #25935, 5.000000000000000000 ) ;
#54618 = EDGE_CURVE ( 'NONE', #40555, #34975, #42873, .T. ) ;
#54619 = AXIS2_PLACEMENT_3D ( 'NONE', #27362, #47347, #52969 ) ;
#54620 = ORIENTED_EDGE ( 'NONE', *, *, #38646, .T. ) ;
#54621 = CARTESIAN_POINT ( 'NONE',  ( -27.08704841010922948, -1.313007237774859615, -1.888108843319753261 ) ) ;
#54622 = EDGE_CURVE ( 'NONE', #50924, #48019, #31204, .T. ) ;
#54623 = ORIENTED_EDGE ( 'NONE', *, *, #24742, .T. ) ;
#54624 = CARTESIAN_POINT ( 'NONE',  ( -35.00000000000000000, 0.000000000000000000, 0.000000000000000000 ) ) ;
#54625 = DIRECTION ( 'NONE',  ( -1.000000000000000000, 0.000000000000000000, 0.000000000000000000 ) ) ;
#54626 = CARTESIAN_POINT ( 'NONE',  ( -37.00000000000000711, 11.95840593935201390, 2.346765782874478123 ) ) ;
#54627 = AXIS2_PLACEMENT_3D ( 'NONE', #24781, #30412, #5155 ) ;
#54628 = EDGE_CURVE ( 'NONE', #38600, #27683, #39693, .T. ) ;
#54629 = CARTESIAN_POINT ( 'NONE',  ( 2.262775599887389966, -1.187656132454015578, -7.548684916005413470 ) ) ;
#54630 = ORIENTED_EDGE ( 'NONE', *, *, #12218, .F. ) ;
#54631 = ORIENTED_EDGE ( 'NONE', *, *, #44726, .T. ) ;
#54632 = ORIENTED_EDGE ( 'NONE', *, *, #45930, .F. ) ;
#54633 = CARTESIAN_POINT ( 'NONE',  ( 0.3218525148189841922, -7.695007528464951285, -9.550803867331140395 ) ) ;
#54634 = CIRCLE ( 'NONE', #5788, 12.75000000000000178 ) ;
#54635 = VERTEX_POINT ( 'NONE', #15129 ) ;
#54636 = CARTESIAN_POINT ( 'NONE',  ( 2.507146904658096975, 5.774795220010187968, 5.128007631637082397 ) ) ;
#54637 = CARTESIAN_POINT ( 'NONE',  ( 35.00000000000000000, 2.544412758415841580, -11.91791701451267471 ) ) ;
#54638 = CARTESIAN_POINT ( 'NONE',  ( 0.2706063244538052248, 10.51833723927421538, 6.275112929891649927 ) ) ;
#54639 = CARTESIAN_POINT ( 'NONE',  ( 35.00000000000000000, 4.705694406421931860E-17, -3.469127814946512892E-15 ) ) ;
#54640 = VERTEX_POINT ( 'NONE', #45078 ) ;
#54641 = CARTESIAN_POINT ( 'NONE',  ( -16.00005080000000035, 3.673940397442054445E-16, 2.999999999999995559 ) ) ;
#54642 = CARTESIAN_POINT ( 'NONE',  ( -8.761386526128427832, -27.42676914488344408, -14.81571904625959135 ) ) ;
#54643 = CARTESIAN_POINT ( 'NONE',  ( 35.00000000000000000, 11.91791701451269780, 2.544412758415707909 ) ) ;
#54645 = VERTEX_POINT ( 'NONE', #9159 ) ;
#54644 = DIRECTION ( 'NONE',  ( 1.000000000000000000, -0.000000000000000000, 0.000000000000000000 ) ) ;
#54646 = FACE_OUTER_BOUND ( 'NONE', #36281, .T. ) ;
#54647 = ORIENTED_EDGE ( 'NONE', *, *, #28978, .T. ) ;
#54648 = VECTOR ( 'NONE', #55337, 1000.000000000000000 ) ;
#54649 = CARTESIAN_POINT ( 'NONE',  ( -29.76537318338597871, -3.714251817591057492, -11.41077529405955637 ) ) ;
#54650 = ORIENTED_EDGE ( 'NONE', *, *, #63498, .F. ) ;
#54651 = CARTESIAN_POINT ( 'NONE',  ( -29.57682744818767162, 0.08430219135412277132, -12.00160382718744323 ) ) ;
#54652 = CARTESIAN_POINT ( 'NONE',  ( 0.3610902822527226053, 3.951920836718878505, -11.62472836966319178 ) ) ;
#54653 = DIRECTION ( 'NONE',  ( 0.000000000000000000, 0.7196168960969817618, 0.6943713148249616163 ) ) ;
#54654 = CYLINDRICAL_SURFACE ( 'NONE', #17372, 7.499999999999988454 ) ;
#54655 = EDGE_CURVE ( 'NONE', #23486, #31809, #34739, .T. ) ;
#54656 = CARTESIAN_POINT ( 'NONE',  ( 0.2651627923886342164, -11.53745192040745238, 4.105544202112507257 ) ) ;
#54657 = CARTESIAN_POINT ( 'NONE',  ( -6.584448747071861341, -1.675181234638447814, -13.39582994125472482 ) ) ;
#54658 = CARTESIAN_POINT ( 'NONE',  ( 0.3675815128205912052, -3.951233083390393030, -11.62724744438069635 ) ) ;
#54660 = EDGE_LOOP ( 'NONE', ( #5571, #57305, #5052, #55280 ) ) ;
#54659 = CARTESIAN_POINT ( 'NONE',  ( 11.84688083938066150, 13.39238687512208870, -1.708653298068749438 ) ) ;
#54661 = ORIENTED_EDGE ( 'NONE', *, *, #22214, .T. ) ;
#54662 = CARTESIAN_POINT ( 'NONE',  ( 37.00000000000000711, 2.772148766916279872, 11.86701198550352920 ) ) ;
#54663 = EDGE_LOOP ( 'NONE', ( #56794, #42527, #19145, #56756 ) ) ;
#54664 = ORIENTED_EDGE ( 'NONE', *, *, #64171, .F. ) ;
#54665 = EDGE_CURVE ( 'NONE', #27434, #22936, #14247, .T. ) ;
#54666 = CARTESIAN_POINT ( 'NONE',  ( -10.00000000000000178, 0.000000000000000000, 0.000000000000000000 ) ) ;
#54667 = CARTESIAN_POINT ( 'NONE',  ( 35.00000000000000000, 4.705694406421931860E-17, -3.469127814946512892E-15 ) ) ;
#54668 = CARTESIAN_POINT ( 'NONE',  ( 0.3040950598368144520, -11.43390362554250395, -4.428852722102847750 ) ) ;
#54669 = CARTESIAN_POINT ( 'NONE',  ( -22.28121537037576871, 2.114437713163361821, 3.028566507474710345 ) ) ;
#54670 = CARTESIAN_POINT ( 'NONE',  ( -22.28121537037577227, 1.565596675942166671, -3.345440028056684945 ) ) ;
#54671 = CIRCLE ( 'NONE', #61008, 5.000000000000001776 ) ;
#54672 = CARTESIAN_POINT ( 'NONE',  ( 0.3053067050349155820, 10.73055518945195352, -5.928821939311815115 ) ) ;
#54673 = LINE ( 'NONE', #4108, #40672 ) ;
#54674 = ORIENTED_EDGE ( 'NONE', *, *, #14415, .F. ) ;
#54675 = CARTESIAN_POINT ( 'NONE',  ( 2.665405856346786173, -6.944580094494293476, -6.580881457836790460 ) ) ;
#54676 = CARTESIAN_POINT ( 'NONE',  ( 37.00000000000000711, -10.63508530065518443, 4.986700593229810963 ) ) ;
#54677 = CARTESIAN_POINT ( 'NONE',  ( -17.55783715699735836, -5.649761354908354960, 12.26190536833593292 ) ) ;
#54678 = EDGE_CURVE ( 'NONE', #61909, #57845, #11543, .T. ) ;
#54679 = VERTEX_POINT ( 'NONE', #8395 ) ;
#54680 = CARTESIAN_POINT ( 'NONE',  ( 36.06679944573490104, -2.440416481716450203, -22.47657575504853256 ) ) ;
#54681 = DIRECTION ( 'NONE',  ( 0.000000000000000000, 0.01356324068817992175, -0.9999080150203990547 ) ) ;
#54682 = ORIENTED_EDGE ( 'NONE', *, *, #49496, .F. ) ;
#54683 = DIRECTION ( 'NONE',  ( 0.000000000000000000, 0.000000000000000000, -1.000000000000000000 ) ) ;
#54684 = CARTESIAN_POINT ( 'NONE',  ( 0.3675815128205894289, -12.27743992903066328, 0.2638082659427993804 ) ) ;
#54685 = PLANE ( 'NONE',  #38582 ) ;
#54686 = EDGE_CURVE ( 'NONE', #52583, #49787, #38523, .T. ) ;
#54687 = ADVANCED_FACE ( 'NONE', ( #13060 ), #13379, .T. ) ;
#54688 = FACE_OUTER_BOUND ( 'NONE', #22735, .T. ) ;
#54689 = LINE ( 'NONE', #61288, #1185 ) ;
#54690 = AXIS2_PLACEMENT_3D ( 'NONE', #59012, #38034, #38372 ) ;
#54691 = VERTEX_POINT ( 'NONE', #9050 ) ;
#54692 = CARTESIAN_POINT ( 'NONE',  ( 37.00000000000000711, 4.705694406421931860E-17, -3.469127814946512892E-15 ) ) ;
#54693 = CARTESIAN_POINT ( 'NONE',  ( 2.941278708680199916, -3.185832147968484573, 5.248410529370215016 ) ) ;
#54694 = CARTESIAN_POINT ( 'NONE',  ( -35.00000000000000000, -6.307491713049102167, 9.908974237959624176 ) ) ;
#54695 = EDGE_LOOP ( 'NONE', ( #41401, #51339, #39469, #55721 ) ) ;
#54696 = EDGE_CURVE ( 'NONE', #52407, #53488, #49626, .T. ) ;
#54697 = CARTESIAN_POINT ( 'NONE',  ( 21.48046541981384649, 13.30940734634045519, -2.295139786869221599 ) ) ;
#54698 = DIRECTION ( 'NONE',  ( 0.000000000000000000, 0.8169148498130255343, -0.5767582926624998940 ) ) ;
#54699 = ORIENTED_EDGE ( 'NONE', *, *, #7413, .F. ) ;
#54700 = AXIS2_PLACEMENT_3D ( 'NONE', #56180, #19649, #14945 ) ;
#54701 = ORIENTED_EDGE ( 'NONE', *, *, #47530, .T. ) ;
#54702 = DIRECTION ( 'NONE',  ( 0.000000000000000000, -0.01356324068817998940, 0.9999080150203990547 ) ) ;
#54703 = VECTOR ( 'NONE', #10683, 1000.000000000000000 ) ;
#54704 = ORIENTED_EDGE ( 'NONE', *, *, #14272, .T. ) ;
#54705 = CARTESIAN_POINT ( 'NONE',  ( 35.00000000000000000, -11.44858830469738109, 2.627174906297032209 ) ) ;
#54706 = CARTESIAN_POINT ( 'NONE',  ( 0.000000000000000000, 2.562706407243636075, 6.312399813420339179 ) ) ;
#54707 = LINE ( 'NONE', #9128, #6758 ) ;
#54708 = CYLINDRICAL_SURFACE ( 'NONE', #53480, 5.594511299047803199 ) ;
#54709 = CARTESIAN_POINT ( 'NONE',  ( 2.241352910868908310, 0.08337961031704246850, 7.633946224498473931 ) ) ;
#54711 = EDGE_LOOP ( 'NONE', ( #21189, #1264, #26103, #2647 ) ) ;
#54710 = CARTESIAN_POINT ( 'NONE',  ( 2.241526690369556540, -7.634439869182789273, 0.01730530154274034782 ) ) ;
#54712 = CARTESIAN_POINT ( 'NONE',  ( 0.000000000000000000, 0.000000000000000000, 0.000000000000000000 ) ) ;
#54713 = ORIENTED_EDGE ( 'NONE', *, *, #43330, .T. ) ;
#54714 = DIRECTION ( 'NONE',  ( 1.000000000000000000, 0.000000000000000000, 0.000000000000000000 ) ) ;
#54715 = ORIENTED_EDGE ( 'NONE', *, *, #396, .T. ) ;
#54716 = ORIENTED_EDGE ( 'NONE', *, *, #29617, .T. ) ;
#54717 = DIRECTION ( 'NONE',  ( -0.1699641022377680333, 0.000000000000000000, 0.9854502544271371844 ) ) ;
#54718 = CARTESIAN_POINT ( 'NONE',  ( -1.046707184715866212, -26.56309036555506253, 16.21005351936545935 ) ) ;
#54719 = CARTESIAN_POINT ( 'NONE',  ( -3.674131796199469946, 7.080541174871527232, 9.698525384827776818 ) ) ;
#54720 = CIRCLE ( 'NONE', #29222, 5.000000000000000888 ) ;
#54721 = EDGE_CURVE ( 'NONE', #22718, #42768, #38315, .T. ) ;
#54722 = DIRECTION ( 'NONE',  ( 1.000000000000000000, 0.000000000000000000, 0.000000000000000000 ) ) ;
#54723 = CARTESIAN_POINT ( 'NONE',  ( 0.3665391374699467075, -12.04754782681756176, -2.392238720110582584 ) ) ;
#54724 = DIRECTION ( 'NONE',  ( 1.000000000000000000, 0.000000000000000000, 0.000000000000000000 ) ) ;
#54725 = ORIENTED_EDGE ( 'NONE', *, *, #60717, .T. ) ;
#54726 = EDGE_CURVE ( 'NONE', #27953, #48271, #61018, .T. ) ;
#54727 = VERTEX_POINT ( 'NONE', #8731 ) ;
#54728 = CARTESIAN_POINT ( 'NONE',  ( 0.2648978790185602672, -12.03635331166813494, 2.256510822326103671 ) ) ;
#54729 = CARTESIAN_POINT ( 'NONE',  ( -25.00000000000000355, -9.999999999999998224, 1.530808498934191521E-15 ) ) ;
#54730 = ORIENTED_EDGE ( 'NONE', *, *, #62667, .T. ) ;
#54731 = EDGE_CURVE ( 'NONE', #41856, #60581, #29330, .T. ) ;
#54732 = CARTESIAN_POINT ( 'NONE',  ( -37.00000000000000711, -10.42955799785324444, 6.303578524886909840 ) ) ;
#54733 = CARTESIAN_POINT ( 'NONE',  ( 0.3218525148189821938, -10.49750909897047713, -6.342972338926902154 ) ) ;
#54734 = CARTESIAN_POINT ( 'NONE',  ( 35.00000000000000000, -0.7536123767497623360, 11.72195762423410237 ) ) ;
#54735 = CARTESIAN_POINT ( 'NONE',  ( -22.29115169517546136, 3.075985640626810014, -2.098196790595514560 ) ) ;
#54736 = CARTESIAN_POINT ( 'NONE',  ( 2.034671305879936831, -11.35598636043418885, -2.716450156984207442 ) ) ;
#54737 = DIRECTION ( 'NONE',  ( 0.000000000000000000, -0.01356324068817991828, 0.9999080150203990547 ) ) ;
#54738 = VERTEX_POINT ( 'NONE', #17730 ) ;
#54739 = VECTOR ( 'NONE', #37893, 1000.000000000000000 ) ;
#54740 = ORIENTED_EDGE ( 'NONE', *, *, #28178, .T. ) ;
#54741 = EDGE_CURVE ( 'NONE', #20276, #57966, #22769, .T. ) ;
#54742 = DIRECTION ( 'NONE',  ( 0.000000000000000000, 0.000000000000000000, 1.000000000000000000 ) ) ;
#54743 = EDGE_CURVE ( 'NONE', #40981, #35757, #45576, .T. ) ;
#54744 = DIRECTION ( 'NONE',  ( 0.000000000000000000, 0.01356324068817998940, -0.9999080150203989437 ) ) ;
#54745 = CARTESIAN_POINT ( 'NONE',  ( 35.00000000000000000, 2.527899948230813987, 12.49688848680881037 ) ) ;
#54746 = EDGE_CURVE ( 'NONE', #61504, #60604, #51273, .T. ) ;
#54747 = CIRCLE ( 'NONE', #12246, 2.899999999999994582 ) ;
#54748 = DIRECTION ( 'NONE',  ( -1.000000000000000000, 0.000000000000000000, 0.000000000000000000 ) ) ;
#54749 = CYLINDRICAL_SURFACE ( 'NONE', #29104, 12.18649999999999878 ) ;
#54750 = FACE_OUTER_BOUND ( 'NONE', #14930, .T. ) ;
#54751 = CARTESIAN_POINT ( 'NONE',  ( 2.241537034860906275, 5.851376807350209042, -4.903726641589465807 ) ) ;
#54752 = DIRECTION ( 'NONE',  ( 0.000000000000000000, -0.01356324068817992175, 0.9999080150203990547 ) ) ;
#54753 = DIRECTION ( 'NONE',  ( 1.000000000000000000, -0.000000000000000000, 0.000000000000000000 ) ) ;
#54754 = EDGE_LOOP ( 'NONE', ( #2646, #25318, #22255, #44590, #26167, #64032 ) ) ;
#54755 = CARTESIAN_POINT ( 'NONE',  ( 0.2648978790185593790, 12.08224454301448958, 1.996248716311670446 ) ) ;
#54756 = CARTESIAN_POINT ( 'NONE',  ( 0.3040950598368144520, -12.02925914197703605, -2.376091969481339827 ) ) ;
#54757 = CARTESIAN_POINT ( 'NONE',  ( 22.05617246934746589, 13.47655295422366173, -0.7978008018308921923 ) ) ;
#54758 = EDGE_CURVE ( 'NONE', #3708, #24592, #8372, .T. ) ;
#54759 = VECTOR ( 'NONE', #61848, 1000.000000000000000 ) ;
#54760 = EDGE_CURVE ( 'NONE', #57580, #56864, #40271, .T. ) ;
#54761 = CARTESIAN_POINT ( 'NONE',  ( 2.835339799623983748, -6.612744557053408023, -4.197472173747776480 ) ) ;
#54762 = CARTESIAN_POINT ( 'NONE',  ( -28.21046445815681381, -10.37508796587660598, -6.038083143907718053 ) ) ;
#54763 =( BOUNDED_SURFACE ( )  B_SPLINE_SURFACE ( 3, 1, ( 
 ( #34758, #3891 ),
 ( #35431, #30443 ),
 ( #34455, #54756 ),
 ( #24470, #30124 ) ),
 .UNSPECIFIED., .F., .F., .F. ) 
 B_SPLINE_SURFACE_WITH_KNOTS ( ( 4, 4 ),
 ( 2, 2 ),
 ( 0.000000000000000000, 1.000000000000000000 ),
 ( 0.000000000000000000, 1.000000000000000000 ),
 .UNSPECIFIED. ) 
 GEOMETRIC_REPRESENTATION_ITEM ( )  RATIONAL_B_SPLINE_SURFACE ( (
 ( 1.000000000000000000, 1.000000000000000000),
 ( 0.9942764183789327692, 0.8450855930916580938),
 ( 0.9942764183789327692, 0.8450855930916580938),
 ( 1.000000000000000000, 1.000000000000000000) ) ) 
 REPRESENTATION_ITEM ( '' )  SURFACE ( )  );
#54764 = EDGE_LOOP ( 'NONE', ( #15669, #18695, #60916, #20102 ) ) ;
#54765 = CARTESIAN_POINT ( 'NONE',  ( 2.273267844204864385, -2.472013099045079709, 7.234348261136797298 ) ) ;
#54766 = DIRECTION ( 'NONE',  ( 0.000000000000000000, -0.01356324068817992175, 0.9999080150203990547 ) ) ;
#54767 = B_SPLINE_CURVE_WITH_KNOTS ( 'NONE', 3,
 ( #37512, #47186, #1942, #21904, #11265, #63109, #31533, #7239, #62133, #6285, #53136, #1631, #7580, #958, #17572, #46506 ),
 .UNSPECIFIED., .F., .F.,
 ( 4, 3, 3, 3, 3, 4 ),
 ( 0.000000000000000000, 0.0002999043160757369070, 0.0005998071753051058795, 0.0008997092107374633427, 0.001204458948196129951, 0.001510329163477479742 ),
 .UNSPECIFIED. ) ;
#54768 = CARTESIAN_POINT ( 'NONE',  ( -7.016966734453155219, -28.45964332337148406, -10.94381053768293555 ) ) ;
#54769 = ORIENTED_EDGE ( 'NONE', *, *, #33340, .F. ) ;
#54770 = CARTESIAN_POINT ( 'NONE',  ( 0.5572780756280709680, -6.434474476007936872, 10.53376864352695996 ) ) ;
#54771 = CARTESIAN_POINT ( 'NONE',  ( 47.00000000000000711, 4.705694406421931860E-17, -3.469127814946512892E-15 ) ) ;
#54772 = DIRECTION ( 'NONE',  ( 1.000000000000000000, 0.000000000000000000, -0.000000000000000000 ) ) ;
#54773 = CARTESIAN_POINT ( 'NONE',  ( 0.2657645697724698164, -7.987126944299682840, 9.283243433323047356 ) ) ;
#54774 = FACE_OUTER_BOUND ( 'NONE', #21925, .T. ) ;
#54775 = LINE ( 'NONE', #4568, #37166 ) ;
#54776 = VERTEX_POINT ( 'NONE', #4747 ) ;
#54777 = CARTESIAN_POINT ( 'NONE',  ( -36.00000000000000711, -12.68495603654570836, -1.286231064351445630 ) ) ;
#54778 = CARTESIAN_POINT ( 'NONE',  ( -27.09252613521593744, 1.304094283669213095, 1.914180209340453409 ) ) ;
#54780 = AXIS2_PLACEMENT_3D ( 'NONE', #23850, #44108, #29454 ) ;
#54779 = CARTESIAN_POINT ( 'NONE',  ( -18.34821779656727969, 6.410806818984529087, -11.88355244879351247 ) ) ;
#54781 = CARTESIAN_POINT ( 'NONE',  ( 3.152665057734040488, 0.000000000000000000, 0.000000000000000000 ) ) ;
#54782 =( BOUNDED_SURFACE ( )  B_SPLINE_SURFACE ( 3, 1, ( 
 ( #44419, #49133 ),
 ( #34463, #3591 ),
 ( #19832, #9184 ),
 ( #44118, #29462 ) ),
 .UNSPECIFIED., .F., .F., .F. ) 
 B_SPLINE_SURFACE_WITH_KNOTS ( ( 4, 4 ),
 ( 2, 2 ),
 ( 0.000000000000000000, 1.000000000000000000 ),
 ( 0.000000000000000000, 1.000000000000000000 ),
 .UNSPECIFIED. ) 
 GEOMETRIC_REPRESENTATION_ITEM ( )  RATIONAL_B_SPLINE_SURFACE ( (
 ( 1.000000000000000000, 1.000000000000000000),
 ( 0.8716676215708681896, 0.8964445200148167814),
 ( 0.8716676215708681896, 0.8964445200148167814),
 ( 1.000000000000000000, 1.000000000000000000) ) ) 
 REPRESENTATION_ITEM ( '' )  SURFACE ( )  );
#54783 = CARTESIAN_POINT ( 'NONE',  ( 2.258463476536646031, 7.546439757228825762, -1.192666169132556186 ) ) ;
#54784 = CARTESIAN_POINT ( 'NONE',  ( 2.241449424704146764, -3.763973574060585747, 6.642105568284094375 ) ) ;
#54785 = CARTESIAN_POINT ( 'NONE',  ( 37.00000000000000711, 4.705694406421931860E-17, -3.469127814946512892E-15 ) ) ;
#54786 = CARTESIAN_POINT ( 'NONE',  ( 2.241352910868908310, 1.243507963608194045, -7.532448145350496560 ) ) ;
#54787 = ORIENTED_EDGE ( 'NONE', *, *, #43907, .T. ) ;
#54788 = VERTEX_POINT ( 'NONE', #34630 ) ;
#54789 = CARTESIAN_POINT ( 'NONE',  ( 1.719304012339819332, -8.755325027794356174, 9.242227816401850760 ) ) ;
#54790 = ORIENTED_EDGE ( 'NONE', *, *, #7328, .F. ) ;
#54791 = AXIS2_PLACEMENT_3D ( 'NONE', #52359, #2472, #1494 ) ;
#54792 = DIRECTION ( 'NONE',  ( -1.000000000000000000, 0.000000000000000000, 0.000000000000000000 ) ) ;
#54793 = CARTESIAN_POINT ( 'NONE',  ( -16.98800322446194855, 2.922502605998049674, 25.00000000000000000 ) ) ;
#54794 = ORIENTED_EDGE ( 'NONE', *, *, #31540, .T. ) ;
#54795 = DIRECTION ( 'NONE',  ( 0.000000000000000000, -0.01356324068817998940, 0.9999080150203990547 ) ) ;
#54796 = EDGE_CURVE ( 'NONE', #37474, #25513, #62302, .T. ) ;
#54797 = CARTESIAN_POINT ( 'NONE',  ( 35.00000000000000000, -11.50504120060945645, -4.018060380616356397 ) ) ;
#54798 = CARTESIAN_POINT ( 'NONE',  ( -35.00000000000000000, -10.54834585426215732, -6.102719229070786788 ) ) ;
#54799 = ORIENTED_EDGE ( 'NONE', *, *, #34524, .T. ) ;
#54800 = EDGE_LOOP ( 'NONE', ( #40291, #10772, #24603, #18083 ) ) ;
#54801 = CYLINDRICAL_SURFACE ( 'NONE', #25747, 2.899999999999994582 ) ;
#54802 = DIRECTION ( 'NONE',  ( 0.000000000000000000, -0.5987040770935736500, 0.8009703041134121904 ) ) ;
#54803 = ORIENTED_EDGE ( 'NONE', *, *, #47823, .T. ) ;
#54804 = DIRECTION ( 'NONE',  ( 0.000000000000000000, 0.01356324068817998940, -0.9999080150203990547 ) ) ;
#54805 = ORIENTED_EDGE ( 'NONE', *, *, #15145, .T. ) ;
#54806 = CARTESIAN_POINT ( 'NONE',  ( -19.62362846926598436, -4.052573403833369170, -11.29610975316521859 ) ) ;
#54807 = DIRECTION ( 'NONE',  ( -0.000000000000000000, -0.000000000000000000, -1.000000000000000000 ) ) ;
#54809 = ADVANCED_FACE ( 'NONE', ( #15654 ), #7556, .F. ) ;
#54808 = DIRECTION ( 'NONE',  ( 0.000000000000000000, 0.000000000000000000, 1.000000000000000000 ) ) ;
#54810 = CARTESIAN_POINT ( 'NONE',  ( -27.01437459610461644, 25.00000000000000000, -2.220455681983952267 ) ) ;
#54811 = CARTESIAN_POINT ( 'NONE',  ( 35.00000000000000000, -12.17626345777663310, 0.4993900848168664752 ) ) ;
#54812 = ORIENTED_EDGE ( 'NONE', *, *, #65233, .F. ) ;
#54813 = CARTESIAN_POINT ( 'NONE',  ( 37.00000000000000711, -9.076753354953932984, 8.954052073409695112 ) ) ;
#54814 = DIRECTION ( 'NONE',  ( 1.000000000000000000, 0.000000000000000000, 0.000000000000000000 ) ) ;
#54815 = DIRECTION ( 'NONE',  ( 0.000000000000000000, 0.6051742151937661296, -0.7960930657056429771 ) ) ;
#54816 = LINE ( 'NONE', #54157, #8339 ) ;
#54817 = CARTESIAN_POINT ( 'NONE',  ( 11.50502875988115115, 13.34043489419269335, -2.074406423247350695 ) ) ;
#54818 = CARTESIAN_POINT ( 'NONE',  ( -22.31328051695926007, -3.148362328073157190, 2.109671368890621679 ) ) ;
#54819 = DIRECTION ( 'NONE',  ( -0.000000000000000000, -0.000000000000000000, -1.000000000000000000 ) ) ;
#54820 = DIRECTION ( 'NONE',  ( -1.000000000000000000, 0.000000000000000000, 0.000000000000000000 ) ) ;
#54821 = DIRECTION ( 'NONE',  ( 0.000000000000000000, 0.01356324068817998940, -0.9999080150203989437 ) ) ;
#54822 = ORIENTED_EDGE ( 'NONE', *, *, #26048, .F. ) ;
#54823 = CARTESIAN_POINT ( 'NONE',  ( -15.95149727525144101, 8.394611330425535201, -8.575054620236299385 ) ) ;
#54824 = AXIS2_PLACEMENT_3D ( 'NONE', #48704, #33717, #39358 ) ;
#54825 = ORIENTED_EDGE ( 'NONE', *, *, #63479, .F. ) ;
#54826 = DIRECTION ( 'NONE',  ( 1.000000000000000000, 0.000000000000000000, 0.000000000000000000 ) ) ;
#54827 = CARTESIAN_POINT ( 'NONE',  ( 2.251139882113958546, -7.499076289418093566, -1.448366094935489734 ) ) ;
#54828 = CARTESIAN_POINT ( 'NONE',  ( 35.00000000000000000, -4.018060380616318206, 11.50504120060946533 ) ) ;
#54829 = CARTESIAN_POINT ( 'NONE',  ( 0.2651627923886298865, -12.07509237025072757, 2.039714259676136177 ) ) ;
#54830 = CARTESIAN_POINT ( 'NONE',  ( 2.298277635560276533, -6.709004959608396490, 3.682855706290112163 ) ) ;
#54831 = VERTEX_POINT ( 'NONE', #60240 ) ;
#54832 = FACE_OUTER_BOUND ( 'NONE', #34989, .T. ) ;
#54833 = CARTESIAN_POINT ( 'NONE',  ( 37.00000000000000711, -6.711949091238068377, 10.84030624090613237 ) ) ;
#54834 = CARTESIAN_POINT ( 'NONE',  ( 35.00000000000000000, -8.258652103341374229, 8.352657516904754331 ) ) ;
#54835 = CARTESIAN_POINT ( 'NONE',  ( 1.014383007554948701, 2.605923236272134069, 12.22116704270659326 ) ) ;
#54836 = EDGE_CURVE ( 'NONE', #31870, #45916, #64190, .T. ) ;
#54837 = DIRECTION ( 'NONE',  ( 0.000000000000000000, 0.9346839223284527653, -0.3554799084909000539 ) ) ;
#54838 = ORIENTED_EDGE ( 'NONE', *, *, #61695, .T. ) ;
#54839 = CARTESIAN_POINT ( 'NONE',  ( 37.00000000000000711, -2.185196060783960892, -11.54110654723648466 ) ) ;
#54840 = ORIENTED_EDGE ( 'NONE', *, *, #29247, .F. ) ;
#54841 = LINE ( 'NONE', #35529, #43952 ) ;
#54842 = FACE_OUTER_BOUND ( 'NONE', #46730, .T. ) ;
#54843 = LINE ( 'NONE', #19913, #8707 ) ;
#54844 = CARTESIAN_POINT ( 'NONE',  ( 6.806520558696398382, -6.060494548531525361, 12.06920317132890830 ) ) ;
#54845 = EDGE_CURVE ( 'NONE', #14040, #61553, #20673, .T. ) ;
#54846 = ORIENTED_EDGE ( 'NONE', *, *, #52411, .T. ) ;
#54847 = EDGE_LOOP ( 'NONE', ( #55352, #63830 ) ) ;
#54848 = CARTESIAN_POINT ( 'NONE',  ( -27.08429572838383947, 0.9410937941434112108, -2.089332284968719922 ) ) ;
#54849 = CARTESIAN_POINT ( 'NONE',  ( -35.00000000000000000, -3.033604067594665388, 12.38385022362080790 ) ) ;
#54850 = DIRECTION ( 'NONE',  ( -1.000000000000000000, 0.000000000000000000, 0.000000000000000000 ) ) ;
#54851 = DIRECTION ( 'NONE',  ( -1.000000000000000000, 0.000000000000000000, 0.000000000000000000 ) ) ;
#54852 = CARTESIAN_POINT ( 'NONE',  ( 0.3053067050349166922, 12.25734436043224918, 0.2307671807672694586 ) ) ;
#54853 = CARTESIAN_POINT ( 'NONE',  ( 37.00000000000000711, -6.917234959366766134, 9.493370459201765144 ) ) ;
#54854 = B_SPLINE_CURVE_WITH_KNOTS ( 'NONE', 3,
 ( #59790, #14530, #34810, #55114, #9543, #19874, #3942, #29834, #4602, #50147, #40134, #60432, #14853, #35142, #4923, #55452 ),
 .UNSPECIFIED., .F., .F.,
 ( 4, 3, 3, 3, 3, 4 ),
 ( 1.563658610346375187E-18, 0.0002176109881720206360, 0.0004352086762394547577, 0.0006528017811446803521, 0.0007615147961451621938, 0.0009453342004947411833 ),
 .UNSPECIFIED. ) ;
#54855 = DIRECTION ( 'NONE',  ( -1.000000000000000000, 0.000000000000000000, 0.000000000000000000 ) ) ;
#54856 = PLANE ( 'NONE',  #42416 ) ;
#54857 = ORIENTED_EDGE ( 'NONE', *, *, #19337, .F. ) ;
#54858 = EDGE_LOOP ( 'NONE', ( #45548, #17722, #13334, #24179 ) ) ;
#54859 = VERTEX_POINT ( 'NONE', #35620 ) ;
#54860 = FACE_OUTER_BOUND ( 'NONE', #40025, .T. ) ;
#54861 = CARTESIAN_POINT ( 'NONE',  ( 35.00000000000000000, 10.93004082984027825, 6.564808257521645096 ) ) ;
#54862 = ORIENTED_EDGE ( 'NONE', *, *, #12712, .F. ) ;
#54863 = FACE_BOUND ( 'NONE', #26987, .T. ) ;
#54864 = ORIENTED_EDGE ( 'NONE', *, *, #5525, .T. ) ;
#54865 = FACE_OUTER_BOUND ( 'NONE', #47296, .T. ) ;
#54866 = EDGE_CURVE ( 'NONE', #19699, #7095, #34509, .T. ) ;
#54867 = CARTESIAN_POINT ( 'NONE',  ( 5.514970785353741078, -0.003262412238248251547, 0.003415090918276177286 ) ) ;
#54868 = CARTESIAN_POINT ( 'NONE',  ( 6.849147238560869155, -8.368406977534899482, 8.611611683099951620 ) ) ;
#54869 = ORIENTED_EDGE ( 'NONE', *, *, #52496, .F. ) ;
#54870 = ORIENTED_EDGE ( 'NONE', *, *, #5740, .F. ) ;
#54871 = CYLINDRICAL_SURFACE ( 'NONE', #39549, 12.75000000000000178 ) ;
#54872 = ADVANCED_FACE ( 'NONE', ( #17322 ), #36929, .T. ) ;
#54873 = ORIENTED_EDGE ( 'NONE', *, *, #31465, .F. ) ;
#54874 = CARTESIAN_POINT ( 'NONE',  ( 35.00000000000000000, 11.81949347079746637, -2.968224442958448783 ) ) ;
#54875 = VERTEX_POINT ( 'NONE', #1044 ) ;
#54876 = ORIENTED_EDGE ( 'NONE', *, *, #45855, .F. ) ;
#54877 = ORIENTED_EDGE ( 'NONE', *, *, #46594, .T. ) ;
#54878 = CARTESIAN_POINT ( 'NONE',  ( 35.00000000000000000, -4.041347439435937439, -11.02904044024207764 ) ) ;
#54879 = CARTESIAN_POINT ( 'NONE',  ( -37.00000000000000711, -5.246972444134096136, 10.99909370905155548 ) ) ;
#54881 = ADVANCED_FACE ( 'NONE', ( #6362 ), #35509, .T. ) ;
#54880 = CARTESIAN_POINT ( 'NONE',  ( 35.00000000000000000, -12.66641127287626567, -1.457575200925504966 ) ) ;
#54882 = DIRECTION ( 'NONE',  ( -1.000000000000000000, 0.000000000000000000, 0.000000000000000000 ) ) ;
#54883 = ORIENTED_EDGE ( 'NONE', *, *, #701, .F. ) ;
#54884 = CARTESIAN_POINT ( 'NONE',  ( 2.262775599886256206, -7.131180968652209629, -2.745802076335803310 ) ) ;
#54885 = EDGE_LOOP ( 'NONE', ( #63778, #34660, #14970, #46697 ) ) ;
#54886 = CARTESIAN_POINT ( 'NONE',  ( -35.00000000000000000, -0.4353888892047496628, -11.73808581813438501 ) ) ;
#54887 = CARTESIAN_POINT ( 'NONE',  ( -35.00000000000000000, 10.30098186818257666, -5.644643009978957515 ) ) ;
#54888 = ORIENTED_EDGE ( 'NONE', *, *, #55843, .F. ) ;
#54889 = CARTESIAN_POINT ( 'NONE',  ( 0.2956976708475431703, -10.72256944221091146, 5.936640677855330672 ) ) ;
#54890 = CYLINDRICAL_SURFACE ( 'NONE', #19076, 12.75000000000000178 ) ;
#54891 = CARTESIAN_POINT ( 'NONE',  ( 2.288423627607474753, -6.704349683466392484, -3.684511167348268668 ) ) ;
#54892 = ORIENTED_EDGE ( 'NONE', *, *, #12424, .F. ) ;
#54893 = VERTEX_POINT ( 'NONE', #56577 ) ;
#54894 = CARTESIAN_POINT ( 'NONE',  ( 2.288423627607479194, -7.648392725410194437, 0.1612945702821492744 ) ) ;
#54895 = EDGE_CURVE ( 'NONE', #5144, #1474, #31259, .T. ) ;
#54896 = VERTEX_POINT ( 'NONE', #21313 ) ;
#54897 = CARTESIAN_POINT ( 'NONE',  ( -26.99479954988168018, -12.46966287028880593, 5.172898835462513389 ) ) ;
#54898 = CARTESIAN_POINT ( 'NONE',  ( 1.194176325881342704, 9.940715479868448057, 7.670099510969100365 ) ) ;
#54899 = LINE ( 'NONE', #9653, #61109 ) ;
#54900 = CARTESIAN_POINT ( 'NONE',  ( 0.3278977287071226931, -9.235688435081675252, -8.073566434006671955 ) ) ;
#54901 = DIRECTION ( 'NONE',  ( -1.000000000000000000, 0.000000000000000000, -0.000000000000000000 ) ) ;
#54902 = ORIENTED_EDGE ( 'NONE', *, *, #30160, .T. ) ;
#54903 = CARTESIAN_POINT ( 'NONE',  ( 0.000000000000000000, 0.000000000000000000, 0.000000000000000000 ) ) ;
#54904 = CIRCLE ( 'NONE', #60218, 6.936499999999990784 ) ;
#54905 = CARTESIAN_POINT ( 'NONE',  ( 0.000000000000000000, 1.018311147294260977, -6.861346417234475581 ) ) ;
#54906 = AXIS2_PLACEMENT_3D ( 'NONE', #22976, #63194, #43229 ) ;
#54907 = DIRECTION ( 'NONE',  ( -1.000000000000000000, 0.000000000000000000, 0.000000000000000000 ) ) ;
#54908 = CARTESIAN_POINT ( 'NONE',  ( -36.00000000000000711, -6.711949091238219367, 10.84030624090604356 ) ) ;
#54909 = DIRECTION ( 'NONE',  ( 0.000000000000000000, 0.01356324068817998940, -0.9999080150203990547 ) ) ;
#54910 = CARTESIAN_POINT ( 'NONE',  ( 5.536195898058073439, 0.004468797463753786288, -0.007230647766619106506 ) ) ;
#54911 = CARTESIAN_POINT ( 'NONE',  ( -35.00000000000000000, -9.240395740215685549, 7.251710744571544964 ) ) ;
#54912 = EDGE_CURVE ( 'NONE', #1959, #31052, #11659, .T. ) ;
#54913 = B_SPLINE_CURVE_WITH_KNOTS ( 'NONE', 3,
 ( #50534, #4977, #44212, #49552, #55170, #9953, #30548, #15264, #59510, #19281, #19619, #34233, #40529, #39217, #39880, #54542 ),
 .UNSPECIFIED., .F., .F.,
 ( 4, 3, 3, 3, 3, 4 ),
 ( 0.000000000000000000, 0.0002999043160757325702, 0.0005998071753050972059, 0.0008997092107374515249, 0.001204458948195627748, 0.001510329163476482276 ),
 .UNSPECIFIED. ) ;
#54914 = ORIENTED_EDGE ( 'NONE', *, *, #34410, .T. ) ;
#54915 = CARTESIAN_POINT ( 'NONE',  ( -27.08506889328344158, -1.324351020478542029, -1.872884652028469432 ) ) ;
#54916 = ORIENTED_EDGE ( 'NONE', *, *, #53545, .F. ) ;
#54917 = CARTESIAN_POINT ( 'NONE',  ( -47.00000000000000711, 0.000000000000000000, 0.000000000000000000 ) ) ;
#54918 = CARTESIAN_POINT ( 'NONE',  ( 35.00000000000000000, 4.705694406421931860E-17, -3.469127814946512892E-15 ) ) ;
#54919 = CARTESIAN_POINT ( 'NONE',  ( 0.2653519890518172830, 6.123106317427155609, 10.60551359205152089 ) ) ;
#54920 = LINE ( 'NONE', #25647, #6343 ) ;
#54921 = ORIENTED_EDGE ( 'NONE', *, *, #9009, .T. ) ;
#54922 = ORIENTED_EDGE ( 'NONE', *, *, #23262, .T. ) ;
#54923 = ORIENTED_EDGE ( 'NONE', *, *, #15601, .T. ) ;
#54924 = DIRECTION ( 'NONE',  ( -1.000000000000000000, 0.000000000000000000, 0.000000000000000000 ) ) ;
#54925 = CARTESIAN_POINT ( 'NONE',  ( -27.28563326141737733, 11.69479555401723836, -2.740829448094128207 ) ) ;
#54926 = EDGE_CURVE ( 'NONE', #19720, #24646, #56918, .T. ) ;
#54927 = B_SPLINE_CURVE_WITH_KNOTS ( 'NONE', 3,
 ( #31495, #46790, #60440, #1902, #57110, #53439, #43102, #22511, #62094, #47781, #22850, #2581, #62722, #37467, #16853, #27480 ),
 .UNSPECIFIED., .F., .F.,
 ( 4, 3, 3, 3, 3, 4 ),
 ( 3.247553071957733784E-15, 0.0002126834539179960960, 0.0004253519300366789910, 0.0006380165497224953193, 0.0007442707582429170226, 0.0009453531351412618015 ),
 .UNSPECIFIED. ) ;
#54928 = ORIENTED_EDGE ( 'NONE', *, *, #9823, .F. ) ;
#54929 = CARTESIAN_POINT ( 'NONE',  ( 35.00000000000000000, 0.4353888892050056802, 11.73808581813437080 ) ) ;
#54930 = CARTESIAN_POINT ( 'NONE',  ( 0.3057689695767478177, -9.241339546505145108, 8.055876362038318916 ) ) ;
#54931 = FACE_OUTER_BOUND ( 'NONE', #14450, .T. ) ;
#54932 = ORIENTED_EDGE ( 'NONE', *, *, #15493, .F. ) ;
#54933 = DIRECTION ( 'NONE',  ( -1.000000000000000000, -0.000000000000000000, 0.000000000000000000 ) ) ;
#54934 = EDGE_CURVE ( 'NONE', #19566, #62364, #53577, .T. ) ;
#54935 = CARTESIAN_POINT ( 'NONE',  ( 3.702144525957853816, -26.71142515285320584, -15.98786919972985920 ) ) ;
#54936 = FACE_OUTER_BOUND ( 'NONE', #5739, .T. ) ;
#54938 = ORIENTED_EDGE ( 'NONE', *, *, #54374, .F. ) ;
#54937 = CARTESIAN_POINT ( 'NONE',  ( 2.000000000000001776, 5.107597897712416568, -4.693343793638371508 ) ) ;
#54939 = DIRECTION ( 'NONE',  ( 0.000000000000000000, 1.000000000000000000, 0.000000000000000000 ) ) ;
#54940 = ADVANCED_FACE ( 'NONE', ( #1708 ), #42225, .T. ) ;
#54941 = VERTEX_POINT ( 'NONE', #32580 ) ;
#54942 = CARTESIAN_POINT ( 'NONE',  ( 0.9296196016835478471, -9.812579935705070255, 7.691217109781775640 ) ) ;
#54943 = EDGE_LOOP ( 'NONE', ( #45537, #17493, #48264, #40533 ) ) ;
#54944 = DIRECTION ( 'NONE',  ( 0.000000000000000000, -0.01356324068817998940, 0.9999080150203990547 ) ) ;
#54945 = CARTESIAN_POINT ( 'NONE',  ( 12.19958943313458022, -11.82211122194439312, -2.065116011828826093 ) ) ;
#54946 = CARTESIAN_POINT ( 'NONE',  ( 1.937114397841932290, -8.920887662793532513, 9.228205347192421470 ) ) ;
#54947 = CARTESIAN_POINT ( 'NONE',  ( 37.00000000000000711, 4.705694406421931860E-17, -3.469127814946512892E-15 ) ) ;
#54948 = DIRECTION ( 'NONE',  ( 1.000000000000000000, 0.000000000000000000, -0.000000000000000000 ) ) ;
#54949 = AXIS2_PLACEMENT_3D ( 'NONE', #46366, #16748, #21074 ) ;
#54950 = EDGE_CURVE ( 'NONE', #52686, #32582, #51604, .T. ) ;
#54951 = CARTESIAN_POINT ( 'NONE',  ( -27.09364415740216714, -0.1694361397562798854, -2.313349100776210143 ) ) ;
#54952 = DIRECTION ( 'NONE',  ( 1.000000000000000000, 0.000000000000000000, 0.000000000000000000 ) ) ;
#54954 = VERTEX_POINT ( 'NONE', #7012 ) ;
#54953 = LINE ( 'NONE', #9381, #59678 ) ;
#54955 =( BOUNDED_CURVE ( )  B_SPLINE_CURVE ( 3, ( #37228, #22267, #22618, #36911 ),
 .UNSPECIFIED., .F., .F. ) 
 B_SPLINE_CURVE_WITH_KNOTS ( ( 4, 4 ),
 ( 1.253538260309761343, 1.290660968744300696 ),
 .UNSPECIFIED. ) 
 CURVE ( )  GEOMETRIC_REPRESENTATION_ITEM ( )  RATIONAL_B_SPLINE_CURVE ( ( 1.000000000000000000, 0.9998851620069661994, 0.9998851620069661994, 1.000000000000000000 ) ) 
 REPRESENTATION_ITEM ( '' )  );
#54956 = EDGE_LOOP ( 'NONE', ( #12698, #3832, #62307, #50387 ) ) ;
#54957 = CARTESIAN_POINT ( 'NONE',  ( 12.56483561494067658, -13.26188203154483247, -2.530721474258640580 ) ) ;
#54958 = ORIENTED_EDGE ( 'NONE', *, *, #16399, .T. ) ;
#54959 = EDGE_CURVE ( 'NONE', #20105, #11073, #55956, .T. ) ;
#54960 = VERTEX_POINT ( 'NONE', #720 ) ;
#54961 = CARTESIAN_POINT ( 'NONE',  ( 22.57855258442565116, 3.026812727784649493, 13.15630665159948975 ) ) ;
#54962 = CARTESIAN_POINT ( 'NONE',  ( 2.000000000000001776, 3.155844197800107498, 6.177028383390443800 ) ) ;
#54963 = CARTESIAN_POINT ( 'NONE',  ( 22.78424990826529850, -4.691658877507586034, 11.04575192261954442 ) ) ;
#54964 = CARTESIAN_POINT ( 'NONE',  ( 0.2653519890538380555, 6.776488011961817416E-18, -12.24619734961521722 ) ) ;
#54965 = EDGE_CURVE ( 'NONE', #26733, #13869, #49369, .T. ) ;
#54966 = CARTESIAN_POINT ( 'NONE',  ( -22.27704833740210333, 1.521679877253185875, -3.351945466913922367 ) ) ;
#54967 = CARTESIAN_POINT ( 'NONE',  ( 2.276905613632199454, 7.236369456722091087, 2.469846004796125261 ) ) ;
#54968 = CARTESIAN_POINT ( 'NONE',  ( -35.00000000000000000, -10.25474254703948418, -6.584150480049660636 ) ) ;
#54969 = EDGE_CURVE ( 'NONE', #18633, #42493, #36275, .T. ) ;
#54970 = ORIENTED_EDGE ( 'NONE', *, *, #9414, .F. ) ;
#54971 = CARTESIAN_POINT ( 'NONE',  ( -41.00000000000000711, -1.694065894508600678E-18, 1.500000000000000222 ) ) ;
#54972 = EDGE_CURVE ( 'NONE', #3010, #8331, #24892, .T. ) ;
#54973 = CARTESIAN_POINT ( 'NONE',  ( 0.000000000000000000, 0.4804830611970061227, 6.919838746524539452 ) ) ;
#54974 = CARTESIAN_POINT ( 'NONE',  ( 2.000000000000001776, 6.164400007374793766, -2.900694413976553143 ) ) ;
#54975 = VERTEX_POINT ( 'NONE', #56009 ) ;
#54976 = AXIS2_PLACEMENT_3D ( 'NONE', #14934, #60181, #4339 ) ;
#54977 = AXIS2_PLACEMENT_3D ( 'NONE', #31045, #52658, #11103 ) ;
#54978 = CARTESIAN_POINT ( 'NONE',  ( 46.20808592110949320, -0.7439837506150870361, -13.26238176883679643 ) ) ;
#54979 = CARTESIAN_POINT ( 'NONE',  ( -35.04834644901396956, -0.01306875526353248884, 0.004537648929124128358 ) ) ;
#54980 = CARTESIAN_POINT ( 'NONE',  ( -49.66779747649344046, -0.06758380666729577047, -4.082965791224115293 ) ) ;
#54981 = ORIENTED_EDGE ( 'NONE', *, *, #9816, .T. ) ;
#54982 = CARTESIAN_POINT ( 'NONE',  ( 2.259830038565000976, 6.684701880279376063, -3.700395974956069090 ) ) ;
#54983 = CARTESIAN_POINT ( 'NONE',  ( 0.2646305136544065406, -11.46223899740603258, 4.312539723326095142 ) ) ;
#54984 = CARTESIAN_POINT ( 'NONE',  ( 2.745955655249697980, 2.199760390095205409, 11.80339285908471147 ) ) ;
#54985 = CIRCLE ( 'NONE', #45395, 12.75000000000000178 ) ;
#54986 = ADVANCED_FACE ( 'NONE', ( #29741 ), #10446, .T. ) ;
#54987 = EDGE_CURVE ( 'NONE', #48877, #11231, #28082, .T. ) ;
#54988 = VECTOR ( 'NONE', #14207, 1000.000000000000000 ) ;
#54989 = DIRECTION ( 'NONE',  ( 1.000000000000000000, 0.000000000000000000, 0.000000000000000000 ) ) ;
#54990 = DIRECTION ( 'NONE',  ( -1.000000000000000000, 0.000000000000000000, 0.000000000000000000 ) ) ;
#54991 = VERTEX_POINT ( 'NONE', #51036 ) ;
#54992 = CARTESIAN_POINT ( 'NONE',  ( -37.00000000000000711, 0.000000000000000000, 0.000000000000000000 ) ) ;
#54993 = CARTESIAN_POINT ( 'NONE',  ( -22.27713295444592845, 3.528329525272667411, 1.050517974988984360 ) ) ;
#54994 = FACE_OUTER_BOUND ( 'NONE', #18323, .T. ) ;
#54995 = VERTEX_POINT ( 'NONE', #20769 ) ;
#54996 = CARTESIAN_POINT ( 'NONE',  ( 22.02397509040500623, 12.24077527228601170, -5.706323397743170212 ) ) ;
#54997 = DIRECTION ( 'NONE',  ( -1.000000000000000000, -0.000000000000000000, -0.000000000000000000 ) ) ;
#54998 = VERTEX_POINT ( 'NONE', #15445 ) ;
#54999 = EDGE_CURVE ( 'NONE', #6075, #22574, #46404, .T. ) ;
#55000 = EDGE_LOOP ( 'NONE', ( #35240, #17261, #10105, #27871 ) ) ;
#55001 = EDGE_LOOP ( 'NONE', ( #14767, #10034, #43086, #35319 ) ) ;
#55002 = CARTESIAN_POINT ( 'NONE',  ( -35.05012975565874456, 0.01363945138522194150, -0.002839961651364783513 ) ) ;
#55003 = EDGE_CURVE ( 'NONE', #15374, #11147, #25105, .T. ) ;
#55004 = ORIENTED_EDGE ( 'NONE', *, *, #48722, .T. ) ;
#55005 = CARTESIAN_POINT ( 'NONE',  ( 1.198791140419046553, -12.26651935498936119, -2.686891236233052371 ) ) ;
#55006 = CARTESIAN_POINT ( 'NONE',  ( 0.2653519789438752996, 6.104019611498720188, -10.61653328464220891 ) ) ;
#55007 = CARTESIAN_POINT ( 'NONE',  ( -35.00000000000000000, 7.499679039484183463, -9.040300684349618976 ) ) ;
#55008 = CARTESIAN_POINT ( 'NONE',  ( -37.00000000000000711, 2.250029553613937416, -12.54989509947648685 ) ) ;
#55009 = CARTESIAN_POINT ( 'NONE',  ( -10.55354650058127319, -33.11426855636985778, 11.57717840647777408 ) ) ;
#55010 = DIRECTION ( 'NONE',  ( 0.000000000000000000, -0.9346839223284501008, 0.3554799084909072149 ) ) ;
#55012 = VERTEX_POINT ( 'NONE', #25761 ) ;
#55011 = CARTESIAN_POINT ( 'NONE',  ( 2.241528039335007438, -7.634443721858079179, -0.01573255094249829955 ) ) ;
#55013 = DIRECTION ( 'NONE',  ( 1.000000000000000000, -0.000000000000000000, 0.000000000000000000 ) ) ;
#55014 = ADVANCED_FACE ( 'NONE', ( #36037 ), #56336, .T. ) ;
#55015 = VERTEX_POINT ( 'NONE', #4840 ) ;
#55016 = DIRECTION ( 'NONE',  ( 0.000000000000000000, 0.9847383929261610547, -0.1740410799127649344 ) ) ;
#55017 = ORIENTED_EDGE ( 'NONE', *, *, #15821, .T. ) ;
#55018 = EDGE_LOOP ( 'NONE', ( #39621, #13212, #56166, #26529 ) ) ;
#55019 = CARTESIAN_POINT ( 'NONE',  ( -22.28073302975500525, -0.9342220484184691198, 3.572053042948124535 ) ) ;
#55020 = CARTESIAN_POINT ( 'NONE',  ( 14.79723931605636444, -33.90329588773487757, 8.884483617263549959 ) ) ;
#55021 = CIRCLE ( 'NONE', #64596, 12.18649999999999878 ) ;
#55022 = CARTESIAN_POINT ( 'NONE',  ( 2.177405672432191963, 8.997150696567555173, 6.668684901897946382 ) ) ;
#55023 = DIRECTION ( 'NONE',  ( -1.000000000000000000, 0.000000000000000000, 0.000000000000000000 ) ) ;
#55024 = CARTESIAN_POINT ( 'NONE',  ( 35.00000000000000000, -12.70128625845191728, 1.113475361586618195 ) ) ;
#55025 = CARTESIAN_POINT ( 'NONE',  ( -17.83419946441818027, -9.720786832536937538, -9.367833439828872955 ) ) ;
#55026 = ORIENTED_EDGE ( 'NONE', *, *, #7460, .T. ) ;
#55027 = AXIS2_PLACEMENT_3D ( 'NONE', #2251, #6913, #21553 ) ;
#55028 = ORIENTED_EDGE ( 'NONE', *, *, #58022, .T. ) ;
#55029 = LINE ( 'NONE', #39744, #41150 ) ;
#55030 = ORIENTED_EDGE ( 'NONE', *, *, #41402, .F. ) ;
#55031 = EDGE_CURVE ( 'NONE', #14676, #63186, #45059, .T. ) ;
#55032 = CIRCLE ( 'NONE', #52899, 12.75000000000000178 ) ;
#55033 = EDGE_CURVE ( 'NONE', #27125, #52558, #42918, .T. ) ;
#55034 = ORIENTED_EDGE ( 'NONE', *, *, #23344, .F. ) ;
#55035 = CARTESIAN_POINT ( 'NONE',  ( 2.263328370261531663, -7.499672967744978713, 1.466596409249135036 ) ) ;
#55036 = CIRCLE ( 'NONE', #60304, 5.000000000000000888 ) ;
#55037 = CARTESIAN_POINT ( 'NONE',  ( -22.27756824490284160, 0.9591204781040340022, -3.555646273932179025 ) ) ;
#55038 = CARTESIAN_POINT ( 'NONE',  ( 37.00000000000000711, 6.307491713049029336, -9.908974237959670361 ) ) ;
#55039 = ADVANCED_FACE ( 'NONE', ( #812 ), #15343, .F. ) ;
#55040 = CARTESIAN_POINT ( 'NONE',  ( -22.27715239060371744, 1.072868796692262761, -3.521735673127126098 ) ) ;
#55041 = CARTESIAN_POINT ( 'NONE',  ( 22.88594695219327235, -4.822122601967141264, 25.00000000000000000 ) ) ;
#55042 = EDGE_CURVE ( 'NONE', #53863, #1800, #65225, .T. ) ;
#55043 = DIRECTION ( 'NONE',  ( 0.000000000000000000, -0.1764146379942750087, -0.9843159429275484262 ) ) ;
#55044 = ORIENTED_EDGE ( 'NONE', *, *, #56022, .T. ) ;
#55045 = ORIENTED_EDGE ( 'NONE', *, *, #35678, .T. ) ;
#55046 = EDGE_CURVE ( 'NONE', #37865, #27549, #10135, .T. ) ;
#55047 = DIRECTION ( 'NONE',  ( -1.000000000000000000, 0.000000000000000000, 0.000000000000000000 ) ) ;
#55048 = CARTESIAN_POINT ( 'NONE',  ( 2.556980015514111582, 4.795979673457668291, -6.074557383032923141 ) ) ;
#55049 = CARTESIAN_POINT ( 'NONE',  ( 0.000000000000000000, -4.444115772890149252, 5.163689623839303522 ) ) ;
#55050 = CARTESIAN_POINT ( 'NONE',  ( -17.96927786591849241, -9.630624776632362938, -7.160636282608098924 ) ) ;
#55051 = CIRCLE ( 'NONE', #22161, 5.000000000000000888 ) ;
#55052 = DIRECTION ( 'NONE',  ( 0.000000000000000000, -0.01356324068817999114, 0.9999080150203989437 ) ) ;
#55053 = AXIS2_PLACEMENT_3D ( 'NONE', #36117, #26487, #31163 ) ;
#55054 = DIRECTION ( 'NONE',  ( -0.000000000000000000, -0.000000000000000000, -1.000000000000000000 ) ) ;
#55055 = LINE ( 'NONE', #35426, #31170 ) ;
#55056 = DIRECTION ( 'NONE',  ( 0.000000000000000000, 0.01356324068817991828, -0.9999080150203990547 ) ) ;
#55057 = CARTESIAN_POINT ( 'NONE',  ( 1.719304012338833676, 5.066286238785588480, 11.67935079956406597 ) ) ;
#55058 = ORIENTED_EDGE ( 'NONE', *, *, #5528, .T. ) ;
#55059 = CARTESIAN_POINT ( 'NONE',  ( 0.2653519890518182822, 12.06015162724940737, 2.126521162241097329 ) ) ;
#55060 = FACE_OUTER_BOUND ( 'NONE', #43715, .T. ) ;
#55061 = DIRECTION ( 'NONE',  ( 0.000000000000000000, -0.2355298848897586228, -0.9718671068226442111 ) ) ;
#55062 = ADVANCED_FACE ( 'NONE', ( #9455 ), #504, .T. ) ;
#55063 = DIRECTION ( 'NONE',  ( 0.5702167306099040767, -0.8214942970785323872, 0.000000000000000000 ) ) ;
#55064 = ADVANCED_FACE ( 'NONE', ( #31070 ), #25423, .T. ) ;
#55065 = CARTESIAN_POINT ( 'NONE',  ( 1.194176325881345591, -4.773862381874661054, -11.61285876598811129 ) ) ;
#55066 = VECTOR ( 'NONE', #5037, 1000.000000000000000 ) ;
#55067 = AXIS2_PLACEMENT_3D ( 'NONE', #38415, #8482, #58733 ) ;
#55068 = VERTEX_POINT ( 'NONE', #27707 ) ;
#55069 = CARTESIAN_POINT ( 'NONE',  ( 2.241449424704146320, 7.634218943782391520, -0.06135604983230691367 ) ) ;
#55070 = CARTESIAN_POINT ( 'NONE',  ( 2.705197763288466728, 6.601241161176674588, 4.134294772209909929 ) ) ;
#55071 = CARTESIAN_POINT ( 'NONE',  ( -5.492202615392249854, -31.64503107144835070, -13.74436444834396021 ) ) ;
#55072 = ORIENTED_EDGE ( 'NONE', *, *, #24094, .T. ) ;
#55073 = AXIS2_PLACEMENT_3D ( 'NONE', #63218, #32944, #44246 ) ;
#55074 = FACE_OUTER_BOUND ( 'NONE', #2942, .T. ) ;
#55075 = CARTESIAN_POINT ( 'NONE',  ( -35.00000000000000000, 12.08151691381195825, -4.074242145635880163 ) ) ;
#55076 = LINE ( 'NONE', #20817, #56701 ) ;
#55077 = EDGE_CURVE ( 'NONE', #13985, #22233, #9892, .T. ) ;
#55078 = AXIS2_PLACEMENT_3D ( 'NONE', #11532, #6894, #6569 ) ;
#55079 = CARTESIAN_POINT ( 'NONE',  ( 1.198791140417290624, 12.54673713002838120, 0.5160125886320254818 ) ) ;
#55080 = CARTESIAN_POINT ( 'NONE',  ( 0.3632410797595219121, -11.44577450250090145, 4.445654054452488069 ) ) ;
#55081 = CARTESIAN_POINT ( 'NONE',  ( 1.547277799341818305, 12.34637640861389940, -2.861188171560576698 ) ) ;
#55082 = VERTEX_POINT ( 'NONE', #57330 ) ;
#55083 = DIRECTION ( 'NONE',  ( 0.000000000000000000, 0.01356324068817998940, -0.9999080150203990547 ) ) ;
#55084 = CARTESIAN_POINT ( 'NONE',  ( -27.09048036756548328, 1.306202114107882339, 1.905306051557086322 ) ) ;
#55085 = DIRECTION ( 'NONE',  ( -1.000000000000000000, 0.000000000000000000, 0.000000000000000000 ) ) ;
#55086 = DIRECTION ( 'NONE',  ( 1.000000000000000000, 0.000000000000000000, 0.000000000000000000 ) ) ;
#55087 = CARTESIAN_POINT ( 'NONE',  ( -35.00000000000000000, 11.78745411414839594, 3.093009498343968211 ) ) ;
#55088 = CARTESIAN_POINT ( 'NONE',  ( 2.244591118396556340, 7.537402265771630638, 1.219892024449276802 ) ) ;
#55089 = CYLINDRICAL_SURFACE ( 'NONE', #2145, 12.74999999999999822 ) ;
#55090 = EDGE_LOOP ( 'NONE', ( #33971, #32163, #28581, #42720 ) ) ;
#55091 = ADVANCED_FACE ( 'NONE', ( #51702, #1806 ), #48014, .F. ) ;
#55092 = ORIENTED_EDGE ( 'NONE', *, *, #33652, .F. ) ;
#55093 = CARTESIAN_POINT ( 'NONE',  ( 35.00000000000000000, 4.705694406421931860E-17, -3.469127814946512892E-15 ) ) ;
#55094 = VERTEX_POINT ( 'NONE', #11752 ) ;
#55095 = EDGE_CURVE ( 'NONE', #56356, #63372, #29125, .T. ) ;
#55096 = CARTESIAN_POINT ( 'NONE',  ( 2.080613030138687147, 0.000000000000000000, -7.580821595991582562 ) ) ;
#55097 = AXIS2_PLACEMENT_3D ( 'NONE', #11632, #7293, #2336 ) ;
#55098 = CARTESIAN_POINT ( 'NONE',  ( 5.516018279890452902, -0.006629829924290984305, -0.001397286410094293998 ) ) ;
#55099 = EDGE_LOOP ( 'NONE', ( #23923, #6460, #65500, #22604 ) ) ;
#55100 = LINE ( 'NONE', #14516, #17061 ) ;
#55101 = CARTESIAN_POINT ( 'NONE',  ( -27.19357181888462094, -12.48377454417556542, 5.138615876886901468 ) ) ;
#55102 = AXIS2_PLACEMENT_3D ( 'NONE', #7431, #62972, #17437 ) ;
#55103 = CARTESIAN_POINT ( 'NONE',  ( 23.20064169955008282, 3.175852713112300663, 13.12357665716721478 ) ) ;
#55104 = ORIENTED_EDGE ( 'NONE', *, *, #3971, .F. ) ;
#55105 = VERTEX_POINT ( 'NONE', #47034 ) ;
#55106 = CARTESIAN_POINT ( 'NONE',  ( 35.00000000000000000, -7.094637218249427058, -10.59380114696467601 ) ) ;
#55107 = ORIENTED_EDGE ( 'NONE', *, *, #18318, .T. ) ;
#55108 = CARTESIAN_POINT ( 'NONE',  ( -27.08776759928964495, 0.5731512436792131071, -2.229418711698792244 ) ) ;
#55109 = ORIENTED_EDGE ( 'NONE', *, *, #18767, .T. ) ;
#55110 = CARTESIAN_POINT ( 'NONE',  ( 0.2638984909335716500, -8.023974293733243002, 9.252728947331050335 ) ) ;
#55111 = EDGE_CURVE ( 'NONE', #44528, #27612, #11127, .T. ) ;
#55113 = AXIS2_PLACEMENT_3D ( 'NONE', #23193, #57469, #43454 ) ;
#55112 = CARTESIAN_POINT ( 'NONE',  ( -4.989057617119011745, -0.9162120371760335003, 25.00000000000000000 ) ) ;
#55114 = CARTESIAN_POINT ( 'NONE',  ( 2.507146904658096087, -4.047319006787518880, 6.577532285019752401 ) ) ;
#55115 = DIRECTION ( 'NONE',  ( 0.8867529933577789070, 0.000000000000000000, -0.4622435816439414147 ) ) ;
#55116 = EDGE_CURVE ( 'NONE', #59829, #47105, #12092, .T. ) ;
#55117 = LINE ( 'NONE', #65091, #45012 ) ;
#55118 = CIRCLE ( 'NONE', #43429, 12.75000000000000178 ) ;
#55119 = ORIENTED_EDGE ( 'NONE', *, *, #22003, .F. ) ;
#55120 = CARTESIAN_POINT ( 'NONE',  ( 2.665405856346783509, -2.226920474533445216, 9.304623509366210854 ) ) ;
#55121 = CARTESIAN_POINT ( 'NONE',  ( -35.00000000000000000, 11.70009620280411688, 1.039216533672945753 ) ) ;
#55122 = ADVANCED_FACE ( 'NONE', ( #36387 ), #56696, .T. ) ;
#55123 = CARTESIAN_POINT ( 'NONE',  ( -35.00000000000000000, -12.02534193257723949, 4.237174932027182095 ) ) ;
#55124 = CARTESIAN_POINT ( 'NONE',  ( -22.27384469013076185, -2.985904959940905545, 2.154627400808026838 ) ) ;
#55125 = DIRECTION ( 'NONE',  ( -1.000000000000000000, 0.000000000000000000, 0.000000000000000000 ) ) ;
#55126 = CARTESIAN_POINT ( 'NONE',  ( -27.10113028276154878, 1.613062633976926730, -1.697941299269287940 ) ) ;
#55127 = DIRECTION ( 'NONE',  ( -1.000000000000000000, 0.000000000000000000, 0.000000000000000000 ) ) ;
#55128 = CARTESIAN_POINT ( 'NONE',  ( 12.10998784662220729, 8.443435280036798218, -8.526922110106905706 ) ) ;
#55129 = AXIS2_PLACEMENT_3D ( 'NONE', #53689, #64298, #9096 ) ;
#55130 = FACE_OUTER_BOUND ( 'NONE', #35825, .T. ) ;
#55131 = EDGE_LOOP ( 'NONE', ( #22204, #21935, #44756, #23939 ) ) ;
#55132 = CARTESIAN_POINT ( 'NONE',  ( 0.2801149460245120348, 0.1962575296605416630, 12.24954625471156788 ) ) ;
#55133 = EDGE_CURVE ( 'NONE', #22402, #3402, #55869, .T. ) ;
#55134 =( BOUNDED_SURFACE ( )  B_SPLINE_SURFACE ( 3, 1, ( 
 ( #27633, #6388 ),
 ( #26658, #47935 ),
 ( #42937, #37944 ),
 ( #1073, #33933 ) ),
 .UNSPECIFIED., .F., .F., .F. ) 
 B_SPLINE_SURFACE_WITH_KNOTS ( ( 4, 4 ),
 ( 2, 2 ),
 ( 0.000000000000000000, 1.000000000000000000 ),
 ( 0.000000000000000000, 1.000000000000000000 ),
 .UNSPECIFIED. ) 
 GEOMETRIC_REPRESENTATION_ITEM ( )  RATIONAL_B_SPLINE_SURFACE ( (
 ( 1.000000000000000000, 1.000000000000000000),
 ( 0.8716676215708681896, 0.8964445200148167814),
 ( 0.8716676215708681896, 0.8964445200148167814),
 ( 1.000000000000000000, 1.000000000000000000) ) ) 
 REPRESENTATION_ITEM ( '' )  SURFACE ( )  );
#55135 = ORIENTED_EDGE ( 'NONE', *, *, #31973, .T. ) ;
#55136 = CARTESIAN_POINT ( 'NONE',  ( -3.224836612564374594, -7.386197834073436219, 9.465828205825033592 ) ) ;
#55137 = DIRECTION ( 'NONE',  ( 0.000000000000000000, 0.01356324068817992175, -0.9999080150203990547 ) ) ;
#55138 = CARTESIAN_POINT ( 'NONE',  ( 2.241526690369556540, -4.894066724724294382, 5.859443871527027170 ) ) ;
#55139 = DIRECTION ( 'NONE',  ( 0.000000000000000000, -0.6876994588534143249, -0.7259954919231393911 ) ) ;
#55140 = DIRECTION ( 'NONE',  ( -1.000000000000000000, 0.000000000000000000, 0.000000000000000000 ) ) ;
#55141 = ORIENTED_EDGE ( 'NONE', *, *, #18415, .T. ) ;
#55142 = CARTESIAN_POINT ( 'NONE',  ( -11.31756720043940767, -8.578238994477491275, -10.42748751657815198 ) ) ;
#55143 = CARTESIAN_POINT ( 'NONE',  ( 2.781367136451822653, 2.381060477055604530, -7.442815111163104014 ) ) ;
#55144 = CARTESIAN_POINT ( 'NONE',  ( -27.08704841010891684, 2.081152044925695499, 0.9786466045353945375 ) ) ;
#55145 = CARTESIAN_POINT ( 'NONE',  ( 1.459561108992817546, 2.815016945600459675, 12.32692860927455492 ) ) ;
#55146 = CIRCLE ( 'NONE', #38195, 12.18649999999999878 ) ;
#55147 = EDGE_CURVE ( 'NONE', #3036, #51673, #17082, .T. ) ;
#55148 = DIRECTION ( 'NONE',  ( 1.000000000000000000, 0.000000000000000000, 0.000000000000000000 ) ) ;
#55149 =( BOUNDED_SURFACE ( )  B_SPLINE_SURFACE ( 3, 1, ( 
 ( #21393, #41669 ),
 ( #61962, #36682 ),
 ( #1778, #16722 ),
 ( #6432, #22040 ) ),
 .UNSPECIFIED., .F., .F., .F. ) 
 B_SPLINE_SURFACE_WITH_KNOTS ( ( 4, 4 ),
 ( 2, 2 ),
 ( 0.000000000000000000, 1.000000000000000000 ),
 ( 0.000000000000000000, 1.000000000000000000 ),
 .UNSPECIFIED. ) 
 GEOMETRIC_REPRESENTATION_ITEM ( )  RATIONAL_B_SPLINE_SURFACE ( (
 ( 1.000000000000000000, 1.000000000000000000),
 ( 0.8716676215708681896, 0.8964445200148167814),
 ( 0.8716676215708681896, 0.8964445200148167814),
 ( 1.000000000000000000, 1.000000000000000000) ) ) 
 REPRESENTATION_ITEM ( '' )  SURFACE ( )  );
#55150 = ORIENTED_EDGE ( 'NONE', *, *, #17689, .F. ) ;
#55151 = AXIS2_PLACEMENT_3D ( 'NONE', #48297, #34273, #33939 ) ;
#55152 = DIRECTION ( 'NONE',  ( 0.000000000000000000, 0.01356324068817998940, -0.9999080150203990547 ) ) ;
#55153 = ORIENTED_EDGE ( 'NONE', *, *, #19130, .T. ) ;
#55154 = CARTESIAN_POINT ( 'NONE',  ( 0.3006302518452033667, -0.2259616664571391098, -12.25587491745529967 ) ) ;
#55155 = CARTESIAN_POINT ( 'NONE',  ( -14.82142464308439322, -33.91165328791086608, 8.853132628085452538 ) ) ;
#55156 = FACE_OUTER_BOUND ( 'NONE', #26240, .T. ) ;
#55157 = CARTESIAN_POINT ( 'NONE',  ( -29.68541646480311869, -1.416020129149132334, -13.42553116244736877 ) ) ;
#55158 = CIRCLE ( 'NONE', #29703, 1.750000000000000000 ) ;
#55159 = ORIENTED_EDGE ( 'NONE', *, *, #7105, .T. ) ;
#55160 = ORIENTED_EDGE ( 'NONE', *, *, #21092, .F. ) ;
#55161 = DIRECTION ( 'NONE',  ( -1.000000000000000000, 0.000000000000000000, 0.000000000000000000 ) ) ;
#55162 = EDGE_LOOP ( 'NONE', ( #43378, #54647, #24975, #42030 ) ) ;
#55163 = CIRCLE ( 'NONE', #14793, 5.000000000000000888 ) ;
#55164 = CARTESIAN_POINT ( 'NONE',  ( 2.241352910868908754, 7.503490710578232914, 1.407733736974891681 ) ) ;
#55165 = DIRECTION ( 'NONE',  ( 1.000000000000000000, -0.000000000000000000, 0.000000000000000000 ) ) ;
#55166 = CARTESIAN_POINT ( 'NONE',  ( 5.520433897694421610, -0.009283255140285535598, 0.01186170453199870446 ) ) ;
#55167 = LINE ( 'NONE', #39215, #61932 ) ;
#55168 = CARTESIAN_POINT ( 'NONE',  ( 2.034671305879985237, -6.436604249850708115, 9.742055912616539359 ) ) ;
#55169 = DIRECTION ( 'NONE',  ( 0.000000000000000000, -0.5767582926625031137, -0.8169148498130233138 ) ) ;
#55170 = CARTESIAN_POINT ( 'NONE',  ( 1.375507693218805505, -12.60244951981748507, -0.5913006932462674392 ) ) ;
#55171 = ORIENTED_EDGE ( 'NONE', *, *, #10474, .F. ) ;
#55172 = EDGE_CURVE ( 'NONE', #1814, #37251, #49520, .T. ) ;
#55174 = ORIENTED_EDGE ( 'NONE', *, *, #57127, .T. ) ;
#55173 = CARTESIAN_POINT ( 'NONE',  ( -22.65996813707687352, -0.2230532344361122188, 4.828298130757384676 ) ) ;
#55175 = AXIS2_PLACEMENT_3D ( 'NONE', #31943, #52265, #6705 ) ;
#55176 = ORIENTED_EDGE ( 'NONE', *, *, #50916, .F. ) ;
#55177 = CARTESIAN_POINT ( 'NONE',  ( 1.283627346226853927, -2.725559306499029777, -12.28700367512553804 ) ) ;
#55178 = EDGE_CURVE ( 'NONE', #53714, #21888, #27072, .T. ) ;
#55179 = CARTESIAN_POINT ( 'NONE',  ( -37.00000000000000711, -7.608228585767650820, -10.23119532541081078 ) ) ;
#55180 = ORIENTED_EDGE ( 'NONE', *, *, #29881, .T. ) ;
#55181 = FACE_BOUND ( 'NONE', #11379, .T. ) ;
#55182 = ORIENTED_EDGE ( 'NONE', *, *, #64279, .F. ) ;
#55183 = CARTESIAN_POINT ( 'NONE',  ( 47.00000000000000711, 4.705694406421931860E-17, -3.469127814946512892E-15 ) ) ;
#55184 = DIRECTION ( 'NONE',  ( 0.000000000000000000, -0.7381862504172023165, 0.6745969609292585822 ) ) ;
#55185 = DIRECTION ( 'NONE',  ( 0.000000000000000000, 1.000000000000000000, 0.000000000000000000 ) ) ;
#55186 = CARTESIAN_POINT ( 'NONE',  ( -27.09569413923794556, -2.259195818742708806, -0.5521997980586369481 ) ) ;
#55187 = ORIENTED_EDGE ( 'NONE', *, *, #2080, .F. ) ;
#55188 = VERTEX_POINT ( 'NONE', #6798 ) ;
#55189 = DIRECTION ( 'NONE',  ( -1.000000000000000000, 0.000000000000000000, 0.000000000000000000 ) ) ;
#55190 = ORIENTED_EDGE ( 'NONE', *, *, #33567, .F. ) ;
#55191 = CARTESIAN_POINT ( 'NONE',  ( 35.00000000000000000, -5.927257550915237871, 10.64792938439761549 ) ) ;
#55192 = ORIENTED_EDGE ( 'NONE', *, *, #36342, .F. ) ;
#55193 = ORIENTED_EDGE ( 'NONE', *, *, #33043, .T. ) ;
#55194 = ORIENTED_EDGE ( 'NONE', *, *, #60871, .F. ) ;
#55195 = DIRECTION ( 'NONE',  ( 0.000000000000000000, 0.000000000000000000, 1.000000000000000000 ) ) ;
#55196 = EDGE_CURVE ( 'NONE', #53449, #6611, #39945, .T. ) ;
#55197 = CARTESIAN_POINT ( 'NONE',  ( 3.474069148988125466, -25.85800187936594341, 15.46552914816621005 ) ) ;
#55198 = AXIS2_PLACEMENT_3D ( 'NONE', #2594, #41814, #47155 ) ;
#55199 = VECTOR ( 'NONE', #11534, 1000.000000000000000 ) ;
#55200 = CARTESIAN_POINT ( 'NONE',  ( -22.71097035706202405, 4.510116093748279376, -2.118550233809386896 ) ) ;
#55201 = CARTESIAN_POINT ( 'NONE',  ( -22.59969328935896371, -2.921971394153427770, 3.618004136135737792 ) ) ;
#55202 = ORIENTED_EDGE ( 'NONE', *, *, #21731, .F. ) ;
#55203 = CARTESIAN_POINT ( 'NONE',  ( 2.251139882113693425, -2.495216312515288415, -7.218573619021111831 ) ) ;
#55204 = ORIENTED_EDGE ( 'NONE', *, *, #51882, .F. ) ;
#55205 = AXIS2_PLACEMENT_3D ( 'NONE', #17366, #11697, #47619 ) ;
#55206 = DIRECTION ( 'NONE',  ( 1.000000000000000000, 0.000000000000000000, -0.000000000000000000 ) ) ;
#55207 = B_SPLINE_CURVE_WITH_KNOTS ( 'NONE', 3,
 ( #13444, #63009, #28744, #17472, #49059, #3513, #44047, #64318, #54996, #30053, #50366, #4813, #64628, #54367, #54697, #5126, #9118, #34391 ),
 .UNSPECIFIED., .F., .F.,
 ( 4, 2, 2, 2, 2, 2, 2, 2, 4 ),
 ( 1.734723475976807094E-18, 0.001213967396161172267, 0.002427934792322344101, 0.003641902188483516368, 0.004855869584644688201, 0.006069836980805859601, 0.007283804376967032736, 0.008497771773128205003, 0.009711739169289378137 ),
 .UNSPECIFIED. ) ;
#55208 = DIRECTION ( 'NONE',  ( -1.000000000000000000, 0.000000000000000000, -0.000000000000000000 ) ) ;
#55209 = ORIENTED_EDGE ( 'NONE', *, *, #16385, .F. ) ;
#55210 = CARTESIAN_POINT ( 'NONE',  ( -27.69447987491729890, 12.79070223153173202, -4.327645566905162333 ) ) ;
#55211 = CARTESIAN_POINT ( 'NONE',  ( 0.2638984909335720941, -12.09426044257623012, -1.930290337334179984 ) ) ;
#55212 = CARTESIAN_POINT ( 'NONE',  ( 2.242418902651939661, -6.661183998167568454, -3.730710532463432649 ) ) ;
#55213 = VECTOR ( 'NONE', #63746, 1000.000000000000000 ) ;
#55214 = ADVANCED_FACE ( 'NONE', ( #31402 ), #47676, .T. ) ;
#55215 = B_SPLINE_CURVE_WITH_KNOTS ( 'NONE', 3,
 ( #22442, #42707, #32720, #53030, #27113, #1845, #63004, #37740, #7465, #27757, #48060, #2519, #22790, #15161 ),
 .UNSPECIFIED., .F., .F.,
 ( 4, 2, 2, 2, 2, 2, 4 ),
 ( 7.113556129967474992E-17, 0.002809884958117719617, 0.004214827437176541479, 0.005619769916235362907, 0.007024712395294183467, 0.008429654874353006630, 0.01123953983247064949 ),
 .UNSPECIFIED. ) ;
#55216 = ORIENTED_EDGE ( 'NONE', *, *, #39016, .T. ) ;
#55217 = FACE_OUTER_BOUND ( 'NONE', #39895, .T. ) ;
#55218 = VECTOR ( 'NONE', #48807, 1000.000000000000000 ) ;
#55219 = VERTEX_POINT ( 'NONE', #21426 ) ;
#55220 = CARTESIAN_POINT ( 'NONE',  ( 0.2915757698887297411, 10.71881693660621870, 5.940579417090813941 ) ) ;
#55221 = CARTESIAN_POINT ( 'NONE',  ( -19.88336747883694500, -13.23946304221971282, -2.721115890609613341 ) ) ;
#55222 = CARTESIAN_POINT ( 'NONE',  ( -19.56743653832047514, -30.00000000000000000, 5.000000000000000888 ) ) ;
#55223 = CARTESIAN_POINT ( 'NONE',  ( 2.245754705088263137, -3.721112460997302751, -6.667819336165746513 ) ) ;
#55224 = FACE_OUTER_BOUND ( 'NONE', #42304, .T. ) ;
#55225 = ORIENTED_EDGE ( 'NONE', *, *, #3009, .T. ) ;
#55226 = DIRECTION ( 'NONE',  ( 0.000000000000000000, -0.01356324068817998940, 0.9999080150203990547 ) ) ;
#55228 = CIRCLE ( 'NONE', #11690, 5.000000000000000888 ) ;
#55227 = CARTESIAN_POINT ( 'NONE',  ( 0.3675815128205894289, 5.910255304480596550, -10.76447900494934196 ) ) ;
#55229 = CARTESIAN_POINT ( 'NONE',  ( -35.04834644901396956, -0.006670072992075125155, 0.01211993185716846860 ) ) ;
#55230 = CARTESIAN_POINT ( 'NONE',  ( -30.01205539201145811, -3.373358488642692166, 13.07763805471449992 ) ) ;
#55231 = EDGE_CURVE ( 'NONE', #42736, #56824, #57012, .T. ) ;
#55232 = CARTESIAN_POINT ( 'NONE',  ( -15.75855542457931335, -29.13485235466247403, -10.82860303369087873 ) ) ;
#55233 = CARTESIAN_POINT ( 'NONE',  ( 3.047904605210424833, -5.398304302092578055, 5.772373816836799953 ) ) ;
#55234 = EDGE_CURVE ( 'NONE', #1325, #23499, #16131, .T. ) ;
#55235 = CARTESIAN_POINT ( 'NONE',  ( 0.9232058338315058954, 11.58467545991560144, -4.617996777200457537 ) ) ;
#55236 = CARTESIAN_POINT ( 'NONE',  ( -7.291047549687195151, -5.640864668324916842, -10.59540170654024926 ) ) ;
#55237 = FACE_OUTER_BOUND ( 'NONE', #37981, .T. ) ;
#55238 = CIRCLE ( 'NONE', #23348, 2.899999999999995026 ) ;
#55239 = AXIS2_PLACEMENT_3D ( 'NONE', #20131, #16125, #56720 ) ;
#55240 = EDGE_CURVE ( 'NONE', #37470, #57809, #13404, .T. ) ;
#55241 = AXIS2_PLACEMENT_3D ( 'NONE', #16063, #1114, #41328 ) ;
#55242 = ORIENTED_EDGE ( 'NONE', *, *, #35521, .F. ) ;
#55243 = DIRECTION ( 'NONE',  ( 0.000000000000000000, -0.9718671068226435450, 0.2355298848897615926 ) ) ;
#55244 = ORIENTED_EDGE ( 'NONE', *, *, #28603, .F. ) ;
#55245 = DIRECTION ( 'NONE',  ( 1.000000000000000000, 0.000000000000000000, 0.000000000000000000 ) ) ;
#55246 = DIRECTION ( 'NONE',  ( -1.000000000000000000, 0.000000000000000000, 0.000000000000000000 ) ) ;
#55247 = DIRECTION ( 'NONE',  ( -0.000000000000000000, -1.000000000000000000, -0.000000000000000000 ) ) ;
#55248 = LINE ( 'NONE', #49940, #1024 ) ;
#55249 = ORIENTED_EDGE ( 'NONE', *, *, #17818, .F. ) ;
#55250 = ADVANCED_FACE ( 'NONE', ( #34006 ), #34342, .T. ) ;
#55251 = ORIENTED_EDGE ( 'NONE', *, *, #62323, .F. ) ;
#55252 = EDGE_LOOP ( 'NONE', ( #40648, #50307, #11110, #2285 ) ) ;
#55253 = CARTESIAN_POINT ( 'NONE',  ( 2.994568964204215700, 3.069094401380881187, -7.263701055179695665 ) ) ;
#55254 = VECTOR ( 'NONE', #32665, 1000.000000000000000 ) ;
#55255 = CARTESIAN_POINT ( 'NONE',  ( 2.907497136250889902, 3.613027414876690546, -6.976431712756583359 ) ) ;
#55256 = ORIENTED_EDGE ( 'NONE', *, *, #58648, .F. ) ;
#55257 = FACE_OUTER_BOUND ( 'NONE', #11954, .T. ) ;
#55258 = LINE ( 'NONE', #40621, #13451 ) ;
#55259 = CIRCLE ( 'NONE', #44605, 5.000000000000000888 ) ;
#55260 = CARTESIAN_POINT ( 'NONE',  ( 35.00000000000000000, -6.584150480049477672, 10.25474254703959431 ) ) ;
#55261 = ORIENTED_EDGE ( 'NONE', *, *, #21216, .T. ) ;
#55262 = CARTESIAN_POINT ( 'NONE',  ( -3.650755842799267459, -28.29207189712390402, -13.56609188631114193 ) ) ;
#55263 = DIRECTION ( 'NONE',  ( -0.000000000000000000, -0.000000000000000000, -1.000000000000000000 ) ) ;
#55265 = ORIENTED_EDGE ( 'NONE', *, *, #29215, .T. ) ;
#55264 = CARTESIAN_POINT ( 'NONE',  ( 40.99999999999999289, -25.49182303066451993, -1.512869109757712716 ) ) ;
#55266 = DIRECTION ( 'NONE',  ( -1.000000000000000000, 0.000000000000000000, 0.000000000000000000 ) ) ;
#55267 = ORIENTED_EDGE ( 'NONE', *, *, #42042, .F. ) ;
#55268 = DIRECTION ( 'NONE',  ( 1.000000000000000000, -0.000000000000000000, 0.000000000000000000 ) ) ;
#55269 = ORIENTED_EDGE ( 'NONE', *, *, #43146, .T. ) ;
#55270 = CARTESIAN_POINT ( 'NONE',  ( -22.71097035706202760, -2.118550233809395777, -4.510116093748293586 ) ) ;
#55271 = CARTESIAN_POINT ( 'NONE',  ( 12.94129669753463041, -11.57272345498358312, -3.180035631305769606 ) ) ;
#55272 = CARTESIAN_POINT ( 'NONE',  ( -36.00000000000000711, 8.624332853796195408, -9.390600770287900190 ) ) ;
#55273 = CARTESIAN_POINT ( 'NONE',  ( 0.4613984246114886112, -6.399144685811640976, -10.51786362586221024 ) ) ;
#55274 = CARTESIAN_POINT ( 'NONE',  ( -25.15598030215514314, -10.22730567488070008, 6.279923306559322960 ) ) ;
#55275 = LINE ( 'NONE', #19395, #58013 ) ;
#55276 = CARTESIAN_POINT ( 'NONE',  ( 2.244591118396559004, 5.779440292195835660, -4.989853642775266884 ) ) ;
#55277 = CARTESIAN_POINT ( 'NONE',  ( 35.00000000000000000, -6.753013023069642351, 10.14433819232440825 ) ) ;
#55278 = CARTESIAN_POINT ( 'NONE',  ( -35.00000000000000000, -0.4353888892047496628, -11.73808581813438501 ) ) ;
#55280 = ORIENTED_EDGE ( 'NONE', *, *, #56898, .T. ) ;
#55279 = DIRECTION ( 'NONE',  ( -1.000000000000000000, 0.000000000000000000, -0.000000000000000000 ) ) ;
#55281 = AXIS2_PLACEMENT_3D ( 'NONE', #36109, #5572, #19860 ) ;
#55282 = ORIENTED_EDGE ( 'NONE', *, *, #50842, .F. ) ;
#55283 = DIRECTION ( 'NONE',  ( 0.000000000000000000, -0.6269146997508042718, -0.7790879021242460567 ) ) ;
#55284 = ORIENTED_EDGE ( 'NONE', *, *, #36174, .T. ) ;
#55285 = ORIENTED_EDGE ( 'NONE', *, *, #43244, .F. ) ;
#55286 = CARTESIAN_POINT ( 'NONE',  ( 0.3006302518452025341, 8.051021221755775059, 9.243299516615051559 ) ) ;
#55287 = DIRECTION ( 'NONE',  ( 0.000000000000000000, -0.01356324068817992001, 0.9999080150203990547 ) ) ;
#55288 = CARTESIAN_POINT ( 'NONE',  ( -22.27786964138239867, 1.536369256421363350, -3.347945419004150214 ) ) ;
#55289 = ADVANCED_FACE ( 'NONE', ( #49650 ), #28696, .T. ) ;
#55290 = CARTESIAN_POINT ( 'NONE',  ( 2.263328370259788169, 7.228205514765998707, 2.479726736365276185 ) ) ;
#55291 = VECTOR ( 'NONE', #38471, 1000.000000000000000 ) ;
#55292 = AXIS2_PLACEMENT_3D ( 'NONE', #26513, #10553, #50814 ) ;
#55293 = AXIS2_PLACEMENT_3D ( 'NONE', #8233, #7575, #3607 ) ;
#55294 = CARTESIAN_POINT ( 'NONE',  ( 35.00000000000000000, -9.821084925794620446, -7.215058775251224077 ) ) ;
#55295 = ORIENTED_EDGE ( 'NONE', *, *, #25301, .T. ) ;
#55296 = FACE_OUTER_BOUND ( 'NONE', #6428, .T. ) ;
#55297 = DIRECTION ( 'NONE',  ( 0.000000000000000000, 0.000000000000000000, 1.000000000000000000 ) ) ;
#55298 = CARTESIAN_POINT ( 'NONE',  ( 1.375507693217489891, 12.30831170622553650, 2.770709900325457831 ) ) ;
#55299 = EDGE_LOOP ( 'NONE', ( #52270, #65221, #19718, #47668 ) ) ;
#55300 = B_SPLINE_CURVE_WITH_KNOTS ( 'NONE', 3,
 ( #37268, #11032, #36940, #11998, #47918, #56590, #22296, #61893, #62868, #16352, #36624, #52896, #56930, #11349, #31619, #32280, #51932, #6374, #27292, #47586, #46935, #1396 ),
 .UNSPECIFIED., .F., .F.,
 ( 4, 2, 2, 2, 2, 2, 2, 2, 2, 2, 4 ),
 ( 8.673617379884034509E-19, 0.001199317212602414714, 0.002398634425204828561, 0.003597951637807242625, 0.004797268850409656255, 0.005396927456710863720, 0.005996586063012071185, 0.006596244669313276916, 0.007195903275614484382, 0.008395220488216890639, 0.009594537700819298631 ),
 .UNSPECIFIED. ) ;
#55301 = AXIS2_PLACEMENT_3D ( 'NONE', #49076, #59353, #3850 ) ;
#55302 = AXIS2_PLACEMENT_3D ( 'NONE', #29936, #38943, #59231 ) ;
#55303 = EDGE_CURVE ( 'NONE', #9194, #57308, #36731, .T. ) ;
#55304 = AXIS2_PLACEMENT_3D ( 'NONE', #40995, #10728, #56635 ) ;
#55305 = CIRCLE ( 'NONE', #27669, 11.99999999999998757 ) ;
#55306 = CARTESIAN_POINT ( 'NONE',  ( 46.64267184946613298, -0.6617291737840894639, 12.54075111122643804 ) ) ;
#55307 = EDGE_CURVE ( 'NONE', #35243, #21572, #27185, .T. ) ;
#55308 = AXIS2_PLACEMENT_3D ( 'NONE', #49514, #44822, #65416 ) ;
#55309 = DIRECTION ( 'NONE',  ( -0.000000000000000000, -1.000000000000000000, -0.000000000000000000 ) ) ;
#55310 = CARTESIAN_POINT ( 'NONE',  ( -35.00000000000000000, 6.584150480049696164, -10.25474254703945931 ) ) ;
#55311 = EDGE_CURVE ( 'NONE', #5064, #35179, #49487, .T. ) ;
#55312 = ORIENTED_EDGE ( 'NONE', *, *, #15454, .T. ) ;
#55313 = CARTESIAN_POINT ( 'NONE',  ( 2.247206125382829267, 6.670391186503692893, -3.717496781928021132 ) ) ;
#55314 = CARTESIAN_POINT ( 'NONE',  ( -37.00000000000000711, -12.16893194857547655, -3.805206332242601963 ) ) ;
#55315 = CARTESIAN_POINT ( 'NONE',  ( 1.959574367826918628, 1.098676416133668399, 11.95516700061986626 ) ) ;
#55316 = VECTOR ( 'NONE', #8584, 1000.000000000000000 ) ;
#55317 = ADVANCED_FACE ( 'NONE', ( #3127 ), #38342, .T. ) ;
#55318 = CARTESIAN_POINT ( 'NONE',  ( 35.00000000000000000, -10.68873102412837639, 6.950793414699901085 ) ) ;
#55319 = LINE ( 'NONE', #9761, #34059 ) ;
#55320 = AXIS2_PLACEMENT_3D ( 'NONE', #60262, #14684, #34967 ) ;
#55321 = ORIENTED_EDGE ( 'NONE', *, *, #1109, .T. ) ;
#55322 = CARTESIAN_POINT ( 'NONE',  ( 2.941278708680199916, -6.068329152486370504, -0.9331242451665616722 ) ) ;
#55323 = EDGE_CURVE ( 'NONE', #35208, #51496, #2771, .T. ) ;
#55324 = DIRECTION ( 'NONE',  ( -1.000000000000000000, 0.000000000000000000, 0.000000000000000000 ) ) ;
#55325 = CARTESIAN_POINT ( 'NONE',  ( 0.9232058338315058954, 5.905985151448303938, -10.98407661738922592 ) ) ;
#55326 = ORIENTED_EDGE ( 'NONE', *, *, #21027, .T. ) ;
#55327 = CARTESIAN_POINT ( 'NONE',  ( 9.220846792691668625, 1.923872522168136090, 13.36437008182772779 ) ) ;
#55328 = CIRCLE ( 'NONE', #63814, 12.74999999999999822 ) ;
#55329 = DIRECTION ( 'NONE',  ( 0.000000000000000000, -0.2618041379715496664, 0.9651210252299831094 ) ) ;
#55330 = ORIENTED_EDGE ( 'NONE', *, *, #47640, .F. ) ;
#55331 = ORIENTED_EDGE ( 'NONE', *, *, #4902, .F. ) ;
#55332 = ORIENTED_EDGE ( 'NONE', *, *, #24854, .T. ) ;
#55333 = VECTOR ( 'NONE', #17129, 1000.000000000000000 ) ;
#55334 = AXIS2_PLACEMENT_3D ( 'NONE', #46330, #21032, #1098 ) ;
#55335 = ORIENTED_EDGE ( 'NONE', *, *, #64334, .F. ) ;
#55336 = EDGE_CURVE ( 'NONE', #59597, #47265, #25058, .T. ) ;
#55337 = DIRECTION ( 'NONE',  ( 1.000000000000000000, 0.000000000000000000, 0.000000000000000000 ) ) ;
#55338 = CARTESIAN_POINT ( 'NONE',  ( 0.2648978790185619880, 6.008231198269132989, -10.67083876753485328 ) ) ;
#55339 = CARTESIAN_POINT ( 'NONE',  ( -41.00000000000000711, -25.03188948156373783, 4.499999999999997335 ) ) ;
#55340 = CARTESIAN_POINT ( 'NONE',  ( 0.2653519991613827456, 4.209134909048904305, -11.50013121838203745 ) ) ;
#55341 =( BOUNDED_CURVE ( )  B_SPLINE_CURVE ( 3, ( #4236, #3614, #39465, #8558 ),
 .UNSPECIFIED., .F., .F. ) 
 B_SPLINE_CURVE_WITH_KNOTS ( ( 4, 4 ),
 ( 5.469309591143874272, 5.496147290052819656 ),
 .UNSPECIFIED. ) 
 CURVE ( )  GEOMETRIC_REPRESENTATION_ITEM ( )  RATIONAL_B_SPLINE_CURVE ( ( 1.000000000000000000, 0.9999399790604226457, 0.9999399790604226457, 1.000000000000000000 ) ) 
 REPRESENTATION_ITEM ( '' )  );
#55342 = AXIS2_PLACEMENT_3D ( 'NONE', #17439, #46381, #62975 ) ;
#55344 = EDGE_CURVE ( 'NONE', #31156, #8369, #71, .T. ) ;
#55343 = CARTESIAN_POINT ( 'NONE',  ( -18.91767133624980701, -28.94173879345719058, 6.680047468371234309 ) ) ;
#55345 = CARTESIAN_POINT ( 'NONE',  ( 24.71169205770840094, -2.101182526020552999, -13.33689344900551887 ) ) ;
#55347 = VERTEX_POINT ( 'NONE', #10697 ) ;
#55346 = CARTESIAN_POINT ( 'NONE',  ( 2.241449424704146764, -7.634218943782393296, 0.06135604983225357439 ) ) ;
#55348 = CARTESIAN_POINT ( 'NONE',  ( 35.00000000000000000, -3.033604067594490417, 12.38385022362084520 ) ) ;
#55349 = ORIENTED_EDGE ( 'NONE', *, *, #53131, .F. ) ;
#55350 = CARTESIAN_POINT ( 'NONE',  ( -20.79170840334646542, 25.00000000000000000, -3.921648409140116698 ) ) ;
#55351 = ORIENTED_EDGE ( 'NONE', *, *, #61600, .T. ) ;
#55352 = ORIENTED_EDGE ( 'NONE', *, *, #28482, .F. ) ;
#55353 = CARTESIAN_POINT ( 'NONE',  ( -37.00000000000000711, -8.927548052240958043, 8.295159312811820840 ) ) ;
#55354 = VECTOR ( 'NONE', #60251, 1000.000000000000000 ) ;
#55355 = CARTESIAN_POINT ( 'NONE',  ( 11.12775972613914099, -27.93149659178545008, 13.86083901436676591 ) ) ;
#55356 = FACE_OUTER_BOUND ( 'NONE', #16991, .T. ) ;
#55357 = DIRECTION ( 'NONE',  ( 1.000000000000000000, 0.000000000000000000, 0.000000000000000000 ) ) ;
#55358 = CARTESIAN_POINT ( 'NONE',  ( 1.462291587748811850, -2.816455204775985433, 12.32753368892814905 ) ) ;
#55359 = CARTESIAN_POINT ( 'NONE',  ( 2.269879328255102635, 5.949827370242536162, 4.798845682294834880 ) ) ;
#55360 = ORIENTED_EDGE ( 'NONE', *, *, #48366, .F. ) ;
#55361 = ORIENTED_EDGE ( 'NONE', *, *, #54845, .T. ) ;
#55362 = DIRECTION ( 'NONE',  ( 0.000000000000000000, -0.2618041379715496664, 0.9651210252299831094 ) ) ;
#55363 = VERTEX_POINT ( 'NONE', #4429 ) ;
#55364 = CIRCLE ( 'NONE', #64883, 7.499999999999988454 ) ;
#55365 = ORIENTED_EDGE ( 'NONE', *, *, #13241, .F. ) ;
#55366 = AXIS2_PLACEMENT_3D ( 'NONE', #30808, #593, #16536 ) ;
#55367 = CARTESIAN_POINT ( 'NONE',  ( 2.000000000000001776, 0.000000000000000000, 0.000000000000000000 ) ) ;
#55368 = CARTESIAN_POINT ( 'NONE',  ( 35.00000000000000000, 4.705694406421931860E-17, -3.469127814946512892E-15 ) ) ;
#55369 = FACE_OUTER_BOUND ( 'NONE', #25916, .T. ) ;
#55370 = DIRECTION ( 'NONE',  ( -1.000000000000000000, 0.000000000000000000, 0.000000000000000000 ) ) ;
#55371 = ADVANCED_FACE ( 'NONE', ( #60590 ), #25032, .T. ) ;
#55372 = DIRECTION ( 'NONE',  ( -0.000000000000000000, -0.000000000000000000, -1.000000000000000000 ) ) ;
#55373 = CYLINDRICAL_SURFACE ( 'NONE', #41827, 5.000000000000000888 ) ;
#55374 = VECTOR ( 'NONE', #8915, 1000.000000000000000 ) ;
#55375 = VERTEX_POINT ( 'NONE', #34970 ) ;
#55376 = ORIENTED_EDGE ( 'NONE', *, *, #50377, .T. ) ;
#55377 = AXIS2_PLACEMENT_3D ( 'NONE', #24685, #65243, #19711 ) ;
#55378 = CIRCLE ( 'NONE', #13984, 5.000000000000000000 ) ;
#55379 = DIRECTION ( 'NONE',  ( -1.000000000000000000, 0.000000000000000000, -0.000000000000000000 ) ) ;
#55380 = CARTESIAN_POINT ( 'NONE',  ( 2.263328370261526779, 7.499672967744992036, -1.466596409249078636 ) ) ;
#55381 = EDGE_CURVE ( 'NONE', #11936, #18330, #11240, .T. ) ;
#55382 = CARTESIAN_POINT ( 'NONE',  ( 0.000000000000000000, 0.000000000000000000, 0.000000000000000000 ) ) ;
#55383 = AXIS2_PLACEMENT_3D ( 'NONE', #49854, #35189, #45500 ) ;
#55384 = CARTESIAN_POINT ( 'NONE',  ( 37.00000000000000711, 4.705694406421931860E-17, -3.469127814946512892E-15 ) ) ;
#55385 = EDGE_CURVE ( 'NONE', #16289, #63348, #60265, .T. ) ;
#55386 = CARTESIAN_POINT ( 'NONE',  ( -28.66013792860432119, -1.826836065344825233, 0.1826938850344062559 ) ) ;
#55387 = DIRECTION ( 'NONE',  ( 0.000000000000000000, -0.01356324068817999114, 0.9999080150203989437 ) ) ;
#55388 = CARTESIAN_POINT ( 'NONE',  ( 2.000000000000001776, 3.786546189469178092, 5.663561025469147303 ) ) ;
#55389 = CARTESIAN_POINT ( 'NONE',  ( 11.74548640120467979, 25.00000000000000000, -8.184666801472349817 ) ) ;
#55390 = EDGE_CURVE ( 'NONE', #31183, #47524, #5080, .T. ) ;
#55391 = VERTEX_POINT ( 'NONE', #15675 ) ;
#55392 = CARTESIAN_POINT ( 'NONE',  ( 2.440552418640498100, -0.1974238147509794761, 7.698292014589399379 ) ) ;
#55393 = FACE_OUTER_BOUND ( 'NONE', #6552, .T. ) ;
#55394 = CARTESIAN_POINT ( 'NONE',  ( 2.406456491625670324, -7.176027849161538796, -7.573451137023475610 ) ) ;
#55395 = AXIS2_PLACEMENT_3D ( 'NONE', #18154, #28135, #7175 ) ;
#55396 = CIRCLE ( 'NONE', #40537, 7.499999999999988454 ) ;
#55397 = AXIS2_PLACEMENT_3D ( 'NONE', #13587, #44187, #61117 ) ;
#55398 = FACE_OUTER_BOUND ( 'NONE', #38944, .T. ) ;
#55399 = DIRECTION ( 'NONE',  ( 1.000000000000000000, 0.000000000000000000, 0.000000000000000000 ) ) ;
#55400 = ORIENTED_EDGE ( 'NONE', *, *, #43608, .T. ) ;
#55401 = DIRECTION ( 'NONE',  ( -0.000000000000000000, -1.000000000000000000, -0.000000000000000000 ) ) ;
#55402 = EDGE_CURVE ( 'NONE', #26919, #13695, #16564, .T. ) ;
#55403 = VECTOR ( 'NONE', #60021, 1000.000000000000000 ) ;
#55404 = CARTESIAN_POINT ( 'NONE',  ( 13.74768401152558894, -27.65692779101644305, -12.04119239038937117 ) ) ;
#55405 = VERTEX_POINT ( 'NONE', #20357 ) ;
#55406 = DIRECTION ( 'NONE',  ( 1.000000000000000000, -0.000000000000000000, 0.000000000000000000 ) ) ;
#55407 = DIRECTION ( 'NONE',  ( 1.000000000000000000, -0.000000000000000000, 0.000000000000000000 ) ) ;
#55408 = CARTESIAN_POINT ( 'NONE',  ( 2.000000000000001776, 5.450255447309745982, 4.087611905901426645 ) ) ;
#55409 = EDGE_CURVE ( 'NONE', #36164, #36570, #55275, .T. ) ;
#55410 = AXIS2_PLACEMENT_3D ( 'NONE', #23083, #48687, #6817 ) ;
#55412 = ORIENTED_EDGE ( 'NONE', *, *, #21092, .T. ) ;
#55411 = CARTESIAN_POINT ( 'NONE',  ( 0.3160775863651050233, -8.065044686487370384, 9.237902461149218425 ) ) ;
#55413 = CARTESIAN_POINT ( 'NONE',  ( -9.732421658388632935, -11.42231192723528999, -7.206575063207262488 ) ) ;
#55414 = ADVANCED_FACE ( 'NONE', ( #65259 ), #59960, .T. ) ;
#55415 = DIRECTION ( 'NONE',  ( 1.000000000000000000, 0.000000000000000000, 0.000000000000000000 ) ) ;
#55416 = EDGE_CURVE ( 'NONE', #7383, #1422, #40750, .T. ) ;
#55417 = ORIENTED_EDGE ( 'NONE', *, *, #31723, .T. ) ;
#55418 = ADVANCED_FACE ( 'NONE', ( #34652 ), #44979, .T. ) ;
#55419 = CARTESIAN_POINT ( 'NONE',  ( 0.3218525148189815277, 7.695007528465018787, 9.550803867331095987 ) ) ;
#55420 = AXIS2_PLACEMENT_3D ( 'NONE', #44995, #20634, #681 ) ;
#55421 = CARTESIAN_POINT ( 'NONE',  ( -27.09729107899804745, 1.302895495070948151, 1.932259710106483341 ) ) ;
#55422 = CARTESIAN_POINT ( 'NONE',  ( -15.49709305134071791, 8.465732809859909835, -10.51591234632406113 ) ) ;
#55423 = DIRECTION ( 'NONE',  ( 0.000000000000000000, -0.1740410799127685426, -0.9847383929261604996 ) ) ;
#55424 = DIRECTION ( 'NONE',  ( -1.000000000000000000, 0.000000000000000000, 0.000000000000000000 ) ) ;
#55425 = EDGE_CURVE ( 'NONE', #46122, #27103, #29317, .T. ) ;
#55426 = FACE_OUTER_BOUND ( 'NONE', #31065, .T. ) ;
#55427 = CYLINDRICAL_SURFACE ( 'NONE', #23364, 5.683183579532407492 ) ;
#55428 = VERTEX_POINT ( 'NONE', #738 ) ;
#55429 = CARTESIAN_POINT ( 'NONE',  ( 2.305787727787084407, -5.047606869483094449, 5.756228004061441084 ) ) ;
#55430 = EDGE_LOOP ( 'NONE', ( #28559, #53342, #32848, #24150 ) ) ;
#55431 =( NAMED_UNIT ( * ) SI_UNIT ( $, .STERADIAN. ) SOLID_ANGLE_UNIT ( ) );
#55433 = DIRECTION ( 'NONE',  ( -1.000000000000000000, 0.000000000000000000, 0.000000000000000000 ) ) ;
#55432 = AXIS2_PLACEMENT_3D ( 'NONE', #8545, #44431, #35102 ) ;
#55434 = VECTOR ( 'NONE', #35485, 1000.000000000000000 ) ;
#55435 = CIRCLE ( 'NONE', #7647, 5.000000000000000000 ) ;
#55436 = CARTESIAN_POINT ( 'NONE',  ( 0.000000000000000000, -5.585096664091900642, -4.113602740025990911 ) ) ;
#55437 = ORIENTED_EDGE ( 'NONE', *, *, #31018, .T. ) ;
#55438 = FACE_OUTER_BOUND ( 'NONE', #31894, .T. ) ;
#55439 = CARTESIAN_POINT ( 'NONE',  ( 11.80992030851978747, 11.76240988603115767, -2.380505417832655457 ) ) ;
#55440 = CARTESIAN_POINT ( 'NONE',  ( 24.17956874138577916, -3.375310251640146308, 13.07616833750467045 ) ) ;
#55441 = EDGE_LOOP ( 'NONE', ( #12552, #64590, #41804, #11597 ) ) ;
#55442 = ORIENTED_EDGE ( 'NONE', *, *, #65634, .F. ) ;
#55443 = CARTESIAN_POINT ( 'NONE',  ( 2.899286259009685285, 0.3564726075924497528, -7.845618522360449099 ) ) ;
#55444 = ORIENTED_EDGE ( 'NONE', *, *, #39553, .F. ) ;
#55445 = CARTESIAN_POINT ( 'NONE',  ( -27.09833916700227263, 0.5492787772350139486, -2.268067253344199230 ) ) ;
#55446 = VERTEX_POINT ( 'NONE', #41280 ) ;
#55447 = CIRCLE ( 'NONE', #19343, 2.899999999999996358 ) ;
#55448 = CARTESIAN_POINT ( 'NONE',  ( 2.080613030138688480, 3.872983346207417021, -1.000000000000000000 ) ) ;
#55449 = CARTESIAN_POINT ( 'NONE',  ( 2.241352910868908754, -4.843133558968088614, -5.901537464758503937 ) ) ;
#55450 = AXIS2_PLACEMENT_3D ( 'NONE', #26452, #1198, #51089 ) ;
#55451 = ADVANCED_FACE ( 'NONE', ( #6719 ), #32290, .T. ) ;
#55452 = CARTESIAN_POINT ( 'NONE',  ( 3.152665057734127974, -4.377619405892426485, 6.622010822086644488 ) ) ;
#55453 = CARTESIAN_POINT ( 'NONE',  ( 0.2653141617321027046, -10.62747662594935072, 6.084921229689382649 ) ) ;
#55454 = CARTESIAN_POINT ( 'NONE',  ( 35.00000000000000000, 12.42372387097886310, 2.865935305911484932 ) ) ;
#55455 = ORIENTED_EDGE ( 'NONE', *, *, #1904, .T. ) ;
#55456 = CARTESIAN_POINT ( 'NONE',  ( 1.109979610370754655, -11.92772269523372231, 3.830786822172774109 ) ) ;
#55457 = CIRCLE ( 'NONE', #34183, 12.75000000000000178 ) ;
#55458 = CARTESIAN_POINT ( 'NONE',  ( 2.440552418640497656, 4.020120046181139273, -6.568204543009788843 ) ) ;
#55459 = CARTESIAN_POINT ( 'NONE',  ( -36.00000000000000711, 5.865551165831237590, -11.32068061209289134 ) ) ;
#55460 = CARTESIAN_POINT ( 'NONE',  ( 12.18790794593922655, 11.12778131062980336, -7.651757715589151410 ) ) ;
#55461 = CARTESIAN_POINT ( 'NONE',  ( -37.00000000000000711, 0.000000000000000000, 0.000000000000000000 ) ) ;
#55462 = CARTESIAN_POINT ( 'NONE',  ( 2.000000000000001776, 6.812627895098307462, 2.855765430652717818 ) ) ;
#55463 = CARTESIAN_POINT ( 'NONE',  ( 37.00000000000000711, 0.6593684648220483613, -12.73293890771483738 ) ) ;
#55464 = ADVANCED_FACE ( 'NONE', ( #6383 ), #14346, .F. ) ;
#55465 = CARTESIAN_POINT ( 'NONE',  ( 37.00000000000000711, 11.37311665002363270, 2.936739658819908616 ) ) ;
#55466 = ORIENTED_EDGE ( 'NONE', *, *, #41882, .T. ) ;
#55467 = CARTESIAN_POINT ( 'NONE',  ( -37.00000000000000711, -1.030638227056651424, 12.14284015767849567 ) ) ;
#55468 = AXIS2_PLACEMENT_3D ( 'NONE', #5929, #14860, #45808 ) ;
#55469 = ORIENTED_EDGE ( 'NONE', *, *, #9535, .F. ) ;
#55470 = CARTESIAN_POINT ( 'NONE',  ( -2.960381377298834327, -6.422849866723894685, 10.16751138944930588 ) ) ;
#55471 = DIRECTION ( 'NONE',  ( 1.000000000000000000, 0.000000000000000000, 0.000000000000000000 ) ) ;
#55472 = CARTESIAN_POINT ( 'NONE',  ( -35.00000000000000000, 4.426194442447240363, 11.35427606708807957 ) ) ;
#55473 = CYLINDRICAL_SURFACE ( 'NONE', #54340, 5.000000000000000888 ) ;
#55474 = DIRECTION ( 'NONE',  ( 0.000000000000000000, 0.04924826701373889726, 0.9987865678893281807 ) ) ;
#55475 = EDGE_CURVE ( 'NONE', #18023, #3400, #22975, .T. ) ;
#55476 = ORIENTED_EDGE ( 'NONE', *, *, #62816, .F. ) ;
#55477 = CARTESIAN_POINT ( 'NONE',  ( 0.2646305136544065406, 7.770320294339299494, -9.465888453932885582 ) ) ;
#55478 = CARTESIAN_POINT ( 'NONE',  ( 2.491965175173692426, 2.439431489055845503, -7.322278065135876091 ) ) ;
#55479 = AXIS2_PLACEMENT_3D ( 'NONE', #16345, #5057, #30961 ) ;
#55480 = FACE_OUTER_BOUND ( 'NONE', #43601, .T. ) ;
#55481 = CARTESIAN_POINT ( 'NONE',  ( -22.27878402819508707, 2.612733676624913848, 2.600576127690894523 ) ) ;
#55482 = ADVANCED_FACE ( 'NONE', ( #21686 ), #52279, .T. ) ;
#55483 = AXIS2_PLACEMENT_3D ( 'NONE', #52630, #17702, #42602 ) ;
#55484 = CIRCLE ( 'NONE', #21506, 12.15774668701806149 ) ;
#55485 = CARTESIAN_POINT ( 'NONE',  ( 5.530133899448235191, 0.01536822665454940992, 0.004396748047611668750 ) ) ;
#55486 = CARTESIAN_POINT ( 'NONE',  ( 35.00000000000000000, -12.74613886779084382, 0.3137578094510532489 ) ) ;
#55487 = VERTEX_POINT ( 'NONE', #56602 ) ;
#55488 = CARTESIAN_POINT ( 'NONE',  ( -27.08776759928996825, -0.5731512436777455033, 2.229418711700135169 ) ) ;
#55489 = ORIENTED_EDGE ( 'NONE', *, *, #62097, .T. ) ;
#55490 = CARTESIAN_POINT ( 'NONE',  ( 0.2671309869109503299, -0.1620273132354846657, -12.24572650704445032 ) ) ;
#55491 = CYLINDRICAL_SURFACE ( 'NONE', #18254, 12.18649999999999878 ) ;
#55492 = DIRECTION ( 'NONE',  ( -1.000000000000000000, 0.000000000000000000, 0.000000000000000000 ) ) ;
#55493 = ADVANCED_FACE ( 'NONE', ( #20997 ), #46299, .T. ) ;
#55494 = DIRECTION ( 'NONE',  ( -1.000000000000000000, 0.000000000000000000, 0.000000000000000000 ) ) ;
#55495 = EDGE_CURVE ( 'NONE', #2301, #52651, #18712, .T. ) ;
#55496 = CIRCLE ( 'NONE', #1360, 5.000000000000001776 ) ;
#55497 = ORIENTED_EDGE ( 'NONE', *, *, #57273, .T. ) ;
#55498 = ORIENTED_EDGE ( 'NONE', *, *, #32474, .F. ) ;
#55499 = FACE_OUTER_BOUND ( 'NONE', #23114, .T. ) ;
#55500 = EDGE_CURVE ( 'NONE', #60956, #59860, #6070, .T. ) ;
#55501 = VERTEX_POINT ( 'NONE', #61562 ) ;
#55502 = DIRECTION ( 'NONE',  ( 0.000000000000000000, 0.2960891610144441022, 0.9551603052523501836 ) ) ;
#55504 = CIRCLE ( 'NONE', #56611, 12.18650000000000055 ) ;
#55503 = DIRECTION ( 'NONE',  ( 1.000000000000000000, 0.000000000000000000, 0.000000000000000000 ) ) ;
#55505 = CARTESIAN_POINT ( 'NONE',  ( -22.27722022243423794, -3.470949075637794312, -1.227876413014593160 ) ) ;
#55506 = DIRECTION ( 'NONE',  ( -1.000000000000000000, 0.000000000000000000, 0.000000000000000000 ) ) ;
#55507 = CARTESIAN_POINT ( 'NONE',  ( 1.104777566491139673, 9.281442536087595840, -8.411711248088998616 ) ) ;
#55508 = AXIS2_PLACEMENT_3D ( 'NONE', #36875, #11599, #8256 ) ;
#55509 = EDGE_CURVE ( 'NONE', #49767, #9981, #44181, .T. ) ;
#55510 = DIRECTION ( 'NONE',  ( 0.9582930651793755139, -0.2851010602429190910, 0.01979360193296256579 ) ) ;
#55511 = CYLINDRICAL_SURFACE ( 'NONE', #36060, 2.899999999999994582 ) ;
#55512 = VERTEX_POINT ( 'NONE', #7031 ) ;
#55513 = FACE_OUTER_BOUND ( 'NONE', #41526, .T. ) ;
#55514 = VERTEX_POINT ( 'NONE', #16009 ) ;
#55515 = CARTESIAN_POINT ( 'NONE',  ( 1.719304012340731269, -10.22720798541492826, -7.581471372739399861 ) ) ;
#55516 = CARTESIAN_POINT ( 'NONE',  ( 1.719304012341585253, 11.38834240361577521, -5.690355757825364513 ) ) ;
#55517 = VERTEX_POINT ( 'NONE', #57252 ) ;
#55518 = VECTOR ( 'NONE', #35374, 1000.000000000000227 ) ;
#55519 = DIRECTION ( 'NONE',  ( -0.000000000000000000, -0.000000000000000000, -1.000000000000000000 ) ) ;
#55520 = ORIENTED_EDGE ( 'NONE', *, *, #59298, .T. ) ;
#55521 = DIRECTION ( 'NONE',  ( 0.000000000000000000, -0.01356324068818000328, 0.9999080150203990547 ) ) ;
#55522 = DIRECTION ( 'NONE',  ( 0.000000000000000000, 0.01356324068817998940, -0.9999080150203989437 ) ) ;
#55523 = CARTESIAN_POINT ( 'NONE',  ( -37.00000000000000711, 0.000000000000000000, 0.000000000000000000 ) ) ;
#55524 = CARTESIAN_POINT ( 'NONE',  ( -27.10307689719060065, -2.283215755731203611, -0.5470785519252583384 ) ) ;
#55525 = ORIENTED_EDGE ( 'NONE', *, *, #20882, .T. ) ;
#55526 = ORIENTED_EDGE ( 'NONE', *, *, #18650, .F. ) ;
#55527 = CYLINDRICAL_SURFACE ( 'NONE', #12974, 7.499999999999988454 ) ;
#55528 = VERTEX_POINT ( 'NONE', #17344 ) ;
#55529 = CARTESIAN_POINT ( 'NONE',  ( 0.3002738374340854777, 11.59380198135587925, -3.979745968261089839 ) ) ;
#55530 = ORIENTED_EDGE ( 'NONE', *, *, #9747, .T. ) ;
#55531 = CIRCLE ( 'NONE', #15163, 12.18649999999999700 ) ;
#55532 = CIRCLE ( 'NONE', #28998, 6.936499999999989008 ) ;
#55533 = ORIENTED_EDGE ( 'NONE', *, *, #49730, .F. ) ;
#55534 = VERTEX_POINT ( 'NONE', #31323 ) ;
#55535 = CARTESIAN_POINT ( 'NONE',  ( -35.00000000000000000, 10.23119532541083743, -7.608228585767614405 ) ) ;
#55536 = CARTESIAN_POINT ( 'NONE',  ( 4.953976645022758696, -25.99587143922707000, 15.25378271594937019 ) ) ;
#55537 = VECTOR ( 'NONE', #18196, 1000.000000000000000 ) ;
#55538 = PRODUCT_RELATED_PRODUCT_CATEGORY ( 'part', '', ( #54043 ) ) ;
#55539 = AXIS2_PLACEMENT_3D ( 'NONE', #55908, #10666, #392 ) ;
#55540 = CARTESIAN_POINT ( 'NONE',  ( 2.994568964204213923, -0.9739368093814204652, -7.825096839971888762 ) ) ;
#55541 = DIRECTION ( 'NONE',  ( 0.000000000000000000, 0.000000000000000000, 1.000000000000000000 ) ) ;
#55542 = CARTESIAN_POINT ( 'NONE',  ( -22.27218376572352554, -1.571356284315158502, 3.330959526935388659 ) ) ;
#55543 = EDGE_LOOP ( 'NONE', ( #37269, #63908, #50949, #59040 ) ) ;
#55544 = CARTESIAN_POINT ( 'NONE',  ( 2.262775599885880951, -2.480428346600847433, -7.227769107231806878 ) ) ;
#55545 = EDGE_CURVE ( 'NONE', #19299, #35691, #39210, .T. ) ;
#55546 =( BOUNDED_CURVE ( )  B_SPLINE_CURVE ( 3, ( #10273, #44873, #65152, #19624 ),
 .UNSPECIFIED., .F., .F. ) 
 B_SPLINE_CURVE_WITH_KNOTS ( ( 4, 4 ),
 ( 1.570796326794896780, 1.601226737761092922 ),
 .UNSPECIFIED. ) 
 CURVE ( )  GEOMETRIC_REPRESENTATION_ITEM ( )  RATIONAL_B_SPLINE_CURVE ( ( 1.000000000000000000, 0.9999228339960630763, 0.9999228339960630763, 1.000000000000000000 ) ) 
 REPRESENTATION_ITEM ( '' )  );
#55547 = VERTEX_POINT ( 'NONE', #47598 ) ;
#55548 = CARTESIAN_POINT ( 'NONE',  ( 35.00000000000000000, 4.705694406421931860E-17, -3.469127814946512892E-15 ) ) ;
#55550 = CARTESIAN_POINT ( 'NONE',  ( -2.729590200410152434, 12.79012149208910465, 4.331891749362731581 ) ) ;
#55549 = VECTOR ( 'NONE', #31008, 1000.000000000000000 ) ;
#55551 = ORIENTED_EDGE ( 'NONE', *, *, #10742, .F. ) ;
#55552 = CARTESIAN_POINT ( 'NONE',  ( -27.65083951610984059, 12.87947692035696612, -4.055531763492385977 ) ) ;
#55553 = AXIS2_PLACEMENT_3D ( 'NONE', #42204, #15635, #16639 ) ;
#55554 = CARTESIAN_POINT ( 'NONE',  ( 0.3040950598368152291, -12.11647736519419993, -1.881452845810500207 ) ) ;
#55555 = CARTESIAN_POINT ( 'NONE',  ( 35.00000000000000000, 10.84030624090615724, 6.711949091238026632 ) ) ;
#55556 = EDGE_CURVE ( 'NONE', #37018, #12385, #48427, .T. ) ;
#55557 = VECTOR ( 'NONE', #56484, 1000.000000000000000 ) ;
#55558 = ORIENTED_EDGE ( 'NONE', *, *, #13119, .F. ) ;
#55559 = CARTESIAN_POINT ( 'NONE',  ( 2.241352910868908310, -7.633946224498474820, 0.08337961031701579540 ) ) ;
#55560 = VERTEX_POINT ( 'NONE', #26653 ) ;
#55561 = CARTESIAN_POINT ( 'NONE',  ( 1.719304012338199517, 0.000000000000000000, 0.000000000000000000 ) ) ;
#55562 = CARTESIAN_POINT ( 'NONE',  ( 1.104777566491148777, 9.895624035730071100, 7.679758239385173546 ) ) ;
#55563 = AXIS2_PLACEMENT_3D ( 'NONE', #28141, #23820, #27462 ) ;
#55564 = CARTESIAN_POINT ( 'NONE',  ( -16.81808179455697783, -29.42526233323303586, 9.774508714121763475 ) ) ;
#55565 = CARTESIAN_POINT ( 'NONE',  ( 2.259830038564642596, -3.700395974956430578, -6.684701880279044772 ) ) ;
#55566 = CARTESIAN_POINT ( 'NONE',  ( 0.3675815128205894289, -9.235491948680062180, 8.093875121226046687 ) ) ;
#55567 = EDGE_CURVE ( 'NONE', #60864, #45219, #50565, .T. ) ;
#55568 = ADVANCED_FACE ( 'NONE', ( #2733 ), #48595, .T. ) ;
#55569 = VERTEX_POINT ( 'NONE', #13972 ) ;
#55570 = DIRECTION ( 'NONE',  ( 1.000000000000000000, 0.000000000000000000, 0.000000000000000000 ) ) ;
#55571 = LINE ( 'NONE', #61515, #13133 ) ;
#55572 = CARTESIAN_POINT ( 'NONE',  ( -27.15525204139122906, -1.707635684994321279, 1.831989866434732273 ) ) ;
#55573 = DIRECTION ( 'NONE',  ( 0.000000000000000000, 0.01356324068817992175, -0.9999080150203990547 ) ) ;
#55574 = EDGE_CURVE ( 'NONE', #57258, #65189, #27979, .T. ) ;
#55575 = VECTOR ( 'NONE', #35077, 1000.000000000000000 ) ;
#55576 = CARTESIAN_POINT ( 'NONE',  ( -14.60253471108646117, -28.81751583403978501, -11.78204505887442011 ) ) ;
#55577 = CARTESIAN_POINT ( 'NONE',  ( -35.04643116707788408, -0.01193867652720878580, 0.002453861112621663620 ) ) ;
#55578 = CARTESIAN_POINT ( 'NONE',  ( 2.266490820343222357, -5.947069344280059511, -4.800466063945444617 ) ) ;
#55579 = CARTESIAN_POINT ( 'NONE',  ( -35.00000000000000000, 0.000000000000000000, 0.000000000000000000 ) ) ;
#55580 = DIRECTION ( 'NONE',  ( 0.000000000000000000, 0.6876994588534245390, -0.7259954919231297321 ) ) ;
#55581 = VECTOR ( 'NONE', #64719, 1000.000000000000227 ) ;
#55582 = CIRCLE ( 'NONE', #20548, 5.000000000000000888 ) ;
#55583 = EDGE_CURVE ( 'NONE', #55926, #3384, #7015, .T. ) ;
#55584 = CIRCLE ( 'NONE', #35388, 4.999999999999999112 ) ;
#55585 = AXIS2_PLACEMENT_3D ( 'NONE', #37594, #26625, #52248 ) ;
#55586 = ORIENTED_EDGE ( 'NONE', *, *, #50264, .T. ) ;
#55587 = CARTESIAN_POINT ( 'NONE',  ( -27.09861164373156228, -1.303360234155845676, -1.936722219471114892 ) ) ;
#55588 = ADVANCED_FACE ( 'NONE', ( #22666 ), #63856, .T. ) ;
#55589 = ORIENTED_EDGE ( 'NONE', *, *, #51994, .T. ) ;
#55590 = CARTESIAN_POINT ( 'NONE',  ( -29.68541646480307250, -1.416020129149132334, 13.42553116244733680 ) ) ;
#55591 = CARTESIAN_POINT ( 'NONE',  ( 35.00000000000000000, 7.817492529713852889, -9.348667969174437431 ) ) ;
#55592 = DIRECTION ( 'NONE',  ( 0.000000000000000000, -0.01356324068817999114, 0.9999080150203989437 ) ) ;
#55593 = AXIS2_PLACEMENT_3D ( 'NONE', #61754, #12200, #32468 ) ;
#55594 = CARTESIAN_POINT ( 'NONE',  ( 5.515188684475870851, -0.003709313826050263888, -0.003857086913166431381 ) ) ;
#55595 = VERTEX_POINT ( 'NONE', #8674 ) ;
#55596 = B_SPLINE_CURVE_WITH_KNOTS ( 'NONE', 3,
 ( #9392, #36574, #19408, #26586, #51878, #36225, #54964 ),
 .UNSPECIFIED., .F., .F.,
 ( 4, 3, 4 ),
 ( 2.737610485525898696E-18, 6.607593386745468696E-05, 0.0001321430428585257952 ),
 .UNSPECIFIED. ) ;
#55597 = CIRCLE ( 'NONE', #51337, 2.899999999999994582 ) ;
#55598 = VERTEX_POINT ( 'NONE', #17995 ) ;
#55599 = ORIENTED_EDGE ( 'NONE', *, *, #51742, .F. ) ;
#55600 = CARTESIAN_POINT ( 'NONE',  ( 36.00000000000000711, -8.496612874013091954, 9.506317355798456603 ) ) ;
#55601 = CIRCLE ( 'NONE', #19526, 5.000000000000000888 ) ;
#55602 = CARTESIAN_POINT ( 'NONE',  ( -37.00000000000000711, -3.704519465651228138, -11.60979404548638705 ) ) ;
#55603 = ORIENTED_EDGE ( 'NONE', *, *, #19483, .F. ) ;
#55604 = DIRECTION ( 'NONE',  ( 1.000000000000000000, 0.000000000000000000, -0.000000000000000000 ) ) ;
#55605 = CARTESIAN_POINT ( 'NONE',  ( 2.665405856346786173, -9.505137710817301411, 1.089747929268660931 ) ) ;
#55606 = VERTEX_POINT ( 'NONE', #33617 ) ;
#55607 = AXIS2_PLACEMENT_3D ( 'NONE', #53649, #18405, #37683 ) ;
#55608 = CARTESIAN_POINT ( 'NONE',  ( 2.273267844205335120, 4.797225296800435856, -5.952585402747609500 ) ) ;
#55609 = CIRCLE ( 'NONE', #5693, 5.000000000000000000 ) ;
#55610 = CARTESIAN_POINT ( 'NONE',  ( 3.168054457075692554, -30.71813892570141036, -15.09231838820015170 ) ) ;
#55611 = CARTESIAN_POINT ( 'NONE',  ( 35.00000000000000000, -11.74226168163341555, -0.3025107581130825896 ) ) ;
#55613 = VERTEX_POINT ( 'NONE', #13331 ) ;
#55612 = CARTESIAN_POINT ( 'NONE',  ( 2.000000000000001776, 2.562706407243739992, -6.312399813420325856 ) ) ;
#55614 = CARTESIAN_POINT ( 'NONE',  ( -36.00000000000000711, -10.39746860227885428, -7.379373053628983214 ) ) ;
#55615 = ORIENTED_EDGE ( 'NONE', *, *, #8900, .T. ) ;
#55616 = CARTESIAN_POINT ( 'NONE',  ( 35.00000000000000000, 6.307491713049029336, -9.908974237959670361 ) ) ;
#55617 = ORIENTED_EDGE ( 'NONE', *, *, #23767, .F. ) ;
#55618 = DIRECTION ( 'NONE',  ( -1.000000000000000000, 0.000000000000000000, 0.000000000000000000 ) ) ;
#55619 = CARTESIAN_POINT ( 'NONE',  ( 2.000000000000001776, 1.225832621831950187, -6.827324998361564923 ) ) ;
#55620 = CARTESIAN_POINT ( 'NONE',  ( -8.419536088379066641, -32.40770164630938410, 12.72556558505709212 ) ) ;
#55621 = LINE ( 'NONE', #10057, #47142 ) ;
#55622 = CARTESIAN_POINT ( 'NONE',  ( 19.28625800530496903, -1.699513388191772778, 11.87904264843580471 ) ) ;
#55623 = AXIS2_PLACEMENT_3D ( 'NONE', #54133, #64106, #43157 ) ;
#55624 = CARTESIAN_POINT ( 'NONE',  ( 0.3632410797595229113, -12.27601307605977965, 0.2628628737173034358 ) ) ;
#55625 = CARTESIAN_POINT ( 'NONE',  ( -29.43980975494970309, -3.641506875706034041, -12.99959336572439561 ) ) ;
#55626 = DIRECTION ( 'NONE',  ( -1.000000000000000000, -0.000000000000000000, -0.000000000000000000 ) ) ;
#55627 = PLANE ( 'NONE',  #23734 ) ;
#55629 = ORIENTED_EDGE ( 'NONE', *, *, #43589, .T. ) ;
#55628 = CARTESIAN_POINT ( 'NONE',  ( 7.228533150787943562, -7.187350446428427020, 11.43552089456373899 ) ) ;
#55630 = CARTESIAN_POINT ( 'NONE',  ( -35.00000000000000000, 11.74614673114903951, 0.01609748574465447862 ) ) ;
#55631 = EDGE_CURVE ( 'NONE', #48262, #19477, #61409, .T. ) ;
#55632 = ORIENTED_EDGE ( 'NONE', *, *, #24711, .T. ) ;
#55633 = CARTESIAN_POINT ( 'NONE',  ( -25.00000000000000355, -28.99999999999999645, -5.000000000000000888 ) ) ;
#55634 = VERTEX_POINT ( 'NONE', #63211 ) ;
#55635 = ORIENTED_EDGE ( 'NONE', *, *, #28283, .F. ) ;
#55636 = CARTESIAN_POINT ( 'NONE',  ( -35.00000000000000000, 1.488153103997124971, -11.65150730582933036 ) ) ;
#55637 = DIRECTION ( 'NONE',  ( -1.000000000000000000, 0.000000000000000000, 0.000000000000000000 ) ) ;
#55638 = CARTESIAN_POINT ( 'NONE',  ( -27.08935880048753120, -2.219773948423732435, 0.6272370006475057602 ) ) ;
#55639 = DIRECTION ( 'NONE',  ( 0.000000000000000000, 0.9246979985058709772, 0.3807014730195252272 ) ) ;
#55640 = CIRCLE ( 'NONE', #16328, 12.18649999999999878 ) ;
#55641 = DIRECTION ( 'NONE',  ( -1.000000000000000000, 0.000000000000000000, 0.000000000000000000 ) ) ;
#55642 = EDGE_CURVE ( 'NONE', #31041, #65063, #22503, .T. ) ;
#55643 = CARTESIAN_POINT ( 'NONE',  ( 35.00000000000000000, -6.307491713048959170, 9.908974237959705889 ) ) ;
#55644 = VECTOR ( 'NONE', #64702, 1000.000000000000000 ) ;
#55645 = ORIENTED_EDGE ( 'NONE', *, *, #33773, .T. ) ;
#55646 = CARTESIAN_POINT ( 'NONE',  ( -32.00000000000000000, 15.00000000000000000, 0.000000000000000000 ) ) ;
#55647 = VECTOR ( 'NONE', #21871, 1000.000000000000114 ) ;
#55648 = CARTESIAN_POINT ( 'NONE',  ( 0.000000000000000000, -7.493043167941588756, -0.3229614270520431152 ) ) ;
#55649 = CARTESIAN_POINT ( 'NONE',  ( -37.00000000000000711, 9.913596905230114942, 8.017674001891819557 ) ) ;
#55650 = EDGE_CURVE ( 'NONE', #1032, #30904, #16793, .T. ) ;
#55651 = ORIENTED_EDGE ( 'NONE', *, *, #6326, .F. ) ;
#55652 = AXIS2_PLACEMENT_3D ( 'NONE', #37343, #57653, #17406 ) ;
#55653 = CARTESIAN_POINT ( 'NONE',  ( -37.00000000000000711, 4.237174932027226504, 12.02534193257722528 ) ) ;
#55654 = VECTOR ( 'NONE', #19223, 1000.000000000000000 ) ;
#55655 = CARTESIAN_POINT ( 'NONE',  ( -22.70624764888619751, 1.907540768355125316, 4.891815784104529996 ) ) ;
#55656 = DIRECTION ( 'NONE',  ( -0.000000000000000000, -1.000000000000000000, -0.000000000000000000 ) ) ;
#55657 = EDGE_LOOP ( 'NONE', ( #65346, #6954 ) ) ;
#55658 = CARTESIAN_POINT ( 'NONE',  ( 2.261269890822072970, 6.685978463722182852, -3.699080366006626708 ) ) ;
#55659 = CARTESIAN_POINT ( 'NONE',  ( 15.08189101924520870, -34.00125857029218679, 8.507794521696036227 ) ) ;
#55660 = CARTESIAN_POINT ( 'NONE',  ( 37.00000000000000711, 0.7214809346830272085, 11.72397916322010936 ) ) ;
#55661 = DIRECTION ( 'NONE',  ( 1.000000000000000000, 0.000000000000000000, 0.000000000000000000 ) ) ;
#55662 = DIRECTION ( 'NONE',  ( 0.000000000000000000, 0.01356324068817998940, -0.9999080150203990547 ) ) ;
#55663 = ORIENTED_EDGE ( 'NONE', *, *, #56127, .F. ) ;
#55664 = LINE ( 'NONE', #19765, #33215 ) ;
#55665 = CARTESIAN_POINT ( 'NONE',  ( -22.27721038036499834, 3.438655654856790811, 1.315315479297472390 ) ) ;
#55666 = CARTESIAN_POINT ( 'NONE',  ( -22.29382655386184808, 3.584644999358090889, -1.036465316386231850 ) ) ;
#55667 = ORIENTED_EDGE ( 'NONE', *, *, #38918, .T. ) ;
#55668 = DIRECTION ( 'NONE',  ( 0.000000000000000000, 0.000000000000000000, 1.000000000000000000 ) ) ;
#55669 = DIRECTION ( 'NONE',  ( -1.000000000000000000, 0.000000000000000000, 0.000000000000000000 ) ) ;
#55670 = ORIENTED_EDGE ( 'NONE', *, *, #28003, .T. ) ;
#55671 = VECTOR ( 'NONE', #47553, 1000.000000000000000 ) ;
#55672 = EDGE_CURVE ( 'NONE', #34466, #50843, #53591, .T. ) ;
#55673 = CIRCLE ( 'NONE', #60988, 12.74999999999999822 ) ;
#55674 = ORIENTED_EDGE ( 'NONE', *, *, #30837, .F. ) ;
#55675 = VERTEX_POINT ( 'NONE', #7694 ) ;
#55676 = EDGE_CURVE ( 'NONE', #59, #57650, #8343, .T. ) ;
#55677 = ORIENTED_EDGE ( 'NONE', *, *, #12055, .F. ) ;
#55678 = CARTESIAN_POINT ( 'NONE',  ( 2.000000000000001776, 1.530946385938383614, 7.342084388195340594 ) ) ;
#55679 = DIRECTION ( 'NONE',  ( 0.3939253465568944290, 0.8008152550167598749, -0.4511294145502736663 ) ) ;
#55680 = DIRECTION ( 'NONE',  ( 0.1034490876700550344, -0.000000000000000000, 0.9946347501772866417 ) ) ;
#55681 = CARTESIAN_POINT ( 'NONE',  ( 0.2653519789438757992, 4.167744179924070203, -11.51519617080776925 ) ) ;
#55682 = FACE_OUTER_BOUND ( 'NONE', #12405, .T. ) ;
#55683 = CARTESIAN_POINT ( 'NONE',  ( -11.18139917412363182, -29.23077454460525360, 7.530122743832658117 ) ) ;
#55684 = CARTESIAN_POINT ( 'NONE',  ( 24.18120799216340089, -3.372877268056853506, -13.07685726758646538 ) ) ;
#55686 = ORIENTED_EDGE ( 'NONE', *, *, #6188, .T. ) ;
#55685 = DIRECTION ( 'NONE',  ( -1.000000000000000000, 0.000000000000000000, 0.000000000000000000 ) ) ;
#55687 = DIRECTION ( 'NONE',  ( -1.000000000000000000, 0.000000000000000000, 0.000000000000000000 ) ) ;
#55688 = ORIENTED_EDGE ( 'NONE', *, *, #22722, .T. ) ;
#55689 = DIRECTION ( 'NONE',  ( -1.000000000000000000, 0.000000000000000000, 0.000000000000000000 ) ) ;
#55690 = CIRCLE ( 'NONE', #37597, 12.18650000000000055 ) ;
#55691 = EDGE_LOOP ( 'NONE', ( #33339, #14403, #38847, #20416 ) ) ;
#55692 = VERTEX_POINT ( 'NONE', #48286 ) ;
#55693 = CARTESIAN_POINT ( 'NONE',  ( 0.2911222467163634420, 9.524109243548085857, -7.711756541611588744 ) ) ;
#55694 = CARTESIAN_POINT ( 'NONE',  ( 15.59065549519832494, -34.16917994668085612, 7.755393724195712934 ) ) ;
#55695 = AXIS2_PLACEMENT_3D ( 'NONE', #14828, #10507, #35114 ) ;
#55696 = CYLINDRICAL_SURFACE ( 'NONE', #4664, 12.74999999999999822 ) ;
#55697 = EDGE_CURVE ( 'NONE', #9459, #6270, #38936, .T. ) ;
#55698 = CARTESIAN_POINT ( 'NONE',  ( 0.000000000000000000, 0.000000000000000000, 0.000000000000000000 ) ) ;
#55699 = CARTESIAN_POINT ( 'NONE',  ( 35.00000000000000000, 4.705694406421931860E-17, -3.469127814946512892E-15 ) ) ;
#55700 = CARTESIAN_POINT ( 'NONE',  ( 2.000000000000001776, 4.409940824963425321, 5.354199675985255702 ) ) ;
#55701 = VERTEX_POINT ( 'NONE', #23980 ) ;
#55702 = EDGE_CURVE ( 'NONE', #20343, #6763, #6225, .T. ) ;
#55703 = ORIENTED_EDGE ( 'NONE', *, *, #41970, .T. ) ;
#55704 = ADVANCED_FACE ( 'NONE', ( #54573 ), #51470, .T. ) ;
#55705 = DIRECTION ( 'NONE',  ( 0.000000000000000000, 0.3193015301359806157, -0.9476531711828021232 ) ) ;
#55706 = ORIENTED_EDGE ( 'NONE', *, *, #45374, .T. ) ;
#55707 = AXIS2_PLACEMENT_3D ( 'NONE', #61011, #21080, #30081 ) ;
#55708 = ADVANCED_FACE ( 'NONE', ( #56425 ), #30085, .F. ) ;
#55709 = ORIENTED_EDGE ( 'NONE', *, *, #24265, .T. ) ;
#55710 = PLANE ( 'NONE',  #18998 ) ;
#55711 = CARTESIAN_POINT ( 'NONE',  ( 10.16591523190729163, 8.042301321965682703, -8.910861195510744182 ) ) ;
#55712 = CARTESIAN_POINT ( 'NONE',  ( -22.29018399051993882, 0.9010028109495269444, -3.609810019245846213 ) ) ;
#55713 = CARTESIAN_POINT ( 'NONE',  ( 18.39714084132998195, 4.205996179170882421, 11.25142999110358133 ) ) ;
#55714 = CARTESIAN_POINT ( 'NONE',  ( -22.27716857039623477, 1.095155339732109212, -3.514919882996453193 ) ) ;
#55715 = DIRECTION ( 'NONE',  ( -1.000000000000000000, 0.000000000000000000, -0.000000000000000000 ) ) ;
#55716 = AXIS2_PLACEMENT_3D ( 'NONE', #39509, #59802, #65102 ) ;
#55717 = ADVANCED_FACE ( 'NONE', ( #15523 ), #5236, .T. ) ;
#55718 = DIRECTION ( 'NONE',  ( 0.000000000000000000, 0.4198891015602656540, -0.9075754196709564514 ) ) ;
#55719 = ORIENTED_EDGE ( 'NONE', *, *, #64979, .T. ) ;
#55720 = ADVANCED_FACE ( 'NONE', ( #30804 ), #10872, .T. ) ;
#55721 = ORIENTED_EDGE ( 'NONE', *, *, #6347, .T. ) ;
#55722 = CARTESIAN_POINT ( 'NONE',  ( -37.00000000000000711, 0.000000000000000000, 0.000000000000000000 ) ) ;
#55723 = VECTOR ( 'NONE', #30704, 1000.000000000000227 ) ;
#55724 = SURFACE_STYLE_FILL_AREA ( #35417 ) ;
#55725 = DIRECTION ( 'NONE',  ( -1.000000000000000000, 0.000000000000000000, 0.000000000000000000 ) ) ;
#55726 = CARTESIAN_POINT ( 'NONE',  ( 3.708583301347321726, -10.51590576721076964, 5.781912091200419823 ) ) ;
#55727 = DIRECTION ( 'NONE',  ( 0.8317381556525372810, -0.5551681190699946367, 0.000000000000000000 ) ) ;
#55728 = EDGE_CURVE ( 'NONE', #7867, #9912, #17905, .T. ) ;
#55729 = CARTESIAN_POINT ( 'NONE',  ( 23.75192053619575461, -3.113835264533937774, -13.14002899460337304 ) ) ;
#55730 = DIRECTION ( 'NONE',  ( 0.000000000000000000, 0.2149704402110246271, -0.9766205557100866574 ) ) ;
#55731 = CARTESIAN_POINT ( 'NONE',  ( 2.524535260912044610, 6.060306679218721904, 4.796565674004597213 ) ) ;
#55732 = ORIENTED_EDGE ( 'NONE', *, *, #12383, .F. ) ;
#55733 = AXIS2_PLACEMENT_3D ( 'NONE', #10619, #39906, #25602 ) ;
#55734 = CARTESIAN_POINT ( 'NONE',  ( 2.373367633546870969, -0.1808255748566004184, 7.676289145832772221 ) ) ;
#55735 = DIRECTION ( 'NONE',  ( 1.000000000000000000, 0.000000000000000000, 0.000000000000000000 ) ) ;
#55736 = CIRCLE ( 'NONE', #21807, 12.18649999999999878 ) ;
#55737 = DIRECTION ( 'NONE',  ( 0.000000000000000000, 0.01356324068817998940, -0.9999080150203990547 ) ) ;
#55738 = CARTESIAN_POINT ( 'NONE',  ( 0.9232058338315048962, 12.21058493388773591, 2.536181247095406377 ) ) ;
#55739 =( BOUNDED_SURFACE ( )  B_SPLINE_SURFACE ( 3, 1, ( 
 ( #27745, #11157 ),
 ( #12893, #43143 ),
 ( #52809, #38153 ),
 ( #31851, #37173 ) ),
 .UNSPECIFIED., .F., .F., .F. ) 
 B_SPLINE_SURFACE_WITH_KNOTS ( ( 4, 4 ),
 ( 2, 2 ),
 ( 0.000000000000000000, 1.000000000000000000 ),
 ( 0.000000000000000000, 1.000000000000000000 ),
 .UNSPECIFIED. ) 
 GEOMETRIC_REPRESENTATION_ITEM ( )  RATIONAL_B_SPLINE_SURFACE ( (
 ( 1.000000000000000000, 1.000000000000000000),
 ( 0.9942764183789327692, 0.8450855930916585379),
 ( 0.9942764183789327692, 0.8450855930916585379),
 ( 1.000000000000000000, 1.000000000000000000) ) ) 
 REPRESENTATION_ITEM ( '' )  SURFACE ( )  );
#55740 = VERTEX_POINT ( 'NONE', #896 ) ;
#55741 = CARTESIAN_POINT ( 'NONE',  ( -18.17455973634320898, -4.727991781583684272, -12.64561680075576255 ) ) ;
#55742 = CARTESIAN_POINT ( 'NONE',  ( 26.73134588528545663, 13.02586532392652785, 3.554799201164403843 ) ) ;
#55743 = CARTESIAN_POINT ( 'NONE',  ( 8.754896909465220034, -28.78086681028207749, -9.883947858767701433 ) ) ;
#55744 = ORIENTED_EDGE ( 'NONE', *, *, #59149, .T. ) ;
#55745 = CARTESIAN_POINT ( 'NONE',  ( -22.31328051695926007, 3.781397440874590732, -0.2528478350593763024 ) ) ;
#55746 = CARTESIAN_POINT ( 'NONE',  ( -2.532614230583026593, 25.00000000000000000, 10.89930238848911337 ) ) ;
#55747 = CARTESIAN_POINT ( 'NONE',  ( 37.00000000000000711, -11.30684963584392477, -4.545979934229371189 ) ) ;
#55749 = EDGE_LOOP ( 'NONE', ( #19445, #65614, #60099, #10774 ) ) ;
#55748 = FACE_OUTER_BOUND ( 'NONE', #52377, .T. ) ;
#55750 = CARTESIAN_POINT ( 'NONE',  ( 1.000000000000000888, 6.664893814313728626, 3.439359016433498173 ) ) ;
#55751 = EDGE_CURVE ( 'NONE', #50088, #10101, #1894, .T. ) ;
#55752 = CARTESIAN_POINT ( 'NONE',  ( -24.42101984568203221, -4.276292373951995351, -0.3620223918248546835 ) ) ;
#55753 = EDGE_LOOP ( 'NONE', ( #29136, #31061, #23373, #65624 ) ) ;
#55754 = CARTESIAN_POINT ( 'NONE',  ( -35.00000000000000000, -8.551552972817024312, -8.052525312709976291 ) ) ;
#55755 = DIRECTION ( 'NONE',  ( 0.000000000000000000, -0.01356324068817992175, 0.9999080150203990547 ) ) ;
#55756 = CARTESIAN_POINT ( 'NONE',  ( 22.57855258442564761, -4.427776684447072952, -11.15324139578564910 ) ) ;
#55757 = CARTESIAN_POINT ( 'NONE',  ( 8.498256429135825130, 5.239437556988991496, -12.44347423756361160 ) ) ;
#55758 = DIRECTION ( 'NONE',  ( 0.000000000000000000, 1.000000000000000000, -0.000000000000000000 ) ) ;
#55759 = CARTESIAN_POINT ( 'NONE',  ( 35.00000000000000000, 4.705694406421931860E-17, -3.469127814946512892E-15 ) ) ;
#55760 = CARTESIAN_POINT ( 'NONE',  ( 0.3164563675027644019, 11.43920928915630952, -4.419430877662233748 ) ) ;
#55761 = CIRCLE ( 'NONE', #39805, 2.899999999999996358 ) ;
#55762 = ORIENTED_EDGE ( 'NONE', *, *, #27436, .F. ) ;
#55763 = CYLINDRICAL_SURFACE ( 'NONE', #49113, 5.000000000000000888 ) ;
#55764 = ORIENTED_EDGE ( 'NONE', *, *, #46953, .F. ) ;
#55765 = DIRECTION ( 'NONE',  ( 0.000000000000000000, 0.01356324068817998940, -0.9999080150203990547 ) ) ;
#55766 = B_SPLINE_CURVE_WITH_KNOTS ( 'NONE', 3,
 ( #30952, #61874, #61222, #52247, #15647, #56221, #35614, #10665, #391, #51264, #31602, #51915, #41914, #6356, #51595, #10338, #26624, #5715, #40607, #6688, #25986, #55907, #6044, #21658, #46271, #62198, #30614, #41250, #26301, #61532, #47261, #46918, #1702, #50926, #46581, #1036, #16333, #36607, #15974, #36922, #21306, #41584, #16651, #5371, #48258, #17314, #38225, #33253, #2014, #48567, #32903, #63827, #2361, #47567 ),
 .UNSPECIFIED., .F., .F.,
 ( 4, 2, 2, 2, 2, 2, 2, 2, 2, 2, 2, 2, 2, 2, 2, 2, 2, 2, 2, 2, 2, 2, 2, 2, 2, 2, 4 ),
 ( 0.000000000000000000, 0.004712545709777831403, 0.007068818564666746670, 0.009425091419555662806, 0.01413763712933349681, 0.01649390998422241295, 0.01885018283911132908, 0.02356272854888913360, 0.02591900140377803932, 0.02827527425866694158, 0.03063154711355584384, 0.03180968354100029150, 0.03298781996844474262, 0.03770036567822253326, 0.04005663853311142858, 0.04123477496055587971, 0.04241291138800033084, 0.04712545709777812841, 0.04948172995266704455, 0.05183800280755595374, 0.05655054851733376520, 0.06126309422711157665, 0.06361936708200048585, 0.06597563993688938810, 0.07068818564666720650, 0.07304445850155609488, 0.07540073135644499713 ),
 .UNSPECIFIED. ) ;
#55767 = CARTESIAN_POINT ( 'NONE',  ( -35.00000000000000000, 0.000000000000000000, 0.000000000000000000 ) ) ;
#55768 = EDGE_CURVE ( 'NONE', #9488, #64485, #58253, .T. ) ;
#55769 = DIRECTION ( 'NONE',  ( 0.000000000000000000, 0.01356324068817992522, -0.9999080150203990547 ) ) ;
#55770 = VERTEX_POINT ( 'NONE', #30489 ) ;
#55771 = CARTESIAN_POINT ( 'NONE',  ( -35.04709527796842394, 0.01120703303052542066, -0.005220632201003577721 ) ) ;
#55772 = CARTESIAN_POINT ( 'NONE',  ( 35.00000000000000000, 0.8294751490779324055, -12.15823808070322798 ) ) ;
#55773 = EDGE_CURVE ( 'NONE', #30777, #11634, #51904, .T. ) ;
#55774 = CARTESIAN_POINT ( 'NONE',  ( -22.27715526084302056, -1.423304177213873700, 3.395518526174210905 ) ) ;
#55775 = ORIENTED_EDGE ( 'NONE', *, *, #35866, .F. ) ;
#55776 = ORIENTED_EDGE ( 'NONE', *, *, #28967, .F. ) ;
#55777 = CARTESIAN_POINT ( 'NONE',  ( -22.27706485742869091, 2.985151051101503583, -2.154081322712197544 ) ) ;
#55778 = EDGE_CURVE ( 'NONE', #332, #983, #52929, .T. ) ;
#55779 = ORIENTED_EDGE ( 'NONE', *, *, #39331, .T. ) ;
#55780 = CARTESIAN_POINT ( 'NONE',  ( 0.000000000000000000, 0.000000000000000000, 0.000000000000000000 ) ) ;
#55781 = FACE_OUTER_BOUND ( 'NONE', #65147, .T. ) ;
#55782 = DIRECTION ( 'NONE',  ( 0.000000000000000000, 0.9937233664769765662, -0.1118654143051581590 ) ) ;
#55783 = CIRCLE ( 'NONE', #32367, 6.936499999999995225 ) ;
#55784 = DIRECTION ( 'NONE',  ( -0.000000000000000000, -0.000000000000000000, -1.000000000000000000 ) ) ;
#55785 = CARTESIAN_POINT ( 'NONE',  ( 0.000000000000000000, -33.00000000000000000, 0.000000000000000000 ) ) ;
#55786 = CARTESIAN_POINT ( 'NONE',  ( -37.00000000000000711, 10.63508530065528923, -4.986700593229593359 ) ) ;
#55787 = EDGE_CURVE ( 'NONE', #28939, #10128, #19986, .T. ) ;
#55788 = DIRECTION ( 'NONE',  ( 1.000000000000000000, 0.000000000000000000, 0.000000000000000000 ) ) ;
#55789 = ORIENTED_EDGE ( 'NONE', *, *, #64868, .T. ) ;
#55790 = CARTESIAN_POINT ( 'NONE',  ( 2.241352910868908310, 7.633946224498473931, -0.08337961031706911386 ) ) ;
#55791 = ADVANCED_FACE ( 'NONE', ( #17831 ), #42096, .T. ) ;
#55792 = CARTESIAN_POINT ( 'NONE',  ( 2.000000000000001776, -6.338823199656690832, 2.816798305433647620 ) ) ;
#55793 = ADVANCED_FACE ( 'NONE', ( #12179 ), #22492, .T. ) ;
#55794 = CARTESIAN_POINT ( 'NONE',  ( 2.241528039335008327, 5.838210500619377186, 4.919377664485117485 ) ) ;
#55795 = CARTESIAN_POINT ( 'NONE',  ( 2.241526690369555208, -7.515450538999844277, 1.342748965918859616 ) ) ;
#55796 = DIRECTION ( 'NONE',  ( 0.000000000000000000, 0.9289767198167925288, -0.3701381553399118451 ) ) ;
#55797 = CARTESIAN_POINT ( 'NONE',  ( 1.000000000000000888, -1.693411908627144635, -7.306323022404617618 ) ) ;
#55798 = CARTESIAN_POINT ( 'NONE',  ( 2.990245332647871290, 7.779904630197308713, 3.377079998295634766 ) ) ;
#55799 = DIRECTION ( 'NONE',  ( 0.9688695217174486674, 1.734723475976807292E-15, -0.2475719085175099865 ) ) ;
#55800 = ADVANCED_FACE ( 'NONE', ( #53426 ), #2218, .T. ) ;
#55801 = AXIS2_PLACEMENT_3D ( 'NONE', #42953, #63232, #53270 ) ;
#55802 = B_SPLINE_CURVE_WITH_KNOTS ( 'NONE', 3,
 ( #14111, #7839, #12799, #63340, #23448, #48410, #17806, #33428, #54382, #34405, #22807, #38071, #58375, #43725, #54037, #2537, #2860, #49408, #24104 ),
 .UNSPECIFIED., .F., .F.,
 ( 4, 3, 3, 3, 3, 3, 4 ),
 ( 6.508826038821075435E-18, 2.825908398831318295E-05, 4.208813692484010587E-05, 5.591713746943977590E-05, 6.279584083232033951E-05, 9.105792820296882426E-05, 0.0001153131102488863535 ),
 .UNSPECIFIED. ) ;
#55803 = ORIENTED_EDGE ( 'NONE', *, *, #39001, .T. ) ;
#55804 = CARTESIAN_POINT ( 'NONE',  ( 0.000000000000000000, -3.805198749487401777, -5.799611601383285020 ) ) ;
#55805 = EDGE_CURVE ( 'NONE', #43228, #2417, #5140, .T. ) ;
#55806 = ORIENTED_EDGE ( 'NONE', *, *, #58765, .F. ) ;
#55807 = CARTESIAN_POINT ( 'NONE',  ( -35.00000000000000000, -12.00000000000000000, 0.000000000000000000 ) ) ;
#55808 = CARTESIAN_POINT ( 'NONE',  ( 0.2653519890538381665, 0.02202471025205905014, 12.24619734961521544 ) ) ;
#55809 = CARTESIAN_POINT ( 'NONE',  ( -16.78314026428192207, 7.533399764774538987, -11.20369790611374228 ) ) ;
#55810 = ADVANCED_FACE ( 'NONE', ( #6882 ), #63365, .T. ) ;
#55811 = CARTESIAN_POINT ( 'NONE',  ( 2.589278595513128778, -7.670769623692313743, -1.107986312493487890 ) ) ;
#55812 = CARTESIAN_POINT ( 'NONE',  ( -35.00000000000000000, -8.573591947375380329, 8.029056188533655103 ) ) ;
#55813 = VERTEX_POINT ( 'NONE', #38096 ) ;
#55814 = CARTESIAN_POINT ( 'NONE',  ( 36.00000000000000711, -4.561791185930328396, 11.90598845858538013 ) ) ;
#55815 = CARTESIAN_POINT ( 'NONE',  ( 2.430348790456984265, 2.448665558939242537, -7.297553103283330067 ) ) ;
#55816 = LINE ( 'NONE', #57128, #2498 ) ;
#55817 = CARTESIAN_POINT ( 'NONE',  ( 2.241509619876138171, -6.592435552901097395, -3.850348903238783649 ) ) ;
#55818 = B_SPLINE_CURVE_WITH_KNOTS ( 'NONE', 3,
 ( #8076, #18391, #11804, #33660, #8726, #24024 ),
 .UNSPECIFIED., .F., .F.,
 ( 4, 2, 4 ),
 ( 0.006113759649309998857, 0.008271820019582997591, 0.01042988038985599719 ),
 .UNSPECIFIED. ) ;
#55819 = CARTESIAN_POINT ( 'NONE',  ( 29.51976981715666781, -4.571419055710073565, 11.09513982864076276 ) ) ;
#55820 = DIRECTION ( 'NONE',  ( 1.000000000000000000, 0.000000000000000000, 0.000000000000000000 ) ) ;
#55821 = CIRCLE ( 'NONE', #50512, 6.936499999999989008 ) ;
#55822 = ORIENTED_EDGE ( 'NONE', *, *, #13626, .F. ) ;
#55823 = CARTESIAN_POINT ( 'NONE',  ( -27.09030469827931853, -0.5638997280354804964, 2.239626370113432685 ) ) ;
#55824 = ORIENTED_EDGE ( 'NONE', *, *, #10696, .T. ) ;
#55825 = CARTESIAN_POINT ( 'NONE',  ( 0.2648978790185584908, 12.24533305150758089, 0.1321385342562836074 ) ) ;
#55826 = CARTESIAN_POINT ( 'NONE',  ( -22.71097035706202405, -4.510116093748277599, 2.118550233809401107 ) ) ;
#55827 = CARTESIAN_POINT ( 'NONE',  ( 28.78308862069595264, -9.765596609978194564, 6.977306409396123676 ) ) ;
#55828 = DIRECTION ( 'NONE',  ( 0.000000000000000000, 0.01356324068817992175, -0.9999080150203990547 ) ) ;
#55829 = CIRCLE ( 'NONE', #27156, 2.899999999999996803 ) ;
#55830 = EDGE_CURVE ( 'NONE', #57845, #50922, #27963, .T. ) ;
#55831 = EDGE_LOOP ( 'NONE', ( #44506, #3851, #15632, #37308 ) ) ;
#55832 = ORIENTED_EDGE ( 'NONE', *, *, #23159, .T. ) ;
#55833 = CARTESIAN_POINT ( 'NONE',  ( 0.3665391374699464300, -1.872534962004717141, -12.13918562134720425 ) ) ;
#55834 = ORIENTED_EDGE ( 'NONE', *, *, #10886, .T. ) ;
#55835 = CARTESIAN_POINT ( 'NONE',  ( 2.000000000000001776, 0.000000000000000000, 0.000000000000000000 ) ) ;
#55836 = DIRECTION ( 'NONE',  ( 0.000000000000000000, -0.7617968321374944951, -0.6478160128811867313 ) ) ;
#55837 = CYLINDRICAL_SURFACE ( 'NONE', #56423, 12.74999999999999822 ) ;
#55838 = CARTESIAN_POINT ( 'NONE',  ( -27.45775109278351067, 10.51123867646838583, -8.471355351200609007 ) ) ;
#55839 = DIRECTION ( 'NONE',  ( 0.000000000000000000, 0.01356324068817992695, -0.9999080150203990547 ) ) ;
#55840 = CARTESIAN_POINT ( 'NONE',  ( 0.8375941296816615811, 10.95781044612504473, -5.882592429484091667 ) ) ;
#55841 = CARTESIAN_POINT ( 'NONE',  ( -22.31328051695926007, 1.076152733467212741, 3.633840107626929328 ) ) ;
#55842 = VERTEX_POINT ( 'NONE', #32766 ) ;
#55843 = EDGE_CURVE ( 'NONE', #45661, #36765, #63542, .T. ) ;
#55844 = CARTESIAN_POINT ( 'NONE',  ( -7.959843492831086387, -7.020518735649992514, -9.756886859334462869 ) ) ;
#55845 = VERTEX_POINT ( 'NONE', #43089 ) ;
#55846 = CARTESIAN_POINT ( 'NONE',  ( -27.08954555554373300, 1.900922216191360148, -1.307633183325732640 ) ) ;
#55847 = EDGE_CURVE ( 'NONE', #27703, #17490, #60366, .T. ) ;
#55848 = EDGE_LOOP ( 'NONE', ( #51984, #1715, #38105, #13589 ) ) ;
#55849 = CARTESIAN_POINT ( 'NONE',  ( -22.27711351828769892, 3.575417021793781736, -0.8770428151440373687 ) ) ;
#55850 = ORIENTED_EDGE ( 'NONE', *, *, #11648, .T. ) ;
#55851 = CARTESIAN_POINT ( 'NONE',  ( 35.00000000000000000, -10.32377448871663006, 6.475373545682407972 ) ) ;
#55852 = CARTESIAN_POINT ( 'NONE',  ( 5.417119996861458731, -9.515710175651925340, -9.580509969479626520 ) ) ;
#55853 = CARTESIAN_POINT ( 'NONE',  ( 1.000000000000000888, -4.604744433234619017, -5.919993978425545755 ) ) ;
#55854 = ORIENTED_EDGE ( 'NONE', *, *, #7110, .T. ) ;
#55855 = VERTEX_POINT ( 'NONE', #43409 ) ;
#55856 = CARTESIAN_POINT ( 'NONE',  ( 2.931247277082679403, -6.988361004535458498, 3.607110715259723932 ) ) ;
#55857 = EDGE_CURVE ( 'NONE', #57966, #3825, #7255, .T. ) ;
#55858 = ORIENTED_EDGE ( 'NONE', *, *, #8285, .F. ) ;
#55859 = DIRECTION ( 'NONE',  ( -1.000000000000000000, -0.000000000000000000, 0.000000000000000000 ) ) ;
#55860 = ORIENTED_EDGE ( 'NONE', *, *, #20887, .F. ) ;
#55861 = EDGE_LOOP ( 'NONE', ( #53220, #34662, #55028, #33105 ) ) ;
#55862 = VERTEX_POINT ( 'NONE', #57761 ) ;
#55863 = CARTESIAN_POINT ( 'NONE',  ( 2.889800649504073782, -3.882893708502079377, 4.732281052280299605 ) ) ;
#55864 = CARTESIAN_POINT ( 'NONE',  ( 9.722110222095130538, -26.73349363795547973, 14.00621188957225449 ) ) ;
#55865 = DIRECTION ( 'NONE',  ( -1.000000000000000000, 0.000000000000000000, 0.000000000000000000 ) ) ;
#55866 = CARTESIAN_POINT ( 'NONE',  ( -34.00000000000000000, 1.836970198721036590E-16, 0.000000000000000000 ) ) ;
#55867 = DIRECTION ( 'NONE',  ( 0.000000000000000000, -0.01356324068817998940, 0.9999080150203990547 ) ) ;
#55868 = VERTEX_POINT ( 'NONE', #63688 ) ;
#55869 = CIRCLE ( 'NONE', #26146, 12.74999999999999822 ) ;
#55870 = DIRECTION ( 'NONE',  ( 0.000000000000000000, 0.01356324068817991828, -0.9999080150203990547 ) ) ;
#55871 = AXIS2_PLACEMENT_3D ( 'NONE', #11788, #32070, #2511 ) ;
#55872 = ORIENTED_EDGE ( 'NONE', *, *, #9844, .T. ) ;
#55873 = LINE ( 'NONE', #40567, #10456 ) ;
#55874 = CARTESIAN_POINT ( 'NONE',  ( -3.363016410184096028, 10.07324327587569002, 8.995337225020698213 ) ) ;
#55875 = ORIENTED_EDGE ( 'NONE', *, *, #2730, .T. ) ;
#55876 = CARTESIAN_POINT ( 'NONE',  ( 0.2759803524722206913, -10.70204612651779819, 5.960075719898805247 ) ) ;
#55877 = CARTESIAN_POINT ( 'NONE',  ( 5.530133899448235191, 0.009387834778845855280, -0.01293763278443441425 ) ) ;
#55878 = DIRECTION ( 'NONE',  ( 0.000000000000000000, 0.000000000000000000, 1.000000000000000000 ) ) ;
#55879 = EDGE_CURVE ( 'NONE', #14040, #16694, #17786, .T. ) ;
#55880 = VECTOR ( 'NONE', #9720, 1000.000000000000000 ) ;
#55881 = VERTEX_POINT ( 'NONE', #17515 ) ;
#55882 = DIRECTION ( 'NONE',  ( 0.000000000000000000, 0.01356324068817998940, -0.9999080150203990547 ) ) ;
#55883 = EDGE_CURVE ( 'NONE', #3051, #33198, #6235, .T. ) ;
#55884 = ORIENTED_EDGE ( 'NONE', *, *, #30107, .T. ) ;
#55885 = CARTESIAN_POINT ( 'NONE',  ( -25.32301808527470044, -7.777392180360524598, 11.03968484280607676 ) ) ;
#55886 = CARTESIAN_POINT ( 'NONE',  ( -2.024814117303733063, -26.59886070765379529, 16.15701038285739344 ) ) ;
#55887 = EDGE_CURVE ( 'NONE', #65451, #20070, #13612, .T. ) ;
#55888 = FACE_OUTER_BOUND ( 'NONE', #49576, .T. ) ;
#55889 = CARTESIAN_POINT ( 'NONE',  ( 37.00000000000000711, 4.705694406421931860E-17, -3.469127814946512892E-15 ) ) ;
#55890 = ORIENTED_EDGE ( 'NONE', *, *, #55847, .F. ) ;
#55891 = CARTESIAN_POINT ( 'NONE',  ( 2.655192694323545766, 4.290256727312732110, -8.589732161580133862 ) ) ;
#55892 = DIRECTION ( 'NONE',  ( 1.000000000000000000, -0.000000000000000000, 0.000000000000000000 ) ) ;
#55893 = CARTESIAN_POINT ( 'NONE',  ( 0.000000000000000000, 0.8935325819929771374, -7.446583077151355923 ) ) ;
#55894 = CARTESIAN_POINT ( 'NONE',  ( 22.08055403950514517, -12.79402759897448583, -4.312350172591147057 ) ) ;
#55895 = DIRECTION ( 'NONE',  ( 0.000000000000000000, 0.01356324068817998940, -0.9999080150203990547 ) ) ;
#55896 = CARTESIAN_POINT ( 'NONE',  ( -35.04643116707788408, -0.007621814750504232738, -0.009511118309140503824 ) ) ;
#55897 = CARTESIAN_POINT ( 'NONE',  ( 1.452237505248555660, 11.67686475128086343, -4.880303821310893575 ) ) ;
#55898 = CARTESIAN_POINT ( 'NONE',  ( 0.3665391374699465965, 9.237363111276877703, -8.095513416941136242 ) ) ;
#55899 = CARTESIAN_POINT ( 'NONE',  ( 2.276198483117257254, 0.1540629821339370153, -7.644465698238555262 ) ) ;
#55900 = EDGE_CURVE ( 'NONE', #54137, #39298, #27807, .T. ) ;
#55901 = VECTOR ( 'NONE', #24415, 1000.000000000000000 ) ;
#55902 = ORIENTED_EDGE ( 'NONE', *, *, #53341, .F. ) ;
#55903 = ADVANCED_FACE ( 'NONE', ( #38775 ), #54407, .T. ) ;
#55904 = CIRCLE ( 'NONE', #50601, 12.18649999999999878 ) ;
#55905 = ORIENTED_EDGE ( 'NONE', *, *, #43667, .T. ) ;
#55906 = DIRECTION ( 'NONE',  ( 0.000000000000000000, -0.8835120444460178302, -0.4684084406997996997 ) ) ;
#55907 = CARTESIAN_POINT ( 'NONE',  ( 48.06591103469481396, -0.3868811097602622984, -6.642178517338836130 ) ) ;
#55908 = CARTESIAN_POINT ( 'NONE',  ( 2.000000000000001776, 0.3246585432987117992, -6.805031400696120336 ) ) ;
#55909 = CARTESIAN_POINT ( 'NONE',  ( 2.290907136834313906, -1.168459104840546825, -7.561169784528830817 ) ) ;
#55910 = ORIENTED_EDGE ( 'NONE', *, *, #33206, .F. ) ;
#55911 = EDGE_CURVE ( 'NONE', #47398, #49321, #35194, .T. ) ;
#55912 = EDGE_LOOP ( 'NONE', ( #22332, #19852, #20004, #47267 ) ) ;
#55913 = ORIENTED_EDGE ( 'NONE', *, *, #27839, .F. ) ;
#55914 = CARTESIAN_POINT ( 'NONE',  ( 29.70345330596045130, -6.346709636665306853, 10.23243518362844107 ) ) ;
#55915 = B_SPLINE_CURVE_WITH_KNOTS ( 'NONE', 3,
 ( #18476, #58364, #8467, #54026, #3838, #8805, #28109, #49060, #28416, #42714, #3514, #39050, #23436 ),
 .UNSPECIFIED., .F., .F.,
 ( 4, 3, 3, 3, 4 ),
 ( 3.127317220692750759E-18, 6.607593386745410421E-05, 0.0001321518677373518646, 0.0001982171734706181221, 0.0002642860854759469282 ),
 .UNSPECIFIED. ) ;
#55916 = DIRECTION ( 'NONE',  ( 0.000000000000000000, 0.6051742151937610226, 0.7960930657056469739 ) ) ;
#55917 = ORIENTED_EDGE ( 'NONE', *, *, #42291, .F. ) ;
#55918 = CARTESIAN_POINT ( 'NONE',  ( 1.948354844646291939, -0.7204626209691626926, -11.94326855455706848 ) ) ;
#55919 = CARTESIAN_POINT ( 'NONE',  ( -17.71957339262799280, 3.746001421221477834, -11.40215424527250754 ) ) ;
#55920 = CYLINDRICAL_SURFACE ( 'NONE', #5732, 7.499999999999988454 ) ;
#55921 = ORIENTED_EDGE ( 'NONE', *, *, #55390, .F. ) ;
#55922 =( BOUNDED_CURVE ( )  B_SPLINE_CURVE ( 3, ( #41874, #37199, #41205, #6004 ),
 .UNSPECIFIED., .F., .F. ) 
 B_SPLINE_CURVE_WITH_KNOTS ( ( 4, 4 ),
 ( 4.761198528795062224, 4.801918529528334645 ),
 .UNSPECIFIED. ) 
 CURVE ( )  GEOMETRIC_REPRESENTATION_ITEM ( )  RATIONAL_B_SPLINE_CURVE ( ( 1.000000000000000000, 0.9998618282348130659, 0.9998618282348130659, 1.000000000000000000 ) ) 
 REPRESENTATION_ITEM ( '' )  );
#55923 = CARTESIAN_POINT ( 'NONE',  ( 35.00000000000000000, 11.16627499335655216, 3.645068577060061266 ) ) ;
#55924 = CARTESIAN_POINT ( 'NONE',  ( -5.813762929211843122, -31.14503107144930638, -14.54886001617044222 ) ) ;
#55925 = CARTESIAN_POINT ( 'NONE',  ( 145.1370849898475797, 3.309064568108273190E-14, 0.000000000000000000 ) ) ;
#55926 = VERTEX_POINT ( 'NONE', #8499 ) ;
#55927 = B_SPLINE_CURVE_WITH_KNOTS ( 'NONE', 3,
 ( #50660, #19418, #40324, #10084, #55298, #5103, #9743, #50344, #44650, #55962, #60618, #15056, #19747, #35336, #30366, #25370 ),
 .UNSPECIFIED., .F., .F.,
 ( 4, 3, 3, 3, 3, 4 ),
 ( 0.000000000000000000, 0.0002999043160757478032, 0.0005998071753051258288, 0.0008997092107374931582, 0.001204458948194910874, 0.001510329163474998003 ),
 .UNSPECIFIED. ) ;
#55928 = EDGE_CURVE ( 'NONE', #43917, #33557, #48676, .T. ) ;
#55929 = ORIENTED_EDGE ( 'NONE', *, *, #30165, .F. ) ;
#55930 = CARTESIAN_POINT ( 'NONE',  ( 1.198791140419160683, -9.943044756148728069, 7.669598593075038551 ) ) ;
#55931 = ORIENTED_EDGE ( 'NONE', *, *, #25701, .F. ) ;
#55932 = CARTESIAN_POINT ( 'NONE',  ( -35.04709527796842394, -0.01117341439755767385, 0.005292201869320362073 ) ) ;
#55933 = EDGE_CURVE ( 'NONE', #9681, #48363, #32719, .T. ) ;
#55934 = CYLINDRICAL_SURFACE ( 'NONE', #59604, 5.000000000000000888 ) ;
#55935 = CARTESIAN_POINT ( 'NONE',  ( -25.00000000000000355, -3.797884998337192286, 23.99999999999999289 ) ) ;
#55936 = CARTESIAN_POINT ( 'NONE',  ( -23.47007829566609871, 4.659361080304749159, 0.3944522252365621484 ) ) ;
#55937 = CARTESIAN_POINT ( 'NONE',  ( 0.3654063281920715833, -12.27672420655579444, 0.2633658439602916124 ) ) ;
#55938 = CARTESIAN_POINT ( 'NONE',  ( 10.62696271159157568, 0.6044469518327795221, 11.98545746328775863 ) ) ;
#55939 = DIRECTION ( 'NONE',  ( 1.000000000000000000, 0.000000000000000000, -0.000000000000000000 ) ) ;
#55940 = CARTESIAN_POINT ( 'NONE',  ( 0.000000000000000000, 0.000000000000000000, 0.000000000000000000 ) ) ;
#55942 = ORIENTED_EDGE ( 'NONE', *, *, #29547, .T. ) ;
#55941 = CARTESIAN_POINT ( 'NONE',  ( -17.29244623348158783, 2.525873743887551814, -13.26159725786978072 ) ) ;
#55943 = CARTESIAN_POINT ( 'NONE',  ( 0.000000000000000000, 0.000000000000000000, 0.000000000000000000 ) ) ;
#55944 = ORIENTED_EDGE ( 'NONE', *, *, #52349, .F. ) ;
#55945 = DIRECTION ( 'NONE',  ( -1.000000000000000000, 0.000000000000000000, 0.000000000000000000 ) ) ;
#55946 = EDGE_LOOP ( 'NONE', ( #8606, #19859, #3628, #56345 ) ) ;
#55947 = CARTESIAN_POINT ( 'NONE',  ( 37.00000000000000711, 9.512294188640899151, -6.891188680298859559 ) ) ;
#55948 = ORIENTED_EDGE ( 'NONE', *, *, #42392, .F. ) ;
#55949 = CARTESIAN_POINT ( 'NONE',  ( 0.3057689695767479843, 8.055876362038343785, 9.241339546505109581 ) ) ;
#55950 = CARTESIAN_POINT ( 'NONE',  ( 35.00000000000000000, 10.49626516989280844, 7.238157050195512809 ) ) ;
#55951 = CARTESIAN_POINT ( 'NONE',  ( 0.3665391374699464300, -11.44911061034383515, -4.447929964102962153 ) ) ;
#55952 = CARTESIAN_POINT ( 'NONE',  ( 37.00000000000000711, -5.391785509271032062, -10.43555801961473861 ) ) ;
#55953 = EDGE_CURVE ( 'NONE', #55012, #59346, #65621, .T. ) ;
#55954 = CARTESIAN_POINT ( 'NONE',  ( 3.780834652287974773, 8.352030633203074927, -10.60629927458383470 ) ) ;
#55955 = ORIENTED_EDGE ( 'NONE', *, *, #62441, .T. ) ;
#55956 = B_SPLINE_CURVE_WITH_KNOTS ( 'NONE', 3,
 ( #42553, #37255, #20975, #11988, #57902, #41259, #46926, #62859, #57567, #46277, #22286, #47573, #11020, #41920, #2023, #25994 ),
 .UNSPECIFIED., .F., .F.,
 ( 4, 3, 3, 3, 3, 4 ),
 ( 0.000000000000000000, 0.0002176109881720306378, 0.0004352086762394722676, 0.0006528017811447081077, 0.0007615147961451940693, 0.0009453342004947466043 ),
 .UNSPECIFIED. ) ;
#55957 = CARTESIAN_POINT ( 'NONE',  ( 1.719304012340734378, -11.38834240361519612, -5.690355757825884986 ) ) ;
#55958 = EDGE_CURVE ( 'NONE', #28659, #41303, #20838, .T. ) ;
#55959 = ORIENTED_EDGE ( 'NONE', *, *, #36964, .F. ) ;
#55960 = DIRECTION ( 'NONE',  ( -1.000000000000000000, -0.000000000000000000, -0.000000000000000000 ) ) ;
#55961 = DIRECTION ( 'NONE',  ( 1.000000000000000000, 0.000000000000000000, -0.000000000000000000 ) ) ;
#55962 = CARTESIAN_POINT ( 'NONE',  ( 0.9296196016820552632, 12.19921892949952280, 2.573053270830167438 ) ) ;
#55963 = B_SPLINE_CURVE_WITH_KNOTS ( 'NONE', 3,
 ( #12772, #6499, #63000, #17462, #37734, #52391 ),
 .UNSPECIFIED., .F., .F.,
 ( 4, 2, 4 ),
 ( 0.004590869839051449006, 0.006605404212303630021, 0.008619938585555811036 ),
 .UNSPECIFIED. ) ;
#55964 = EDGE_LOOP ( 'NONE', ( #13963, #45067, #4515, #27617 ) ) ;
#55965 = CARTESIAN_POINT ( 'NONE',  ( -27.09364415740165200, -1.009938549038089661, 2.088137158971413943 ) ) ;
#55966 = CARTESIAN_POINT ( 'NONE',  ( 35.00000000000000000, -11.67026961469347768, -4.564151185897032725 ) ) ;
#55967 = CARTESIAN_POINT ( 'NONE',  ( 3.152665057734040488, 0.000000000000000000, 0.000000000000000000 ) ) ;
#55968 = CARTESIAN_POINT ( 'NONE',  ( 2.000000000000001776, 6.539067737394540281, -2.314222412769769033 ) ) ;
#55969 = EDGE_LOOP ( 'NONE', ( #50324, #6548, #18672, #54362 ) ) ;
#55970 = DIRECTION ( 'NONE',  ( 1.000000000000000000, 0.000000000000000000, -0.000000000000000000 ) ) ;
#55971 = LINE ( 'NONE', #9755, #61185 ) ;
#55972 = CARTESIAN_POINT ( 'NONE',  ( 1.287602823387597351, -3.781900355161777583, -12.00540336274513820 ) ) ;
#55973 = DIRECTION ( 'NONE',  ( -1.000000000000000000, 0.000000000000000000, 0.000000000000000000 ) ) ;
#55974 = CARTESIAN_POINT ( 'NONE',  ( 18.31241578173652940, -9.284453232853790539, 9.826491150957114229 ) ) ;
#55975 = EDGE_CURVE ( 'NONE', #16757, #65704, #28454, .T. ) ;
#55976 = VERTEX_POINT ( 'NONE', #14458 ) ;
#55977 = AXIS2_PLACEMENT_3D ( 'NONE', #3478, #62974, #53344 ) ;
#55978 = FACE_OUTER_BOUND ( 'NONE', #18788, .T. ) ;
#55979 = CARTESIAN_POINT ( 'NONE',  ( -1.734723475976807094E-15, -3.469446951953614189E-15, 12.00000000000000178 ) ) ;
#55980 = CARTESIAN_POINT ( 'NONE',  ( -35.00000000000000000, 0.000000000000000000, 0.000000000000000000 ) ) ;
#55981 = ORIENTED_EDGE ( 'NONE', *, *, #18836, .T. ) ;
#55982 = CARTESIAN_POINT ( 'NONE',  ( -18.56118279717487951, 4.671099544038118445, 11.05659470145910639 ) ) ;
#55983 = DIRECTION ( 'NONE',  ( 0.000000000000000000, 0.01356324068817998940, -0.9999080150203989437 ) ) ;
#55984 = ORIENTED_EDGE ( 'NONE', *, *, #11633, .T. ) ;
#55985 = ORIENTED_EDGE ( 'NONE', *, *, #789, .T. ) ;
#55986 = AXIS2_PLACEMENT_3D ( 'NONE', #8263, #49179, #43838 ) ;
#55987 = ORIENTED_EDGE ( 'NONE', *, *, #61191, .F. ) ;
#55988 = EDGE_CURVE ( 'NONE', #39732, #18175, #24130, .T. ) ;
#55989 = VERTEX_POINT ( 'NONE', #54732 ) ;
#55990 = CARTESIAN_POINT ( 'NONE',  ( 35.00000000000000000, 4.705694406421931860E-17, -3.469127814946512892E-15 ) ) ;
#55991 = CARTESIAN_POINT ( 'NONE',  ( 2.889800649504073782, -5.334644486274216391, 3.002151847318898170 ) ) ;
#55992 = CARTESIAN_POINT ( 'NONE',  ( -35.00000000000000000, -12.12087942037210553, 1.262958560998716617 ) ) ;
#55993 = CARTESIAN_POINT ( 'NONE',  ( -22.59983133926799681, -2.272383229042376662, -4.058100437359478008 ) ) ;
#55994 = CARTESIAN_POINT ( 'NONE',  ( -21.24030193723618609, 25.00000000000000000, -5.230344621181295395 ) ) ;
#55995 = CARTESIAN_POINT ( 'NONE',  ( -19.30028080049353179, -29.00000000000000000, 5.863682654924961213 ) ) ;
#55996 = DIRECTION ( 'NONE',  ( 0.000000000000000000, 0.1387779952735747890, -0.9903235168508558450 ) ) ;
#55998 = ORIENTED_EDGE ( 'NONE', *, *, #47388, .F. ) ;
#55997 = CYLINDRICAL_SURFACE ( 'NONE', #30843, 12.18649999999999878 ) ;
#55999 = CARTESIAN_POINT ( 'NONE',  ( 2.241528039335009215, -2.625917297988434651, 7.168649579907117264 ) ) ;
#56000 = EDGE_CURVE ( 'NONE', #58250, #29408, #29129, .T. ) ;
#56001 = EDGE_LOOP ( 'NONE', ( #20789, #4257, #33337, #25268 ) ) ;
#56002 = CARTESIAN_POINT ( 'NONE',  ( 0.3040950598368152291, -11.60568999039892191, -3.956873563689648154 ) ) ;
#56003 = ORIENTED_EDGE ( 'NONE', *, *, #10043, .T. ) ;
#56004 = ORIENTED_EDGE ( 'NONE', *, *, #8715, .T. ) ;
#56005 = CARTESIAN_POINT ( 'NONE',  ( -22.28284753389937123, -0.9231250029035025229, 3.581493264753373040 ) ) ;
#56006 = CARTESIAN_POINT ( 'NONE',  ( 13.91355800505865759, -33.59315906254626327, 9.938744394552985639 ) ) ;
#56007 = EDGE_CURVE ( 'NONE', #63926, #42135, #22111, .T. ) ;
#56008 = FACE_OUTER_BOUND ( 'NONE', #45462, .T. ) ;
#56009 = CARTESIAN_POINT ( 'NONE',  ( 2.000000000000001776, -3.805198749487460841, 5.799611601383201531 ) ) ;
#56010 = CARTESIAN_POINT ( 'NONE',  ( -35.00000000000000000, 2.080187960898735255, -12.57916205664478859 ) ) ;
#56011 = CARTESIAN_POINT ( 'NONE',  ( 0.2872850955227740921, -12.02931961709053077, 2.333231805482948840 ) ) ;
#56012 = ORIENTED_EDGE ( 'NONE', *, *, #30380, .F. ) ;
#56013 = ORIENTED_EDGE ( 'NONE', *, *, #14598, .T. ) ;
#56014 = CARTESIAN_POINT ( 'NONE',  ( 0.3675815128205894289, 12.04510820461659293, 2.391755495700645273 ) ) ;
#56015 = ORIENTED_EDGE ( 'NONE', *, *, #1523, .T. ) ;
#56016 = EDGE_LOOP ( 'NONE', ( #10630, #62107, #8967, #26073 ) ) ;
#56017 = CARTESIAN_POINT ( 'NONE',  ( 26.08439714455133185, 25.00000000000000000, 3.743551691817327942 ) ) ;
#56018 = CARTESIAN_POINT ( 'NONE',  ( -27.09602251845210930, -2.320865065108512759, 0.1644056400645283189 ) ) ;
#56019 = CARTESIAN_POINT ( 'NONE',  ( 2.241536586108911155, 1.331908602351639770, 7.517390684805875800 ) ) ;
#56020 = DIRECTION ( 'NONE',  ( -1.000000000000000000, 0.000000000000000000, 0.000000000000000000 ) ) ;
#56021 = CARTESIAN_POINT ( 'NONE',  ( -22.27719412087655471, 1.358750377066217929, -3.421752300520414014 ) ) ;
#56022 = EDGE_CURVE ( 'NONE', #4847, #23300, #64588, .T. ) ;
#56023 = CARTESIAN_POINT ( 'NONE',  ( -9.097493606629301510, -2.480532761269033770, -11.74397547306413259 ) ) ;
#56025 = VERTEX_POINT ( 'NONE', #9153 ) ;
#56024 = AXIS2_PLACEMENT_3D ( 'NONE', #17924, #58848, #22924 ) ;
#56026 = ORIENTED_EDGE ( 'NONE', *, *, #64842, .T. ) ;
#56027 = CARTESIAN_POINT ( 'NONE',  ( 2.000000000000001776, 0.000000000000000000, 0.000000000000000000 ) ) ;
#56028 = PLANE ( 'NONE',  #41409 ) ;
#56029 = CIRCLE ( 'NONE', #20992, 12.18650000000000411 ) ;
#56030 = CYLINDRICAL_SURFACE ( 'NONE', #46873, 5.000000000000000888 ) ;
#56031 = ADVANCED_FACE ( 'NONE', ( #29432 ), #49733, .T. ) ;
#56032 = CARTESIAN_POINT ( 'NONE',  ( -27.20164183316782314, -2.642567708136704052, 0.1019800881472514298 ) ) ;
#56033 = CARTESIAN_POINT ( 'NONE',  ( -37.00000000000000711, 7.717887834988368390, -8.854740511458771834 ) ) ;
#56034 = AXIS2_PLACEMENT_3D ( 'NONE', #49345, #58310, #58658 ) ;
#56035 = DIRECTION ( 'NONE',  ( -1.000000000000000000, 0.000000000000000000, 0.000000000000000000 ) ) ;
#56036 = CARTESIAN_POINT ( 'NONE',  ( 37.00000000000000711, 10.99909370905164430, 5.246972444133898072 ) ) ;
#56037 = CARTESIAN_POINT ( 'NONE',  ( -27.08418179957658722, -2.174042548349536919, -0.7235373421492772295 ) ) ;
#56038 = ORIENTED_EDGE ( 'NONE', *, *, #17299, .F. ) ;
#56039 = CARTESIAN_POINT ( 'NONE',  ( 2.770579946183334030, -0.3031629740256286953, 7.804957730865693222 ) ) ;
#56040 = DIRECTION ( 'NONE',  ( 0.000000000000000000, -0.01356324068817998940, 0.9999080150203990547 ) ) ;
#56041 = DIRECTION ( 'NONE',  ( 1.000000000000000000, -0.000000000000000000, 0.000000000000000000 ) ) ;
#56042 = FACE_OUTER_BOUND ( 'NONE', #12461, .T. ) ;
#56043 = CARTESIAN_POINT ( 'NONE',  ( 2.368238019615328316, -7.150288915654845034, 2.793778585134697678 ) ) ;
#56044 = EDGE_CURVE ( 'NONE', #38122, #58003, #35058, .T. ) ;
#56045 = ORIENTED_EDGE ( 'NONE', *, *, #6607, .F. ) ;
#56046 = CARTESIAN_POINT ( 'NONE',  ( 2.241449424704146320, -3.870245369721776019, -6.580749518451838753 ) ) ;
#56047 = CARTESIAN_POINT ( 'NONE',  ( 2.639814597422670328, 6.594772041715931898, 4.103563379978007575 ) ) ;
#56048 = CARTESIAN_POINT ( 'NONE',  ( 15.96609733983705226, -34.98269025770574103, -4.990963945245213473 ) ) ;
#56049 = VERTEX_POINT ( 'NONE', #15456 ) ;
#56050 = EDGE_CURVE ( 'NONE', #28763, #28121, #46618, .T. ) ;
#56051 = CARTESIAN_POINT ( 'NONE',  ( -22.27706485742869091, -0.9832726768967594566, 3.547445275915920071 ) ) ;
#56052 = CARTESIAN_POINT ( 'NONE',  ( 0.2638984909335716500, -12.24571285024408951, -0.1991813963115269814 ) ) ;
#56053 = CARTESIAN_POINT ( 'NONE',  ( 2.000000000000001776, 0.000000000000000000, 0.000000000000000000 ) ) ;
#56055 = ORIENTED_EDGE ( 'NONE', *, *, #13119, .T. ) ;
#56054 = FACE_OUTER_BOUND ( 'NONE', #32124, .T. ) ;
#56056 = LINE ( 'NONE', #36087, #33119 ) ;
#56057 = CIRCLE ( 'NONE', #32692, 12.18650000000000055 ) ;
#56058 = EDGE_CURVE ( 'NONE', #42804, #21758, #10458, .T. ) ;
#56059 = CARTESIAN_POINT ( 'NONE',  ( 11.74548640120467979, -8.775604215601116920, -8.184666801472349817 ) ) ;
#56060 = B_SPLINE_CURVE_WITH_KNOTS ( 'NONE', 3,
 ( #41112, #62375, #16836, #56086, #15836, #1233, #41437, #31481, #36114, #36796, #31159, #51778, #25849, #52442, #51121, #26484, #46138, #61728, #57091, #6880 ),
 .UNSPECIFIED., .F., .F.,
 ( 4, 2, 2, 2, 2, 2, 2, 2, 2, 4 ),
 ( 0.000000000000000000, 0.001253695096289122709, 0.001880542644433685039, 0.002507390192578247152, 0.003761085288867371812, 0.005014780385156495171, 0.006268475481445620265, 0.007522170577734745359, 0.008775865674023870452, 0.01002956077031299555 ),
 .UNSPECIFIED. ) ;
#56061 = VERTEX_POINT ( 'NONE', #19804 ) ;
#56062 = CARTESIAN_POINT ( 'NONE',  ( 0.2911222467163546157, 7.711756541611694438, 9.524109243547997039 ) ) ;
#56063 = DIRECTION ( 'NONE',  ( -1.000000000000000000, -0.000000000000000000, -0.000000000000000000 ) ) ;
#56064 = AXIS2_PLACEMENT_3D ( 'NONE', #52768, #7194, #23487 ) ;
#56065 = CARTESIAN_POINT ( 'NONE',  ( -27.10719052120871098, -2.295785794152564563, -0.5475695427849640584 ) ) ;
#56066 = CARTESIAN_POINT ( 'NONE',  ( 1.198791140420482959, -1.670544840357492955, -12.44572864632847953 ) ) ;
#56067 = CARTESIAN_POINT ( 'NONE',  ( 8.437200413559441614, 4.476360154859202467, -12.73625532737110966 ) ) ;
#56068 = CARTESIAN_POINT ( 'NONE',  ( -17.50119111604729483, 2.686101418262018647, 13.23107945010674413 ) ) ;
#56069 = CARTESIAN_POINT ( 'NONE',  ( 0.2655924914740778187, 10.58356227062109411, 6.161287456391719708 ) ) ;
#56070 = VECTOR ( 'NONE', #61327, 1000.000000000000000 ) ;
#56071 = ORIENTED_EDGE ( 'NONE', *, *, #39569, .T. ) ;
#56072 = DIRECTION ( 'NONE',  ( -1.000000000000000000, 0.000000000000000000, 0.000000000000000000 ) ) ;
#56073 = ORIENTED_EDGE ( 'NONE', *, *, #58242, .T. ) ;
#56074 = AXIS2_PLACEMENT_3D ( 'NONE', #41295, #12933, #61580 ) ;
#56075 = DIRECTION ( 'NONE',  ( 1.000000000000000000, 0.000000000000000000, 0.000000000000000000 ) ) ;
#56076 = CYLINDRICAL_SURFACE ( 'NONE', #48611, 1.399999999999999911 ) ;
#56077 = CARTESIAN_POINT ( 'NONE',  ( 2.717984159219991369, 1.631703089060316136, 7.620583877640733306 ) ) ;
#56078 = EDGE_CURVE ( 'NONE', #36827, #21425, #60417, .T. ) ;
#56079 = CARTESIAN_POINT ( 'NONE',  ( 0.2646305136544072623, 4.064188116014705976, -11.55263159009954421 ) ) ;
#56080 = VERTEX_POINT ( 'NONE', #15767 ) ;
#56081 = FACE_OUTER_BOUND ( 'NONE', #28186, .T. ) ;
#56082 = CARTESIAN_POINT ( 'NONE',  ( 11.37704067788454942, 11.83906243856773344, -1.962618476695794589 ) ) ;
#56083 = DIRECTION ( 'NONE',  ( 1.000000000000000000, 0.000000000000000000, 0.000000000000000000 ) ) ;
#56084 = ORIENTED_EDGE ( 'NONE', *, *, #52671, .F. ) ;
#56085 = ORIENTED_EDGE ( 'NONE', *, *, #53772, .F. ) ;
#56086 = CARTESIAN_POINT ( 'NONE',  ( 27.22053583440688840, -12.68463422843485056, 4.622893925193950260 ) ) ;
#56087 = ORIENTED_EDGE ( 'NONE', *, *, #13054, .F. ) ;
#56088 = CARTESIAN_POINT ( 'NONE',  ( 24.73855084333399290, -8.970947471680776886, -7.973041315719463284 ) ) ;
#56089 = CARTESIAN_POINT ( 'NONE',  ( 35.00000000000000000, 4.705694406421931860E-17, -3.469127814946512892E-15 ) ) ;
#56090 = CARTESIAN_POINT ( 'NONE',  ( -27.10422407540562517, 2.346206748218702121, -0.1544383239736422664 ) ) ;
#56091 = DIRECTION ( 'NONE',  ( 0.3865475372811021382, 0.3335716741247249928, -0.8598319252293108450 ) ) ;
#56092 = CARTESIAN_POINT ( 'NONE',  ( 9.650011408859196393, 13.48023745212357838, -0.7481333718491257612 ) ) ;
#56093 = CARTESIAN_POINT ( 'NONE',  ( 0.2652384529303147276, -10.57229402027111931, 6.180212112237623678 ) ) ;
#56094 = LINE ( 'NONE', #9893, #14194 ) ;
#56095 = ORIENTED_EDGE ( 'NONE', *, *, #64037, .T. ) ;
#56096 = CARTESIAN_POINT ( 'NONE',  ( 3.152665057734040488, 0.000000000000000000, 0.000000000000000000 ) ) ;
#56097 = VECTOR ( 'NONE', #8840, 1000.000000000000000 ) ;
#56098 = DIRECTION ( 'NONE',  ( 1.000000000000000000, 0.000000000000000000, 0.000000000000000000 ) ) ;
#56099 = LINE ( 'NONE', #26186, #39126 ) ;
#56100 = CARTESIAN_POINT ( 'NONE',  ( -27.05874794189610455, 1.734723475976807094E-15, -8.673617379884035472E-15 ) ) ;
#56101 = CARTESIAN_POINT ( 'NONE',  ( -37.00000000000000711, 0.000000000000000000, 0.000000000000000000 ) ) ;
#56102 = CARTESIAN_POINT ( 'NONE',  ( 0.2801149460245125344, -10.70654700624298883, -5.954809120985829374 ) ) ;
#56103 = DIRECTION ( 'NONE',  ( -0.9606638835031803270, 0.07465901992590978642, -0.2674900627617606830 ) ) ;
#56104 = CARTESIAN_POINT ( 'NONE',  ( 0.3537226245948383307, 9.233810598191778851, 8.088784578751326393 ) ) ;
#56105 = CIRCLE ( 'NONE', #14647, 5.000000000000001776 ) ;
#56106 = EDGE_CURVE ( 'NONE', #4994, #46189, #10475, .T. ) ;
#56107 = ORIENTED_EDGE ( 'NONE', *, *, #44325, .F. ) ;
#56108 = CARTESIAN_POINT ( 'NONE',  ( 11.74548640120467979, 10.73597826697114677, -8.184666801472349817 ) ) ;
#56109 = CIRCLE ( 'NONE', #51871, 7.499999999999988454 ) ;
#56110 = CIRCLE ( 'NONE', #64601, 5.000000000000000888 ) ;
#56111 =( BOUNDED_CURVE ( )  B_SPLINE_CURVE ( 3, ( #32287, #52605, #47596, #2039 ),
 .UNSPECIFIED., .F., .F. ) 
 B_SPLINE_CURVE_WITH_KNOTS ( ( 4, 4 ),
 ( 1.213047816902216081, 1.252925267387245523 ),
 .UNSPECIFIED. ) 
 CURVE ( )  GEOMETRIC_REPRESENTATION_ITEM ( )  RATIONAL_B_SPLINE_CURVE ( ( 1.000000000000000000, 0.9998674868020707152, 0.9998674868020707152, 1.000000000000000000 ) ) 
 REPRESENTATION_ITEM ( '' )  );
#56112 = VERTEX_POINT ( 'NONE', #40060 ) ;
#56113 = CARTESIAN_POINT ( 'NONE',  ( 0.2650492433740069820, 0.1101179680248975945, 12.24562113162318866 ) ) ;
#56114 = DIRECTION ( 'NONE',  ( 1.000000000000000000, 0.000000000000000000, -0.000000000000000000 ) ) ;
#56115 = CARTESIAN_POINT ( 'NONE',  ( 0.2653519890518167834, -12.06014856238022226, 2.126538543978039542 ) ) ;
#56116 = CARTESIAN_POINT ( 'NONE',  ( 2.257661810676208081, 2.485866587321733601, -7.224098098130338208 ) ) ;
#56117 = EDGE_LOOP ( 'NONE', ( #34865, #12720, #40325, #17745 ) ) ;
#56118 = CARTESIAN_POINT ( 'NONE',  ( 2.000000000000001776, -5.814643797626954935, 3.550179297009551149 ) ) ;
#56119 = CARTESIAN_POINT ( 'NONE',  ( 2.263328370261528555, -3.697218830763996600, 6.687792802426776539 ) ) ;
#56120 = CARTESIAN_POINT ( 'NONE',  ( 0.5572780756284287929, -12.20533540249709148, 1.841882550626854131 ) ) ;
#56121 = CIRCLE ( 'NONE', #43392, 12.18650000000000055 ) ;
#56122 = DIRECTION ( 'NONE',  ( -0.4531421102008652557, 0.000000000000000000, -0.8914382917301156839 ) ) ;
#56123 = EDGE_CURVE ( 'NONE', #2304, #35366, #13663, .T. ) ;
#56124 = CARTESIAN_POINT ( 'NONE',  ( -17.13751750617693403, -7.344255242515008497, 9.496604519765444508 ) ) ;
#56125 = FACE_OUTER_BOUND ( 'NONE', #11350, .T. ) ;
#56126 = ORIENTED_EDGE ( 'NONE', *, *, #49992, .F. ) ;
#56127 = EDGE_CURVE ( 'NONE', #3146, #23034, #27476, .T. ) ;
#56128 = DIRECTION ( 'NONE',  ( 0.000000000000000000, -0.01356324068817998940, 0.9999080150203990547 ) ) ;
#56129 = ORIENTED_EDGE ( 'NONE', *, *, #48292, .F. ) ;
#56130 = ADVANCED_FACE ( 'NONE', ( #174 ), #55710, .T. ) ;
#56131 = DIRECTION ( 'NONE',  ( -1.000000000000000000, 0.000000000000000000, 0.000000000000000000 ) ) ;
#56132 = CARTESIAN_POINT ( 'NONE',  ( 2.241451721903215066, 7.153019588493075176, 2.668222118333474224 ) ) ;
#56133 = CARTESIAN_POINT ( 'NONE',  ( 28.96537032880950591, -9.359309874800233686, 7.513625803917611812 ) ) ;
#56134 = CARTESIAN_POINT ( 'NONE',  ( -10.76005699428653806, -6.156792290948529534, 10.30836155159126299 ) ) ;
#56135 = VECTOR ( 'NONE', #33949, 1000.000000000000000 ) ;
#56136 = EDGE_LOOP ( 'NONE', ( #56172, #42081, #40195, #13559 ) ) ;
#56138 = ORIENTED_EDGE ( 'NONE', *, *, #17173, .T. ) ;
#56137 = EDGE_CURVE ( 'NONE', #52670, #1326, #26418, .T. ) ;
#56139 = CARTESIAN_POINT ( 'NONE',  ( 10.75853767213705225, 7.830989516993144051, -10.99661780661415733 ) ) ;
#56140 = ORIENTED_EDGE ( 'NONE', *, *, #38746, .T. ) ;
#56141 = CARTESIAN_POINT ( 'NONE',  ( 1.719304012338439325, 7.017415949612858306, 10.62216384465677521 ) ) ;
#56142 = DIRECTION ( 'NONE',  ( 0.3939253465568944290, -0.9034404741085553248, -0.1691689424289794796 ) ) ;
#56143 = DIRECTION ( 'NONE',  ( 0.000000000000000000, 0.01356324068817998940, -0.9999080150203990547 ) ) ;
#56144 = CYLINDRICAL_SURFACE ( 'NONE', #1433, 12.18649999999999878 ) ;
#56145 = CARTESIAN_POINT ( 'NONE',  ( 2.350038591458111892, -5.855794476068393983, 8.861946706685715824 ) ) ;
#56146 = EDGE_CURVE ( 'NONE', #42786, #42779, #30734, .T. ) ;
#56147 = FACE_OUTER_BOUND ( 'NONE', #51388, .T. ) ;
#56148 = DIRECTION ( 'NONE',  ( 0.000000000000000000, 0.000000000000000000, 1.000000000000000000 ) ) ;
#56149 = ORIENTED_EDGE ( 'NONE', *, *, #37821, .T. ) ;
#56150 = CARTESIAN_POINT ( 'NONE',  ( -7.594202851097166196, -6.461772726810069756, -10.13291195006097745 ) ) ;
#56151 = ORIENTED_EDGE ( 'NONE', *, *, #29958, .T. ) ;
#56152 = CARTESIAN_POINT ( 'NONE',  ( -22.27716857039623477, 2.496432241075919212, 2.705892286796375945 ) ) ;
#56153 = CARTESIAN_POINT ( 'NONE',  ( 0.2671309869109484425, -9.276621593297562640, 7.995521393275787148 ) ) ;
#56154 = VECTOR ( 'NONE', #55510, 1000.000000000000114 ) ;
#56155 = CARTESIAN_POINT ( 'NONE',  ( -27.09364415740165910, 1.918701019213897574, -1.303410551736464917 ) ) ;
#56156 = ORIENTED_EDGE ( 'NONE', *, *, #16756, .F. ) ;
#56157 = ADVANCED_FACE ( 'NONE', ( #21094 ), #35110, .F. ) ;
#56158 = CARTESIAN_POINT ( 'NONE',  ( -22.27711653538342773, 3.657713416444739352, -0.4190680140413353127 ) ) ;
#56160 = ORIENTED_EDGE ( 'NONE', *, *, #54038, .F. ) ;
#56159 = AXIS2_PLACEMENT_3D ( 'NONE', #24009, #18706, #19682 ) ;
#56161 = DIRECTION ( 'NONE',  ( 0.000000000000000000, 0.6943713148249588407, -0.7196168960969844264 ) ) ;
#56162 = DIRECTION ( 'NONE',  ( -0.000000000000000000, -0.000000000000000000, -1.000000000000000000 ) ) ;
#56163 = DIRECTION ( 'NONE',  ( -1.000000000000000000, 0.000000000000000000, 0.000000000000000000 ) ) ;
#56164 = CARTESIAN_POINT ( 'NONE',  ( 2.907497136250587033, 7.252103438786942746, -3.021847490615504839 ) ) ;
#56165 = ORIENTED_EDGE ( 'NONE', *, *, #64731, .T. ) ;
#56167 = EDGE_CURVE ( 'NONE', #41839, #7978, #51950, .T. ) ;
#56166 = ORIENTED_EDGE ( 'NONE', *, *, #23182, .F. ) ;
#56168 = AXIS2_PLACEMENT_3D ( 'NONE', #31801, #56795, #57423 ) ;
#56169 = DIRECTION ( 'NONE',  ( 0.000000000000000000, -0.01356324068818000328, 0.9999080150203990547 ) ) ;
#56170 = VERTEX_POINT ( 'NONE', #30422 ) ;
#56171 = CARTESIAN_POINT ( 'NONE',  ( -28.41827485489077532, 3.509237424706437292, -11.47541949982828413 ) ) ;
#56172 = ORIENTED_EDGE ( 'NONE', *, *, #59985, .F. ) ;
#56173 = ORIENTED_EDGE ( 'NONE', *, *, #51761, .F. ) ;
#56174 = AXIS2_PLACEMENT_3D ( 'NONE', #47701, #53011, #2144 ) ;
#56175 = ORIENTED_EDGE ( 'NONE', *, *, #39769, .T. ) ;
#56176 = CYLINDRICAL_SURFACE ( 'NONE', #46887, 3.594603870727467676 ) ;
#56177 = CARTESIAN_POINT ( 'NONE',  ( 10.63650944684269994, -26.92414420718871426, 13.64813004266018481 ) ) ;
#56178 = DIRECTION ( 'NONE',  ( 1.000000000000000000, 0.000000000000000000, 0.000000000000000000 ) ) ;
#56179 = DIRECTION ( 'NONE',  ( -0.000000000000000000, -1.000000000000000000, -0.000000000000000000 ) ) ;
#56180 = CARTESIAN_POINT ( 'NONE',  ( 22.00000000000000711, -20.00000000000000000, 2.449293598294706907E-15 ) ) ;
#56181 = VERTEX_POINT ( 'NONE', #30095 ) ;
#56182 = CARTESIAN_POINT ( 'NONE',  ( -25.86628395826706850, -5.139808748864358456, 10.84354029019568522 ) ) ;
#56183 = ORIENTED_EDGE ( 'NONE', *, *, #64329, .T. ) ;
#56184 = DIRECTION ( 'NONE',  ( -1.000000000000000000, 0.000000000000000000, 0.000000000000000000 ) ) ;
#56185 = DIRECTION ( 'NONE',  ( 0.000000000000000000, -1.000000000000000000, 0.000000000000000000 ) ) ;
#56186 = DIRECTION ( 'NONE',  ( 1.000000000000000000, -0.000000000000000000, 0.000000000000000000 ) ) ;
#56187 = CARTESIAN_POINT ( 'NONE',  ( 0.3665391374699467075, 6.368473106897276637, -10.50279796150430123 ) ) ;
#56188 = CARTESIAN_POINT ( 'NONE',  ( 3.152665057734104437, -3.546019893116280741, -7.102135024645891193 ) ) ;
#56189 = CARTESIAN_POINT ( 'NONE',  ( 2.835339799623983748, -7.825540862019406241, -0.3287452556171494011 ) ) ;
#56190 = ADVANCED_FACE ( 'NONE', ( #50403 ), #40731, .T. ) ;
#56191 = ADVANCED_FACE ( 'NONE', ( #36399 ), #45382, .T. ) ;
#56192 = CIRCLE ( 'NONE', #2041, 2.899999999999997247 ) ;
#56193 = ORIENTED_EDGE ( 'NONE', *, *, #16948, .F. ) ;
#56194 = CARTESIAN_POINT ( 'NONE',  ( 35.00000000000000000, 9.493370459201798894, 6.917234959366719060 ) ) ;
#56195 = ORIENTED_EDGE ( 'NONE', *, *, #21624, .F. ) ;
#56196 = CARTESIAN_POINT ( 'NONE',  ( -38.56928140186734311, -26.58605982982061633, -4.500000000000001776 ) ) ;
#56197 =( LENGTH_UNIT ( ) NAMED_UNIT ( * ) SI_UNIT ( .MILLI., .METRE. ) );
#56198 = CARTESIAN_POINT ( 'NONE',  ( 10.33711885797364083, -13.43829105577338190, -1.303661106969844274 ) ) ;
#56199 = CARTESIAN_POINT ( 'NONE',  ( 2.430348790457064201, 4.016278121583625627, 6.566563360302290597 ) ) ;
#56200 = CARTESIAN_POINT ( 'NONE',  ( 37.00000000000000711, 4.705694406421931860E-17, -3.469127814946512892E-15 ) ) ;
#56201 = ORIENTED_EDGE ( 'NONE', *, *, #20418, .F. ) ;
#56202 = ADVANCED_FACE ( 'NONE', ( #62625 ), #42669, .F. ) ;
#56203 = LINE ( 'NONE', #1356, #6935 ) ;
#56204 = CARTESIAN_POINT ( 'NONE',  ( 1.547277799339724202, 5.744300480442041668, -11.29700934613367558 ) ) ;
#56205 = CARTESIAN_POINT ( 'NONE',  ( 22.04496710003973803, 10.54007463054590232, -5.749627913936380175 ) ) ;
#56206 = CARTESIAN_POINT ( 'NONE',  ( 22.36482863261543486, -13.46837713145126791, -0.9234811557364140944 ) ) ;
#56207 = CIRCLE ( 'NONE', #49855, 12.75000000000000178 ) ;
#56208 = EDGE_CURVE ( 'NONE', #31482, #4661, #40188, .T. ) ;
#56209 = CIRCLE ( 'NONE', #10583, 5.000000000000000000 ) ;
#56210 = CARTESIAN_POINT ( 'NONE',  ( 0.3632410797595229113, 12.27601307605977610, -0.2628628737173892005 ) ) ;
#56211 = DIRECTION ( 'NONE',  ( 1.000000000000000000, -0.000000000000000000, 0.000000000000000000 ) ) ;
#56212 = EDGE_CURVE ( 'NONE', #59369, #34055, #23265, .T. ) ;
#56213 = CARTESIAN_POINT ( 'NONE',  ( 5.536195898058073439, 0.0002547682446687991073, -0.008496323383586253108 ) ) ;
#56214 = CARTESIAN_POINT ( 'NONE',  ( 5.530133899448235191, 0.003876417824003443660, -0.01550764871776217670 ) ) ;
#56215 = DIRECTION ( 'NONE',  ( -1.000000000000000000, -0.000000000000000000, 0.000000000000000000 ) ) ;
#56216 = AXIS2_PLACEMENT_3D ( 'NONE', #9968, #50545, #30250 ) ;
#56217 = VERTEX_POINT ( 'NONE', #58006 ) ;
#56218 = AXIS2_PLACEMENT_3D ( 'NONE', #56880, #25612, #20294 ) ;
#56219 = ORIENTED_EDGE ( 'NONE', *, *, #26485, .T. ) ;
#56220 = DIRECTION ( 'NONE',  ( 1.000000000000000000, 0.000000000000000000, 0.000000000000000000 ) ) ;
#56221 = CARTESIAN_POINT ( 'NONE',  ( 32.70177428389710172, -2.904144763113409411, -22.74422317523287163 ) ) ;
#56222 = FACE_OUTER_BOUND ( 'NONE', #29732, .T. ) ;
#56223 = EDGE_CURVE ( 'NONE', #52684, #31963, #4134, .T. ) ;
#56224 = CARTESIAN_POINT ( 'NONE',  ( -36.00000000000000711, 12.73293890771483383, 0.6593684648220944355 ) ) ;
#56225 = EDGE_LOOP ( 'NONE', ( #11352, #46632, #4643, #59785 ) ) ;
#56226 = EDGE_CURVE ( 'NONE', #57752, #42222, #27719, .T. ) ;
#56227 = ORIENTED_EDGE ( 'NONE', *, *, #42655, .T. ) ;
#56228 = VERTEX_POINT ( 'NONE', #12416 ) ;
#56229 = CARTESIAN_POINT ( 'NONE',  ( -27.28563798457900447, 2.896153581097023366, 0.04047623855284953470 ) ) ;
#56230 = ADVANCED_FACE ( 'NONE', ( #12746 ), #52688, .T. ) ;
#56232 = CARTESIAN_POINT ( 'NONE',  ( -35.00000000000000000, -0.3025107581132014389, 11.74226168163341200 ) ) ;
#56231 = CIRCLE ( 'NONE', #62577, 5.000000000000000000 ) ;
#56233 = ORIENTED_EDGE ( 'NONE', *, *, #58368, .T. ) ;
#56234 = EDGE_CURVE ( 'NONE', #31673, #62587, #47688, .T. ) ;
#56235 = CARTESIAN_POINT ( 'NONE',  ( 2.305787727787083519, -2.461236246751120849, 7.249469779319902329 ) ) ;
#56236 = DIRECTION ( 'NONE',  ( 0.000000000000000000, 0.8169148498130255343, -0.5767582926624997830 ) ) ;
#56237 = ORIENTED_EDGE ( 'NONE', *, *, #5145, .T. ) ;
#56238 = CARTESIAN_POINT ( 'NONE',  ( 2.305787727787084407, 4.792270232040973355, -5.970480882365174047 ) ) ;
#56239 = CIRCLE ( 'NONE', #54114, 12.75000000000000178 ) ;
#56240 = CARTESIAN_POINT ( 'NONE',  ( 11.32820571420733735, -29.68697874620919563, -9.642237626533519901 ) ) ;
#56241 = DIRECTION ( 'NONE',  ( 0.000000000000000000, -0.01356324068817992175, 0.9999080150203990547 ) ) ;
#56242 = ORIENTED_EDGE ( 'NONE', *, *, #51060, .F. ) ;
#56243 = EDGE_CURVE ( 'NONE', #48365, #16579, #45510, .T. ) ;
#56244 = CYLINDRICAL_SURFACE ( 'NONE', #8711, 2.899999999999994582 ) ;
#56245 = ORIENTED_EDGE ( 'NONE', *, *, #60288, .T. ) ;
#56246 = CARTESIAN_POINT ( 'NONE',  ( -37.00000000000000711, 9.196955404009424129, -8.830544224262844466 ) ) ;
#56247 = VERTEX_POINT ( 'NONE', #22759 ) ;
#56248 = CARTESIAN_POINT ( 'NONE',  ( 13.40667394824980896, -10.89379735224136603, -5.037499513965738807 ) ) ;
#56249 = AXIS2_PLACEMENT_3D ( 'NONE', #4660, #65778, #60825 ) ;
#56250 = CARTESIAN_POINT ( 'NONE',  ( -5.596759081073452435, -31.66776075797034196, 13.71641508080542771 ) ) ;
#56251 = CARTESIAN_POINT ( 'NONE',  ( 2.305787727787084407, 3.971363876083963351, 6.545285700970541853 ) ) ;
#56252 = DIRECTION ( 'NONE',  ( -1.000000000000000000, 0.000000000000000000, 0.000000000000000000 ) ) ;
#56253 = DIRECTION ( 'NONE',  ( -1.000000000000000000, 0.000000000000000000, 0.000000000000000000 ) ) ;
#56254 = CARTESIAN_POINT ( 'NONE',  ( 37.00000000000000711, 4.705694406421931860E-17, -3.469127814946512892E-15 ) ) ;
#56255 = CARTESIAN_POINT ( 'NONE',  ( -35.00000000000000000, -7.251710744571512102, -9.240395740215712195 ) ) ;
#56256 = CYLINDRICAL_SURFACE ( 'NONE', #26716, 12.74999999999999822 ) ;
#56258 = ORIENTED_EDGE ( 'NONE', *, *, #49628, .T. ) ;
#56257 = CARTESIAN_POINT ( 'NONE',  ( 2.000000000000001776, 6.338823199656684615, 2.816798305433696470 ) ) ;
#56259 = AXIS2_PLACEMENT_3D ( 'NONE', #49858, #19918, #33897 ) ;
#56260 = DIRECTION ( 'NONE',  ( 0.000000000000000000, 0.000000000000000000, 1.000000000000000000 ) ) ;
#56261 = EDGE_LOOP ( 'NONE', ( #50025, #12257, #24078, #63075 ) ) ;
#56262 = DIRECTION ( 'NONE',  ( 0.000000000000000000, -0.01356324068817999114, 0.9999080150203989437 ) ) ;
#56263 = CARTESIAN_POINT ( 'NONE',  ( 2.639814597422741382, -5.782006333156036959, -5.186391178752193909 ) ) ;
#56264 = VERTEX_POINT ( 'NONE', #27080 ) ;
#56265 = CARTESIAN_POINT ( 'NONE',  ( 24.97568612634365692, 8.683198485571637093, -8.285225425757136719 ) ) ;
#56266 = DIRECTION ( 'NONE',  ( 0.000000000000000000, -0.01356324068817999114, 0.9999080150203989437 ) ) ;
#56267 = CIRCLE ( 'NONE', #10593, 5.000000000000000000 ) ;
#56268 = CARTESIAN_POINT ( 'NONE',  ( -27.09833916700227263, -2.238843247505192480, 0.6583442518269273513 ) ) ;
#56269 = DIRECTION ( 'NONE',  ( -1.000000000000000000, 0.000000000000000000, 0.000000000000000000 ) ) ;
#56270 = CARTESIAN_POINT ( 'NONE',  ( 2.247112776669945244, 7.214825360829727252, 2.501955819910834933 ) ) ;
#56271 = EDGE_CURVE ( 'NONE', #32582, #37450, #33833, .T. ) ;
#56272 = ORIENTED_EDGE ( 'NONE', *, *, #39656, .T. ) ;
#56273 = CARTESIAN_POINT ( 'NONE',  ( -17.50773065187699018, -5.755997118861490236, -10.53071770204327251 ) ) ;
#56274 = ORIENTED_EDGE ( 'NONE', *, *, #42596, .F. ) ;
#56275 = B_SPLINE_CURVE_WITH_KNOTS ( 'NONE', 3,
 ( #46845, #16912, #63120, #7593, #63430, #58141, #11275, #62448, #22900, #26894, #62141, #37850, #47197, #26556, #17899, #11914 ),
 .UNSPECIFIED., .F., .F.,
 ( 4, 3, 3, 3, 3, 4 ),
 ( 0.000000000000000000, 0.0002999043160757648252, 0.0005998071753051594391, 0.0008997092107375431400, 0.001204458948196864606, 0.001510329163478875110 ),
 .UNSPECIFIED. ) ;
#56276 = DIRECTION ( 'NONE',  ( 1.000000000000000000, 0.000000000000000000, 0.000000000000000000 ) ) ;
#56277 = CARTESIAN_POINT ( 'NONE',  ( -27.01437459610461644, 25.00000000000000000, -2.220455681983952267 ) ) ;
#56278 = CARTESIAN_POINT ( 'NONE',  ( 0.2650492594609233921, -7.786980091309387397, -9.451471004987412883 ) ) ;
#56279 = ORIENTED_EDGE ( 'NONE', *, *, #31502, .F. ) ;
#56280 = EDGE_CURVE ( 'NONE', #51182, #19771, #21140, .T. ) ;
#56281 = CARTESIAN_POINT ( 'NONE',  ( 0.3164563675027650125, -4.419430877662271051, -11.43920928915629176 ) ) ;
#56282 = AXIS2_PLACEMENT_3D ( 'NONE', #6345, #42533, #2692 ) ;
#56283 = AXIS2_PLACEMENT_3D ( 'NONE', #34097, #3566, #39094 ) ;
#56284 = CARTESIAN_POINT ( 'NONE',  ( -35.05175862995318425, 0.005323180402356034180, -0.01139565579897153236 ) ) ;
#56285 = CARTESIAN_POINT ( 'NONE',  ( 48.71973356879950501, -0.2586908456632806552, 8.066649094095312833 ) ) ;
#56286 = DIRECTION ( 'NONE',  ( -1.000000000000000000, 0.000000000000000000, 0.000000000000000000 ) ) ;
#56287 = CARTESIAN_POINT ( 'NONE',  ( 0.3106921474978474040, -5.925601485921598410, -10.73438344699978231 ) ) ;
#56289 = ORIENTED_EDGE ( 'NONE', *, *, #54987, .F. ) ;
#56288 = EDGE_CURVE ( 'NONE', #43782, #47123, #12614, .T. ) ;
#56290 = CARTESIAN_POINT ( 'NONE',  ( 0.2653519890518143964, 2.126521162241218565, -12.06015162724940026 ) ) ;
#56291 = DIRECTION ( 'NONE',  ( 0.000000000000000000, 0.000000000000000000, 1.000000000000000000 ) ) ;
#56292 = CARTESIAN_POINT ( 'NONE',  ( 0.7446945582524610030, -3.906659168236780388, -11.77484212699384614 ) ) ;
#56293 = EDGE_CURVE ( 'NONE', #48492, #35533, #41288, .T. ) ;
#56294 = CARTESIAN_POINT ( 'NONE',  ( -15.21621911491949319, 7.970342840283608510, 10.89608346908821446 ) ) ;
#56295 = CARTESIAN_POINT ( 'NONE',  ( 19.28625800530497258, -6.413918128308385036, 11.87904264843581537 ) ) ;
#56296 =( BOUNDED_SURFACE ( )  B_SPLINE_SURFACE ( 3, 1, ( 
 ( #46762, #1874 ),
 ( #21505, #16517 ),
 ( #32754, #11509 ),
 ( #47437, #62066 ) ),
 .UNSPECIFIED., .F., .F., .F. ) 
 B_SPLINE_SURFACE_WITH_KNOTS ( ( 4, 4 ),
 ( 2, 2 ),
 ( 0.000000000000000000, 1.000000000000000000 ),
 ( 0.000000000000000000, 1.000000000000000000 ),
 .UNSPECIFIED. ) 
 GEOMETRIC_REPRESENTATION_ITEM ( )  RATIONAL_B_SPLINE_SURFACE ( (
 ( 1.000000000000000000, 1.000000000000000000),
 ( 0.6933888150995267674, 0.9895912004443193632),
 ( 0.6933888150995267674, 0.9895912004443193632),
 ( 1.000000000000000000, 1.000000000000000000) ) ) 
 REPRESENTATION_ITEM ( '' )  SURFACE ( )  );
#56297 = ORIENTED_EDGE ( 'NONE', *, *, #19231, .T. ) ;
#56298 = LINE ( 'NONE', #11091, #31080 ) ;
#56299 = FACE_OUTER_BOUND ( 'NONE', #23971, .T. ) ;
#56300 = CARTESIAN_POINT ( 'NONE',  ( -22.27719381268171617, 3.561499689648256251, -0.9326100520993079179 ) ) ;
#56301 = ORIENTED_EDGE ( 'NONE', *, *, #41595, .T. ) ;
#56302 = CARTESIAN_POINT ( 'NONE',  ( 2.257661810676420355, -6.547845034191119851, 3.936095962955278527 ) ) ;
#56303 = DIRECTION ( 'NONE',  ( 0.000000000000000000, 0.01356324068817992175, -0.9999080150203990547 ) ) ;
#56304 = ORIENTED_EDGE ( 'NONE', *, *, #20271, .F. ) ;
#56305 = CIRCLE ( 'NONE', #27640, 7.499999999999988454 ) ;
#56306 = ORIENTED_EDGE ( 'NONE', *, *, #30204, .F. ) ;
#56307 = ORIENTED_EDGE ( 'NONE', *, *, #60114, .T. ) ;
#56308 = EDGE_CURVE ( 'NONE', #13765, #34180, #38107, .T. ) ;
#56309 = CARTESIAN_POINT ( 'NONE',  ( -27.08429572838383947, -1.632445743623433421, 1.608131779585712406 ) ) ;
#56310 = ORIENTED_EDGE ( 'NONE', *, *, #43276, .F. ) ;
#56311 = EDGE_CURVE ( 'NONE', #30052, #82, #43420, .T. ) ;
#56312 = CARTESIAN_POINT ( 'NONE',  ( 0.000000000000000000, 3.341639490130849488, -6.078525953551423555 ) ) ;
#56313 = CARTESIAN_POINT ( 'NONE',  ( -22.29195009621226475, -3.580440466953070278, 1.030739959031457209 ) ) ;
#56314 = CARTESIAN_POINT ( 'NONE',  ( 2.000000000000001776, 2.664846396702580833, -6.404188155572981600 ) ) ;
#56315 = CIRCLE ( 'NONE', #36176, 12.75000000000000178 ) ;
#56316 = CYLINDRICAL_SURFACE ( 'NONE', #31153, 6.936499999999988120 ) ;
#56317 = ORIENTED_EDGE ( 'NONE', *, *, #25990, .T. ) ;
#56318 = DIRECTION ( 'NONE',  ( 0.000000000000000000, 0.000000000000000000, -1.000000000000000000 ) ) ;
#56319 = CARTESIAN_POINT ( 'NONE',  ( -13.50035326695106797, -34.20038524408859359, 9.091202907900893138 ) ) ;
#56320 = CARTESIAN_POINT ( 'NONE',  ( -35.00000000000000000, 12.16893194857549965, 3.805206332242515366 ) ) ;
#56322 = ORIENTED_EDGE ( 'NONE', *, *, #61455, .F. ) ;
#56321 = LINE ( 'NONE', #21413, #24490 ) ;
#56323 = EDGE_CURVE ( 'NONE', #24519, #52930, #41709, .T. ) ;
#56324 = AXIS2_PLACEMENT_3D ( 'NONE', #63023, #32097, #31458 ) ;
#56325 = ORIENTED_EDGE ( 'NONE', *, *, #8180, .T. ) ;
#56326 = DIRECTION ( 'NONE',  ( 0.000000000000000000, 0.000000000000000000, 1.000000000000000000 ) ) ;
#56327 = VERTEX_POINT ( 'NONE', #62004 ) ;
#56328 = ORIENTED_EDGE ( 'NONE', *, *, #50993, .F. ) ;
#56329 = DIRECTION ( 'NONE',  ( 0.000000000000000000, -0.01356324068817991828, 0.9999080150203990547 ) ) ;
#56330 = CARTESIAN_POINT ( 'NONE',  ( 5.268658153349320195, -26.87458176590442704, 15.73590792199922461 ) ) ;
#56331 = DIRECTION ( 'NONE',  ( 0.000000000000000000, -0.01356324068817998940, 0.9999080150203990547 ) ) ;
#56332 = AXIS2_PLACEMENT_3D ( 'NONE', #30215, #8621, #13598 ) ;
#56333 = EDGE_LOOP ( 'NONE', ( #47563, #44970, #3090, #34804 ) ) ;
#56334 = AXIS2_PLACEMENT_3D ( 'NONE', #23998, #34283, #64853 ) ;
#56335 = AXIS2_PLACEMENT_3D ( 'NONE', #27007, #21700, #31642 ) ;
#56337 = CIRCLE ( 'NONE', #1148, 7.499999999999988454 ) ;
#56336 = CYLINDRICAL_SURFACE ( 'NONE', #17446, 12.75000000000000178 ) ;
#56338 = EDGE_CURVE ( 'NONE', #2803, #29586, #2132, .T. ) ;
#56339 = CARTESIAN_POINT ( 'NONE',  ( 19.67311005600952711, -0.7004819783312107306, 25.00000000000000000 ) ) ;
#56340 = CARTESIAN_POINT ( 'NONE',  ( 0.2647959493198551728, -12.03358727341676015, 2.271080632828021972 ) ) ;
#56341 = ORIENTED_EDGE ( 'NONE', *, *, #7833, .F. ) ;
#56342 = ORIENTED_EDGE ( 'NONE', *, *, #15732, .F. ) ;
#56343 = CARTESIAN_POINT ( 'NONE',  ( -24.42101984568203932, -3.522366633939671310, -2.451666775035121759 ) ) ;
#56344 = ORIENTED_EDGE ( 'NONE', *, *, #5131, .T. ) ;
#56345 = ORIENTED_EDGE ( 'NONE', *, *, #19391, .F. ) ;
#56346 = DIRECTION ( 'NONE',  ( 1.000000000000000000, -0.000000000000000000, -0.000000000000000000 ) ) ;
#56347 = CARTESIAN_POINT ( 'NONE',  ( 1.547277799338548920, -10.62321481610073626, 6.911346840320337748 ) ) ;
#56348 = CARTESIAN_POINT ( 'NONE',  ( -22.27710395300133328, 0.9764373854729221369, -3.549456197028682869 ) ) ;
#56349 = CARTESIAN_POINT ( 'NONE',  ( 16.84448096326508804, -10.22195168550365985, 6.309017530714546851 ) ) ;
#56350 = DIRECTION ( 'NONE',  ( 1.000000000000000000, 0.000000000000000000, 0.000000000000000000 ) ) ;
#56351 = CARTESIAN_POINT ( 'NONE',  ( -37.00000000000000711, -3.827046518385164742, 11.56998259273176188 ) ) ;
#56352 = DIRECTION ( 'NONE',  ( 1.000000000000000000, 0.000000000000000000, 0.000000000000000000 ) ) ;
#56353 = AXIS2_PLACEMENT_3D ( 'NONE', #13189, #17532, #38787 ) ;
#56354 = VECTOR ( 'NONE', #53791, 1000.000000000000000 ) ;
#56355 = EDGE_CURVE ( 'NONE', #13695, #6530, #1817, .T. ) ;
#56356 = VERTEX_POINT ( 'NONE', #27391 ) ;
#56357 = VECTOR ( 'NONE', #41633, 1000.000000000000000 ) ;
#56358 = DIRECTION ( 'NONE',  ( 0.000000000000000000, -0.01356324068817998940, 0.9999080150203990547 ) ) ;
#56359 = DIRECTION ( 'NONE',  ( 0.000000000000000000, 0.01356324068817991828, -0.9999080150203990547 ) ) ;
#56360 = AXIS2_PLACEMENT_3D ( 'NONE', #29283, #45229, #24286 ) ;
#56361 = CARTESIAN_POINT ( 'NONE',  ( -22.30625920655495165, 3.403091720605023962, 1.672644928563048472 ) ) ;
#56362 = LINE ( 'NONE', #60362, #23889 ) ;
#56363 = DIRECTION ( 'NONE',  ( 0.000000000000000000, -0.01356324068817991828, 0.9999080150203990547 ) ) ;
#56364 = AXIS2_PLACEMENT_3D ( 'NONE', #65176, #18674, #38934 ) ;
#56365 = CARTESIAN_POINT ( 'NONE',  ( 35.00000000000000000, 10.32377448871667625, -6.475373545682339582 ) ) ;
#56366 = CARTESIAN_POINT ( 'NONE',  ( 3.780834652287974773, 8.352030633203074927, -8.616471685210672860 ) ) ;
#56367 = CARTESIAN_POINT ( 'NONE',  ( 8.437200413559441614, 4.476360154859203355, -11.13383131558893346 ) ) ;
#56368 = VECTOR ( 'NONE', #4482, 1000.000000000000000 ) ;
#56369 = EDGE_CURVE ( 'NONE', #39884, #46591, #41428, .T. ) ;
#56370 = ORIENTED_EDGE ( 'NONE', *, *, #64874, .T. ) ;
#56371 = LINE ( 'NONE', #10817, #53693 ) ;
#56372 = CARTESIAN_POINT ( 'NONE',  ( 5.516018279890452902, 0.003580555109620797271, 0.005752102158673854694 ) ) ;
#56373 = CARTESIAN_POINT ( 'NONE',  ( 14.06742311317152172, -34.40796758970507341, 8.422011900743699542 ) ) ;
#56374 = ADVANCED_FACE ( 'NONE', ( #59970 ), #28070, .T. ) ;
#56375 = AXIS2_PLACEMENT_3D ( 'NONE', #30379, #30688, #25073 ) ;
#56376 = CIRCLE ( 'NONE', #47892, 12.18650000000000055 ) ;
#56377 = CIRCLE ( 'NONE', #39377, 12.18649999999999878 ) ;
#56378 = CARTESIAN_POINT ( 'NONE',  ( -27.09220147993978145, 10.57952257801956009, 5.663481862083665774 ) ) ;
#56379 = DIRECTION ( 'NONE',  ( 1.000000000000000000, 0.000000000000000000, 0.000000000000000000 ) ) ;
#56380 = ORIENTED_EDGE ( 'NONE', *, *, #16259, .T. ) ;
#56381 = CIRCLE ( 'NONE', #3299, 5.000000000000001776 ) ;
#56382 = CARTESIAN_POINT ( 'NONE',  ( 2.080613030138687147, 0.000000000000000000, 0.000000000000000000 ) ) ;
#56383 = CARTESIAN_POINT ( 'NONE',  ( -27.23354391799197316, -11.01738125875938046, -7.819786289819207425 ) ) ;
#56384 = CARTESIAN_POINT ( 'NONE',  ( 2.247206125382827935, 1.211896144126927144, 7.539576157880604868 ) ) ;
#56385 = VERTEX_POINT ( 'NONE', #13095 ) ;
#56386 = DIRECTION ( 'NONE',  ( -1.000000000000000000, -1.836970198721029688E-16, 0.000000000000000000 ) ) ;
#56387 = CARTESIAN_POINT ( 'NONE',  ( -16.18648497833802224, 7.819859351283344751, -9.103005354533555860 ) ) ;
#56388 = CARTESIAN_POINT ( 'NONE',  ( -35.00000000000000000, -2.544412758415929066, 11.91791701451265340 ) ) ;
#56390 = ORIENTED_EDGE ( 'NONE', *, *, #48956, .T. ) ;
#56389 = DIRECTION ( 'NONE',  ( -1.000000000000000000, 0.000000000000000000, 0.000000000000000000 ) ) ;
#56391 = DIRECTION ( 'NONE',  ( 0.000000000000000000, 0.000000000000000000, 1.000000000000000000 ) ) ;
#56392 = ADVANCED_FACE ( 'NONE', ( #19067 ), #34663, .T. ) ;
#56393 = CIRCLE ( 'NONE', #3308, 12.75000000000000178 ) ;
#56394 = CARTESIAN_POINT ( 'NONE',  ( 2.305787727787083519, -7.249469779319894336, -2.461236246751144829 ) ) ;
#56395 = ORIENTED_EDGE ( 'NONE', *, *, #15773, .T. ) ;
#56396 = CARTESIAN_POINT ( 'NONE',  ( 2.889800649504073782, 4.645655809191365115, 3.986129653162664432 ) ) ;
#56397 = LINE ( 'NONE', #17147, #52125 ) ;
#56398 = CARTESIAN_POINT ( 'NONE',  ( 22.86339282875463752, 2.804778511300523913, -11.66987002196172796 ) ) ;
#56399 = DIRECTION ( 'NONE',  ( 0.000000000000000000, 0.01356324068817998940, -0.9999080150203990547 ) ) ;
#56400 = CARTESIAN_POINT ( 'NONE',  ( 26.17141335727526652, 13.01134923558398704, 3.602278675730977930 ) ) ;
#56401 = AXIS2_PLACEMENT_3D ( 'NONE', #3113, #23375, #43644 ) ;
#56402 = CARTESIAN_POINT ( 'NONE',  ( -10.95212338237647920, -9.902220863987562183, 25.00000000000000000 ) ) ;
#56404 = VERTEX_POINT ( 'NONE', #59305 ) ;
#56403 = CARTESIAN_POINT ( 'NONE',  ( 0.4613984246114877230, 0.2828900474740380644, 12.30830943644279962 ) ) ;
#56405 = B_SPLINE_CURVE_WITH_KNOTS ( 'NONE', 3,
 ( #798, #20755, #61975, #10119, #21063, #61307, #25746 ),
 .UNSPECIFIED., .F., .F.,
 ( 4, 3, 4 ),
 ( 8.760178018519042877E-15, 0.002398160485435057911, 0.005002426799385541190 ),
 .UNSPECIFIED. ) ;
#56406 = ORIENTED_EDGE ( 'NONE', *, *, #49029, .F. ) ;
#56407 = DIRECTION ( 'NONE',  ( 0.000000000000000000, -0.4935949184179322380, 0.8696919319575150409 ) ) ;
#56408 = AXIS2_PLACEMENT_3D ( 'NONE', #10215, #30494, #50791 ) ;
#56409 = ORIENTED_EDGE ( 'NONE', *, *, #18844, .T. ) ;
#56410 = DIRECTION ( 'NONE',  ( 0.000000000000000000, 0.000000000000000000, 1.000000000000000000 ) ) ;
#56411 = CYLINDRICAL_SURFACE ( 'NONE', #34749, 12.75000000000000178 ) ;
#56412 = EDGE_CURVE ( 'NONE', #51352, #57823, #63957, .T. ) ;
#56413 = CARTESIAN_POINT ( 'NONE',  ( 0.2869720083484316731, 11.44147823180130885, 4.386174336869626877 ) ) ;
#56414 = CARTESIAN_POINT ( 'NONE',  ( 5.514624014163232779, -0.0005510299962882055525, 0.004104370840204387381 ) ) ;
#56415 = EDGE_LOOP ( 'NONE', ( #16329, #65253, #15667, #39471 ) ) ;
#56417 = DIRECTION ( 'NONE',  ( 0.000000000000000000, 0.000000000000000000, 1.000000000000000000 ) ) ;
#56416 = CIRCLE ( 'NONE', #22484, 12.74999999999999822 ) ;
#56418 = FACE_OUTER_BOUND ( 'NONE', #62455, .T. ) ;
#56419 = CARTESIAN_POINT ( 'NONE',  ( -22.27720387087365239, -1.337073746937880614, 3.430312021254888322 ) ) ;
#56420 = VERTEX_POINT ( 'NONE', #3477 ) ;
#56421 = EDGE_LOOP ( 'NONE', ( #62474, #9446, #64259, #22553 ) ) ;
#56422 = PLANE ( 'NONE',  #47020 ) ;
#56423 = AXIS2_PLACEMENT_3D ( 'NONE', #61147, #45858, #56143 ) ;
#56424 = EDGE_LOOP ( 'NONE', ( #18244, #4777, #61617, #17164 ) ) ;
#56425 = FACE_OUTER_BOUND ( 'NONE', #48603, .T. ) ;
#56426 = FACE_OUTER_BOUND ( 'NONE', #62024, .T. ) ;
#56427 = CARTESIAN_POINT ( 'NONE',  ( 0.3675815128205894289, -0.2638082659427565813, -12.27743992903066328 ) ) ;
#56428 = CARTESIAN_POINT ( 'NONE',  ( -35.00000000000000000, -9.557269938331609538, 7.561043153947932360 ) ) ;
#56429 = CIRCLE ( 'NONE', #15028, 5.000000000000000000 ) ;
#56430 = AXIS2_PLACEMENT_3D ( 'NONE', #22342, #37654, #52943 ) ;
#56431 = CARTESIAN_POINT ( 'NONE',  ( -35.00000000000000000, 9.908974237959645492, 6.307491713049065751 ) ) ;
#56432 = DIRECTION ( 'NONE',  ( 1.000000000000000000, 0.000000000000000000, 0.000000000000000000 ) ) ;
#56433 = AXIS2_PLACEMENT_3D ( 'NONE', #26861, #31829, #16877 ) ;
#56434 = CARTESIAN_POINT ( 'NONE',  ( -36.00000000000000711, 11.10408318471068689, -6.265926637539373623 ) ) ;
#56435 = EDGE_CURVE ( 'NONE', #21573, #7430, #43668, .T. ) ;
#56436 = ORIENTED_EDGE ( 'NONE', *, *, #41562, .T. ) ;
#56437 = DIRECTION ( 'NONE',  ( 0.000000000000000000, 0.000000000000000000, 1.000000000000000000 ) ) ;
#56438 = ADVANCED_FACE ( 'NONE', ( #23745 ), #58674, .T. ) ;
#56439 = DIRECTION ( 'NONE',  ( -1.000000000000000000, 0.000000000000000000, 0.000000000000000000 ) ) ;
#56440 = DIRECTION ( 'NONE',  ( -1.000000000000000000, 0.000000000000000000, 0.000000000000000000 ) ) ;
#56441 = CARTESIAN_POINT ( 'NONE',  ( -9.329544065157421073, 10.53307963029291372, -5.752532211403271312 ) ) ;
#56442 = CARTESIAN_POINT ( 'NONE',  ( -36.00000000000000711, 10.12742074351907817, -7.745827850122903868 ) ) ;
#56443 = CARTESIAN_POINT ( 'NONE',  ( 2.000000000000001776, 1.145812388885126820, 6.715725538143592743 ) ) ;
#56444 = CARTESIAN_POINT ( 'NONE',  ( -28.66013792860432119, -0.4872053345172048244, 1.770123732198246591 ) ) ;
#56445 = DIRECTION ( 'NONE',  ( -1.000000000000000000, 0.000000000000000000, 0.000000000000000000 ) ) ;
#56446 = CIRCLE ( 'NONE', #46911, 12.18649999999999878 ) ;
#56447 = VERTEX_POINT ( 'NONE', #18753 ) ;
#56448 = VECTOR ( 'NONE', #18939, 1000.000000000000000 ) ;
#56449 = ORIENTED_EDGE ( 'NONE', *, *, #33904, .F. ) ;
#56450 = EDGE_CURVE ( 'NONE', #54975, #51469, #63612, .T. ) ;
#56451 = CARTESIAN_POINT ( 'NONE',  ( 37.00000000000000711, 4.705694406421931860E-17, -3.469127814946512892E-15 ) ) ;
#56452 = CIRCLE ( 'NONE', #27771, 12.18650000000000055 ) ;
#56453 = ORIENTED_EDGE ( 'NONE', *, *, #30877, .F. ) ;
#56454 = LINE ( 'NONE', #36823, #36191 ) ;
#56455 = CYLINDRICAL_SURFACE ( 'NONE', #38856, 2.899999999999994582 ) ;
#56456 = CARTESIAN_POINT ( 'NONE',  ( 2.249013661412238907, 4.816366775941330225, 5.926694833810642216 ) ) ;
#56457 = CARTESIAN_POINT ( 'NONE',  ( 37.00000000000000711, -12.12087942037208776, 1.262958560998883595 ) ) ;
#56458 = ADVANCED_FACE ( 'NONE', ( #13730 ), #14065, .T. ) ;
#56459 = ORIENTED_EDGE ( 'NONE', *, *, #4045, .T. ) ;
#56460 = CARTESIAN_POINT ( 'NONE',  ( 35.00000000000000000, -7.608228585767794705, -10.23119532541070420 ) ) ;
#56462 = VECTOR ( 'NONE', #30101, 1000.000000000000000 ) ;
#56461 = CARTESIAN_POINT ( 'NONE',  ( 35.00000000000000000, 4.705694406421931860E-17, -3.469127814946512892E-15 ) ) ;
#56463 = DIRECTION ( 'NONE',  ( 0.3865475372811021382, -0.9114221272958290543, 0.1410344188397309739 ) ) ;
#56464 = DIRECTION ( 'NONE',  ( -1.000000000000000000, -0.000000000000000000, -0.000000000000000000 ) ) ;
#56465 = DIRECTION ( 'NONE',  ( 0.000000000000000000, -0.01356324068817991828, 0.9999080150203990547 ) ) ;
#56466 = VECTOR ( 'NONE', #52370, 1000.000000000000000 ) ;
#56467 = CARTESIAN_POINT ( 'NONE',  ( 2.288423627607476973, 2.767471693622796991, 7.131972212895015595 ) ) ;
#56468 = EDGE_LOOP ( 'NONE', ( #36612, #27818, #19307, #35848 ) ) ;
#56469 = CARTESIAN_POINT ( 'NONE',  ( 21.90174657591892071, 25.00000000000000000, -0.7349207973210698519 ) ) ;
#56470 = VERTEX_POINT ( 'NONE', #9085 ) ;
#56471 = VECTOR ( 'NONE', #58808, 1000.000000000000000 ) ;
#56472 = DIRECTION ( 'NONE',  ( 0.000000000000000000, 0.01356324068817991828, -0.9999080150203990547 ) ) ;
#56473 = DIRECTION ( 'NONE',  ( 0.000000000000000000, -0.9289767198167950824, 0.3701381553399052948 ) ) ;
#56474 = DIRECTION ( 'NONE',  ( 0.000000000000000000, 0.01356324068817992175, -0.9999080150203990547 ) ) ;
#56475 = CARTESIAN_POINT ( 'NONE',  ( -10.87564620705865082, -6.846636899367037010, 9.863669315241368807 ) ) ;
#56476 = CIRCLE ( 'NONE', #64955, 2.214855479030549468 ) ;
#56477 = VECTOR ( 'NONE', #40732, 1000.000000000000114 ) ;
#56478 = AXIS2_PLACEMENT_3D ( 'NONE', #26699, #51982, #21732 ) ;
#56479 = ORIENTED_EDGE ( 'NONE', *, *, #11498, .T. ) ;
#56480 = VERTEX_POINT ( 'NONE', #54331 ) ;
#56481 = PLANE ( 'NONE',  #25493 ) ;
#56482 = ORIENTED_EDGE ( 'NONE', *, *, #11490, .T. ) ;
#56483 = CARTESIAN_POINT ( 'NONE',  ( 2.255723233588949661, -6.548644987607536549, -3.933511348457504830 ) ) ;
#56484 = DIRECTION ( 'NONE',  ( -1.000000000000000000, 0.000000000000000000, 0.000000000000000000 ) ) ;
#56485 = CARTESIAN_POINT ( 'NONE',  ( -22.27721701579900682, -3.478642907697087949, -1.205877546543716816 ) ) ;
#56486 = CARTESIAN_POINT ( 'NONE',  ( -25.00000000000000355, -3.797884998337192286, 24.99999999999999289 ) ) ;
#56487 = CARTESIAN_POINT ( 'NONE',  ( 22.57855258442565116, 3.026812727784649493, 11.61199400236328749 ) ) ;
#56488 = CARTESIAN_POINT ( 'NONE',  ( -11.20102014733715201, -9.173601788332002016, 9.918148130496701853 ) ) ;
#56489 = CARTESIAN_POINT ( 'NONE',  ( -7.990345058477248408, -1.715916948163764166, 11.87819946997459120 ) ) ;
#56490 = ORIENTED_EDGE ( 'NONE', *, *, #41634, .T. ) ;
#56491 = ADVANCED_FACE ( 'NONE', ( #8113 ), #12596, .F. ) ;
#56492 = CARTESIAN_POINT ( 'NONE',  ( 1.719304012339844867, -11.38834240361479644, 5.690355757826019989 ) ) ;
#56493 = VERTEX_POINT ( 'NONE', #44635 ) ;
#56494 = DIRECTION ( 'NONE',  ( 0.000000000000000000, 0.9246979985058709772, 0.3807014730195252827 ) ) ;
#56495 = AXIS2_PLACEMENT_3D ( 'NONE', #39536, #19605, #4963 ) ;
#56496 = DIRECTION ( 'NONE',  ( 0.000000000000000000, 0.01356324068817998940, -0.9999080150203989437 ) ) ;
#56497 = EDGE_CURVE ( 'NONE', #4780, #52024, #16504, .T. ) ;
#56498 = AXIS2_PLACEMENT_3D ( 'NONE', #7564, #63095, #38478 ) ;
#56499 = CARTESIAN_POINT ( 'NONE',  ( 18.46659823902355768, 7.261787737648400132, 11.40465664842433924 ) ) ;
#56500 = ORIENTED_EDGE ( 'NONE', *, *, #24116, .F. ) ;
#56501 = CIRCLE ( 'NONE', #207, 4.999999999999998224 ) ;
#56502 = CARTESIAN_POINT ( 'NONE',  ( -14.80332308495294136, -33.90539544390878035, 8.876538241603904922 ) ) ;
#56503 = ORIENTED_EDGE ( 'NONE', *, *, #22860, .T. ) ;
#56504 = CYLINDRICAL_SURFACE ( 'NONE', #32248, 12.74999999999999822 ) ;
#56505 = DIRECTION ( 'NONE',  ( 1.000000000000000000, -0.000000000000000000, -0.000000000000000000 ) ) ;
#56506 = CARTESIAN_POINT ( 'NONE',  ( 3.152665057736177445, 3.161213418915486795, 7.281573230473766145 ) ) ;
#56507 = CARTESIAN_POINT ( 'NONE',  ( -33.44920912455759066, -2.804301875032225499, 22.47723755754419628 ) ) ;
#56508 = EDGE_LOOP ( 'NONE', ( #32186, #37914, #5603, #13377 ) ) ;
#56509 = AXIS2_PLACEMENT_3D ( 'NONE', #49571, #3371, #48278 ) ;
#56510 = VERTEX_POINT ( 'NONE', #54961 ) ;
#56511 = CARTESIAN_POINT ( 'NONE',  ( 5.516018279890452902, -0.005042957932158615743, 0.004525000489649755146 ) ) ;
#56512 = ORIENTED_EDGE ( 'NONE', *, *, #20567, .T. ) ;
#56513 = DIRECTION ( 'NONE',  ( -1.000000000000000000, 0.000000000000000000, 0.000000000000000000 ) ) ;
#56514 = ORIENTED_EDGE ( 'NONE', *, *, #21176, .T. ) ;
#56515 = CIRCLE ( 'NONE', #22361, 7.938172270156617749 ) ;
#56516 = ORIENTED_EDGE ( 'NONE', *, *, #31860, .F. ) ;
#56517 = ORIENTED_EDGE ( 'NONE', *, *, #9278, .T. ) ;
#56518 = B_SPLINE_CURVE_WITH_KNOTS ( 'NONE', 3,
 ( #63560, #18031, #38295, #33324, #53625, #49306, #8064, #28333, #33962, #48627, #63902, #3753, #24010 ),
 .UNSPECIFIED., .F., .F.,
 ( 4, 3, 3, 3, 4 ),
 ( 3.127317220692750759E-18, 6.607593386745608287E-05, 0.0001321518677373537348, 0.0001982171734706250610, 0.0002642860854759490966 ),
 .UNSPECIFIED. ) ;
#56519 = LINE ( 'NONE', #6001, #8620 ) ;
#56520 = CARTESIAN_POINT ( 'NONE',  ( 1.719304012338199295, 11.67935079956398958, 5.066286238785226992 ) ) ;
#56521 = EDGE_CURVE ( 'NONE', #62520, #13985, #50995, .T. ) ;
#56522 = CARTESIAN_POINT ( 'NONE',  ( 2.440552418640497212, -1.142369876085273184, -7.615619946579185395 ) ) ;
#56523 = CARTESIAN_POINT ( 'NONE',  ( 2.298277635560276533, 2.772101951899060612, -7.133696409974365160 ) ) ;
#56524 = CARTESIAN_POINT ( 'NONE',  ( -37.00000000000000711, 9.752226076388895493, 6.547236723514054724 ) ) ;
#56525 = ORIENTED_EDGE ( 'NONE', *, *, #18267, .F. ) ;
#56526 = CARTESIAN_POINT ( 'NONE',  ( 37.00000000000000711, -11.54110654723647400, 2.185196060784003524 ) ) ;
#56527 = CIRCLE ( 'NONE', #4513, 4.999999999999999112 ) ;
#56528 = EDGE_CURVE ( 'NONE', #13407, #49728, #9728, .T. ) ;
#56529 = ORIENTED_EDGE ( 'NONE', *, *, #32611, .F. ) ;
#56530 =( BOUNDED_SURFACE ( )  B_SPLINE_SURFACE ( 3, 1, ( 
 ( #2838, #13750 ),
 ( #28403, #3158 ),
 ( #33716, #24079 ),
 ( #34039, #29385 ) ),
 .UNSPECIFIED., .F., .F., .F. ) 
 B_SPLINE_SURFACE_WITH_KNOTS ( ( 4, 4 ),
 ( 2, 2 ),
 ( 0.000000000000000000, 1.000000000000000000 ),
 ( 0.000000000000000000, 1.000000000000000000 ),
 .UNSPECIFIED. ) 
 GEOMETRIC_REPRESENTATION_ITEM ( )  RATIONAL_B_SPLINE_SURFACE ( (
 ( 1.000000000000000000, 1.000000000000000000),
 ( 0.6933888150995267674, 0.9895912004443193632),
 ( 0.6933888150995267674, 0.9895912004443193632),
 ( 1.000000000000000000, 1.000000000000000000) ) ) 
 REPRESENTATION_ITEM ( '' )  SURFACE ( )  );
#56531 = CARTESIAN_POINT ( 'NONE',  ( 2.000000000000001776, -0.2704997240205401221, 6.931223712253438585 ) ) ;
#56532 = EDGE_CURVE ( 'NONE', #11586, #41673, #7302, .T. ) ;
#56533 = CARTESIAN_POINT ( 'NONE',  ( -3.288880356639787728, 9.825749110095811645, 9.264667814138983104 ) ) ;
#56534 = EDGE_CURVE ( 'NONE', #38662, #35317, #29674, .T. ) ;
#56535 = DIRECTION ( 'NONE',  ( 0.000000000000000000, 0.9635499925192236859, -0.2675283385292184235 ) ) ;
#56536 = CARTESIAN_POINT ( 'NONE',  ( 0.2717059086739026519, -8.007130974639977694, -9.268607328094613962 ) ) ;
#56537 = DIRECTION ( 'NONE',  ( 1.000000000000000000, -0.000000000000000000, 0.000000000000000000 ) ) ;
#56538 = CARTESIAN_POINT ( 'NONE',  ( 2.899286259009685729, -7.845618522360447322, -0.3564726075924216087 ) ) ;
#56539 = CIRCLE ( 'NONE', #17376, 12.18650000000000055 ) ;
#56540 = AXIS2_PLACEMENT_3D ( 'NONE', #2686, #17947, #49213 ) ;
#56541 = AXIS2_PLACEMENT_3D ( 'NONE', #43367, #53032, #7467 ) ;
#56542 = EDGE_LOOP ( 'NONE', ( #51968, #24108, #17761, #59675 ) ) ;
#56543 = EDGE_CURVE ( 'NONE', #10925, #61800, #61453, .T. ) ;
#56544 = DIRECTION ( 'NONE',  ( 0.000000000000000000, 0.6745969609292609137, 0.7381862504172000961 ) ) ;
#56545 = ORIENTED_EDGE ( 'NONE', *, *, #56137, .T. ) ;
#56546 = ADVANCED_FACE ( 'NONE', ( #10073 ), #10710, .T. ) ;
#56547 = CARTESIAN_POINT ( 'NONE',  ( -10.79971841461723336, -9.842872838453388340, -6.865048668419079014 ) ) ;
#56548 = DIRECTION ( 'NONE',  ( -1.000000000000000000, -0.000000000000000000, 0.000000000000000000 ) ) ;
#56549 = CARTESIAN_POINT ( 'NONE',  ( 2.639814597422736941, 6.111633106000494919, -4.793557287999567151 ) ) ;
#56550 = CARTESIAN_POINT ( 'NONE',  ( 2.589278595513019088, 4.081908913131758965, 6.588350318048411758 ) ) ;
#56551 = CARTESIAN_POINT ( 'NONE',  ( -37.00000000000000711, 0.000000000000000000, 0.000000000000000000 ) ) ;
#56552 = ORIENTED_EDGE ( 'NONE', *, *, #49874, .T. ) ;
#56553 = DIRECTION ( 'NONE',  ( 1.000000000000000000, 0.000000000000000000, 0.000000000000000000 ) ) ;
#56554 = CARTESIAN_POINT ( 'NONE',  ( 0.3160775863651064110, 2.365582350580221593, -12.03278055228168775 ) ) ;
#56555 = CARTESIAN_POINT ( 'NONE',  ( 22.61260652651741054, 9.961396833084766200, -6.701065456133467713 ) ) ;
#56556 = CARTESIAN_POINT ( 'NONE',  ( 37.25000000000000711, -20.00000000000000000, 1.500000000000002887 ) ) ;
#56557 = CIRCLE ( 'NONE', #61858, 12.18649999999999878 ) ;
#56558 = EDGE_CURVE ( 'NONE', #58400, #4690, #24344, .T. ) ;
#56559 = DIRECTION ( 'NONE',  ( -1.000000000000000000, 0.000000000000000000, -0.000000000000000000 ) ) ;
#56560 = AXIS2_PLACEMENT_3D ( 'NONE', #30169, #50138, #45451 ) ;
#56561 = CARTESIAN_POINT ( 'NONE',  ( 2.241509619876138171, 2.575142053947867105, 7.187074272457164348 ) ) ;
#56562 = FACE_OUTER_BOUND ( 'NONE', #42013, .T. ) ;
#56563 = CARTESIAN_POINT ( 'NONE',  ( -20.79170840334646542, -11.34110549087206898, -3.921648409140116698 ) ) ;
#56564 = FACE_OUTER_BOUND ( 'NONE', #39970, .T. ) ;
#56565 = ORIENTED_EDGE ( 'NONE', *, *, #28909, .T. ) ;
#56566 = CIRCLE ( 'NONE', #45932, 5.000000000000000888 ) ;
#56567 = VERTEX_POINT ( 'NONE', #21011 ) ;
#56568 = CARTESIAN_POINT ( 'NONE',  ( 0.3665391374699464300, -2.392238720110541284, 12.04754782681756708 ) ) ;
#56569 = DIRECTION ( 'NONE',  ( 0.000000000000000000, 0.000000000000000000, -1.000000000000000000 ) ) ;
#56570 = CARTESIAN_POINT ( 'NONE',  ( -35.00000000000000000, 0.000000000000000000, 0.000000000000000000 ) ) ;
#56571 = LINE ( 'NONE', #56224, #65766 ) ;
#56572 = ORIENTED_EDGE ( 'NONE', *, *, #6470, .F. ) ;
#56573 = VECTOR ( 'NONE', #7388, 1000.000000000000000 ) ;
#56574 = AXIS2_PLACEMENT_3D ( 'NONE', #61541, #15986, #51605 ) ;
#56575 = ORIENTED_EDGE ( 'NONE', *, *, #10244, .F. ) ;
#56576 = ORIENTED_EDGE ( 'NONE', *, *, #11090, .F. ) ;
#56577 = CARTESIAN_POINT ( 'NONE',  ( 1.719304012341272836, -1.452142814148833949, -12.64775761152634281 ) ) ;
#56578 = AXIS2_PLACEMENT_3D ( 'NONE', #25798, #27106, #56040 ) ;
#56579 = EDGE_CURVE ( 'NONE', #6611, #59647, #20047, .T. ) ;
#56581 = AXIS2_PLACEMENT_3D ( 'NONE', #24089, #60310, #19438 ) ;
#56580 = LINE ( 'NONE', #26633, #33220 ) ;
#56582 = B_SPLINE_CURVE_WITH_KNOTS ( 'NONE', 3,
 ( #64537, #23682, #29956, #19008, #55230, #34610 ),
 .UNSPECIFIED., .F., .F.,
 ( 4, 2, 4 ),
 ( 0.005421911171979544933, 0.006610292730091626295, 0.007798674288203707658 ),
 .UNSPECIFIED. ) ;
#56583 = ORIENTED_EDGE ( 'NONE', *, *, #45086, .F. ) ;
#56584 = CARTESIAN_POINT ( 'NONE',  ( 47.00000000000000711, 4.705694406421931860E-17, -3.469127814946512892E-15 ) ) ;
#56585 = DIRECTION ( 'NONE',  ( -1.000000000000000000, 0.000000000000000000, 0.000000000000000000 ) ) ;
#56586 = ORIENTED_EDGE ( 'NONE', *, *, #59775, .F. ) ;
#56587 = CARTESIAN_POINT ( 'NONE',  ( 2.244591118396916940, 4.825158615932057415, -5.917635828476827342 ) ) ;
#56588 = EDGE_CURVE ( 'NONE', #27860, #10268, #64673, .T. ) ;
#56589 = CARTESIAN_POINT ( 'NONE',  ( 16.25880638383053167, -34.36679772354877116, -6.546306705357506139 ) ) ;
#56590 = CARTESIAN_POINT ( 'NONE',  ( 24.54437410765793004, 1.233057148241763823, 11.94190642173460759 ) ) ;
#56591 = ORIENTED_EDGE ( 'NONE', *, *, #11385, .F. ) ;
#56592 = CARTESIAN_POINT ( 'NONE',  ( 0.3053067050349213551, 12.11120005789973852, -1.901204202464545912 ) ) ;
#56593 = VERTEX_POINT ( 'NONE', #40982 ) ;
#56594 = DIRECTION ( 'NONE',  ( -1.000000000000000000, 0.000000000000000000, 0.000000000000000000 ) ) ;
#56595 = AXIS2_PLACEMENT_3D ( 'NONE', #42352, #62642, #58021 ) ;
#56596 = ORIENTED_EDGE ( 'NONE', *, *, #52708, .T. ) ;
#56597 = DIRECTION ( 'NONE',  ( 1.000000000000000000, 0.000000000000000000, 0.000000000000000000 ) ) ;
#56598 = FACE_OUTER_BOUND ( 'NONE', #61289, .T. ) ;
#56599 = CARTESIAN_POINT ( 'NONE',  ( 145.1370849898475797, 3.309064568108273190E-14, 0.000000000000000000 ) ) ;
#56600 = CIRCLE ( 'NONE', #6675, 12.18649999999999878 ) ;
#56601 = CARTESIAN_POINT ( 'NONE',  ( 35.00000000000000000, 12.08151691381189785, -4.074242145636050694 ) ) ;
#56602 = CARTESIAN_POINT ( 'NONE',  ( -27.08429572838383947, -1.632445743623433421, 1.608131779585712406 ) ) ;
#56603 = EDGE_CURVE ( 'NONE', #1422, #31754, #33575, .T. ) ;
#56604 = CARTESIAN_POINT ( 'NONE',  ( 2.665405856346787949, -8.776564688671564696, -3.808819464940508936 ) ) ;
#56605 = CARTESIAN_POINT ( 'NONE',  ( -37.00000000000000711, -7.238157050195700215, 10.49626516989268588 ) ) ;
#56606 = CARTESIAN_POINT ( 'NONE',  ( 0.2646305136544065406, 1.996350543472993566, 12.08286001766535911 ) ) ;
#56608 = VERTEX_POINT ( 'NONE', #51636 ) ;
#56607 = DIRECTION ( 'NONE',  ( 1.000000000000000000, 0.000000000000000000, 0.000000000000000000 ) ) ;
#56609 = B_SPLINE_CURVE_WITH_KNOTS ( 'NONE', 3,
 ( #47943, #32305, #52618, #7043, #53916, #27313, #2401, #2055, #37950, #58244, #22319, #33300, #18354, #62891, #42590, #32613, #53604, #48605, #22007, #52923, #23322, #38617 ),
 .UNSPECIFIED., .F., .F.,
 ( 4, 3, 3, 3, 3, 3, 3, 4 ),
 ( 1.311167604876506724E-18, 4.449119708436685016E-05, 6.626296329540322600E-05, 8.803456484962410972E-05, 0.0001098060367612766793, 0.0001315774408628458134, 0.0001760698110411108961, 0.0001829697163287834563 ),
 .UNSPECIFIED. ) ;
#56610 = DIRECTION ( 'NONE',  ( -1.000000000000000000, 0.000000000000000000, 0.000000000000000000 ) ) ;
#56611 = AXIS2_PLACEMENT_3D ( 'NONE', #26401, #31398, #6793 ) ;
#56612 = ORIENTED_EDGE ( 'NONE', *, *, #50095, .F. ) ;
#56613 = CARTESIAN_POINT ( 'NONE',  ( 0.3002738374340787608, -4.403689978763143387, 11.43949898053769587 ) ) ;
#56614 = EDGE_CURVE ( 'NONE', #48464, #47999, #63629, .T. ) ;
#56615 = AXIS2_PLACEMENT_3D ( 'NONE', #33112, #32764, #43407 ) ;
#56616 = DIRECTION ( 'NONE',  ( 0.000000000000000000, -0.01356324068817992175, 0.9999080150203990547 ) ) ;
#56617 = EDGE_CURVE ( 'NONE', #29012, #42070, #28724, .T. ) ;
#56618 = ORIENTED_EDGE ( 'NONE', *, *, #44968, .T. ) ;
#56619 = CARTESIAN_POINT ( 'NONE',  ( 37.00000000000000711, -1.039216533672818299, 11.70009620280412399 ) ) ;
#56620 = DIRECTION ( 'NONE',  ( -1.000000000000000000, -0.000000000000000000, 0.000000000000000000 ) ) ;
#56621 = DIRECTION ( 'NONE',  ( 0.000000000000000000, 0.000000000000000000, 1.000000000000000000 ) ) ;
#56622 = CARTESIAN_POINT ( 'NONE',  ( 2.241352910868909643, 7.145045428366612050, -2.689314586382279604 ) ) ;
#56623 = CARTESIAN_POINT ( 'NONE',  ( 12.10998784662220729, 8.443435280036798218, -8.526922110106905706 ) ) ;
#56624 = VERTEX_POINT ( 'NONE', #31970 ) ;
#56625 = CARTESIAN_POINT ( 'NONE',  ( -17.38983135432702909, -6.044891695814540000, -10.36758421901369331 ) ) ;
#56626 = VERTEX_POINT ( 'NONE', #46960 ) ;
#56627 = ADVANCED_FACE ( 'NONE', ( #1078 ), #21698, .T. ) ;
#56628 = DIRECTION ( 'NONE',  ( 0.000000000000000000, -0.8276889981568956722, 0.5611870653623750593 ) ) ;
#56629 = DIRECTION ( 'NONE',  ( 0.000000000000000000, 0.01356324068817998940, -0.9999080150203990547 ) ) ;
#56630 = CARTESIAN_POINT ( 'NONE',  ( -35.00000000000000000, 8.352657516904674395, 8.258652103341463047 ) ) ;
#56631 = EDGE_CURVE ( 'NONE', #47398, #50365, #22006, .T. ) ;
#56632 = ORIENTED_EDGE ( 'NONE', *, *, #19716, .F. ) ;
#56633 = CIRCLE ( 'NONE', #65098, 5.000000000000000000 ) ;
#56634 = VECTOR ( 'NONE', #38085, 1000.000000000000000 ) ;
#56635 = DIRECTION ( 'NONE',  ( 0.000000000000000000, -0.6876994588534143249, -0.7259954919231393911 ) ) ;
#56636 = ADVANCED_FACE ( 'NONE', ( #7042 ), #31336, .T. ) ;
#56637 = VECTOR ( 'NONE', #16050, 1000.000000000000000 ) ;
#56638 = CIRCLE ( 'NONE', #5671, 5.000000000000000888 ) ;
#56639 = EDGE_CURVE ( 'NONE', #8976, #55634, #49845, .T. ) ;
#56640 = CARTESIAN_POINT ( 'NONE',  ( 29.03457606387295087, 7.862146963512124387, 10.97436308512422265 ) ) ;
#56641 = CARTESIAN_POINT ( 'NONE',  ( 47.41189015808931373, -0.5144011408980397881, -11.10762064040663510 ) ) ;
#56642 = CIRCLE ( 'NONE', #30091, 12.18649999999999878 ) ;
#56643 = ADVANCED_FACE ( 'NONE', ( #47610 ), #22318, .T. ) ;
#56644 = DIRECTION ( 'NONE',  ( 1.000000000000000000, 0.000000000000000000, 0.000000000000000000 ) ) ;
#56645 = CARTESIAN_POINT ( 'NONE',  ( 8.485946503340201730, 5.237987331432492510, 12.44894516775456239 ) ) ;
#56646 = PLANE ( 'NONE',  #29851 ) ;
#56647 = CARTESIAN_POINT ( 'NONE',  ( -35.00000000000000000, 8.389074212634412220, -8.839356091079954680 ) ) ;
#56648 = CARTESIAN_POINT ( 'NONE',  ( -35.00000000000000000, -3.287724142101498437, 11.73463472867575064 ) ) ;
#56649 = AXIS2_PLACEMENT_3D ( 'NONE', #22186, #43115, #37146 ) ;
#56650 = B_SPLINE_CURVE_WITH_KNOTS ( 'NONE', 3,
 ( #33502, #6926, #27196, #42457, #62757, #45113, #55079, #54104, #64710, #49773, #44430, #34771, #49468, #65374, #43801, #50441 ),
 .UNSPECIFIED., .F., .F.,
 ( 4, 3, 3, 3, 3, 4 ),
 ( 0.000000000000000000, 0.0002999043160757219992, 0.0005998071753050768229, 0.0008997092107374199746, 0.001204458948194617922, 0.001510329163474479321 ),
 .UNSPECIFIED. ) ;
#56651 = AXIS2_PLACEMENT_3D ( 'NONE', #44773, #65056, #35457 ) ;
#56652 = ORIENTED_EDGE ( 'NONE', *, *, #15882, .T. ) ;
#56653 = CARTESIAN_POINT ( 'NONE',  ( -17.88705001012359830, 6.214010860753471199, 11.98683707068579452 ) ) ;
#56654 = LINE ( 'NONE', #59188, #1241 ) ;
#56655 = AXIS2_PLACEMENT_3D ( 'NONE', #26723, #1473, #52000 ) ;
#56656 = VERTEX_POINT ( 'NONE', #62240 ) ;
#56657 = CARTESIAN_POINT ( 'NONE',  ( 0.9296196016816719032, 10.58347995892850157, 6.590257778216622953 ) ) ;
#56658 = CARTESIAN_POINT ( 'NONE',  ( -22.27719412087655471, 3.421752300520425116, 1.358750377066169301 ) ) ;
#56659 = CIRCLE ( 'NONE', #49220, 6.936499999999989008 ) ;
#56660 = DIRECTION ( 'NONE',  ( 1.000000000000000000, 0.000000000000000000, 0.000000000000000000 ) ) ;
#56661 = VERTEX_POINT ( 'NONE', #56950 ) ;
#56662 = CARTESIAN_POINT ( 'NONE',  ( 26.08439714455133185, -12.97057518889163674, 3.743551691817328386 ) ) ;
#56663 = FACE_OUTER_BOUND ( 'NONE', #28436, .T. ) ;
#56664 = ORIENTED_EDGE ( 'NONE', *, *, #64656, .T. ) ;
#56665 = DIRECTION ( 'NONE',  ( 0.000000000000000000, -0.01356324068817992175, 0.9999080150203990547 ) ) ;
#56666 = VERTEX_POINT ( 'NONE', #17010 ) ;
#56667 = ORIENTED_EDGE ( 'NONE', *, *, #25177, .F. ) ;
#56669 = EDGE_CURVE ( 'NONE', #49156, #51803, #14784, .T. ) ;
#56668 = CARTESIAN_POINT ( 'NONE',  ( -27.08416781016246588, -1.744495588874929393, 1.485424708116787507 ) ) ;
#56670 = VECTOR ( 'NONE', #52183, 1000.000000000000000 ) ;
#56671 = ORIENTED_EDGE ( 'NONE', *, *, #42241, .T. ) ;
#56672 = CARTESIAN_POINT ( 'NONE',  ( 35.00000000000000000, -3.093009498343839869, 11.78745411414842437 ) ) ;
#56673 = CARTESIAN_POINT ( 'NONE',  ( 0.3675815128205912052, -11.44679196252406506, -4.447030445008294919 ) ) ;
#56674 = CARTESIAN_POINT ( 'NONE',  ( 35.00000000000000000, -4.400442035670861785, 11.96656215839372805 ) ) ;
#56675 = CARTESIAN_POINT ( 'NONE',  ( 37.00000000000000711, 4.705694406421931860E-17, -3.469127814946512892E-15 ) ) ;
#56676 = ORIENTED_EDGE ( 'NONE', *, *, #10949, .T. ) ;
#56677 = DIRECTION ( 'NONE',  ( -0.3939253465568943180, -0.5982248387291149161, -0.6978179301705819126 ) ) ;
#56679 = B_SPLINE_CURVE_WITH_KNOTS ( 'NONE', 3,
 ( #12774, #28408, #3161, #23426, #43705, #18467 ),
 .UNSPECIFIED., .F., .F.,
 ( 4, 2, 4 ),
 ( 0.0001654224980408412369, 0.0006219428995476526233, 0.001078463301054463901 ),
 .UNSPECIFIED. ) ;
#56678 = CARTESIAN_POINT ( 'NONE',  ( 11.27382677987933057, -33.37417574758200800, 11.09187761368031211 ) ) ;
#56680 = CARTESIAN_POINT ( 'NONE',  ( 0.000000000000000000, 4.444115772890187444, -5.163689623839299081 ) ) ;
#56682 = ORIENTED_EDGE ( 'NONE', *, *, #65601, .T. ) ;
#56681 = DIRECTION ( 'NONE',  ( -0.3865475372811021937, -0.6075346789811115755, -0.6938894834606104123 ) ) ;
#56683 = CARTESIAN_POINT ( 'NONE',  ( 35.00000000000000000, 12.68495603654573323, 1.286231064351170739 ) ) ;
#56684 = EDGE_LOOP ( 'NONE', ( #62795, #62136, #46952, #46488 ) ) ;
#56685 = AXIS2_PLACEMENT_3D ( 'NONE', #33392, #42350, #32392 ) ;
#56686 = FACE_OUTER_BOUND ( 'NONE', #5576, .T. ) ;
#56687 = ORIENTED_EDGE ( 'NONE', *, *, #33257, .F. ) ;
#56688 = EDGE_CURVE ( 'NONE', #14898, #62196, #46992, .T. ) ;
#56689 = VECTOR ( 'NONE', #58661, 1000.000000000000000 ) ;
#56690 = ORIENTED_EDGE ( 'NONE', *, *, #23268, .F. ) ;
#56691 = DIRECTION ( 'NONE',  ( 0.000000000000000000, 0.000000000000000000, 1.000000000000000000 ) ) ;
#56692 = LINE ( 'NONE', #11123, #2255 ) ;
#56694 = CYLINDRICAL_SURFACE ( 'NONE', #50331, 5.000000000000002665 ) ;
#56693 = AXIS2_PLACEMENT_3D ( 'NONE', #5364, #51907, #382 ) ;
#56695 = VERTEX_POINT ( 'NONE', #28631 ) ;
#56696 = CYLINDRICAL_SURFACE ( 'NONE', #674, 12.75000000000000178 ) ;
#56697 = EDGE_CURVE ( 'NONE', #64338, #21860, #49588, .T. ) ;
#56698 = DIRECTION ( 'NONE',  ( -1.000000000000000000, 0.000000000000000000, 0.000000000000000000 ) ) ;
#56699 = CARTESIAN_POINT ( 'NONE',  ( -36.00000000000000711, -7.379373053628941470, 10.39746860227888270 ) ) ;
#56700 = VERTEX_POINT ( 'NONE', #39257 ) ;
#56701 = VECTOR ( 'NONE', #9190, 1000.000000000000000 ) ;
#56702 = ORIENTED_EDGE ( 'NONE', *, *, #39716, .T. ) ;
#56703 = DIRECTION ( 'NONE',  ( 0.000000000000000000, -0.4935949184179136418, 0.8696919319575254770 ) ) ;
#56704 = ORIENTED_EDGE ( 'NONE', *, *, #52846, .F. ) ;
#56705 = VECTOR ( 'NONE', #26196, 1000.000000000000000 ) ;
#56706 = EDGE_CURVE ( 'NONE', #8645, #634, #35997, .T. ) ;
#56707 = ORIENTED_EDGE ( 'NONE', *, *, #42296, .T. ) ;
#56708 = AXIS2_PLACEMENT_3D ( 'NONE', #29157, #44750, #65032 ) ;
#56709 = CARTESIAN_POINT ( 'NONE',  ( 5.530133899448235191, 0.01459891979722818985, 0.006510401266731672201 ) ) ;
#56710 = CARTESIAN_POINT ( 'NONE',  ( -37.00000000000000711, 8.830544224262947495, 9.196955404009329982 ) ) ;
#56711 = CARTESIAN_POINT ( 'NONE',  ( 36.00000000000000711, 5.710938531231875004, 11.39945968423464784 ) ) ;
#56712 = CARTESIAN_POINT ( 'NONE',  ( -22.31328051695926007, 1.076152733467212741, 3.633840107626929328 ) ) ;
#56713 = CARTESIAN_POINT ( 'NONE',  ( 36.00000000000000711, -12.73293890771483561, -0.6593684648220077271 ) ) ;
#56714 = AXIS2_PLACEMENT_3D ( 'NONE', #30064, #50693, #39056 ) ;
#56715 = DIRECTION ( 'NONE',  ( 1.000000000000000000, -0.000000000000000000, -0.000000000000000000 ) ) ;
#56716 = CARTESIAN_POINT ( 'NONE',  ( -37.00000000000000711, 7.499679039484183463, -9.040300684349618976 ) ) ;
#56717 = VERTEX_POINT ( 'NONE', #8045 ) ;
#56718 = AXIS2_PLACEMENT_3D ( 'NONE', #35491, #25860, #59792 ) ;
#56719 = DIRECTION ( 'NONE',  ( -1.000000000000000000, 0.000000000000000000, 0.000000000000000000 ) ) ;
#56720 = DIRECTION ( 'NONE',  ( 0.000000000000000000, -0.6478160128811839558, 0.7617968321374970486 ) ) ;
#56721 = EDGE_CURVE ( 'NONE', #62845, #36702, #37053, .T. ) ;
#56722 = DIRECTION ( 'NONE',  ( 1.000000000000000000, 0.000000000000000000, -0.000000000000000000 ) ) ;
#56723 = VECTOR ( 'NONE', #42260, 1000.000000000000000 ) ;
#56724 = CARTESIAN_POINT ( 'NONE',  ( -35.00000000000000000, -12.05416472667164207, -1.791059740004549372 ) ) ;
#56725 = EDGE_CURVE ( 'NONE', #29440, #64295, #58243, .T. ) ;
#56726 =( BOUNDED_SURFACE ( )  B_SPLINE_SURFACE ( 3, 1, ( 
 ( #51519, #15254 ),
 ( #35535, #40863 ),
 ( #5968, #61143 ),
 ( #46500, #55833 ) ),
 .UNSPECIFIED., .F., .F., .F. ) 
 B_SPLINE_SURFACE_WITH_KNOTS ( ( 4, 4 ),
 ( 2, 2 ),
 ( 0.000000000000000000, 1.000000000000000000 ),
 ( 0.000000000000000000, 1.000000000000000000 ),
 .UNSPECIFIED. ) 
 GEOMETRIC_REPRESENTATION_ITEM ( )  RATIONAL_B_SPLINE_SURFACE ( (
 ( 1.000000000000000000, 1.000000000000000000),
 ( 0.9942764183789327692, 0.8450855930916580938),
 ( 0.9942764183789327692, 0.8450855930916580938),
 ( 1.000000000000000000, 1.000000000000000000) ) ) 
 REPRESENTATION_ITEM ( '' )  SURFACE ( )  );
#56727 = DIRECTION ( 'NONE',  ( -1.000000000000000000, -0.000000000000000000, -0.000000000000000000 ) ) ;
#56728 = CARTESIAN_POINT ( 'NONE',  ( 1.198791140420632173, 2.686891236233812208, -12.26651935498972357 ) ) ;
#56729 = ADVANCED_FACE ( 'NONE', ( #58593 ), #2746, .T. ) ;
#56730 = CARTESIAN_POINT ( 'NONE',  ( 12.47628546223243617, 0.000000000000000000, -11.99999999999998224 ) ) ;
#56731 = VERTEX_POINT ( 'NONE', #33299 ) ;
#56732 = DIRECTION ( 'NONE',  ( -1.000000000000000000, -1.836970198721029688E-16, -0.000000000000000000 ) ) ;
#56733 = AXIS2_PLACEMENT_3D ( 'NONE', #24838, #38820, #65379 ) ;
#56734 = CARTESIAN_POINT ( 'NONE',  ( 36.00000000000000711, 8.954052073409734192, 9.076753354953895681 ) ) ;
#56735 = CARTESIAN_POINT ( 'NONE',  ( -25.64121911577780821, 4.545061814456081706, 11.11074877336984379 ) ) ;
#56736 = AXIS2_PLACEMENT_3D ( 'NONE', #50516, #65762, #39864 ) ;
#56737 = CARTESIAN_POINT ( 'NONE',  ( 8.395146353829712638, -32.40713589851873166, 12.72020452407952540 ) ) ;
#56738 = VECTOR ( 'NONE', #9114, 1000.000000000000114 ) ;
#56739 = DIRECTION ( 'NONE',  ( 1.000000000000000000, 0.000000000000000000, 0.000000000000000000 ) ) ;
#56740 = CARTESIAN_POINT ( 'NONE',  ( 3.031336079629613600, -7.268683861177229311, 3.088871717871501943 ) ) ;
#56741 = ORIENTED_EDGE ( 'NONE', *, *, #57455, .F. ) ;
#56742 = DIRECTION ( 'NONE',  ( 1.000000000000000000, -0.000000000000000000, -0.000000000000000000 ) ) ;
#56743 = CARTESIAN_POINT ( 'NONE',  ( -27.01437459610461644, -13.31613970204372421, -2.220455681983950935 ) ) ;
#56744 = CARTESIAN_POINT ( 'NONE',  ( 9.989421171649008002, -29.02163280020721103, -8.890648868200056398 ) ) ;
#56745 = ORIENTED_EDGE ( 'NONE', *, *, #64411, .T. ) ;
#56746 = CARTESIAN_POINT ( 'NONE',  ( 3.152665057735509979, 7.102135024646700323, 3.546019893115181620 ) ) ;
#56747 = CARTESIAN_POINT ( 'NONE',  ( -17.96206987120463694, 6.006607899627029568, -10.39122312062567133 ) ) ;
#56748 = CARTESIAN_POINT ( 'NONE',  ( 2.000000000000001776, 6.441884263200846839, -2.217201541069800275 ) ) ;
#56749 = AXIS2_PLACEMENT_3D ( 'NONE', #48376, #12753, #63299 ) ;
#56751 = ORIENTED_EDGE ( 'NONE', *, *, #11536, .T. ) ;
#56750 = DIRECTION ( 'NONE',  ( 1.000000000000000000, -0.000000000000000000, -0.000000000000000000 ) ) ;
#56752 = CARTESIAN_POINT ( 'NONE',  ( 2.000000000000001776, 0.000000000000000000, 0.000000000000000000 ) ) ;
#56753 = AXIS2_PLACEMENT_3D ( 'NONE', #43983, #10596, #25919 ) ;
#56754 = ADVANCED_FACE ( 'NONE', ( #23002 ), #41323, .F. ) ;
#56755 = CARTESIAN_POINT ( 'NONE',  ( 1.719304012338701115, -5.690355757827699534, 11.38834240361771677 ) ) ;
#56756 = ORIENTED_EDGE ( 'NONE', *, *, #64808, .T. ) ;
#56757 = CARTESIAN_POINT ( 'NONE',  ( -35.05175862995318425, 0.01139565579896459346, 0.005323180402349095286 ) ) ;
#56758 = ADVANCED_FACE ( 'NONE', ( #8686 ), #37265, .F. ) ;
#56759 = CARTESIAN_POINT ( 'NONE',  ( 36.00000000000000711, -9.621072037176935154, 8.366449238204463512 ) ) ;
#56760 = CARTESIAN_POINT ( 'NONE',  ( 37.00000000000000711, -12.66641127287626745, -1.457575200925504300 ) ) ;
#56761 = DIRECTION ( 'NONE',  ( -0.3865475372811021382, -0.2971585806051909029, 0.8730852074079729075 ) ) ;
#56762 = CARTESIAN_POINT ( 'NONE',  ( 37.00000000000000711, 5.130401251914885385, 11.05394794832823813 ) ) ;
#56763 = AXIS2_PLACEMENT_3D ( 'NONE', #30724, #46371, #35712 ) ;
#56764 = DIRECTION ( 'NONE',  ( 0.000000000000000000, 0.7381862504171974315, -0.6745969609292639113 ) ) ;
#56766 = EDGE_LOOP ( 'NONE', ( #28402, #54923, #5419, #919 ) ) ;
#56765 = CARTESIAN_POINT ( 'NONE',  ( 0.3341166715381319041, 11.44035855572981752, -4.432780143632383485 ) ) ;
#56767 = ORIENTED_EDGE ( 'NONE', *, *, #22697, .T. ) ;
#56768 = CARTESIAN_POINT ( 'NONE',  ( 2.000000000000001776, 6.164400007374783108, 2.900694413976516728 ) ) ;
#56769 = VERTEX_POINT ( 'NONE', #49277 ) ;
#56770 = VECTOR ( 'NONE', #13502, 1000.000000000000000 ) ;
#56771 = EDGE_CURVE ( 'NONE', #62930, #21730, #51282, .T. ) ;
#56772 = CARTESIAN_POINT ( 'NONE',  ( -47.00000000000000711, 0.000000000000000000, 0.000000000000000000 ) ) ;
#56773 = CIRCLE ( 'NONE', #60974, 5.000000000000000888 ) ;
#56774 = CARTESIAN_POINT ( 'NONE',  ( -35.00000000000000000, 11.13736569743281457, -4.946702696913053643 ) ) ;
#56775 = ORIENTED_EDGE ( 'NONE', *, *, #28693, .T. ) ;
#56776 = CARTESIAN_POINT ( 'NONE',  ( -35.00000000000000000, 0.000000000000000000, 0.000000000000000000 ) ) ;
#56777 = CARTESIAN_POINT ( 'NONE',  ( 5.514970785353741078, -0.003262412238248251547, 0.003415090918276177286 ) ) ;
#56778 = FACE_BOUND ( 'NONE', #20452, .T. ) ;
#56779 = EDGE_LOOP ( 'NONE', ( #61963, #52745, #6651, #35101 ) ) ;
#56780 = ORIENTED_EDGE ( 'NONE', *, *, #56721, .T. ) ;
#56781 = DIRECTION ( 'NONE',  ( -1.000000000000000000, 0.000000000000000000, -0.000000000000000000 ) ) ;
#56782 = EDGE_CURVE ( 'NONE', #18567, #57422, #58343, .T. ) ;
#56783 = EDGE_CURVE ( 'NONE', #41081, #38995, #65713, .T. ) ;
#56784 = AXIS2_PLACEMENT_3D ( 'NONE', #40354, #50373, #46351 ) ;
#56785 = ORIENTED_EDGE ( 'NONE', *, *, #61209, .F. ) ;
#56786 = CARTESIAN_POINT ( 'NONE',  ( 0.3665391374699472626, 2.392238720110459571, 12.04754782681758130 ) ) ;
#56787 = CARTESIAN_POINT ( 'NONE',  ( 2.941278708680199916, -5.814102272488574918, -1.972702289976061563 ) ) ;
#56788 = CARTESIAN_POINT ( 'NONE',  ( 10.88606639118328445, 1.033256646594155947, 13.46088457202628241 ) ) ;
#56789 = EDGE_CURVE ( 'NONE', #26248, #20510, #4119, .T. ) ;
#56790 = CARTESIAN_POINT ( 'NONE',  ( 1.014383007554946481, 12.37541872618881200, 1.731118468093957974 ) ) ;
#56791 = DIRECTION ( 'NONE',  ( 0.000000000000000000, 0.000000000000000000, -1.000000000000000000 ) ) ;
#56792 = DIRECTION ( 'NONE',  ( 1.000000000000000000, 0.000000000000000000, 0.000000000000000000 ) ) ;
#56793 = CARTESIAN_POINT ( 'NONE',  ( 2.284126774967665252, 7.503320429541878944, 1.483972655035240562 ) ) ;
#56794 = ORIENTED_EDGE ( 'NONE', *, *, #9823, .T. ) ;
#56795 = DIRECTION ( 'NONE',  ( -1.000000000000000000, 0.000000000000000000, 0.000000000000000000 ) ) ;
#56796 = EDGE_CURVE ( 'NONE', #56264, #35347, #46257, .T. ) ;
#56797 = CYLINDRICAL_SURFACE ( 'NONE', #31074, 4.999999999999999112 ) ;
#56798 = DIRECTION ( 'NONE',  ( 1.000000000000000000, 0.000000000000000000, 0.000000000000000000 ) ) ;
#56799 = DIRECTION ( 'NONE',  ( 0.000000000000000000, 0.01356324068817991828, -0.9999080150203990547 ) ) ;
#56800 = DIRECTION ( 'NONE',  ( 1.000000000000000000, -0.000000000000000000, -0.000000000000000000 ) ) ;
#56801 = CARTESIAN_POINT ( 'NONE',  ( -17.54726996257253191, 11.36053454945672847, 3.865003848717349033 ) ) ;
#56802 = DIRECTION ( 'NONE',  ( 0.000000000000000000, -0.01356324068817999114, 0.9999080150203989437 ) ) ;
#56803 = EDGE_CURVE ( 'NONE', #48103, #37848, #30583, .T. ) ;
#56804 = AXIS2_PLACEMENT_3D ( 'NONE', #53050, #53393, #48412 ) ;
#56805 = ORIENTED_EDGE ( 'NONE', *, *, #32105, .F. ) ;
#56806 = VERTEX_POINT ( 'NONE', #5338 ) ;
#56807 = LINE ( 'NONE', #31500, #17380 ) ;
#56808 = ADVANCED_FACE ( 'NONE', ( #25611 ), #34727, .F. ) ;
#56809 = EDGE_LOOP ( 'NONE', ( #54594, #58487, #29047, #63196 ) ) ;
#56810 = FACE_OUTER_BOUND ( 'NONE', #50751, .T. ) ;
#56811 = DIRECTION ( 'NONE',  ( 0.000000000000000000, -0.01356324068817991828, 0.9999080150203990547 ) ) ;
#56812 = CARTESIAN_POINT ( 'NONE',  ( 0.6473888112830256114, -9.687359867659742108, -7.698027285532567099 ) ) ;
#56813 = DIRECTION ( 'NONE',  ( -1.000000000000000000, 0.000000000000000000, 0.000000000000000000 ) ) ;
#56814 = ORIENTED_EDGE ( 'NONE', *, *, #52702, .T. ) ;
#56815 = CARTESIAN_POINT ( 'NONE',  ( 0.2646305136544065406, 9.465888453932961966, 7.770320294339206235 ) ) ;
#56816 = DIRECTION ( 'NONE',  ( 1.000000000000000000, 0.000000000000000000, 0.000000000000000000 ) ) ;
#56817 = CYLINDRICAL_SURFACE ( 'NONE', #44949, 4.999999999999999112 ) ;
#56818 = CARTESIAN_POINT ( 'NONE',  ( -22.27710395300133683, 2.585700543510496718, 2.620347679538721941 ) ) ;
#56819 = CIRCLE ( 'NONE', #28131, 12.18650000000000055 ) ;
#56820 = DIRECTION ( 'NONE',  ( 0.000000000000000000, -0.01356324068817998940, 0.9999080150203990547 ) ) ;
#56821 = CARTESIAN_POINT ( 'NONE',  ( -28.66013792860432119, -0.1826938850344149434, -1.826836065344826787 ) ) ;
#56822 = ORIENTED_EDGE ( 'NONE', *, *, #19878, .T. ) ;
#56823 = CARTESIAN_POINT ( 'NONE',  ( 2.000000000000001776, 0.000000000000000000, 0.000000000000000000 ) ) ;
#56824 = VERTEX_POINT ( 'NONE', #40911 ) ;
#56825 = CARTESIAN_POINT ( 'NONE',  ( -22.27218376572352554, 3.547715993389680023, -0.9890213205919581307 ) ) ;
#56826 = DIRECTION ( 'NONE',  ( 1.000000000000000000, -0.000000000000000000, 0.000000000000000000 ) ) ;
#56827 = CARTESIAN_POINT ( 'NONE',  ( -37.00000000000000711, 0.000000000000000000, 0.000000000000000000 ) ) ;
#56828 = CIRCLE ( 'NONE', #15406, 5.000000000000000888 ) ;
#56829 = CARTESIAN_POINT ( 'NONE',  ( -30.18541646480307250, -0.9656489334300984995, -13.47303279728103931 ) ) ;
#56830 = CARTESIAN_POINT ( 'NONE',  ( -10.90165637463012516, -7.508992741355087652, 9.360289953322833867 ) ) ;
#56831 = ORIENTED_EDGE ( 'NONE', *, *, #19154, .T. ) ;
#56832 = ORIENTED_EDGE ( 'NONE', *, *, #50012, .T. ) ;
#56833 = CARTESIAN_POINT ( 'NONE',  ( 0.2655924914740778742, 7.838010948425171875, -9.409507842005947253 ) ) ;
#56834 = ORIENTED_EDGE ( 'NONE', *, *, #46263, .T. ) ;
#56835 = ADVANCED_FACE ( 'NONE', ( #4705 ), #30275, .T. ) ;
#56836 = CARTESIAN_POINT ( 'NONE',  ( -27.08417568107324058, -2.261355310631419702, 0.3682236895270578625 ) ) ;
#56838 = AXIS2_PLACEMENT_3D ( 'NONE', #4538, #35734, #51410 ) ;
#56837 = CARTESIAN_POINT ( 'NONE',  ( 2.000000000000001776, -0.4129979343796691404, -6.800241778083718991 ) ) ;
#56839 = DIRECTION ( 'NONE',  ( -1.000000000000000000, 0.000000000000000000, 0.000000000000000000 ) ) ;
#56840 = DIRECTION ( 'NONE',  ( 1.000000000000000000, 0.000000000000000000, -0.000000000000000000 ) ) ;
#56841 = CARTESIAN_POINT ( 'NONE',  ( -17.29244623348158783, 2.525873743887551814, -13.26159725786978072 ) ) ;
#56842 = CYLINDRICAL_SURFACE ( 'NONE', #25400, 3.477897737712717152 ) ;
#56843 = CARTESIAN_POINT ( 'NONE',  ( -10.37062606838457768, -3.961740123981947193, 11.32887242500305724 ) ) ;
#56844 = VERTEX_POINT ( 'NONE', #50575 ) ;
#56845 = CARTESIAN_POINT ( 'NONE',  ( -9.316560581850643175, -10.03332002416863133, -6.593889625719990377 ) ) ;
#56846 = ORIENTED_EDGE ( 'NONE', *, *, #6098, .F. ) ;
#56848 = CARTESIAN_POINT ( 'NONE',  ( 21.81308386904231256, -12.46974327601525623, -5.176071965619618354 ) ) ;
#56847 = CIRCLE ( 'NONE', #28160, 12.74999999999999822 ) ;
#56849 = CARTESIAN_POINT ( 'NONE',  ( 2.665405856346782620, 8.559192023451593911, -4.274976649834382414 ) ) ;
#56850 = EDGE_CURVE ( 'NONE', #28847, #19799, #21556, .T. ) ;
#56851 = ORIENTED_EDGE ( 'NONE', *, *, #14318, .F. ) ;
#56852 = CARTESIAN_POINT ( 'NONE',  ( 41.00000000000000711, -25.18551001833412784, 3.766049837354531693 ) ) ;
#56853 = CARTESIAN_POINT ( 'NONE',  ( -22.27720412283625961, 3.606406551442371100, -0.7407051501189783060 ) ) ;
#56854 = ORIENTED_EDGE ( 'NONE', *, *, #28806, .F. ) ;
#56855 = CARTESIAN_POINT ( 'NONE',  ( 1.000000000000000888, -7.248432822490228133, -1.926193556693104547 ) ) ;
#56856 = CARTESIAN_POINT ( 'NONE',  ( -37.00000000000000711, 0.1414404973752139416, 12.74921544981111232 ) ) ;
#56857 = CARTESIAN_POINT ( 'NONE',  ( 36.00000000000000711, -1.286231064351218478, 12.68495603654572612 ) ) ;
#56858 = VERTEX_POINT ( 'NONE', #36576 ) ;
#56859 = ORIENTED_EDGE ( 'NONE', *, *, #55077, .T. ) ;
#56860 = ORIENTED_EDGE ( 'NONE', *, *, #8285, .T. ) ;
#56861 = ADVANCED_FACE ( 'NONE', ( #15938 ), #21619, .T. ) ;
#56862 = CARTESIAN_POINT ( 'NONE',  ( 1.459561108993787437, -12.08294179906958554, -3.725588117663319210 ) ) ;
#56863 = VERTEX_POINT ( 'NONE', #20939 ) ;
#56864 = VERTEX_POINT ( 'NONE', #26926 ) ;
#56865 = ORIENTED_EDGE ( 'NONE', *, *, #11396, .F. ) ;
#56866 = CARTESIAN_POINT ( 'NONE',  ( 3.152665057735396736, -5.761241965768377327, 5.461013642406604696 ) ) ;
#56867 = EDGE_CURVE ( 'NONE', #57124, #2445, #47226, .T. ) ;
#56868 = CYLINDRICAL_SURFACE ( 'NONE', #42156, 2.899999999999994582 ) ;
#56869 = VECTOR ( 'NONE', #55961, 1000.000000000000000 ) ;
#56870 = CARTESIAN_POINT ( 'NONE',  ( 47.00000000000000711, 4.705694406421931860E-17, -3.469127814946512892E-15 ) ) ;
#56871 = CARTESIAN_POINT ( 'NONE',  ( -27.20164183316780182, 1.232966507052650318, -2.339520810540422602 ) ) ;
#56872 = CARTESIAN_POINT ( 'NONE',  ( -37.00000000000000711, -2.772148766916031182, -11.86701198550359315 ) ) ;
#56873 = ORIENTED_EDGE ( 'NONE', *, *, #31577, .T. ) ;
#56874 = ORIENTED_EDGE ( 'NONE', *, *, #13962, .T. ) ;
#56875 = CARTESIAN_POINT ( 'NONE',  ( 37.00000000000000711, -6.946017217730009463, -10.01317267707884362 ) ) ;
#56876 = CARTESIAN_POINT ( 'NONE',  ( -3.278282182819570956, 12.28207346570795266, 5.615173697092686211 ) ) ;
#56877 = CARTESIAN_POINT ( 'NONE',  ( 35.00000000000000000, -11.38112321385048631, 2.905556151562744382 ) ) ;
#56878 =( GEOMETRIC_REPRESENTATION_CONTEXT ( 3 ) GLOBAL_UNCERTAINTY_ASSIGNED_CONTEXT ( ( #64196 ) ) GLOBAL_UNIT_ASSIGNED_CONTEXT ( ( #50125, #59436, #33824 ) ) REPRESENTATION_CONTEXT ( 'NONE', 'WORKASPACE' ) );
#56879 = CARTESIAN_POINT ( 'NONE',  ( 0.2759803524722184154, -2.313459762622620097, 12.02930579076649131 ) ) ;
#56880 = CARTESIAN_POINT ( 'NONE',  ( 2.000000000000001776, 0.000000000000000000, 0.000000000000000000 ) ) ;
#56881 = DIRECTION ( 'NONE',  ( 0.000000000000000000, 0.01356324068817998940, -0.9999080150203989437 ) ) ;
#56882 = EDGE_CURVE ( 'NONE', #13729, #16301, #24732, .T. ) ;
#56883 = VERTEX_POINT ( 'NONE', #31890 ) ;
#56884 = CARTESIAN_POINT ( 'NONE',  ( 0.000000000000000000, -1.225832621831887792, 6.827324998361543607 ) ) ;
#56885 = AXIS2_PLACEMENT_3D ( 'NONE', #11317, #31904, #51896 ) ;
#56886 = ORIENTED_EDGE ( 'NONE', *, *, #56614, .F. ) ;
#56887 = CARTESIAN_POINT ( 'NONE',  ( 5.536195898058073439, 0.008071068258923183927, -0.002666509901869637631 ) ) ;
#56888 = CARTESIAN_POINT ( 'NONE',  ( 6.904443316226203109, -26.24011843744382233, -14.86481251185162655 ) ) ;
#56889 = CARTESIAN_POINT ( 'NONE',  ( 17.13446681924521187, -29.51054447109572365, 9.416006455614706283 ) ) ;
#56890 = CARTESIAN_POINT ( 'NONE',  ( -27.09030469827880339, -0.6314616953885191508, -2.221523195520538341 ) ) ;
#56891 = DIRECTION ( 'NONE',  ( -1.000000000000000000, 0.000000000000000000, 0.000000000000000000 ) ) ;
#56892 = VERTEX_POINT ( 'NONE', #31571 ) ;
#56893 = DIRECTION ( 'NONE',  ( 0.000000000000000000, -0.01356324068817991828, 0.9999080150203990547 ) ) ;
#56894 = CARTESIAN_POINT ( 'NONE',  ( 0.2869720083484334494, 2.332746648244354404, -12.02930764912518313 ) ) ;
#56895 = PLANE ( 'NONE',  #55553 ) ;
#56896 = CARTESIAN_POINT ( 'NONE',  ( 2.573738926104373714, 3.667129335223202613, 6.822065037112445829 ) ) ;
#56897 = AXIS2_PLACEMENT_3D ( 'NONE', #42565, #51613, #46599 ) ;
#56898 = EDGE_CURVE ( 'NONE', #13688, #30158, #15832, .T. ) ;
#56899 = B_SPLINE_CURVE_WITH_KNOTS ( 'NONE', 3,
 ( #12049, #46647, #36985, #7378, #27030, #12368, #21726, #16403, #57630, #42616, #22703, #1101, #36670, #62260, #2077, #57956, #63244, #58273, #57290 ),
 .UNSPECIFIED., .F., .F.,
 ( 4, 3, 3, 3, 3, 3, 4 ),
 ( 8.930035652772277260E-18, 2.825908398831343367E-05, 4.208813692484080383E-05, 5.591713746944121247E-05, 6.279584083232122042E-05, 9.105792820296874294E-05, 0.0001153131102488825452 ),
 .UNSPECIFIED. ) ;
#56900 = CARTESIAN_POINT ( 'NONE',  ( 2.000000000000001776, 0.000000000000000000, 0.000000000000000000 ) ) ;
#56901 = FACE_OUTER_BOUND ( 'NONE', #4240, .T. ) ;
#56902 = FACE_OUTER_BOUND ( 'NONE', #22234, .T. ) ;
#56903 = CARTESIAN_POINT ( 'NONE',  ( 35.00000000000000000, -12.63095688309027587, 1.738225594540123042 ) ) ;
#56904 = CARTESIAN_POINT ( 'NONE',  ( 2.305787727787084407, 0.1666591538753756929, -7.654065630109506024 ) ) ;
#56905 = CIRCLE ( 'NONE', #607, 12.74999999999999822 ) ;
#56906 = ORIENTED_EDGE ( 'NONE', *, *, #45559, .F. ) ;
#56907 =( BOUNDED_SURFACE ( )  B_SPLINE_SURFACE ( 3, 1, ( 
 ( #13440, #44043 ),
 ( #33410, #12450 ),
 ( #38052, #2165 ),
 ( #22791, #23104 ) ),
 .UNSPECIFIED., .F., .F., .F. ) 
 B_SPLINE_SURFACE_WITH_KNOTS ( ( 4, 4 ),
 ( 2, 2 ),
 ( 0.000000000000000000, 1.000000000000000000 ),
 ( 0.000000000000000000, 1.000000000000000000 ),
 .UNSPECIFIED. ) 
 GEOMETRIC_REPRESENTATION_ITEM ( )  RATIONAL_B_SPLINE_SURFACE ( (
 ( 1.000000000000000000, 1.000000000000000000),
 ( 0.6933888150995267674, 0.9895912004443193632),
 ( 0.6933888150995267674, 0.9895912004443193632),
 ( 1.000000000000000000, 1.000000000000000000) ) ) 
 REPRESENTATION_ITEM ( '' )  SURFACE ( )  );
#56909 = ORIENTED_EDGE ( 'NONE', *, *, #33303, .T. ) ;
#56908 = EDGE_CURVE ( 'NONE', #44784, #6062, #48814, .T. ) ;
#56910 = CARTESIAN_POINT ( 'NONE',  ( 2.491965175174466474, -6.575382551509648899, 4.041154086925387467 ) ) ;
#56911 = CARTESIAN_POINT ( 'NONE',  ( 9.575800908719084958, 25.00000000000000000, -1.072919909436247154 ) ) ;
#56912 = CARTESIAN_POINT ( 'NONE',  ( 1.283627346226613009, -7.660435136228935349, 9.985833283678374528 ) ) ;
#56913 = CARTESIAN_POINT ( 'NONE',  ( 0.3006302518452044215, -1.905681544119320892, 12.10891847026071844 ) ) ;
#56914 = ADVANCED_FACE ( 'NONE', ( #36894 ), #52210, .T. ) ;
#56915 = ORIENTED_EDGE ( 'NONE', *, *, #34994, .T. ) ;
#56916 = VERTEX_POINT ( 'NONE', #682 ) ;
#56917 = ORIENTED_EDGE ( 'NONE', *, *, #31480, .T. ) ;
#56918 = LINE ( 'NONE', #6696, #34427 ) ;
#56919 = CARTESIAN_POINT ( 'NONE',  ( -22.46509356695199600, 1.314379028669554472, 4.038408495643908580 ) ) ;
#56920 = EDGE_CURVE ( 'NONE', #21262, #5276, #27154, .T. ) ;
#56921 = ORIENTED_EDGE ( 'NONE', *, *, #17102, .T. ) ;
#56922 = AXIS2_PLACEMENT_3D ( 'NONE', #30343, #40968, #30644 ) ;
#56923 = CARTESIAN_POINT ( 'NONE',  ( 0.000000000000000000, 0.000000000000000000, 0.000000000000000000 ) ) ;
#56924 = CARTESIAN_POINT ( 'NONE',  ( 37.00000000000000711, 2.936739658819871313, -11.37311665002364869 ) ) ;
#56925 = ORIENTED_EDGE ( 'NONE', *, *, #2915, .F. ) ;
#56926 = CIRCLE ( 'NONE', #35628, 5.000000000000000000 ) ;
#56927 = CARTESIAN_POINT ( 'NONE',  ( -22.30527770659433173, 0.2559941915621863906, 3.757123197210709087 ) ) ;
#56928 =( BOUNDED_SURFACE ( )  B_SPLINE_SURFACE ( 3, 1, ( 
 ( #36321, #36655 ),
 ( #56956, #62555 ),
 ( #17017, #31646 ),
 ( #61270, #51961 ) ),
 .UNSPECIFIED., .F., .F., .F. ) 
 B_SPLINE_SURFACE_WITH_KNOTS ( ( 4, 4 ),
 ( 2, 2 ),
 ( 0.000000000000000000, 1.000000000000000000 ),
 ( 0.000000000000000000, 1.000000000000000000 ),
 .UNSPECIFIED. ) 
 GEOMETRIC_REPRESENTATION_ITEM ( )  RATIONAL_B_SPLINE_SURFACE ( (
 ( 1.000000000000000000, 1.000000000000000000),
 ( 0.6933888150995267674, 0.9895912004443193632),
 ( 0.6933888150995267674, 0.9895912004443193632),
 ( 1.000000000000000000, 1.000000000000000000) ) ) 
 REPRESENTATION_ITEM ( '' )  SURFACE ( )  );
#56929 = CARTESIAN_POINT ( 'NONE',  ( 17.33919137821675349, -29.56463768738087694, -9.168593624349773208 ) ) ;
#56930 = CARTESIAN_POINT ( 'NONE',  ( 24.80106626973253370, -1.726837946067656171, 11.87669879134540096 ) ) ;
#56931 = VERTEX_POINT ( 'NONE', #3650 ) ;
#56932 = CARTESIAN_POINT ( 'NONE',  ( -35.00000000000000000, 0.000000000000000000, 0.000000000000000000 ) ) ;
#56933 = ORIENTED_EDGE ( 'NONE', *, *, #2098, .T. ) ;
#56934 = EDGE_CURVE ( 'NONE', #45445, #429, #16900, .T. ) ;
#56935 = CARTESIAN_POINT ( 'NONE',  ( 3.152665057735980714, 1.848755561853925533, 7.719888720907654545 ) ) ;
#56936 = LINE ( 'NONE', #62875, #10678 ) ;
#56937 = CARTESIAN_POINT ( 'NONE',  ( -13.24204686117196950, -34.10419274375099974, 9.367294588221389162 ) ) ;
#56938 = CARTESIAN_POINT ( 'NONE',  ( -27.35552965826135008, 3.094132632038936404, 0.2619431035391969198 ) ) ;
#56939 = CARTESIAN_POINT ( 'NONE',  ( -35.00000000000000000, 8.146229107149400406, 9.063649021438985542 ) ) ;
#56940 = CARTESIAN_POINT ( 'NONE',  ( 24.82652845881425208, -10.42385221765392700, -8.578654028722157321 ) ) ;
#56941 = CARTESIAN_POINT ( 'NONE',  ( -37.00000000000000711, 7.745827850123013114, 10.12742074351899468 ) ) ;
#56942 = LINE ( 'NONE', #57255, #27811 ) ;
#56943 = VERTEX_POINT ( 'NONE', #28882 ) ;
#56944 = EDGE_CURVE ( 'NONE', #12123, #52081, #45397, .T. ) ;
#56945 = DIRECTION ( 'NONE',  ( 1.000000000000000000, 0.000000000000000000, -0.000000000000000000 ) ) ;
#56946 = ORIENTED_EDGE ( 'NONE', *, *, #26365, .F. ) ;
#56947 = CYLINDRICAL_SURFACE ( 'NONE', #9401, 12.18650000000000055 ) ;
#56948 = CARTESIAN_POINT ( 'NONE',  ( -25.64121911577780466, -4.545061814456073712, 11.11074877336984912 ) ) ;
#56949 = ORIENTED_EDGE ( 'NONE', *, *, #14727, .F. ) ;
#56950 = CARTESIAN_POINT ( 'NONE',  ( 35.00000000000000000, -4.074242145636090662, -12.08151691381188364 ) ) ;
#56951 = CARTESIAN_POINT ( 'NONE',  ( -29.68541646480307250, -1.416020129149132334, 25.00000000000000000 ) ) ;
#56952 = CARTESIAN_POINT ( 'NONE',  ( -37.00000000000000711, 11.44858830469740241, -2.627174906296955381 ) ) ;
#56953 = CARTESIAN_POINT ( 'NONE',  ( -36.00000000000000711, -4.400442035671033203, 11.96656215839367654 ) ) ;
#56954 = DIRECTION ( 'NONE',  ( 1.000000000000000000, 0.000000000000000000, 0.000000000000000000 ) ) ;
#56955 = VERTEX_POINT ( 'NONE', #7625 ) ;
#56956 = CARTESIAN_POINT ( 'NONE',  ( 5.530133899448235191, 0.01149180883054544931, 0.01111090067015091734 ) ) ;
#56957 = ORIENTED_EDGE ( 'NONE', *, *, #24358, .F. ) ;
#56958 = DIRECTION ( 'NONE',  ( 0.000000000000000000, -0.7381862504172023165, 0.6745969609292584712 ) ) ;
#56959 = CARTESIAN_POINT ( 'NONE',  ( -35.00000000000000000, 0.000000000000000000, 0.000000000000000000 ) ) ;
#56960 = DIRECTION ( 'NONE',  ( 0.000000000000000000, 0.9346839223284554299, -0.3554799084908935036 ) ) ;
#56961 = VERTEX_POINT ( 'NONE', #27908 ) ;
#56962 = CARTESIAN_POINT ( 'NONE',  ( 2.000000000000001776, -3.230174184210094168, 5.998318953995296354 ) ) ;
#56963 = EDGE_CURVE ( 'NONE', #43998, #53899, #45561, .T. ) ;
#56964 = CARTESIAN_POINT ( 'NONE',  ( 28.67799586904336806, 11.72473780571475466, 6.702742294911029575 ) ) ;
#56965 = DIRECTION ( 'NONE',  ( -1.000000000000000000, 0.000000000000000000, 0.000000000000000000 ) ) ;
#56966 = CARTESIAN_POINT ( 'NONE',  ( 12.10998784662220551, 10.46621227226785322, -8.526922110106907482 ) ) ;
#56967 = FACE_OUTER_BOUND ( 'NONE', #3546, .T. ) ;
#56968 = DIRECTION ( 'NONE',  ( -1.000000000000000000, 0.000000000000000000, 0.000000000000000000 ) ) ;
#56969 = CARTESIAN_POINT ( 'NONE',  ( 0.6473888112830220587, 4.540486098228977419, 11.51036712212681401 ) ) ;
#56970 = CARTESIAN_POINT ( 'NONE',  ( 3.152665057734129306, -7.923639299008720549, -0.4801242025592799556 ) ) ;
#56971 = ADVANCED_FACE ( 'NONE', ( #49192 ), #38866, .T. ) ;
#56972 = VERTEX_POINT ( 'NONE', #58504 ) ;
#56973 = CARTESIAN_POINT ( 'NONE',  ( 5.514624014163232779, -0.002529391395135328728, -0.003278974416024598489 ) ) ;
#56974 = CARTESIAN_POINT ( 'NONE',  ( 2.000000000000001776, -0.7281529553922385656, 7.464569195442775751 ) ) ;
#56975 = ORIENTED_EDGE ( 'NONE', *, *, #56, .T. ) ;
#56976 = EDGE_CURVE ( 'NONE', #61504, #32257, #38151, .T. ) ;
#56977 = DIRECTION ( 'NONE',  ( -1.000000000000000000, 0.000000000000000000, 0.000000000000000000 ) ) ;
#56978 = CARTESIAN_POINT ( 'NONE',  ( -22.27721056931765631, 3.486117586310729433, 1.183805672860796188 ) ) ;
#56979 = CARTESIAN_POINT ( 'NONE',  ( 9.150617453175268423, 5.808824337495268608, -10.50676510956234289 ) ) ;
#56980 = ORIENTED_EDGE ( 'NONE', *, *, #37229, .F. ) ;
#56981 = DIRECTION ( 'NONE',  ( 1.000000000000000000, 0.000000000000000000, -0.000000000000000000 ) ) ;
#56982 = EDGE_CURVE ( 'NONE', #54227, #64858, #48766, .T. ) ;
#56983 = VERTEX_POINT ( 'NONE', #13572 ) ;
#56984 = CARTESIAN_POINT ( 'NONE',  ( 0.2958664285830420737, -5.936220506376309380, 10.72286791615087154 ) ) ;
#56985 = ORIENTED_EDGE ( 'NONE', *, *, #32919, .T. ) ;
#56986 = EDGE_LOOP ( 'NONE', ( #6151, #21508, #53969, #56565 ) ) ;
#56987 = LINE ( 'NONE', #11412, #36935 ) ;
#56988 = ADVANCED_FACE ( 'NONE', ( #44174 ), #62545, .F. ) ;
#56989 = ORIENTED_EDGE ( 'NONE', *, *, #45933, .T. ) ;
#56990 = CARTESIAN_POINT ( 'NONE',  ( -25.04938166283714196, -9.464668315551032052, 7.379181612682862657 ) ) ;
#56991 = CARTESIAN_POINT ( 'NONE',  ( -22.27756824490284160, -3.558840239148759910, 0.9472004376381163437 ) ) ;
#56992 = CARTESIAN_POINT ( 'NONE',  ( 37.00000000000000711, 4.705694406421931860E-17, -3.469127814946512892E-15 ) ) ;
#56993 = CYLINDRICAL_SURFACE ( 'NONE', #26933, 12.75000000000000178 ) ;
#56994 = EDGE_LOOP ( 'NONE', ( #8563, #54041, #44169, #65795 ) ) ;
#56995 = DIRECTION ( 'NONE',  ( 0.000000000000000000, 0.9289767198167898643, 0.3701381553399183955 ) ) ;
#56996 = EDGE_CURVE ( 'NONE', #44680, #46784, #48217, .T. ) ;
#56997 = CARTESIAN_POINT ( 'NONE',  ( 5.786001662380198418, -26.09353282112645189, 15.10027383179532023 ) ) ;
#56998 = DIRECTION ( 'NONE',  ( -1.000000000000000000, 0.000000000000000000, 0.000000000000000000 ) ) ;
#57000 = ORIENTED_EDGE ( 'NONE', *, *, #56078, .F. ) ;
#56999 = DIRECTION ( 'NONE',  ( 0.000000000000000000, -0.7621620551276289124, -0.6473862847818364630 ) ) ;
#57001 = CARTESIAN_POINT ( 'NONE',  ( -28.25052396502597674, 10.95476879881297272, -4.908481086492510137 ) ) ;
#57002 = ORIENTED_EDGE ( 'NONE', *, *, #56976, .T. ) ;
#57003 = CARTESIAN_POINT ( 'NONE',  ( 1.719304012338401133, 5.690355757826538685, 11.38834240361399885 ) ) ;
#57004 = B_SPLINE_CURVE_WITH_KNOTS ( 'NONE', 3,
 ( #58336, #13741, #44027, #18765, #23757, #64605, #44330, #38709, #13423, #58688, #3487, #39023, #8443, #59010, #17772, #63623, #3819, #39346, #29065 ),
 .UNSPECIFIED., .F., .F.,
 ( 4, 3, 3, 3, 3, 3, 4 ),
 ( 1.987375409620156722E-18, 2.831840207499653289E-05, 4.217266859840511053E-05, 5.602024318396140769E-05, 6.290810167969449146E-05, 9.120440630945766665E-05, 0.0001153103026479744905 ),
 .UNSPECIFIED. ) ;
#57005 = VERTEX_POINT ( 'NONE', #12934 ) ;
#57006 = AXIS2_PLACEMENT_3D ( 'NONE', #43246, #21684, #22305 ) ;
#57007 = DIRECTION ( 'NONE',  ( 1.000000000000000000, 0.000000000000000000, 0.000000000000000000 ) ) ;
#57008 = EDGE_CURVE ( 'NONE', #64838, #20840, #191, .T. ) ;
#57009 = CARTESIAN_POINT ( 'NONE',  ( 2.241536586108913820, -4.912162027558446553, -5.844297002038589817 ) ) ;
#57010 = CARTESIAN_POINT ( 'NONE',  ( 2.268878695253351729, -7.642144312464380640, -0.1481365927654333114 ) ) ;
#57011 = ORIENTED_EDGE ( 'NONE', *, *, #41357, .T. ) ;
#57012 = LINE ( 'NONE', #49011, #53736 ) ;
#57013 = AXIS2_PLACEMENT_3D ( 'NONE', #58215, #11993, #12317 ) ;
#57014 = CARTESIAN_POINT ( 'NONE',  ( 1.719304012338199517, 0.000000000000000000, -12.73084802173761787 ) ) ;
#57015 = LINE ( 'NONE', #35714, #20316 ) ;
#57017 = ORIENTED_EDGE ( 'NONE', *, *, #43181, .F. ) ;
#57016 = EDGE_CURVE ( 'NONE', #26553, #55701, #1023, .T. ) ;
#57018 = VERTEX_POINT ( 'NONE', #14862 ) ;
#57019 = FACE_OUTER_BOUND ( 'NONE', #22971, .T. ) ;
#57020 = VERTEX_POINT ( 'NONE', #9902 ) ;
#57021 = EDGE_CURVE ( 'NONE', #60276, #32830, #50489, .T. ) ;
#57022 = ORIENTED_EDGE ( 'NONE', *, *, #3426, .T. ) ;
#57023 = DIRECTION ( 'NONE',  ( 0.000000000000000000, -0.01356324068818697166, 0.9999080150203988326 ) ) ;
#57024 = CARTESIAN_POINT ( 'NONE',  ( 2.000000000000001776, 4.409940824963509698, -5.354199675985237050 ) ) ;
#57025 = CARTESIAN_POINT ( 'NONE',  ( 35.00000000000000000, -0.2661492558802491248, 12.18359334611896116 ) ) ;
#57026 = CARTESIAN_POINT ( 'NONE',  ( -22.28694879868232803, 1.011812214896746998, 3.570244315741544661 ) ) ;
#57027 = DIRECTION ( 'NONE',  ( 1.000000000000000000, 0.000000000000000000, 0.000000000000000000 ) ) ;
#57028 = CARTESIAN_POINT ( 'NONE',  ( 35.00000000000000000, 4.705694406421931860E-17, -3.469127814946512892E-15 ) ) ;
#57029 = DIRECTION ( 'NONE',  ( -1.000000000000000000, 0.000000000000000000, -0.000000000000000000 ) ) ;
#57030 = ORIENTED_EDGE ( 'NONE', *, *, #28999, .F. ) ;
#57031 = CYLINDRICAL_SURFACE ( 'NONE', #17973, 2.977897737712716708 ) ;
#57032 = CARTESIAN_POINT ( 'NONE',  ( -4.020473488733464329, -8.896967761833661115, 8.055697172489294289 ) ) ;
#57033 = EDGE_CURVE ( 'NONE', #49321, #45757, #49378, .T. ) ;
#57034 = DIRECTION ( 'NONE',  ( 0.000000000000000000, 0.9635499925192219095, 0.2675283385292247518 ) ) ;
#57035 = EDGE_CURVE ( 'NONE', #29113, #50541, #5230, .T. ) ;
#57036 = CYLINDRICAL_SURFACE ( 'NONE', #30043, 12.18650000000000055 ) ;
#57037 = CARTESIAN_POINT ( 'NONE',  ( 0.2651627682582937684, 12.04449770099953732, -2.213224986694458885 ) ) ;
#57038 = CARTESIAN_POINT ( 'NONE',  ( 1.656291714771122692, 0.7705446217105330620, -11.97644560228689414 ) ) ;
#57039 = CARTESIAN_POINT ( 'NONE',  ( 8.623231295854225209, 3.167640682658209528, -11.57732002835950880 ) ) ;
#57040 = ORIENTED_EDGE ( 'NONE', *, *, #29933, .F. ) ;
#57041 = FACE_OUTER_BOUND ( 'NONE', #18671, .T. ) ;
#57042 = CARTESIAN_POINT ( 'NONE',  ( 0.2657645697724732581, -1.977350809428451983, -12.08564806881062736 ) ) ;
#57043 = CYLINDRICAL_SURFACE ( 'NONE', #61935, 10.70557198542813815 ) ;
#57044 = EDGE_CURVE ( 'NONE', #16664, #26657, #42207, .T. ) ;
#57045 = DIRECTION ( 'NONE',  ( -1.000000000000000000, 0.000000000000000000, 0.000000000000000000 ) ) ;
#57046 = CIRCLE ( 'NONE', #15636, 6.936499999999992561 ) ;
#57047 = EDGE_CURVE ( 'NONE', #32997, #27860, #272, .T. ) ;
#57048 = AXIS2_PLACEMENT_3D ( 'NONE', #62209, #35624, #61231 ) ;
#57049 = CARTESIAN_POINT ( 'NONE',  ( 11.32985899526506834, 0.8050469939657922680, -13.47645748469515681 ) ) ;
#57050 = CARTESIAN_POINT ( 'NONE',  ( 5.516018279890452902, -0.003191189039764480428, 0.005976902763918706153 ) ) ;
#57051 = ORIENTED_EDGE ( 'NONE', *, *, #38212, .T. ) ;
#57052 = CARTESIAN_POINT ( 'NONE',  ( -18.90004703488476423, -4.071512182036163274, -12.87324253533143903 ) ) ;
#57053 = CARTESIAN_POINT ( 'NONE',  ( -27.27771710733888710, -13.23190005995061647, -2.725643356596643585 ) ) ;
#57054 = CARTESIAN_POINT ( 'NONE',  ( 0.3675815128205912052, -12.13672785388549080, -1.872154644482208585 ) ) ;
#57055 = ORIENTED_EDGE ( 'NONE', *, *, #2602, .F. ) ;
#57056 = CARTESIAN_POINT ( 'NONE',  ( 2.368238019615304779, 6.736275681109179736, 3.681632831800409900 ) ) ;
#57057 = CARTESIAN_POINT ( 'NONE',  ( 5.514624014163232779, 0.003946330869975252925, 0.001255375129357681665 ) ) ;
#57058 = ADVANCED_FACE ( 'NONE', ( #40825 ), #61548, .F. ) ;
#57060 = ORIENTED_EDGE ( 'NONE', *, *, #28053, .T. ) ;
#57059 = CARTESIAN_POINT ( 'NONE',  ( 2.963017218115621798, 0.9869543242668126215, 7.812878240621073722 ) ) ;
#57061 = CARTESIAN_POINT ( 'NONE',  ( -27.08639648637141661, 2.223359598374790025, 0.5801562253477756670 ) ) ;
#57062 = CARTESIAN_POINT ( 'NONE',  ( 0.2647959493198541181, -4.326188315749660340, -11.45640103018463130 ) ) ;
#57063 = EDGE_LOOP ( 'NONE', ( #24113, #47466, #14746, #19936 ) ) ;
#57064 = DIRECTION ( 'NONE',  ( 0.000000000000000000, -0.3807014730195283359, 0.9246979985058697560 ) ) ;
#57065 = LINE ( 'NONE', #56759, #20258 ) ;
#57066 = CARTESIAN_POINT ( 'NONE',  ( 24.36224182249226899, -0.009850770392023379049, -12.00517586461388575 ) ) ;
#57067 = LINE ( 'NONE', #46426, #58483 ) ;
#57068 = CARTESIAN_POINT ( 'NONE',  ( 0.2869720083484367246, -11.44147823180128043, -4.386174336869709478 ) ) ;
#57069 = EDGE_CURVE ( 'NONE', #3618, #18279, #39505, .T. ) ;
#57070 = CARTESIAN_POINT ( 'NONE',  ( -22.00000000000000711, -20.00000000000000000, 2.449293598294706907E-15 ) ) ;
#57072 = ORIENTED_EDGE ( 'NONE', *, *, #48586, .T. ) ;
#57071 = DIRECTION ( 'NONE',  ( -1.000000000000000000, 0.000000000000000000, 0.000000000000000000 ) ) ;
#57073 = EDGE_CURVE ( 'NONE', #43919, #38911, #29693, .T. ) ;
#57074 = VERTEX_POINT ( 'NONE', #51794 ) ;
#57075 = CARTESIAN_POINT ( 'NONE',  ( 24.68219558003250924, 0.8422048916808957397, -11.97679777458489347 ) ) ;
#57076 = ORIENTED_EDGE ( 'NONE', *, *, #48405, .F. ) ;
#57077 = DIRECTION ( 'NONE',  ( 1.000000000000000000, 0.000000000000000000, 0.000000000000000000 ) ) ;
#57078 = CARTESIAN_POINT ( 'NONE',  ( 0.5547464869798240938, -11.49049644196206899, 4.506704303875415540 ) ) ;
#57079 = ADVANCED_FACE ( 'NONE', ( #52116 ), #48749, .F. ) ;
#57080 = CIRCLE ( 'NONE', #16863, 7.499999999999988454 ) ;
#57081 = CARTESIAN_POINT ( 'NONE',  ( 2.305787727787084407, 1.493241775258423720, 7.508843116234161563 ) ) ;
#57082 = EDGE_CURVE ( 'NONE', #1623, #14535, #8450, .T. ) ;
#57083 = DIRECTION ( 'NONE',  ( -1.000000000000000000, 0.000000000000000000, 0.000000000000000000 ) ) ;
#57084 = ORIENTED_EDGE ( 'NONE', *, *, #6794, .T. ) ;
#57085 = DIRECTION ( 'NONE',  ( -1.000000000000000000, 0.000000000000000000, 0.000000000000000000 ) ) ;
#57086 = DIRECTION ( 'NONE',  ( -1.000000000000000000, 0.000000000000000000, 0.000000000000000000 ) ) ;
#57087 = CARTESIAN_POINT ( 'NONE',  ( -22.27718112499583469, -1.380338971069141829, 3.412978993569784070 ) ) ;
#57088 = VERTEX_POINT ( 'NONE', #1252 ) ;
#57089 = VERTEX_POINT ( 'NONE', #23086 ) ;
#57090 = EDGE_CURVE ( 'NONE', #65658, #19640, #34997, .T. ) ;
#57091 = CARTESIAN_POINT ( 'NONE',  ( 29.09509651717319301, -8.201516007081412596, 10.73123560021122636 ) ) ;
#57092 = ORIENTED_EDGE ( 'NONE', *, *, #6342, .F. ) ;
#57093 = B_SPLINE_CURVE_WITH_KNOTS ( 'NONE', 3,
 ( #31025, #31354, #51333, #41313, #36668, #16046, #36336, #56645, #11081, #51658 ),
 .UNSPECIFIED., .F., .F.,
 ( 4, 2, 2, 2, 4 ),
 ( 0.000000000000000000, 0.001226751953743790424, 0.002453503907487580848, 0.003680255861231371273, 0.004907007814975161697 ),
 .UNSPECIFIED. ) ;
#57094 = CARTESIAN_POINT ( 'NONE',  ( 2.241449424704146320, 1.265244293929188579, -7.528892370271778489 ) ) ;
#57095 = AXIS2_PLACEMENT_3D ( 'NONE', #61734, #42100, #16195 ) ;
#57096 = CARTESIAN_POINT ( 'NONE',  ( 0.2646305136544065406, -4.064188116014626040, 11.55263159009957263 ) ) ;
#57097 = CARTESIAN_POINT ( 'NONE',  ( 0.2648978790185584908, 6.237101853238694815, -10.53870023327857197 ) ) ;
#57098 = CARTESIAN_POINT ( 'NONE',  ( 47.00000000000000711, 4.705694406421931860E-17, -3.469127814946512892E-15 ) ) ;
#57099 = CARTESIAN_POINT ( 'NONE',  ( 0.000000000000000000, 6.539067737394503865, 2.314222412769824544 ) ) ;
#57100 = CARTESIAN_POINT ( 'NONE',  ( 0.000000000000000000, -6.338823199656649088, -2.816798305433765748 ) ) ;
#57101 = CIRCLE ( 'NONE', #7141, 20.19615242270663558 ) ;
#57102 = CARTESIAN_POINT ( 'NONE',  ( 2.290907136833257418, 7.504812001538602395, 1.488079974904968683 ) ) ;
#57103 = ORIENTED_EDGE ( 'NONE', *, *, #40071, .F. ) ;
#57104 =( BOUNDED_SURFACE ( )  B_SPLINE_SURFACE ( 3, 1, ( 
 ( #17204, #41813 ),
 ( #57122, #36147 ),
 ( #42438, #7208 ),
 ( #6253, #21545 ) ),
 .UNSPECIFIED., .F., .F., .F. ) 
 B_SPLINE_SURFACE_WITH_KNOTS ( ( 4, 4 ),
 ( 2, 2 ),
 ( 0.000000000000000000, 1.000000000000000000 ),
 ( 0.000000000000000000, 1.000000000000000000 ),
 .UNSPECIFIED. ) 
 GEOMETRIC_REPRESENTATION_ITEM ( )  RATIONAL_B_SPLINE_SURFACE ( (
 ( 1.000000000000000000, 1.000000000000000000),
 ( 0.9942764183789327692, 0.8450855930916580938),
 ( 0.9942764183789327692, 0.8450855930916580938),
 ( 1.000000000000000000, 1.000000000000000000) ) ) 
 REPRESENTATION_ITEM ( '' )  SURFACE ( )  );
#57105 = CARTESIAN_POINT ( 'NONE',  ( 37.00000000000000711, 8.854740511458958352, 7.717887834988148121 ) ) ;
#57106 = ORIENTED_EDGE ( 'NONE', *, *, #33029, .T. ) ;
#57107 = CARTESIAN_POINT ( 'NONE',  ( 2.963017218115632012, 4.265970453344018587, -6.619413971958168830 ) ) ;
#57108 = CARTESIAN_POINT ( 'NONE',  ( -35.05012975565874456, 0.01089417657933950019, -0.008684292310216024449 ) ) ;
#57109 = CARTESIAN_POINT ( 'NONE',  ( -8.891032880924177206, 11.36194426013951997, -3.860857758255646921 ) ) ;
#57110 = CARTESIAN_POINT ( 'NONE',  ( 2.907497136250430714, -3.021847490615451992, -7.252103438786913436 ) ) ;
#57111 = DIRECTION ( 'NONE',  ( 1.000000000000000000, -0.000000000000000000, -0.000000000000000000 ) ) ;
#57112 = B_SPLINE_CURVE_WITH_KNOTS ( 'NONE', 3,
 ( #60148, #64790, #14571, #24244, #59837, #25225, #28916 ),
 .UNSPECIFIED., .F., .F.,
 ( 4, 3, 4 ),
 ( 0.000000000000000000, 0.001700533616330529530, 0.005002426799372189890 ),
 .UNSPECIFIED. ) ;
#57113 = DIRECTION ( 'NONE',  ( -1.000000000000000000, 0.000000000000000000, 0.000000000000000000 ) ) ;
#57114 = ORIENTED_EDGE ( 'NONE', *, *, #376, .F. ) ;
#57115 = ADVANCED_FACE ( 'NONE', ( #21533 ), #38365, .T. ) ;
#57116 = ORIENTED_EDGE ( 'NONE', *, *, #39861, .T. ) ;
#57117 = DIRECTION ( 'NONE',  ( 0.000000000000000000, -0.4380125133593848474, 0.8989688749565218906 ) ) ;
#57118 = EDGE_CURVE ( 'NONE', #59596, #54960, #32139, .T. ) ;
#57119 = ORIENTED_EDGE ( 'NONE', *, *, #16212, .F. ) ;
#57120 = DIRECTION ( 'NONE',  ( -1.000000000000000000, 0.000000000000000000, 0.000000000000000000 ) ) ;
#57121 = CARTESIAN_POINT ( 'NONE',  ( 37.00000000000000711, -11.02904044024205987, 4.041347439435972966 ) ) ;
#57122 = CARTESIAN_POINT ( 'NONE',  ( 5.515188684475870851, 0.004804816249379309685, 0.002355816063606825262 ) ) ;
#57123 = CARTESIAN_POINT ( 'NONE',  ( 2.276198483117258142, 1.479169956994163870, -7.501576331167719047 ) ) ;
#57124 = VERTEX_POINT ( 'NONE', #41799 ) ;
#57125 = CARTESIAN_POINT ( 'NONE',  ( 3.459614771489464946, -11.09853614738469396, 25.00000000000000000 ) ) ;
#57126 = CARTESIAN_POINT ( 'NONE',  ( 2.889800649504073782, -3.986129653162679087, 4.645655809191351793 ) ) ;
#57127 = EDGE_CURVE ( 'NONE', #37616, #18279, #45605, .T. ) ;
#57128 = CARTESIAN_POINT ( 'NONE',  ( 2.941278708680199916, -4.788765081995603801, -3.842273877444612129 ) ) ;
#57129 = CARTESIAN_POINT ( 'NONE',  ( -39.53125591517013504, -1.906753238347176582, 20.35939770057402498 ) ) ;
#57130 = VECTOR ( 'NONE', #50715, 1000.000000000000000 ) ;
#57131 = CARTESIAN_POINT ( 'NONE',  ( 0.3537226245948368875, 6.362463382302413706, -10.49813096858602890 ) ) ;
#57132 = CARTESIAN_POINT ( 'NONE',  ( -36.00000000000000711, -12.08151691381193160, 4.074242145635959211 ) ) ;
#57133 = AXIS2_PLACEMENT_3D ( 'NONE', #2418, #62565, #37309 ) ;
#57134 = VERTEX_POINT ( 'NONE', #63622 ) ;
#57135 = CARTESIAN_POINT ( 'NONE',  ( -19.56743653832047158, -29.00000000000000000, -5.000000000000000888 ) ) ;
#57136 = ORIENTED_EDGE ( 'NONE', *, *, #53370, .F. ) ;
#57137 = VECTOR ( 'NONE', #65335, 1000.000000000000000 ) ;
#57138 = CARTESIAN_POINT ( 'NONE',  ( 35.00000000000000000, -11.42599468261425955, 4.237620530777920003 ) ) ;
#57139 = DIRECTION ( 'NONE',  ( 0.000000000000000000, 0.000000000000000000, -1.000000000000000000 ) ) ;
#57140 = DIRECTION ( 'NONE',  ( 0.000000000000000000, -0.01356324068817992175, 0.9999080150203990547 ) ) ;
#57141 = ADVANCED_FACE ( 'NONE', ( #11860 ), #37127, .T. ) ;
#57142 = AXIS2_PLACEMENT_3D ( 'NONE', #40316, #59974, #65274 ) ;
#57143 = CARTESIAN_POINT ( 'NONE',  ( -35.00000000000000000, -9.506317355798309165, -8.496612874013260708 ) ) ;
#57144 = EDGE_CURVE ( 'NONE', #34377, #35021, #62093, .T. ) ;
#57145 = CARTESIAN_POINT ( 'NONE',  ( 35.00000000000000000, -9.040300684349746874, -7.499679039484027143 ) ) ;
#57146 = ORIENTED_EDGE ( 'NONE', *, *, #13564, .T. ) ;
#57147 = ORIENTED_EDGE ( 'NONE', *, *, #34289, .F. ) ;
#57148 = ORIENTED_EDGE ( 'NONE', *, *, #49184, .T. ) ;
#57149 = CARTESIAN_POINT ( 'NONE',  ( -37.00000000000000711, 11.73808581813437968, -0.4353888892048790038 ) ) ;
#57150 = CARTESIAN_POINT ( 'NONE',  ( 3.152665057734040488, 0.000000000000000000, 0.000000000000000000 ) ) ;
#57151 = DIRECTION ( 'NONE',  ( 1.000000000000000000, 0.000000000000000000, -0.000000000000000000 ) ) ;
#57152 = CARTESIAN_POINT ( 'NONE',  ( 35.00000000000000000, 4.705694406421931860E-17, -3.469127814946512892E-15 ) ) ;
#57153 = CARTESIAN_POINT ( 'NONE',  ( 37.00000000000000711, -10.07641281632173325, 6.036400161834665212 ) ) ;
#57154 = CARTESIAN_POINT ( 'NONE',  ( -10.95212338237647920, -9.902220863987562183, 9.175839033069923545 ) ) ;
#57155 = CARTESIAN_POINT ( 'NONE',  ( 0.5572780756296079607, 12.20533540249751248, -1.841882550626559922 ) ) ;
#57156 = ORIENTED_EDGE ( 'NONE', *, *, #6828, .F. ) ;
#57157 = CARTESIAN_POINT ( 'NONE',  ( 1.547277799338534710, -5.744300480442291246, 11.29700934613309293 ) ) ;
#57158 = EDGE_LOOP ( 'NONE', ( #47518, #56957, #30309, #3217 ) ) ;
#57159 = CYLINDRICAL_SURFACE ( 'NONE', #65291, 5.000000000000001776 ) ;
#57160 = ADVANCED_FACE ( 'NONE', ( #5597 ), #29548, .T. ) ;
#57161 = CARTESIAN_POINT ( 'NONE',  ( -37.00000000000000711, -2.905556151562544986, -11.38112321385053960 ) ) ;
#57162 = DIRECTION ( 'NONE',  ( 0.000000000000000000, -0.01356324068817992175, 0.9999080150203990547 ) ) ;
#57163 = EDGE_CURVE ( 'NONE', #38173, #34288, #39039, .T. ) ;
#57164 = DIRECTION ( 'NONE',  ( 0.000000000000000000, -0.01356324068817998940, 0.9999080150203990547 ) ) ;
#57165 = ORIENTED_EDGE ( 'NONE', *, *, #53900, .F. ) ;
#57166 = LINE ( 'NONE', #31548, #21641 ) ;
#57167 = DIRECTION ( 'NONE',  ( 0.000000000000000000, 0.01356324068817998940, -0.9999080150203990547 ) ) ;
#57168 = AXIS2_PLACEMENT_3D ( 'NONE', #34733, #34429, #3208 ) ;
#57169 = CARTESIAN_POINT ( 'NONE',  ( 2.969415267404682091, 3.055358878717733706, 7.260393470501830038 ) ) ;
#57170 = VERTEX_POINT ( 'NONE', #21864 ) ;
#57171 = VERTEX_POINT ( 'NONE', #42108 ) ;
#57172 = EDGE_CURVE ( 'NONE', #10928, #44959, #21055, .T. ) ;
#57173 = CARTESIAN_POINT ( 'NONE',  ( 0.3463514696222815270, 0.2404099497127392404, 13.50000000000000533 ) ) ;
#57174 = ORIENTED_EDGE ( 'NONE', *, *, #55958, .F. ) ;
#57175 = ORIENTED_EDGE ( 'NONE', *, *, #39496, .T. ) ;
#57176 = ORIENTED_EDGE ( 'NONE', *, *, #52964, .T. ) ;
#57177 = ORIENTED_EDGE ( 'NONE', *, *, #45645, .T. ) ;
#57178 = CARTESIAN_POINT ( 'NONE',  ( 0.2834382757448007384, 4.380429851625326165, 11.44241760114836914 ) ) ;
#57180 = CIRCLE ( 'NONE', #15755, 12.74999999999999822 ) ;
#57179 = DIRECTION ( 'NONE',  ( 0.000000000000000000, 0.1081190184239417679, -0.9941379571543595972 ) ) ;
#57181 = DIRECTION ( 'NONE',  ( 0.000000000000000000, 0.7790879021242529401, -0.6269146997507959451 ) ) ;
#57182 = CARTESIAN_POINT ( 'NONE',  ( 35.00000000000000000, -9.196955404009232282, 8.830544224263039865 ) ) ;
#57183 = DIRECTION ( 'NONE',  ( 0.000000000000000000, 0.8515178078024887576, -0.5243256840888532722 ) ) ;
#57184 = ORIENTED_EDGE ( 'NONE', *, *, #29438, .T. ) ;
#57185 = EDGE_CURVE ( 'NONE', #32930, #44305, #63682, .T. ) ;
#57186 = CARTESIAN_POINT ( 'NONE',  ( 1.000000000000000888, -0.08317740279936355896, 7.499538753794337431 ) ) ;
#57187 = CIRCLE ( 'NONE', #49761, 12.18650000000000055 ) ;
#57188 = CIRCLE ( 'NONE', #39115, 5.000000000000001776 ) ;
#57189 = ORIENTED_EDGE ( 'NONE', *, *, #6607, .T. ) ;
#57190 = DIRECTION ( 'NONE',  ( 0.000000000000000000, 0.01356324068817998940, -0.9999080150203990547 ) ) ;
#57191 = FACE_OUTER_BOUND ( 'NONE', #4142, .T. ) ;
#57192 = CIRCLE ( 'NONE', #7279, 5.000000000000000000 ) ;
#57193 = CARTESIAN_POINT ( 'NONE',  ( 0.2646305136544072623, 0.1321451301297840164, 12.24595685781654630 ) ) ;
#57194 = CARTESIAN_POINT ( 'NONE',  ( 0.2671309869109488311, -7.995521393275754285, -9.276621593297592838 ) ) ;
#57195 = CARTESIAN_POINT ( 'NONE',  ( 5.515188684475870851, -0.002355816063606962739, -0.004804816249378818759 ) ) ;
#57196 = CARTESIAN_POINT ( 'NONE',  ( -35.00000000000000000, 11.59605747147786836, 5.300372733891681953 ) ) ;
#57197 = CIRCLE ( 'NONE', #65651, 12.74999999999999822 ) ;
#57198 = ORIENTED_EDGE ( 'NONE', *, *, #38849, .T. ) ;
#57199 = DIRECTION ( 'NONE',  ( 0.000000000000000000, 0.01356324068817992175, -0.9999080150203990547 ) ) ;
#57200 = ADVANCED_FACE ( 'NONE', ( #4453 ), #3486, .T. ) ;
#57201 = ORIENTED_EDGE ( 'NONE', *, *, #11639, .F. ) ;
#57202 = CARTESIAN_POINT ( 'NONE',  ( -35.00000000000000000, -11.65554240571058031, 1.456211999474302798 ) ) ;
#57203 = CARTESIAN_POINT ( 'NONE',  ( 19.41740522748896680, -28.99999999999999645, -5.485033347092790557 ) ) ;
#57204 = DIRECTION ( 'NONE',  ( 0.000000000000000000, -0.01356324068817998940, 0.9999080150203990547 ) ) ;
#57205 = CARTESIAN_POINT ( 'NONE',  ( 2.406456491625719618, 6.212289237905720185, -8.382123850279317168 ) ) ;
#57206 = DIRECTION ( 'NONE',  ( -1.000000000000000000, 0.000000000000000000, 0.000000000000000000 ) ) ;
#57207 = VERTEX_POINT ( 'NONE', #64937 ) ;
#57208 = FACE_OUTER_BOUND ( 'NONE', #42812, .T. ) ;
#57209 = CARTESIAN_POINT ( 'NONE',  ( -10.48620311856347875, -9.720786832536937538, -9.367833439828894271 ) ) ;
#57210 = DIRECTION ( 'NONE',  ( 0.000000000000000000, 0.000000000000000000, 1.000000000000000000 ) ) ;
#57211 = CARTESIAN_POINT ( 'NONE',  ( 0.2651627923886310523, -2.039714259676093544, -12.07509237025072935 ) ) ;
#57212 = CIRCLE ( 'NONE', #17900, 4.999999999999999112 ) ;
#57213 = CARTESIAN_POINT ( 'NONE',  ( 5.520433897694421610, -0.005630909886753050243, -0.01397038704729912546 ) ) ;
#57214 = AXIS2_PLACEMENT_3D ( 'NONE', #51711, #60689, #45714 ) ;
#57215 = LINE ( 'NONE', #26611, #55066 ) ;
#57217 = EDGE_CURVE ( 'NONE', #16200, #34346, #39683, .T. ) ;
#57216 = CARTESIAN_POINT ( 'NONE',  ( 1.937114397841935398, -11.72279974487467236, 5.226660192101551416 ) ) ;
#57218 = EDGE_CURVE ( 'NONE', #27530, #7920, #12901, .T. ) ;
#57219 = VECTOR ( 'NONE', #32991, 1000.000000000000000 ) ;
#57220 = ORIENTED_EDGE ( 'NONE', *, *, #62272, .F. ) ;
#57221 = CIRCLE ( 'NONE', #31710, 4.999999999999999112 ) ;
#57222 = AXIS2_PLACEMENT_3D ( 'NONE', #25334, #40290, #60582 ) ;
#57223 = VERTEX_POINT ( 'NONE', #9094 ) ;
#57224 = CARTESIAN_POINT ( 'NONE',  ( -22.46509356695200665, 4.038408495643943219, -1.314379028669518057 ) ) ;
#57225 = FACE_OUTER_BOUND ( 'NONE', #64109, .T. ) ;
#57226 = DIRECTION ( 'NONE',  ( -1.000000000000000000, 0.000000000000000000, 0.000000000000000000 ) ) ;
#57227 = CIRCLE ( 'NONE', #8378, 6.936499999999992561 ) ;
#57228 = CARTESIAN_POINT ( 'NONE',  ( -47.00000000000000711, 0.000000000000000000, 0.000000000000000000 ) ) ;
#57229 = VERTEX_POINT ( 'NONE', #59981 ) ;
#57230 = ORIENTED_EDGE ( 'NONE', *, *, #15126, .T. ) ;
#57231 = CIRCLE ( 'NONE', #50874, 7.499999999999988454 ) ;
#57232 = VERTEX_POINT ( 'NONE', #39022 ) ;
#57233 = DIRECTION ( 'NONE',  ( 0.000000000000000000, 0.000000000000000000, 1.000000000000000000 ) ) ;
#57234 = EDGE_CURVE ( 'NONE', #10479, #39914, #13740, .T. ) ;
#57235 = FACE_OUTER_BOUND ( 'NONE', #24755, .T. ) ;
#57236 = ORIENTED_EDGE ( 'NONE', *, *, #12914, .T. ) ;
#57237 = CARTESIAN_POINT ( 'NONE',  ( 6.812204945636112896, -4.138731716409435712, 12.84993773446340803 ) ) ;
#57238 = CARTESIAN_POINT ( 'NONE',  ( 25.00000000000000711, -9.999999999999998224, -24.00000000000000000 ) ) ;
#57239 = ORIENTED_EDGE ( 'NONE', *, *, #21483, .T. ) ;
#57240 = CYLINDRICAL_SURFACE ( 'NONE', #38564, 12.74999999999999822 ) ;
#57241 = FACE_OUTER_BOUND ( 'NONE', #44235, .T. ) ;
#57242 = CYLINDRICAL_SURFACE ( 'NONE', #36688, 12.75000000000000178 ) ;
#57243 = ORIENTED_EDGE ( 'NONE', *, *, #26220, .F. ) ;
#57244 = CARTESIAN_POINT ( 'NONE',  ( 1.000000000000000888, 3.795144977083718008, -6.468916029978776017 ) ) ;
#57245 = EDGE_LOOP ( 'NONE', ( #6445, #36029, #9650, #38566 ) ) ;
#57246 = LINE ( 'NONE', #37273, #16712 ) ;
#57247 = CARTESIAN_POINT ( 'NONE',  ( 2.241536586108912488, 4.912162027558490074, 5.844297002038559619 ) ) ;
#57248 = CYLINDRICAL_SURFACE ( 'NONE', #35126, 5.000000000000000888 ) ;
#57249 = ADVANCED_FACE ( 'NONE', ( #59648, #39345 ), #14075, .F. ) ;
#57250 = DIRECTION ( 'NONE',  ( 1.000000000000000000, 0.000000000000000000, 0.000000000000000000 ) ) ;
#57252 = CARTESIAN_POINT ( 'NONE',  ( 37.00000000000000711, 8.496612874013157679, -9.506317355798403312 ) ) ;
#57251 = VECTOR ( 'NONE', #36905, 1000.000000000000114 ) ;
#57253 = CARTESIAN_POINT ( 'NONE',  ( -36.00000000000000711, 7.379373053629018742, -10.39746860227882763 ) ) ;
#57254 = DIRECTION ( 'NONE',  ( -1.000000000000000000, -0.000000000000000000, 0.000000000000000000 ) ) ;
#57255 = CARTESIAN_POINT ( 'NONE',  ( 12.47628546223243617, 0.000000000000000000, 25.00000000000000000 ) ) ;
#57256 = EDGE_LOOP ( 'NONE', ( #5646, #16859, #53252, #7687 ) ) ;
#57257 = DIRECTION ( 'NONE',  ( 0.000000000000000000, -0.01356324068817999114, 0.9999080150203989437 ) ) ;
#57258 = VERTEX_POINT ( 'NONE', #34028 ) ;
#57259 = AXIS2_PLACEMENT_3D ( 'NONE', #58167, #32867, #38532 ) ;
#57260 = DIRECTION ( 'NONE',  ( -1.000000000000000000, 0.000000000000000000, 0.000000000000000000 ) ) ;
#57261 = FACE_OUTER_BOUND ( 'NONE', #20698, .T. ) ;
#57262 = EDGE_LOOP ( 'NONE', ( #63464, #44588, #51261, #62417 ) ) ;
#57263 = CARTESIAN_POINT ( 'NONE',  ( -18.58686583997225839, 5.151216734910813777, 10.83812558286603789 ) ) ;
#57264 = FACE_OUTER_BOUND ( 'NONE', #4480, .T. ) ;
#57265 = DIRECTION ( 'NONE',  ( -1.000000000000000000, 0.000000000000000000, 0.000000000000000000 ) ) ;
#57266 = CARTESIAN_POINT ( 'NONE',  ( -22.27834755396593991, -3.497967921180582973, -1.162947663292853706 ) ) ;
#57267 = CIRCLE ( 'NONE', #9431, 5.000000000000000000 ) ;
#57268 = AXIS2_PLACEMENT_3D ( 'NONE', #58122, #17227, #63097 ) ;
#57269 = ORIENTED_EDGE ( 'NONE', *, *, #5872, .F. ) ;
#57270 = ORIENTED_EDGE ( 'NONE', *, *, #1033, .F. ) ;
#57271 = LINE ( 'NONE', #46633, #25827 ) ;
#57272 = CIRCLE ( 'NONE', #21178, 5.000000000000000000 ) ;
#57273 = EDGE_CURVE ( 'NONE', #61621, #65150, #19745, .T. ) ;
#57274 = VERTEX_POINT ( 'NONE', #34364 ) ;
#57275 = CARTESIAN_POINT ( 'NONE',  ( 3.152665057734045373, -6.378477742800418682, 4.725420687650736085 ) ) ;
#57276 = DIRECTION ( 'NONE',  ( 1.000000000000000000, 0.000000000000000000, 0.000000000000000000 ) ) ;
#57277 = EDGE_CURVE ( 'NONE', #48941, #44984, #28626, .T. ) ;
#57278 = CYLINDRICAL_SURFACE ( 'NONE', #16927, 4.999999999999999112 ) ;
#57279 = ORIENTED_EDGE ( 'NONE', *, *, #5860, .F. ) ;
#57280 = AXIS2_PLACEMENT_3D ( 'NONE', #17982, #17665, #32588 ) ;
#57281 = DIRECTION ( 'NONE',  ( -1.000000000000000000, 0.000000000000000000, 0.000000000000000000 ) ) ;
#57282 = EDGE_CURVE ( 'NONE', #3877, #21253, #65759, .T. ) ;
#57283 =( BOUNDED_CURVE ( )  B_SPLINE_CURVE ( 3, ( #62568, #4546, #26357, #36978 ),
 .UNSPECIFIED., .F., .F. ) 
 B_SPLINE_CURVE_WITH_KNOTS ( ( 4, 4 ),
 ( 2.328873244820985011, 2.340611521109171811 ),
 .UNSPECIFIED. ) 
 CURVE ( )  GEOMETRIC_REPRESENTATION_ITEM ( )  RATIONAL_B_SPLINE_CURVE ( ( 1.000000000000000000, 0.9999885177721090646, 0.9999885177721090646, 1.000000000000000000 ) ) 
 REPRESENTATION_ITEM ( '' )  );
#57284 = CARTESIAN_POINT ( 'NONE',  ( 29.03190650753573010, 11.07607182691292280, 7.728831390951418356 ) ) ;
#57285 = DIRECTION ( 'NONE',  ( 0.000000000000000000, -0.01356324068817999114, 0.9999080150203989437 ) ) ;
#57286 = CARTESIAN_POINT ( 'NONE',  ( 35.00000000000000000, 3.704519465651471499, 11.60979404548630178 ) ) ;
#57287 = CARTESIAN_POINT ( 'NONE',  ( -37.00000000000000711, 4.824807283154123994, 11.80185301892982608 ) ) ;
#57288 = LINE ( 'NONE', #772, #23512 ) ;
#57289 = EDGE_CURVE ( 'NONE', #48293, #52670, #56239, .T. ) ;
#57290 = CARTESIAN_POINT ( 'NONE',  ( 2.241352910868908310, -5.794346703933879184, 4.970878533273742406 ) ) ;
#57291 = FACE_OUTER_BOUND ( 'NONE', #53202, .T. ) ;
#57292 = CIRCLE ( 'NONE', #64712, 12.18650000000000233 ) ;
#57293 = ORIENTED_EDGE ( 'NONE', *, *, #40818, .F. ) ;
#57294 = DIRECTION ( 'NONE',  ( 0.000000000000000000, 0.000000000000000000, 1.000000000000000000 ) ) ;
#57295 = CARTESIAN_POINT ( 'NONE',  ( 0.3537226245948391079, -12.27287980220284425, -0.2609894354290803187 ) ) ;
#57296 = ORIENTED_EDGE ( 'NONE', *, *, #15074, .F. ) ;
#57297 =( BOUNDED_SURFACE ( )  B_SPLINE_SURFACE ( 3, 1, ( 
 ( #29350, #19722 ),
 ( #50311, #419 ),
 ( #5076, #49966 ),
 ( #55932, #61243 ) ),
 .UNSPECIFIED., .F., .F., .F. ) 
 B_SPLINE_SURFACE_WITH_KNOTS ( ( 4, 4 ),
 ( 2, 2 ),
 ( 0.000000000000000000, 1.000000000000000000 ),
 ( 0.000000000000000000, 1.000000000000000000 ),
 .UNSPECIFIED. ) 
 GEOMETRIC_REPRESENTATION_ITEM ( )  RATIONAL_B_SPLINE_SURFACE ( (
 ( 1.000000000000000000, 1.000000000000000000),
 ( 0.8716676215708681896, 0.8964445200148167814),
 ( 0.8716676215708681896, 0.8964445200148167814),
 ( 1.000000000000000000, 1.000000000000000000) ) ) 
 REPRESENTATION_ITEM ( '' )  SURFACE ( )  );
#57298 = AXIS2_PLACEMENT_3D ( 'NONE', #8125, #34674, #65279 ) ;
#57299 = DIRECTION ( 'NONE',  ( 0.000000000000000000, 0.9651210252299803338, 0.2618041379715599914 ) ) ;
#57300 = FACE_OUTER_BOUND ( 'NONE', #25690, .T. ) ;
#57301 = ORIENTED_EDGE ( 'NONE', *, *, #4260, .T. ) ;
#57302 = CYLINDRICAL_SURFACE ( 'NONE', #5516, 2.899999999999994582 ) ;
#57303 = ORIENTED_EDGE ( 'NONE', *, *, #30080, .F. ) ;
#57304 = CARTESIAN_POINT ( 'NONE',  ( 0.3006302518452070860, -5.932248915294235481, 10.72687985734940064 ) ) ;
#57305 = ORIENTED_EDGE ( 'NONE', *, *, #37646, .T. ) ;
#57306 = ORIENTED_EDGE ( 'NONE', *, *, #45329, .F. ) ;
#57307 = CARTESIAN_POINT ( 'NONE',  ( -27.10719052120871098, -1.310802520592025955, -1.962717903527680718 ) ) ;
#57308 = VERTEX_POINT ( 'NONE', #54001 ) ;
#57309 = CARTESIAN_POINT ( 'NONE',  ( -26.09207032238876423, -10.32898249965824355, 6.109300428488008805 ) ) ;
#57310 = CARTESIAN_POINT ( 'NONE',  ( 1.020182472823633058, -11.58401323226483370, -4.691131056023109203 ) ) ;
#57311 = CIRCLE ( 'NONE', #28638, 7.499999999999988454 ) ;
#57312 = DIRECTION ( 'NONE',  ( -1.000000000000000000, 0.000000000000000000, 0.000000000000000000 ) ) ;
#57313 = CARTESIAN_POINT ( 'NONE',  ( 1.283627346226880794, -0.5505361391623975198, -12.57362488724982086 ) ) ;
#57314 = VERTEX_POINT ( 'NONE', #9399 ) ;
#57315 = CARTESIAN_POINT ( 'NONE',  ( 0.3654063281920739148, -7.689576266239727786, 9.573804659448637011 ) ) ;
#57316 = CARTESIAN_POINT ( 'NONE',  ( -2.136460567204509164, -31.12783502484143128, 14.34456412933875846 ) ) ;
#57317 = CARTESIAN_POINT ( 'NONE',  ( 2.368238019615417134, -7.674602282636111994, 0.1797502808085719161 ) ) ;
#57319 = ORIENTED_EDGE ( 'NONE', *, *, #47801, .T. ) ;
#57318 = DIRECTION ( 'NONE',  ( 1.000000000000000000, -0.000000000000000000, 0.000000000000000000 ) ) ;
#57320 = DIRECTION ( 'NONE',  ( 0.000000000000000000, -0.01356324068817991828, 0.9999080150203990547 ) ) ;
#57321 = EDGE_LOOP ( 'NONE', ( #37517, #24278, #11024, #60990 ) ) ;
#57322 = CARTESIAN_POINT ( 'NONE',  ( 37.00000000000000711, 12.31350058095522826, -3.307597835713291801 ) ) ;
#57323 = VECTOR ( 'NONE', #6300, 1000.000000000000000 ) ;
#57324 = VERTEX_POINT ( 'NONE', #24380 ) ;
#57325 = CARTESIAN_POINT ( 'NONE',  ( 23.59784752820392839, -9.149736952257297773, -7.769756470210803734 ) ) ;
#57326 = CYLINDRICAL_SURFACE ( 'NONE', #31053, 12.74999999999999822 ) ;
#57327 = CARTESIAN_POINT ( 'NONE',  ( 1.287602823385623152, -4.819820779359250018, 11.62763122279965522 ) ) ;
#57328 = EDGE_CURVE ( 'NONE', #52513, #32250, #5277, .T. ) ;
#57329 = ORIENTED_EDGE ( 'NONE', *, *, #35696, .T. ) ;
#57330 = CARTESIAN_POINT ( 'NONE',  ( 2.305787727787084407, 6.545285700970527643, 3.971363876083986888 ) ) ;
#57331 = CARTESIAN_POINT ( 'NONE',  ( 2.000000000000001776, 6.777474576704068276, 0.6925993764990892032 ) ) ;
#57332 = CARTESIAN_POINT ( 'NONE',  ( -22.29770266787582145, -3.635870259503085844, -0.8895590726607217613 ) ) ;
#57333 = VERTEX_POINT ( 'NONE', #63966 ) ;
#57334 = VERTEX_POINT ( 'NONE', #18448 ) ;
#57335 = DIRECTION ( 'NONE',  ( -0.000000000000000000, -0.000000000000000000, -1.000000000000000000 ) ) ;
#57336 = ORIENTED_EDGE ( 'NONE', *, *, #19776, .F. ) ;
#57337 = VERTEX_POINT ( 'NONE', #8779 ) ;
#57338 = CARTESIAN_POINT ( 'NONE',  ( -37.00000000000000711, -8.052525312709946093, 8.551552972817052733 ) ) ;
#57339 = DIRECTION ( 'NONE',  ( 0.000000000000000000, -0.01356324068817991828, 0.9999080150203990547 ) ) ;
#57340 = B_SPLINE_CURVE_WITH_KNOTS ( 'NONE', 3,
 ( #25340, #26013, #61560, #30642, #35311, #30983 ),
 .UNSPECIFIED., .F., .F.,
 ( 4, 2, 4 ),
 ( 0.0002637379172017404469, 0.0009975831966478627272, 0.001731428476093984682 ),
 .UNSPECIFIED. ) ;
#57341 = CARTESIAN_POINT ( 'NONE',  ( -37.00000000000000711, 0.000000000000000000, 0.000000000000000000 ) ) ;
#57342 = CARTESIAN_POINT ( 'NONE',  ( -22.29382655386184808, 1.036465316386264712, 3.584644999358078454 ) ) ;
#57343 = DIRECTION ( 'NONE',  ( -1.000000000000000000, 0.000000000000000000, 0.000000000000000000 ) ) ;
#57344 = CARTESIAN_POINT ( 'NONE',  ( -37.00000000000000711, 0.000000000000000000, 0.000000000000000000 ) ) ;
#57345 = AXIS2_PLACEMENT_3D ( 'NONE', #31660, #21030, #46642 ) ;
#57346 = EDGE_CURVE ( 'NONE', #13346, #12647, #38708, .T. ) ;
#57347 = AXIS2_PLACEMENT_3D ( 'NONE', #57861, #62813, #52545 ) ;
#57348 = DIRECTION ( 'NONE',  ( 1.000000000000000000, -0.000000000000000000, 0.000000000000000000 ) ) ;
#57349 = EDGE_CURVE ( 'NONE', #31372, #34842, #21207, .T. ) ;
#57350 = VERTEX_POINT ( 'NONE', #44329 ) ;
#57351 = ADVANCED_FACE ( 'NONE', ( #64604, #448 ), #5432, .F. ) ;
#57352 = CARTESIAN_POINT ( 'NONE',  ( -22.28939870658739864, -3.068935452695155774, 2.099199915896291291 ) ) ;
#57353 = CARTESIAN_POINT ( 'NONE',  ( -3.908087423533649130, -8.112892239103171477, 8.853223187161773922 ) ) ;
#57354 = VECTOR ( 'NONE', #1216, 1000.000000000000000 ) ;
#57355 = CARTESIAN_POINT ( 'NONE',  ( 0.2657645697724715927, 4.330388001246573637, -11.45515365350257042 ) ) ;
#57356 = CARTESIAN_POINT ( 'NONE',  ( 35.00000000000000000, 4.705694406421931860E-17, -3.469127814946512892E-15 ) ) ;
#57357 = EDGE_CURVE ( 'NONE', #64161, #46955, #41539, .T. ) ;
#57358 = CIRCLE ( 'NONE', #39301, 5.000000000000000000 ) ;
#57359 = DIRECTION ( 'NONE',  ( -1.000000000000000000, 0.000000000000000000, 0.000000000000000000 ) ) ;
#57360 = EDGE_CURVE ( 'NONE', #4651, #14286, #62583, .T. ) ;
#57361 = CARTESIAN_POINT ( 'NONE',  ( -27.08429572838383947, -2.208905845566027537, -0.6096735944848257205 ) ) ;
#57362 = VERTEX_POINT ( 'NONE', #6092 ) ;
#57363 = CARTESIAN_POINT ( 'NONE',  ( -27.08418179957658367, 0.4604195552868272645, 2.244544746853581962 ) ) ;
#57364 = FACE_OUTER_BOUND ( 'NONE', #50122, .T. ) ;
#57365 = CARTESIAN_POINT ( 'NONE',  ( 3.152665057735448251, 0.9030954876725900693, -7.886634106564547331 ) ) ;
#57366 = FACE_OUTER_BOUND ( 'NONE', #6267, .T. ) ;
#57367 = ADVANCED_FACE ( 'NONE', ( #55296 ), #9680, .F. ) ;
#57368 = CARTESIAN_POINT ( 'NONE',  ( 8.937200413559439838, 4.243156749116337778, -12.81821838531965518 ) ) ;
#57369 = CARTESIAN_POINT ( 'NONE',  ( -26.05227667049377160, -12.02424670906742321, 6.138434551438939124 ) ) ;
#57370 = ORIENTED_EDGE ( 'NONE', *, *, #42690, .T. ) ;
#57371 = CARTESIAN_POINT ( 'NONE',  ( 3.152665057736253829, 5.761241965767907480, -5.461013642407265500 ) ) ;
#57372 = CARTESIAN_POINT ( 'NONE',  ( 2.000000000000001776, 0.000000000000000000, 0.000000000000000000 ) ) ;
#57373 = CARTESIAN_POINT ( 'NONE',  ( 2.259830038564642596, -4.804964945109423624, -5.940579220576854169 ) ) ;
#57375 = EDGE_CURVE ( 'NONE', #34835, #61726, #54124, .T. ) ;
#57374 = DIRECTION ( 'NONE',  ( 0.000000000000000000, 0.000000000000000000, 1.000000000000000000 ) ) ;
#57376 = VERTEX_POINT ( 'NONE', #41304 ) ;
#57377 = CARTESIAN_POINT ( 'NONE',  ( 2.589278595513552883, 6.829211973730671126, 3.664724287895261945 ) ) ;
#57378 = DIRECTION ( 'NONE',  ( -1.000000000000000000, 0.000000000000000000, 0.000000000000000000 ) ) ;
#57380 = ORIENTED_EDGE ( 'NONE', *, *, #14467, .T. ) ;
#57379 = CARTESIAN_POINT ( 'NONE',  ( 37.00000000000000711, 7.474872387601131152, 9.060822531525964507 ) ) ;
#57381 = CARTESIAN_POINT ( 'NONE',  ( 36.00000000000000711, -10.23119532541067045, 7.608228585767832897 ) ) ;
#57382 = AXIS2_PLACEMENT_3D ( 'NONE', #12870, #38130, #12524 ) ;
#57383 = MECHANICAL_DESIGN_GEOMETRIC_PRESENTATION_REPRESENTATION (  '', ( #17031 ), #23405 ) ;
#57384 = AXIS2_PLACEMENT_3D ( 'NONE', #14737, #29090, #34697 ) ;
#57385 = DIRECTION ( 'NONE',  ( 0.000000000000000000, 0.000000000000000000, 1.000000000000000000 ) ) ;
#57386 = ORIENTED_EDGE ( 'NONE', *, *, #13658, .F. ) ;
#57387 = CARTESIAN_POINT ( 'NONE',  ( -7.489022030332961322, 25.00000000000000000, -10.84914964302385521 ) ) ;
#57388 = FACE_OUTER_BOUND ( 'NONE', #19462, .T. ) ;
#57389 = DIRECTION ( 'NONE',  ( -1.000000000000000000, 0.000000000000000000, 0.000000000000000000 ) ) ;
#57390 = CARTESIAN_POINT ( 'NONE',  ( -3.854685187122629308, -9.944885401855350082, 9.163283342679498844 ) ) ;
#57391 = CARTESIAN_POINT ( 'NONE',  ( 3.152665057734040488, 0.000000000000000000, 0.000000000000000000 ) ) ;
#57392 = CYLINDRICAL_SURFACE ( 'NONE', #29159, 4.999999999999999112 ) ;
#57394 = ORIENTED_EDGE ( 'NONE', *, *, #62308, .T. ) ;
#57393 = CARTESIAN_POINT ( 'NONE',  ( -35.00000000000000000, 4.983891302653582933, 11.73555825188278234 ) ) ;
#57395 = ORIENTED_EDGE ( 'NONE', *, *, #3136, .T. ) ;
#57396 = DIRECTION ( 'NONE',  ( 1.000000000000000000, -0.000000000000000000, 0.000000000000000000 ) ) ;
#57397 = ORIENTED_EDGE ( 'NONE', *, *, #56867, .T. ) ;
#57398 = APPLICATION_PROTOCOL_DEFINITION ( 'draft international standard', 'automotive_design', 1998, #6035 ) ;
#57399 = FACE_OUTER_BOUND ( 'NONE', #39566, .T. ) ;
#57400 = CIRCLE ( 'NONE', #51052, 5.000000000000000000 ) ;
#57401 = CARTESIAN_POINT ( 'NONE',  ( 9.575800908719084958, 11.95193887484099093, -1.072919909436247154 ) ) ;
#57402 = EDGE_CURVE ( 'NONE', #30420, #11603, #9516, .T. ) ;
#57403 = CARTESIAN_POINT ( 'NONE',  ( 2.000000000000001776, 6.767909380267608022, 2.119450094687893138 ) ) ;
#57405 = ORIENTED_EDGE ( 'NONE', *, *, #54895, .T. ) ;
#57404 = CIRCLE ( 'NONE', #55304, 6.936499999999990784 ) ;
#57406 = CARTESIAN_POINT ( 'NONE',  ( 5.514624014163232779, -0.003498325728817824280, 0.002216125254993654876 ) ) ;
#57407 = CARTESIAN_POINT ( 'NONE',  ( -35.00000000000000000, 4.946702696913171771, 11.13736569743276306 ) ) ;
#57408 = ORIENTED_EDGE ( 'NONE', *, *, #63777, .F. ) ;
#57409 = ORIENTED_EDGE ( 'NONE', *, *, #57218, .F. ) ;
#57410 = CARTESIAN_POINT ( 'NONE',  ( 2.251152103363643686, -7.218942724308478276, -2.494172441821568498 ) ) ;
#57411 = EDGE_CURVE ( 'NONE', #36759, #35917, #39252, .T. ) ;
#57412 = ORIENTED_EDGE ( 'NONE', *, *, #39849, .T. ) ;
#57413 = CIRCLE ( 'NONE', #17111, 5.000000000000000888 ) ;
#57414 = CARTESIAN_POINT ( 'NONE',  ( 2.241352910868908310, 1.243507963608194045, -7.532448145350496560 ) ) ;
#57415 = DIRECTION ( 'NONE',  ( -1.000000000000000000, 0.000000000000000000, 0.000000000000000000 ) ) ;
#57416 = CARTESIAN_POINT ( 'NONE',  ( 9.380725061917582153, 2.629308567162621735, 13.24320193369290877 ) ) ;
#57417 = DIRECTION ( 'NONE',  ( -1.000000000000000000, 0.000000000000000000, 0.000000000000000000 ) ) ;
#57418 = CARTESIAN_POINT ( 'NONE',  ( -22.30625920655495165, 0.8854385781085528651, -3.687109008463846926 ) ) ;
#57419 = DIRECTION ( 'NONE',  ( 1.000000000000000000, 0.000000000000000000, 0.000000000000000000 ) ) ;
#57420 = EDGE_CURVE ( 'NONE', #34013, #29113, #6372, .T. ) ;
#57421 = FACE_OUTER_BOUND ( 'NONE', #34713, .T. ) ;
#57422 = VERTEX_POINT ( 'NONE', #25703 ) ;
#57423 = DIRECTION ( 'NONE',  ( 0.000000000000000000, 0.9868265225415254749, 0.1617819965527686754 ) ) ;
#57424 = ORIENTED_EDGE ( 'NONE', *, *, #50453, .F. ) ;
#57425 = AXIS2_PLACEMENT_3D ( 'NONE', #30469, #45432, #60739 ) ;
#57426 = CARTESIAN_POINT ( 'NONE',  ( 37.00000000000000711, 4.946702696913328090, 11.13736569743268845 ) ) ;
#57427 = EDGE_CURVE ( 'NONE', #24785, #44673, #14826, .T. ) ;
#57428 = CARTESIAN_POINT ( 'NONE',  ( -22.51237073810381517, 3.263711251981947115, 2.986282257334718526 ) ) ;
#57429 = CARTESIAN_POINT ( 'NONE',  ( -8.602359018442378158, 8.118472317678492089, -8.864987646168081881 ) ) ;
#57430 = CARTESIAN_POINT ( 'NONE',  ( 2.253265082352433168, -3.929729351083036448, 6.549959928643428242 ) ) ;
#57431 = CARTESIAN_POINT ( 'NONE',  ( 0.2872850955227733705, -10.71476594226529855, -5.944938343726364316 ) ) ;
#57432 = DIRECTION ( 'NONE',  ( -1.000000000000000000, 0.000000000000000000, 0.000000000000000000 ) ) ;
#57433 = ORIENTED_EDGE ( 'NONE', *, *, #10741, .F. ) ;
#57434 = CIRCLE ( 'NONE', #26672, 12.74999999999999822 ) ;
#57435 = CIRCLE ( 'NONE', #93, 12.74999999999999822 ) ;
#57436 = ORIENTED_EDGE ( 'NONE', *, *, #38182, .T. ) ;
#57437 = CIRCLE ( 'NONE', #28754, 12.18650000000000055 ) ;
#57438 = DIRECTION ( 'NONE',  ( -1.000000000000000000, 0.000000000000000000, 0.000000000000000000 ) ) ;
#57439 = EDGE_LOOP ( 'NONE', ( #39080, #42065 ) ) ;
#57440 = VECTOR ( 'NONE', #27393, 1000.000000000000114 ) ;
#57441 = CARTESIAN_POINT ( 'NONE',  ( 0.3006302518452004802, 7.704827863860923109, -9.533790235540664071 ) ) ;
#57442 = EDGE_CURVE ( 'NONE', #16864, #27117, #6555, .T. ) ;
#57443 = CARTESIAN_POINT ( 'NONE',  ( 35.00000000000000000, 4.705694406421931860E-17, -3.469127814946512892E-15 ) ) ;
#57444 = CARTESIAN_POINT ( 'NONE',  ( 35.00000000000000000, -7.817610399097575602, -8.766823244861962294 ) ) ;
#57445 = CARTESIAN_POINT ( 'NONE',  ( 0.2653519890538380555, 6.776488011961817416E-18, -12.24619734961521722 ) ) ;
#57446 = ADVANCED_FACE ( 'NONE', ( #21362 ), #7051, .T. ) ;
#57447 = ORIENTED_EDGE ( 'NONE', *, *, #52394, .T. ) ;
#57448 = CARTESIAN_POINT ( 'NONE',  ( 0.2834382757448011825, 12.09963924911735234, 1.927645269570926523 ) ) ;
#57449 = DIRECTION ( 'NONE',  ( 1.000000000000000000, -0.000000000000000000, -0.000000000000000000 ) ) ;
#57450 = CARTESIAN_POINT ( 'NONE',  ( 0.2650492433740058718, -10.66007796911765126, -6.027445608088962459 ) ) ;
#57451 = DIRECTION ( 'NONE',  ( -1.000000000000000000, 0.000000000000000000, 0.000000000000000000 ) ) ;
#57452 = EDGE_CURVE ( 'NONE', #38595, #33373, #23353, .T. ) ;
#57453 = AXIS2_PLACEMENT_3D ( 'NONE', #38162, #53496, #48827 ) ;
#57454 = AXIS2_PLACEMENT_3D ( 'NONE', #30682, #39696, #19428 ) ;
#57455 = EDGE_CURVE ( 'NONE', #8028, #34466, #13746, .T. ) ;
#57457 = ADVANCED_FACE ( 'NONE', ( #62901 ), #37644, .T. ) ;
#57456 = AXIS2_PLACEMENT_3D ( 'NONE', #65201, #19, #19670 ) ;
#57458 = CARTESIAN_POINT ( 'NONE',  ( 24.82652845881425208, 25.00000000000000000, -8.578654028722157321 ) ) ;
#57459 = AXIS2_PLACEMENT_3D ( 'NONE', #61780, #41832, #47487 ) ;
#57460 = CARTESIAN_POINT ( 'NONE',  ( 9.650000913499871658, -11.97776111335497795, -0.7481793053950416272 ) ) ;
#57461 = VERTEX_POINT ( 'NONE', #61927 ) ;
#57463 = EDGE_CURVE ( 'NONE', #9113, #29799, #47758, .T. ) ;
#57462 = CARTESIAN_POINT ( 'NONE',  ( -18.19295774167957447, -28.79006254106626272, -7.843687167517533254 ) ) ;
#57464 = ORIENTED_EDGE ( 'NONE', *, *, #50393, .T. ) ;
#57465 = CARTESIAN_POINT ( 'NONE',  ( 0.000000000000000000, 6.997684042076945055, -2.698595569414161677 ) ) ;
#57466 = CARTESIAN_POINT ( 'NONE',  ( 0.000000000000000000, 0.000000000000000000, 0.000000000000000000 ) ) ;
#57467 = LINE ( 'NONE', #1928, #23468 ) ;
#57468 = AXIS2_PLACEMENT_3D ( 'NONE', #18256, #43840, #47854 ) ;
#57469 = DIRECTION ( 'NONE',  ( 1.000000000000000000, -0.000000000000000000, 0.000000000000000000 ) ) ;
#57470 = FACE_OUTER_BOUND ( 'NONE', #12345, .T. ) ;
#57471 = VERTEX_POINT ( 'NONE', #31979 ) ;
#57472 = ORIENTED_EDGE ( 'NONE', *, *, #23425, .F. ) ;
#57473 = CARTESIAN_POINT ( 'NONE',  ( 0.2869720083484354478, 1.922200714744161099, 12.10169797402141967 ) ) ;
#57474 = EDGE_LOOP ( 'NONE', ( #23706, #34787, #33533, #46838 ) ) ;
#57475 = AXIS2_PLACEMENT_3D ( 'NONE', #43245, #2387, #43571 ) ;
#57476 = CARTESIAN_POINT ( 'NONE',  ( -27.08421860617808008, -2.271664812096781727, 0.2990745872176354681 ) ) ;
#57477 = CARTESIAN_POINT ( 'NONE',  ( 35.00000000000000000, 4.705694406421931860E-17, -3.469127814946512892E-15 ) ) ;
#57478 = CARTESIAN_POINT ( 'NONE',  ( -35.00000000000000000, 0.000000000000000000, 0.000000000000000000 ) ) ;
#57479 = CARTESIAN_POINT ( 'NONE',  ( 1.104777566491150997, 3.832109395972810084, -11.92547689818819201 ) ) ;
#57480 = FACE_OUTER_BOUND ( 'NONE', #19170, .T. ) ;
#57481 = CARTESIAN_POINT ( 'NONE',  ( 2.259830038566069899, 5.763537486834052537, 5.015955067337202422 ) ) ;
#57482 = CARTESIAN_POINT ( 'NONE',  ( 1.549075743848461251, 12.58108552526874213, -1.533250336941020864 ) ) ;
#57483 = EDGE_LOOP ( 'NONE', ( #65140, #26627, #54119, #26997 ) ) ;
#57484 = CIRCLE ( 'NONE', #131, 12.75000000000000178 ) ;
#57485 = CYLINDRICAL_SURFACE ( 'NONE', #16193, 5.000000000000000888 ) ;
#57486 = VERTEX_POINT ( 'NONE', #41963 ) ;
#57487 = FACE_OUTER_BOUND ( 'NONE', #51946, .T. ) ;
#57489 = DIRECTION ( 'NONE',  ( -1.000000000000000000, 0.000000000000000000, 0.000000000000000000 ) ) ;
#57488 = AXIS2_PLACEMENT_3D ( 'NONE', #4302, #18941, #29245 ) ;
#57490 = EDGE_CURVE ( 'NONE', #51040, #3036, #55051, .T. ) ;
#57491 = AXIS2_PLACEMENT_3D ( 'NONE', #36979, #56965, #57285 ) ;
#57492 = AXIS2_PLACEMENT_3D ( 'NONE', #1277, #27502, #47800 ) ;
#57493 = CARTESIAN_POINT ( 'NONE',  ( 35.00000000000000000, 4.705694406421931860E-17, -3.469127814946512892E-15 ) ) ;
#57494 = ORIENTED_EDGE ( 'NONE', *, *, #40611, .T. ) ;
#57495 = CARTESIAN_POINT ( 'NONE',  ( 5.536195898058073439, -0.007896796515810315664, -0.003145317580921232464 ) ) ;
#57496 =( BOUNDED_CURVE ( )  B_SPLINE_CURVE ( 3, ( #39211, #34550, #38903, #44207 ),
 .UNSPECIFIED., .F., .F. ) 
 B_SPLINE_CURVE_WITH_KNOTS ( ( 4, 4 ),
 ( 1.082322874641048704, 1.128276431546378022 ),
 .UNSPECIFIED. ) 
 CURVE ( )  GEOMETRIC_REPRESENTATION_ITEM ( )  RATIONAL_B_SPLINE_CURVE ( ( 1.000000000000000000, 0.9998240302925252010, 0.9998240302925252010, 1.000000000000000000 ) ) 
 REPRESENTATION_ITEM ( '' )  );
#57497 = FACE_OUTER_BOUND ( 'NONE', #45587, .T. ) ;
#57498 = DIRECTION ( 'NONE',  ( 0.000000000000000000, -0.9796553971857721033, -0.2006870767258996657 ) ) ;
#57499 = VERTEX_POINT ( 'NONE', #52300 ) ;
#57501 = EDGE_LOOP ( 'NONE', ( #18693, #36172, #52443, #823 ) ) ;
#57500 = B_SPLINE_CURVE_WITH_KNOTS ( 'NONE', 3,
 ( #6593, #57131, #21884, #46485, #32159, #7217, #37816, #12523, #36833, #52143, #41824, #12213, #31513, #16230, #22533, #17549, #62413, #937, #41476 ),
 .UNSPECIFIED., .F., .F.,
 ( 4, 3, 3, 3, 3, 3, 4 ),
 ( 9.311523146975038413E-18, 4.457896483014980806E-05, 6.639290541542299884E-05, 8.820687556479185447E-05, 0.0001100173248778954196, 0.0001545671401658161410, 0.0001830328308068609891 ),
 .UNSPECIFIED. ) ;
#57502 = LINE ( 'NONE', #5995, #18365 ) ;
#57503 = ORIENTED_EDGE ( 'NONE', *, *, #37502, .F. ) ;
#57504 = B_SPLINE_CURVE_WITH_KNOTS ( 'NONE', 3,
 ( #49566, #43560, #3703, #33271, #53576, #13954, #54216, #8022, #8660, #4002 ),
 .UNSPECIFIED., .F., .F.,
 ( 4, 3, 3, 4 ),
 ( 5.401523115762192401E-05, 0.0008136511341527791425, 0.004068255670953087148, 0.005063778443040924809 ),
 .UNSPECIFIED. ) ;
#57505 = ORIENTED_EDGE ( 'NONE', *, *, #56226, .T. ) ;
#57506 = EDGE_CURVE ( 'NONE', #58835, #37505, #15941, .T. ) ;
#57507 = ORIENTED_EDGE ( 'NONE', *, *, #51653, .T. ) ;
#57508 = VERTEX_POINT ( 'NONE', #27647 ) ;
#57509 = AXIS2_PLACEMENT_3D ( 'NONE', #40723, #51039, #36716 ) ;
#57510 = CARTESIAN_POINT ( 'NONE',  ( 0.3675815128205894289, 4.447030445008180344, 11.44679196252410946 ) ) ;
#57511 = CARTESIAN_POINT ( 'NONE',  ( 2.000000000000001776, 0.000000000000000000, 0.000000000000000000 ) ) ;
#57512 = CIRCLE ( 'NONE', #37358, 1.750000000000000000 ) ;
#57513 = DIRECTION ( 'NONE',  ( 0.000000000000000000, 0.01356324068817999114, -0.9999080150203990547 ) ) ;
#57514 = DIRECTION ( 'NONE',  ( 0.000000000000000000, 0.000000000000000000, 1.000000000000000000 ) ) ;
#57515 = DIRECTION ( 'NONE',  ( 1.000000000000000000, -0.000000000000000000, 0.000000000000000000 ) ) ;
#57516 = VERTEX_POINT ( 'NONE', #11380 ) ;
#57517 = AXIS2_PLACEMENT_3D ( 'NONE', #64148, #38882, #59172 ) ;
#57518 = CYLINDRICAL_SURFACE ( 'NONE', #31157, 12.75000000000000178 ) ;
#57519 = ORIENTED_EDGE ( 'NONE', *, *, #49382, .F. ) ;
#57520 = CARTESIAN_POINT ( 'NONE',  ( -29.76531599071173062, -3.714239038275569449, -12.97905452356682865 ) ) ;
#57521 = CARTESIAN_POINT ( 'NONE',  ( 35.00000000000000000, 8.699265615723106748, 8.534258022645994757 ) ) ;
#57522 = DIRECTION ( 'NONE',  ( 1.000000000000000000, 0.000000000000000000, 0.000000000000000000 ) ) ;
#57523 = ADVANCED_FACE ( 'NONE', ( #17699 ), #47309, .F. ) ;
#57524 = CARTESIAN_POINT ( 'NONE',  ( 0.3223008802179246901, -8.069628056118055781, -9.236652594547214434 ) ) ;
#57525 = CARTESIAN_POINT ( 'NONE',  ( -37.00000000000000711, -12.01765980939843281, 2.021542716731355771 ) ) ;
#57526 = CIRCLE ( 'NONE', #18212, 2.999999999999995559 ) ;
#57527 = CYLINDRICAL_SURFACE ( 'NONE', #50409, 12.18649999999999878 ) ;
#57528 = VERTEX_POINT ( 'NONE', #12677 ) ;
#57529 = DIRECTION ( 'NONE',  ( -1.000000000000000000, 0.000000000000000000, 0.000000000000000000 ) ) ;
#57530 = AXIS2_PLACEMENT_3D ( 'NONE', #30176, #51126, #30806 ) ;
#57531 = EDGE_LOOP ( 'NONE', ( #48993, #36375, #2459, #33913 ) ) ;
#57532 = CARTESIAN_POINT ( 'NONE',  ( 0.3665391374699464300, -4.447929964102923961, 11.44911061034385114 ) ) ;
#57533 = CARTESIAN_POINT ( 'NONE',  ( 0.3675815128205894289, -0.2638082659429279997, 12.27743992903066150 ) ) ;
#57534 = CARTESIAN_POINT ( 'NONE',  ( -35.00000000000000000, -5.428340790341781741, 10.91072401419408777 ) ) ;
#57536 = AXIS2_PLACEMENT_3D ( 'NONE', #20745, #41329, #11722 ) ;
#57535 = DIRECTION ( 'NONE',  ( 0.000000000000000000, -0.8696919319575131535, -0.4935949184179356797 ) ) ;
#57537 = CARTESIAN_POINT ( 'NONE',  ( 2.262775599886257538, -6.687241191563680687, 3.697834000591617709 ) ) ;
#57538 = ORIENTED_EDGE ( 'NONE', *, *, #28898, .T. ) ;
#57539 = DIRECTION ( 'NONE',  ( 0.000000000000000000, 0.01356324068817992175, -0.9999080150203990547 ) ) ;
#57540 = CARTESIAN_POINT ( 'NONE',  ( 0.2911222467163533945, 2.338869407811021706, -12.02952766044173494 ) ) ;
#57541 = CARTESIAN_POINT ( 'NONE',  ( 2.177405672432017880, 2.605669267166041969, 10.89176600224714697 ) ) ;
#57542 = CARTESIAN_POINT ( 'NONE',  ( 0.2650492433740059828, -2.234874822562814778, -12.04046084639675662 ) ) ;
#57543 = EDGE_CURVE ( 'NONE', #27353, #36393, #31649, .T. ) ;
#57544 = ADVANCED_FACE ( 'NONE', ( #48305 ), #12032, .T. ) ;
#57545 = CIRCLE ( 'NONE', #28853, 12.74999999999999822 ) ;
#57546 = CIRCLE ( 'NONE', #59664, 12.18650000000000411 ) ;
#57547 = ADVANCED_FACE ( 'NONE', ( #21710 ), #41639, .T. ) ;
#57548 = CARTESIAN_POINT ( 'NONE',  ( -22.31328051695926007, -1.671726071983958839, 3.401210163132545539 ) ) ;
#57549 = ORIENTED_EDGE ( 'NONE', *, *, #47111, .F. ) ;
#57551 = EDGE_CURVE ( 'NONE', #25513, #9187, #46940, .T. ) ;
#57550 = CARTESIAN_POINT ( 'NONE',  ( 2.589278595512887193, -0.2408616556819203613, -7.746633201027049331 ) ) ;
#57552 = CARTESIAN_POINT ( 'NONE',  ( -35.00000000000000000, -11.86701198550358427, 2.772148766916072926 ) ) ;
#57553 = VECTOR ( 'NONE', #49973, 1000.000000000000000 ) ;
#57554 = AXIS2_PLACEMENT_3D ( 'NONE', #19603, #39865, #14569 ) ;
#57555 = VERTEX_POINT ( 'NONE', #43594 ) ;
#57556 = CIRCLE ( 'NONE', #41637, 7.499999999999988454 ) ;
#57557 = VERTEX_POINT ( 'NONE', #64852 ) ;
#57558 = CARTESIAN_POINT ( 'NONE',  ( 2.305787727787084407, -6.545285700970554288, 3.971363876083942035 ) ) ;
#57559 = CARTESIAN_POINT ( 'NONE',  ( -27.08485414902839494, -1.622802444812894151, -1.620258667554023368 ) ) ;
#57560 = DIRECTION ( 'NONE',  ( 0.000000000000000000, -1.000000000000000000, 0.000000000000000000 ) ) ;
#57561 = CONICAL_SURFACE ( 'NONE', #46972, 7.938172270156617749, 1.280189991382167047 ) ;
#57562 = CARTESIAN_POINT ( 'NONE',  ( 36.00000000000000711, 7.238157050195626496, -10.49626516989273561 ) ) ;
#57563 = ORIENTED_EDGE ( 'NONE', *, *, #42145, .T. ) ;
#57564 = CIRCLE ( 'NONE', #36272, 7.499999999999988454 ) ;
#57565 = ORIENTED_EDGE ( 'NONE', *, *, #13417, .T. ) ;
#57566 = ORIENTED_EDGE ( 'NONE', *, *, #22959, .T. ) ;
#57567 = CARTESIAN_POINT ( 'NONE',  ( 2.835339799623983748, 7.825540862019418675, 0.3287452556170962770 ) ) ;
#57568 = PRODUCT_DEFINITION ( 'UNKNOWN', '', #41979, #17306 ) ;
#57569 = CARTESIAN_POINT ( 'NONE',  ( -37.00000000000000711, -11.91791701451264629, -2.544412758415973030 ) ) ;
#57570 = EDGE_CURVE ( 'NONE', #45531, #28625, #18995, .T. ) ;
#57571 = ORIENTED_EDGE ( 'NONE', *, *, #35554, .F. ) ;
#57572 = FACE_OUTER_BOUND ( 'NONE', #56421, .T. ) ;
#57573 = CIRCLE ( 'NONE', #48032, 4.999999999999999112 ) ;
#57574 = FACE_OUTER_BOUND ( 'NONE', #12472, .T. ) ;
#57575 = EDGE_CURVE ( 'NONE', #62291, #47988, #28319, .T. ) ;
#57576 = ORIENTED_EDGE ( 'NONE', *, *, #18300, .F. ) ;
#57577 = CARTESIAN_POINT ( 'NONE',  ( 0.2651627923886335503, 11.53745192040748258, -4.105544202112433538 ) ) ;
#57578 = CARTESIAN_POINT ( 'NONE',  ( 35.00000000000000000, -6.657191900728386180, -9.677500615117878624 ) ) ;
#57579 = FACE_OUTER_BOUND ( 'NONE', #27329, .T. ) ;
#57580 = VERTEX_POINT ( 'NONE', #23997 ) ;
#57581 = CARTESIAN_POINT ( 'NONE',  ( 2.000000000000001776, -5.585096664091900642, -4.113602740025990911 ) ) ;
#57582 = ORIENTED_EDGE ( 'NONE', *, *, #58754, .T. ) ;
#57583 = CARTESIAN_POINT ( 'NONE',  ( 0.000000000000000000, -33.00000000000000000, 0.000000000000000000 ) ) ;
#57584 = EDGE_CURVE ( 'NONE', #19021, #37431, #28339, .T. ) ;
#57585 = CONICAL_SURFACE ( 'NONE', #45904, 7.938172270156617749, 1.280189991382167047 ) ;
#57586 = CARTESIAN_POINT ( 'NONE',  ( 1.000000000000000888, 3.224464355699827145, 6.771471746881979392 ) ) ;
#57587 = CARTESIAN_POINT ( 'NONE',  ( 2.000000000000001776, -6.935703035393425253, 0.1051458740707039013 ) ) ;
#57588 = CARTESIAN_POINT ( 'NONE',  ( 2.000000000000001776, -5.457833520448679643, 4.281014542496493824 ) ) ;
#57589 = VECTOR ( 'NONE', #45454, 1000.000000000000000 ) ;
#57591 = CIRCLE ( 'NONE', #246, 5.000000000000000000 ) ;
#57590 = CARTESIAN_POINT ( 'NONE',  ( 2.241526690369556984, -6.602966219605664655, 3.832206765347563326 ) ) ;
#57592 = CARTESIAN_POINT ( 'NONE',  ( 36.00000000000000711, 12.66641127287627810, 1.457575200925408820 ) ) ;
#57593 = FACE_OUTER_BOUND ( 'NONE', #61677, .T. ) ;
#57594 = CARTESIAN_POINT ( 'NONE',  ( 0.3040950598368144520, 1.881452845810376528, 12.11647736519422125 ) ) ;
#57595 = VERTEX_POINT ( 'NONE', #8364 ) ;
#57596 = CARTESIAN_POINT ( 'NONE',  ( 35.00000000000000000, 2.865935305911623487, -12.42372387097883468 ) ) ;
#57597 = EDGE_LOOP ( 'NONE', ( #62789, #25426, #52060, #35810 ) ) ;
#57598 = CARTESIAN_POINT ( 'NONE',  ( 0.3665391374699465965, -1.872534962004882786, 12.13918562134718115 ) ) ;
#57599 = CARTESIAN_POINT ( 'NONE',  ( 37.00000000000000711, 11.29812557209481483, 3.213188559034117819 ) ) ;
#57600 = ADVANCED_FACE ( 'NONE', ( #54596 ), #18696, .F. ) ;
#57601 = EDGE_CURVE ( 'NONE', #51496, #35208, #16844, .T. ) ;
#57602 = VERTEX_POINT ( 'NONE', #3403 ) ;
#57603 = CARTESIAN_POINT ( 'NONE',  ( -17.99474996755618861, 7.056835936932178477, 9.708762815230446819 ) ) ;
#57604 = CARTESIAN_POINT ( 'NONE',  ( -37.00000000000000711, 0.000000000000000000, 0.000000000000000000 ) ) ;
#57605 = DIRECTION ( 'NONE',  ( 0.000000000000000000, 0.5472293298355214164, -0.8369827122275381726 ) ) ;
#57606 = CIRCLE ( 'NONE', #53368, 5.000000000000000000 ) ;
#57607 = EDGE_CURVE ( 'NONE', #53292, #45368, #58294, .T. ) ;
#57608 = ORIENTED_EDGE ( 'NONE', *, *, #49142, .T. ) ;
#57609 = AXIS2_PLACEMENT_3D ( 'NONE', #61361, #41404, #551 ) ;
#57610 = VERTEX_POINT ( 'NONE', #29607 ) ;
#57611 = CARTESIAN_POINT ( 'NONE',  ( 36.00000000000000711, 9.390600770288115129, 8.624332853795948495 ) ) ;
#57612 = CIRCLE ( 'NONE', #24706, 12.75000000000000178 ) ;
#57613 = ORIENTED_EDGE ( 'NONE', *, *, #23596, .F. ) ;
#57614 = CARTESIAN_POINT ( 'NONE',  ( -35.00000000000000000, -11.72397916322012890, 0.7214809346828189307 ) ) ;
#57615 = AXIS2_PLACEMENT_3D ( 'NONE', #38170, #38511, #58831 ) ;
#57616 = DIRECTION ( 'NONE',  ( 0.000000000000000000, 0.000000000000000000, 1.000000000000000000 ) ) ;
#57617 = CYLINDRICAL_SURFACE ( 'NONE', #14947, 5.000000000000000888 ) ;
#57618 = LINE ( 'NONE', #5774, #54092 ) ;
#57619 = DIRECTION ( 'NONE',  ( 0.000000000000000000, -0.01356324068817999114, 0.9999080150203989437 ) ) ;
#57620 = ORIENTED_EDGE ( 'NONE', *, *, #31349, .T. ) ;
#57621 = CARTESIAN_POINT ( 'NONE',  ( -35.00000000000000000, 7.215058775251398160, -9.821084925794490772 ) ) ;
#57622 = EDGE_CURVE ( 'NONE', #49993, #64161, #43268, .T. ) ;
#57623 = ADVANCED_FACE ( 'NONE', ( #64530 ), #38953, .T. ) ;
#57624 = CIRCLE ( 'NONE', #59739, 2.899999999999995470 ) ;
#57625 = CARTESIAN_POINT ( 'NONE',  ( -22.30625920655495165, -3.150098859949341357, 2.110841417170906009 ) ) ;
#57626 = DIRECTION ( 'NONE',  ( 0.000000000000000000, -0.4198891015602528864, -0.9075754196709624466 ) ) ;
#57627 = CARTESIAN_POINT ( 'NONE',  ( 23.18891912316549053, 11.76268964777006509, -6.631469957982857544 ) ) ;
#57628 = DIRECTION ( 'NONE',  ( 0.000000000000000000, -0.8989688749565202253, -0.4380125133593882336 ) ) ;
#57629 = FACE_OUTER_BOUND ( 'NONE', #43695, .T. ) ;
#57630 = CARTESIAN_POINT ( 'NONE',  ( 2.263328370261525446, -5.761609105518017415, 5.019946231381285706 ) ) ;
#57631 = DIRECTION ( 'NONE',  ( 0.000000000000000000, 0.000000000000000000, 1.000000000000000000 ) ) ;
#57632 = CIRCLE ( 'NONE', #28950, 5.000000000000000000 ) ;
#57633 = CIRCLE ( 'NONE', #45946, 12.75000000000000178 ) ;
#57634 = AXIS2_PLACEMENT_3D ( 'NONE', #3093, #48638, #64882 ) ;
#57635 = ORIENTED_EDGE ( 'NONE', *, *, #36603, .F. ) ;
#57636 = CARTESIAN_POINT ( 'NONE',  ( 37.00000000000000711, 5.865551165831078606, -11.32068061209297483 ) ) ;
#57637 = CARTESIAN_POINT ( 'NONE',  ( 35.00000000000000000, 4.705694406421931860E-17, -3.469127814946512892E-15 ) ) ;
#57638 = ORIENTED_EDGE ( 'NONE', *, *, #65406, .T. ) ;
#57639 = CARTESIAN_POINT ( 'NONE',  ( -21.23983773598477498, -7.447593303288433830, 25.00000000000000000 ) ) ;
#57640 = CARTESIAN_POINT ( 'NONE',  ( 1.287602823388407147, -9.277923463524041736, -8.506034117235955705 ) ) ;
#57641 = ORIENTED_EDGE ( 'NONE', *, *, #10807, .T. ) ;
#57642 = DIRECTION ( 'NONE',  ( -1.000000000000000000, -1.836970198721029688E-16, -0.000000000000000000 ) ) ;
#57643 = ORIENTED_EDGE ( 'NONE', *, *, #9168, .F. ) ;
#57644 = AXIS2_PLACEMENT_3D ( 'NONE', #46082, #1175, #55727 ) ;
#57645 = DIRECTION ( 'NONE',  ( -1.000000000000000000, 0.000000000000000000, 0.000000000000000000 ) ) ;
#57646 = EDGE_LOOP ( 'NONE', ( #63685, #11126, #18536, #25199 ) ) ;
#57647 = ORIENTED_EDGE ( 'NONE', *, *, #34019, .T. ) ;
#57648 = AXIS2_PLACEMENT_3D ( 'NONE', #31847, #21578, #20897 ) ;
#57649 = CARTESIAN_POINT ( 'NONE',  ( -27.08421860617808363, -1.817782142550197655, 1.394838596205209225 ) ) ;
#57650 = VERTEX_POINT ( 'NONE', #33308 ) ;
#57651 = DIRECTION ( 'NONE',  ( 0.000000000000000000, -0.7621620551276288014, -0.6473862847818365740 ) ) ;
#57652 = CARTESIAN_POINT ( 'NONE',  ( 5.515188684475870851, 0.005320786921497270942, -0.0005703990286343011730 ) ) ;
#57653 = DIRECTION ( 'NONE',  ( 1.000000000000000000, 0.000000000000000000, -0.000000000000000000 ) ) ;
#57654 = CARTESIAN_POINT ( 'NONE',  ( 9.777179481675013051, 6.950299379875443329, 9.786861771856294467 ) ) ;
#57655 = EDGE_CURVE ( 'NONE', #52589, #29418, #64619, .T. ) ;
#57656 = ORIENTED_EDGE ( 'NONE', *, *, #54950, .F. ) ;
#57657 = CARTESIAN_POINT ( 'NONE',  ( 0.3341166715381265195, -7.691251065848407897, 9.559079491641842452 ) ) ;
#57658 = CIRCLE ( 'NONE', #35360, 5.000000000000000000 ) ;
#57659 = CARTESIAN_POINT ( 'NONE',  ( 8.309432179406254448, -32.38110954670829500, 12.75850010368669629 ) ) ;
#57660 = CARTESIAN_POINT ( 'NONE',  ( 2.781367136452750355, -7.808329083463750209, 0.3081277311327201285 ) ) ;
#57662 = ORIENTED_EDGE ( 'NONE', *, *, #33573, .T. ) ;
#57661 = CARTESIAN_POINT ( 'NONE',  ( 12.49336221634852429, 0.1658369216508866484, -13.50000000000000355 ) ) ;
#57663 = DIRECTION ( 'NONE',  ( 0.000000000000000000, -0.01356324068817991828, 0.9999080150203990547 ) ) ;
#57664 = EDGE_LOOP ( 'NONE', ( #18999, #4791, #45931, #32734 ) ) ;
#57665 = ORIENTED_EDGE ( 'NONE', *, *, #29869, .F. ) ;
#57666 = CARTESIAN_POINT ( 'NONE',  ( 21.44782229496123094, -11.52858179529749094, -3.336984548882474311 ) ) ;
#57667 = DIRECTION ( 'NONE',  ( 0.000000000000000000, 0.07632122047556491595, -0.9970832820307039546 ) ) ;
#57668 = CARTESIAN_POINT ( 'NONE',  ( 0.5572780756280620862, -4.507550621618262809, 11.49107179558539649 ) ) ;
#57669 = ORIENTED_EDGE ( 'NONE', *, *, #29128, .T. ) ;
#57670 = EDGE_CURVE ( 'NONE', #20925, #56892, #53926, .T. ) ;
#57671 = CARTESIAN_POINT ( 'NONE',  ( 0.8320506296491581022, 8.282532257448822932, 9.275353261146570105 ) ) ;
#57672 = CARTESIAN_POINT ( 'NONE',  ( 2.903928887688507210, -8.712847781149033466, -0.9983813550131417358 ) ) ;
#57673 = CARTESIAN_POINT ( 'NONE',  ( 2.241352910868908310, -5.794346703933879184, 4.970878533273742406 ) ) ;
#57674 = ORIENTED_EDGE ( 'NONE', *, *, #61041, .T. ) ;
#57675 = ORIENTED_EDGE ( 'NONE', *, *, #43153, .F. ) ;
#57676 = DIRECTION ( 'NONE',  ( 0.000000000000000000, -1.000000000000000000, 0.000000000000000000 ) ) ;
#57677 = ORIENTED_EDGE ( 'NONE', *, *, #54203, .T. ) ;
#57678 = VECTOR ( 'NONE', #36180, 1000.000000000000000 ) ;
#57679 = ORIENTED_EDGE ( 'NONE', *, *, #56782, .F. ) ;
#57681 = VECTOR ( 'NONE', #48825, 1000.000000000000227 ) ;
#57680 = CARTESIAN_POINT ( 'NONE',  ( 2.000000000000001776, -6.606214214351046721, -2.114938770769991372 ) ) ;
#57682 = DIRECTION ( 'NONE',  ( 0.000000000000000000, 0.01356324068817992175, -0.9999080150203990547 ) ) ;
#57683 = CARTESIAN_POINT ( 'NONE',  ( 2.241506898688420790, -7.187425579579784340, -2.574154135948760302 ) ) ;
#57684 = LINE ( 'NONE', #17440, #35239 ) ;
#57685 = DIRECTION ( 'NONE',  ( -1.000000000000000000, -0.000000000000000000, -0.000000000000000000 ) ) ;
#57686 = DIRECTION ( 'NONE',  ( 0.000000000000000000, 0.01356324068817992175, -0.9999080150203990547 ) ) ;
#57687 = CIRCLE ( 'NONE', #31127, 5.000000000000000888 ) ;
#57688 = CARTESIAN_POINT ( 'NONE',  ( -35.00000000000000000, 10.75351884295727700, -4.725891942574793170 ) ) ;
#57689 =( BOUNDED_CURVE ( )  B_SPLINE_CURVE ( 3, ( #21597, #42169, #11925, #7259 ),
 .UNSPECIFIED., .F., .F. ) 
 B_SPLINE_CURVE_WITH_KNOTS ( ( 4, 4 ),
 ( 1.782871955780958029, 1.816812352449447499 ),
 .UNSPECIFIED. ) 
 CURVE ( )  GEOMETRIC_REPRESENTATION_ITEM ( )  RATIONAL_B_SPLINE_CURVE ( ( 1.000000000000000000, 0.9999040064266120353, 0.9999040064266120353, 1.000000000000000000 ) ) 
 REPRESENTATION_ITEM ( '' )  );
#57690 = EDGE_LOOP ( 'NONE', ( #42924, #779, #48403, #48660 ) ) ;
#57691 = AXIS2_PLACEMENT_3D ( 'NONE', #8360, #63228, #59899 ) ;
#57692 = FACE_OUTER_BOUND ( 'NONE', #22811, .T. ) ;
#57693 = CARTESIAN_POINT ( 'NONE',  ( -22.30527770659433173, -3.125767038151203714, 2.100259071719467130 ) ) ;
#57694 = AXIS2_PLACEMENT_3D ( 'NONE', #27263, #6991, #23258 ) ;
#57695 = ADVANCED_FACE ( 'NONE', ( #49287 ), #14323, .F. ) ;
#57696 = AXIS2_PLACEMENT_3D ( 'NONE', #16505, #26463, #62355 ) ;
#57697 = CARTESIAN_POINT ( 'NONE',  ( -35.00000000000000000, 0.000000000000000000, 0.000000000000000000 ) ) ;
#57698 = DIRECTION ( 'NONE',  ( 1.000000000000000000, -0.000000000000000000, -0.000000000000000000 ) ) ;
#57699 = DIRECTION ( 'NONE',  ( 0.000000000000000000, -0.01356324068817999114, 0.9999080150203989437 ) ) ;
#57700 = CARTESIAN_POINT ( 'NONE',  ( 0.2648978790185593790, 12.08224454301451445, -1.996248716311504801 ) ) ;
#57701 = AXIS2_PLACEMENT_3D ( 'NONE', #9635, #29931, #55870 ) ;
#57702 = DIRECTION ( 'NONE',  ( 0.000000000000000000, -0.5987040770935562195, 0.8009703041134254020 ) ) ;
#57703 = ORIENTED_EDGE ( 'NONE', *, *, #58103, .T. ) ;
#57704 = CARTESIAN_POINT ( 'NONE',  ( 0.000000000000000000, 1.530946385938475762, -7.342084388195351252 ) ) ;
#57705 = CARTESIAN_POINT ( 'NONE',  ( -35.00000000000000000, 0.000000000000000000, 0.000000000000000000 ) ) ;
#57706 = CARTESIAN_POINT ( 'NONE',  ( -24.42101984568203932, -1.824625598916879365, -3.884389025764522163 ) ) ;
#57707 = CARTESIAN_POINT ( 'NONE',  ( 2.556980015514294102, -1.570584617272726913, -7.578583798307318986 ) ) ;
#57708 = EDGE_CURVE ( 'NONE', #33918, #5651, #10409, .T. ) ;
#57709 = AXIS2_PLACEMENT_3D ( 'NONE', #9721, #24053, #29356 ) ;
#57710 = CARTESIAN_POINT ( 'NONE',  ( 2.000000000000001776, -5.814643797626899868, -3.550179297009637747 ) ) ;
#57711 = CARTESIAN_POINT ( 'NONE',  ( -25.66889450307327891, -8.265805117747651920, 10.67728274434794500 ) ) ;
#57712 = ORIENTED_EDGE ( 'NONE', *, *, #41357, .F. ) ;
#57713 = LINE ( 'NONE', #37404, #446 ) ;
#57714 = CARTESIAN_POINT ( 'NONE',  ( 37.00000000000000711, -45.00200000000000244, -4.500000000000000888 ) ) ;
#57715 = CARTESIAN_POINT ( 'NONE',  ( 35.00000000000000000, 10.91072401419418014, 5.428340790341585453 ) ) ;
#57716 = CARTESIAN_POINT ( 'NONE',  ( 0.8320506296491604337, -12.30686996250299714, -1.781423711749702044 ) ) ;
#57717 = VERTEX_POINT ( 'NONE', #364 ) ;
#57718 = DIRECTION ( 'NONE',  ( 0.000000000000000000, -0.01356324068817999114, 0.9999080150203989437 ) ) ;
#57719 = DIRECTION ( 'NONE',  ( -1.000000000000000000, 0.000000000000000000, 0.000000000000000000 ) ) ;
#57720 = CIRCLE ( 'NONE', #31176, 5.000000000000000000 ) ;
#57721 = AXIS2_PLACEMENT_3D ( 'NONE', #25421, #10445, #20441 ) ;
#57723 = VERTEX_POINT ( 'NONE', #49916 ) ;
#57722 = DIRECTION ( 'NONE',  ( 0.000000000000000000, -0.4380125133593849029, 0.8989688749565220016 ) ) ;
#57724 = DIRECTION ( 'NONE',  ( -0.000000000000000000, -0.000000000000000000, -1.000000000000000000 ) ) ;
#57725 = AXIS2_PLACEMENT_3D ( 'NONE', #58620, #43611, #13040 ) ;
#57726 = AXIS2_PLACEMENT_3D ( 'NONE', #64402, #33172, #17890 ) ;
#57727 = EDGE_CURVE ( 'NONE', #8982, #40981, #41928, .T. ) ;
#57728 = CARTESIAN_POINT ( 'NONE',  ( -35.00000000000000000, 3.640372113593719927, -12.21925492305358318 ) ) ;
#57729 = ORIENTED_EDGE ( 'NONE', *, *, #13889, .F. ) ;
#57730 = CARTESIAN_POINT ( 'NONE',  ( 0.2833330754217384118, -9.514385791198149533, 7.719627479384628899 ) ) ;
#57731 = CARTESIAN_POINT ( 'NONE',  ( 5.515188684475870851, 0.005140903460551137644, -0.001485678338381731097 ) ) ;
#57732 = DIRECTION ( 'NONE',  ( 1.000000000000000000, -0.000000000000000000, 0.000000000000000000 ) ) ;
#57733 = LINE ( 'NONE', #12154, #23435 ) ;
#57734 = EDGE_CURVE ( 'NONE', #33841, #1348, #14964, .T. ) ;
#57735 = CARTESIAN_POINT ( 'NONE',  ( -37.00000000000000711, -4.603882218679629545, 10.80631716521665453 ) ) ;
#57736 = EDGE_CURVE ( 'NONE', #54896, #33819, #59329, .T. ) ;
#57737 = CIRCLE ( 'NONE', #11014, 7.499999999999988454 ) ;
#57738 = CARTESIAN_POINT ( 'NONE',  ( 0.9232167919969146430, 11.84868134597557265, 3.872606616958310877 ) ) ;
#57740 = ORIENTED_EDGE ( 'NONE', *, *, #9171, .F. ) ;
#57739 = CARTESIAN_POINT ( 'NONE',  ( 1.547277799337862136, 0.6737945300320472564, 12.65564732076243182 ) ) ;
#57741 = EDGE_CURVE ( 'NONE', #39147, #50042, #62496, .T. ) ;
#57742 = CARTESIAN_POINT ( 'NONE',  ( -36.00000000000000711, 3.805206332242643263, -12.16893194857546412 ) ) ;
#57743 = ORIENTED_EDGE ( 'NONE', *, *, #172, .F. ) ;
#57744 = AXIS2_PLACEMENT_3D ( 'NONE', #54176, #3668, #23932 ) ;
#57745 = ORIENTED_EDGE ( 'NONE', *, *, #27332, .F. ) ;
#57746 = PRODUCT_CONTEXT ( 'NONE', #9387, 'mechanical' ) ;
#57747 = CARTESIAN_POINT ( 'NONE',  ( 1.719304012339844867, -11.67935079956417610, 5.066286238786176455 ) ) ;
#57748 = CARTESIAN_POINT ( 'NONE',  ( -3.978895040306493769, 10.13474746098345491, 6.440914979617118341 ) ) ;
#57749 = EDGE_CURVE ( 'NONE', #43541, #25095, #24674, .T. ) ;
#57750 = CARTESIAN_POINT ( 'NONE',  ( -43.07244751019905493, -1.315220855092201324, -15.87097690372580061 ) ) ;
#57751 = CARTESIAN_POINT ( 'NONE',  ( 35.00000000000000000, 12.09831040184923978, -1.463443770872822736 ) ) ;
#57752 = VERTEX_POINT ( 'NONE', #35254 ) ;
#57753 = AXIS2_PLACEMENT_3D ( 'NONE', #45686, #14434, #145 ) ;
#57754 = CARTESIAN_POINT ( 'NONE',  ( 5.514970785353741078, -0.002796696073589764915, 0.003805873180274771655 ) ) ;
#57756 = ADVANCED_FACE ( 'NONE', ( #689 ), #20643, .T. ) ;
#57755 = CARTESIAN_POINT ( 'NONE',  ( 1.547277799337861692, -3.695326562729266850, 12.12286970032301880 ) ) ;
#57757 = ORIENTED_EDGE ( 'NONE', *, *, #9007, .T. ) ;
#57758 = CIRCLE ( 'NONE', #65186, 5.000000000000000000 ) ;
#57759 = VERTEX_POINT ( 'NONE', #30284 ) ;
#57760 = ORIENTED_EDGE ( 'NONE', *, *, #62906, .F. ) ;
#57761 = CARTESIAN_POINT ( 'NONE',  ( 11.74548640120467979, -10.73597826697111124, -8.184666801472349817 ) ) ;
#57762 = DIRECTION ( 'NONE',  ( -1.000000000000000000, 0.000000000000000000, 0.000000000000000000 ) ) ;
#57763 = CARTESIAN_POINT ( 'NONE',  ( 36.00000000000000711, 11.80185301892980654, -4.824807283154167514 ) ) ;
#57764 = CARTESIAN_POINT ( 'NONE',  ( 0.3675815128205894289, 12.13672785388550324, 1.872154644482125763 ) ) ;
#57765 = CARTESIAN_POINT ( 'NONE',  ( 35.00000000000000000, -3.473736367725341001, -12.26766708251990323 ) ) ;
#57766 = CARTESIAN_POINT ( 'NONE',  ( -27.19357181888462094, -10.84410562793472543, 5.138615876886901468 ) ) ;
#57767 = AXIS2_PLACEMENT_3D ( 'NONE', #50544, #15594, #9967 ) ;
#57768 = EDGE_CURVE ( 'NONE', #49400, #18739, #30643, .T. ) ;
#57769 = DIRECTION ( 'NONE',  ( 1.000000000000000000, 0.000000000000000000, 0.000000000000000000 ) ) ;
#57770 = ORIENTED_EDGE ( 'NONE', *, *, #1480, .F. ) ;
#57771 = CARTESIAN_POINT ( 'NONE',  ( 35.00000000000000000, 4.705694406421931860E-17, -3.469127814946512892E-15 ) ) ;
#57772 = ORIENTED_EDGE ( 'NONE', *, *, #33348, .T. ) ;
#57773 = CARTESIAN_POINT ( 'NONE',  ( 36.00000000000000711, 6.018036132182164266, -11.24036214326523009 ) ) ;
#57774 = CARTESIAN_POINT ( 'NONE',  ( -9.343255928485906026, -12.02898473248699496, -6.138655790224737174 ) ) ;
#57775 = VECTOR ( 'NONE', #21285, 1000.000000000000000 ) ;
#57776 = CARTESIAN_POINT ( 'NONE',  ( 2.245754705088395475, -3.913944702466310765, 6.556487589645220382 ) ) ;
#57777 = AXIS2_PLACEMENT_3D ( 'NONE', #53159, #1965, #17262 ) ;
#57778 = FACE_OUTER_BOUND ( 'NONE', #12657, .T. ) ;
#57779 = VERTEX_POINT ( 'NONE', #4368 ) ;
#57780 = ORIENTED_EDGE ( 'NONE', *, *, #4708, .F. ) ;
#57781 = CARTESIAN_POINT ( 'NONE',  ( 5.514970785353741078, -0.004588761610585017671, 0.001117786416802601067 ) ) ;
#57782 = CIRCLE ( 'NONE', #37592, 12.18649999999999700 ) ;
#57783 = ORIENTED_EDGE ( 'NONE', *, *, #39920, .T. ) ;
#57784 = FACE_OUTER_BOUND ( 'NONE', #52089, .T. ) ;
#57785 = DIRECTION ( 'NONE',  ( 1.000000000000000000, -0.000000000000000000, 0.000000000000000000 ) ) ;
#57786 = CARTESIAN_POINT ( 'NONE',  ( 2.000000000000001776, 5.888698556700818543, -3.665823448873358981 ) ) ;
#57787 = DIRECTION ( 'NONE',  ( 0.000000000000000000, 0.01356324068817998940, -0.9999080150203990547 ) ) ;
#57788 = ORIENTED_EDGE ( 'NONE', *, *, #4625, .T. ) ;
#57789 = AXIS2_PLACEMENT_3D ( 'NONE', #61047, #57045, #10819 ) ;
#57790 = CARTESIAN_POINT ( 'NONE',  ( 0.3109076770649027432, 12.11383728282219430, 1.896437056876507876 ) ) ;
#57791 = DIRECTION ( 'NONE',  ( -1.000000000000000000, -0.000000000000000000, -0.000000000000000000 ) ) ;
#57792 = CYLINDRICAL_SURFACE ( 'NONE', #1448, 12.18649999999999878 ) ;
#57793 = CARTESIAN_POINT ( 'NONE',  ( 35.00000000000000000, 6.475373545682446164, 10.32377448871660519 ) ) ;
#57794 = AXIS2_PLACEMENT_3D ( 'NONE', #17457, #56732, #16479 ) ;
#57795 = EDGE_CURVE ( 'NONE', #41918, #64690, #26383, .T. ) ;
#57796 = FACE_OUTER_BOUND ( 'NONE', #42633, .T. ) ;
#57797 = CARTESIAN_POINT ( 'NONE',  ( 2.000000000000001776, 0.000000000000000000, 0.000000000000000000 ) ) ;
#57798 = ORIENTED_EDGE ( 'NONE', *, *, #27535, .T. ) ;
#57799 = LINE ( 'NONE', #7561, #40254 ) ;
#57800 = EDGE_LOOP ( 'NONE', ( #13943, #36972, #37549, #35618 ) ) ;
#57801 = CARTESIAN_POINT ( 'NONE',  ( -6.514004847085159255, -1.134796399304650372, -13.45231326553087747 ) ) ;
#57802 = CARTESIAN_POINT ( 'NONE',  ( 1.462291587749818600, -8.602888600421563225, 9.267729738232196368 ) ) ;
#57803 = DIRECTION ( 'NONE',  ( 1.000000000000000000, -0.000000000000000000, 0.000000000000000000 ) ) ;
#57804 = DIRECTION ( 'NONE',  ( 0.3509218304786018705, 0.9364047569793457759, 0.000000000000000000 ) ) ;
#57805 = B_SPLINE_CURVE_WITH_KNOTS ( 'NONE', 3,
 ( #59127, #8557, #49479, #28844, #13854, #14195, #28509, #54463, #39464, #45123 ),
 .UNSPECIFIED., .F., .F.,
 ( 4, 3, 3, 4 ),
 ( 5.401523115762189690E-05, 0.0008136511341527787088, 0.004068255670953088883, 0.005063778443040924809 ),
 .UNSPECIFIED. ) ;
#57806 = DIRECTION ( 'NONE',  ( 0.000000000000000000, 0.01356324068817998940, -0.9999080150203990547 ) ) ;
#57807 = AXIS2_PLACEMENT_3D ( 'NONE', #31002, #11371, #57605 ) ;
#57808 = EDGE_CURVE ( 'NONE', #46784, #62148, #49322, .T. ) ;
#57809 = VERTEX_POINT ( 'NONE', #46889 ) ;
#57810 = ORIENTED_EDGE ( 'NONE', *, *, #39569, .F. ) ;
#57811 = CARTESIAN_POINT ( 'NONE',  ( 0.2676618633000465430, 1.968216791520492892, 12.08777609394270414 ) ) ;
#57812 = ORIENTED_EDGE ( 'NONE', *, *, #29268, .T. ) ;
#57813 = CARTESIAN_POINT ( 'NONE',  ( 2.706962116719304312, 3.188935572973642607, 11.57463990576596302 ) ) ;
#57814 = DIRECTION ( 'NONE',  ( 1.000000000000000000, -0.000000000000000000, 0.000000000000000000 ) ) ;
#57815 = CYLINDRICAL_SURFACE ( 'NONE', #44781, 4.999999999999999112 ) ;
#57816 = DIRECTION ( 'NONE',  ( -1.000000000000000000, 0.000000000000000000, 0.000000000000000000 ) ) ;
#57817 = DIRECTION ( 'NONE',  ( 0.000000000000000000, 0.01356324068817991828, -0.9999080150203990547 ) ) ;
#57818 = EDGE_CURVE ( 'NONE', #25796, #17080, #20032, .T. ) ;
#57819 = CARTESIAN_POINT ( 'NONE',  ( 2.244591118396556784, -1.219892024449305223, 7.537402265771622645 ) ) ;
#57820 = CYLINDRICAL_SURFACE ( 'NONE', #36103, 13.50000000000000178 ) ;
#57821 = ORIENTED_EDGE ( 'NONE', *, *, #3467, .T. ) ;
#57822 = ADVANCED_FACE ( 'NONE', ( #1349 ), #22258, .T. ) ;
#57823 = VERTEX_POINT ( 'NONE', #32546 ) ;
#57824 = VECTOR ( 'NONE', #40425, 1000.000000000000000 ) ;
#57825 = CARTESIAN_POINT ( 'NONE',  ( -35.00000000000000000, -12.09831040184925044, 1.463443770872731919 ) ) ;
#57826 = EDGE_LOOP ( 'NONE', ( #30480, #38926, #47811, #2677 ) ) ;
#57827 = CARTESIAN_POINT ( 'NONE',  ( 0.000000000000000000, 5.888698556700773246, 3.665823448873418045 ) ) ;
#57828 = CARTESIAN_POINT ( 'NONE',  ( 5.520433897694421610, 0.01491416502703863355, 0.002108682515300534625 ) ) ;
#57829 = EDGE_CURVE ( 'NONE', #53403, #31959, #31271, .T. ) ;
#57830 = DIRECTION ( 'NONE',  ( 0.000000000000000000, -0.01356324068817999114, 0.9999080150203989437 ) ) ;
#57831 = EDGE_LOOP ( 'NONE', ( #43936, #26378, #64546, #53709 ) ) ;
#57832 = CARTESIAN_POINT ( 'NONE',  ( -37.00000000000000711, -11.66953048682402283, 3.511814412392074480 ) ) ;
#57833 = CARTESIAN_POINT ( 'NONE',  ( -13.91099446267240225, -33.59051099066058299, -9.908177736481542652 ) ) ;
#57835 = EDGE_CURVE ( 'NONE', #19802, #14030, #12609, .T. ) ;
#57834 = CARTESIAN_POINT ( 'NONE',  ( 2.280717697724244264, -5.034569468898799194, -5.756537207046680926 ) ) ;
#57836 = ORIENTED_EDGE ( 'NONE', *, *, #61916, .F. ) ;
#57837 = VERTEX_POINT ( 'NONE', #17625 ) ;
#57838 = CARTESIAN_POINT ( 'NONE',  ( 0.3665391374699472626, -2.392238720110378303, -12.04754782681759728 ) ) ;
#57839 = VERTEX_POINT ( 'NONE', #11628 ) ;
#57840 = ORIENTED_EDGE ( 'NONE', *, *, #48669, .F. ) ;
#57841 = CARTESIAN_POINT ( 'NONE',  ( 2.256373768223413290, 3.934258165100065874, 6.548448293197146164 ) ) ;
#57842 = AXIS2_PLACEMENT_3D ( 'NONE', #50656, #29374, #49667 ) ;
#57843 = ORIENTED_EDGE ( 'NONE', *, *, #56450, .T. ) ;
#57844 = B_SPLINE_CURVE_WITH_KNOTS ( 'NONE', 3,
 ( #43187, #22598, #58170, #42864, #13575, #33863, #63460, #12275, #32539, #23244, #48221, #37881, #6975, #48531, #7971, #52850, #42514, #2323, #2982, #43505, #17618, #12591 ),
 .UNSPECIFIED., .F., .F.,
 ( 4, 3, 3, 3, 3, 3, 3, 4 ),
 ( 8.690541527449942710E-19, 4.449119708436876107E-05, 6.626296329540655992E-05, 8.803456484962991020E-05, 0.0001098060367612845804, 0.0001315774408628562759, 0.0001760698110411223073, 0.0001829697163287816132 ),
 .UNSPECIFIED. ) ;
#57846 = EDGE_CURVE ( 'NONE', #53953, #14946, #26935, .T. ) ;
#57845 = VERTEX_POINT ( 'NONE', #31898 ) ;
#57847 = CARTESIAN_POINT ( 'NONE',  ( -22.27722015946438816, -2.828901469906474286, 2.356370737780152158 ) ) ;
#57848 = AXIS2_PLACEMENT_3D ( 'NONE', #58377, #16816, #37093 ) ;
#57849 = FACE_OUTER_BOUND ( 'NONE', #29922, .T. ) ;
#57850 = DIRECTION ( 'NONE',  ( 1.000000000000000000, 0.000000000000000000, 0.000000000000000000 ) ) ;
#57851 = FACE_OUTER_BOUND ( 'NONE', #8221, .T. ) ;
#57852 = CYLINDRICAL_SURFACE ( 'NONE', #1590, 4.999999999999999112 ) ;
#57853 = ADVANCED_FACE ( 'NONE', ( #47235 ), #52858, .T. ) ;
#57854 = CARTESIAN_POINT ( 'NONE',  ( 17.27839441901508977, 12.20388373500084711, 5.771933972472493402 ) ) ;
#57855 = ORIENTED_EDGE ( 'NONE', *, *, #64914, .T. ) ;
#57856 = CARTESIAN_POINT ( 'NONE',  ( -35.00000000000000000, -10.80478261802186246, 5.636262487437281976 ) ) ;
#57857 = CYLINDRICAL_SURFACE ( 'NONE', #51170, 2.899999999999994582 ) ;
#57858 = EDGE_CURVE ( 'NONE', #50610, #25109, #21106, .T. ) ;
#57859 = LINE ( 'NONE', #12932, #36331 ) ;
#57860 = CARTESIAN_POINT ( 'NONE',  ( -10.00000000000000178, 0.000000000000000000, 0.000000000000000000 ) ) ;
#57861 = CARTESIAN_POINT ( 'NONE',  ( -35.00000000000000000, 0.000000000000000000, 0.000000000000000000 ) ) ;
#57862 = CARTESIAN_POINT ( 'NONE',  ( 35.00000000000000000, -5.814360711498364864, -10.70999494708490829 ) ) ;
#57863 = ORIENTED_EDGE ( 'NONE', *, *, #45933, .F. ) ;
#57864 = CARTESIAN_POINT ( 'NONE',  ( -14.65220012252043880, 8.414276895534435141, -8.555797441148357052 ) ) ;
#57865 = ORIENTED_EDGE ( 'NONE', *, *, #14678, .F. ) ;
#57866 = FACE_OUTER_BOUND ( 'NONE', #35504, .T. ) ;
#57867 = CARTESIAN_POINT ( 'NONE',  ( 2.261269890822071194, 5.942064862945676040, -4.803890999604265133 ) ) ;
#57868 = DIRECTION ( 'NONE',  ( 0.000000000000000000, 0.000000000000000000, 1.000000000000000000 ) ) ;
#57869 = CYLINDRICAL_SURFACE ( 'NONE', #16040, 12.18650000000000055 ) ;
#57870 = CARTESIAN_POINT ( 'NONE',  ( 2.717984159218819862, 7.719081760283970084, 1.073093837952745933 ) ) ;
#57871 = EDGE_LOOP ( 'NONE', ( #35717, #11016, #47044, #51635 ) ) ;
#57872 = PRESENTATION_LAYER_ASSIGNMENT (  '', '', ( #46184 ) ) ;
#57873 = CARTESIAN_POINT ( 'NONE',  ( 37.00000000000000711, -7.499679039483992504, 9.040300684349768190 ) ) ;
#57874 = CARTESIAN_POINT ( 'NONE',  ( -35.00000000000000000, 9.752226076388895493, 6.547236723514054724 ) ) ;
#57875 = CARTESIAN_POINT ( 'NONE',  ( 35.00000000000000000, -5.015831474386232891, 10.62137734850272786 ) ) ;
#57876 = CARTESIAN_POINT ( 'NONE',  ( -3.964071950788559562, 10.45352654835910045, 8.551872867741371564 ) ) ;
#57877 = ADVANCED_FACE ( 'NONE', ( #62486 ), #53416, .F. ) ;
#57878 = EDGE_CURVE ( 'NONE', #27429, #1460, #52553, .T. ) ;
#57879 = CARTESIAN_POINT ( 'NONE',  ( 37.00000000000000711, 9.733281772932162568, -8.235637554476683775 ) ) ;
#57880 = CIRCLE ( 'NONE', #37685, 12.74999999999999822 ) ;
#57881 = EDGE_LOOP ( 'NONE', ( #47178, #26956 ) ) ;
#57882 = PRODUCT_DEFINITION_CONTEXT ( 'detailed design', #61259, 'design' ) ;
#57883 = LINE ( 'NONE', #47559, #14749 ) ;
#57884 = DIRECTION ( 'NONE',  ( 1.000000000000000000, 0.000000000000000000, 0.000000000000000000 ) ) ;
#57886 = AXIS2_PLACEMENT_3D ( 'NONE', #64512, #44552, #64832 ) ;
#57885 = APPLICATION_CONTEXT ( 'automotive_design' ) ;
#57887 = EDGE_CURVE ( 'NONE', #58982, #44487, #14412, .T. ) ;
#57888 = AXIS2_PLACEMENT_3D ( 'NONE', #50697, #41346, #41026 ) ;
#57889 = ADVANCED_FACE ( 'NONE', ( #57866 ), #64450, .F. ) ;
#57890 = ORIENTED_EDGE ( 'NONE', *, *, #47413, .F. ) ;
#57891 = ORIENTED_EDGE ( 'NONE', *, *, #54244, .F. ) ;
#57892 = CARTESIAN_POINT ( 'NONE',  ( 12.47628546223243617, 0.000000000000000000, 13.50000000000000178 ) ) ;
#57894 = CARTESIAN_POINT ( 'NONE',  ( 0.2651627682582926582, 2.213224986694582341, 12.04449770099951422 ) ) ;
#57893 =( BOUNDED_CURVE ( )  B_SPLINE_CURVE ( 3, ( #6850, #3095, #53952, #58963 ),
 .UNSPECIFIED., .F., .F. ) 
 B_SPLINE_CURVE_WITH_KNOTS ( ( 4, 4 ),
 ( 1.796926956229685013, 1.827009492773266297 ),
 .UNSPECIFIED. ) 
 CURVE ( )  GEOMETRIC_REPRESENTATION_ITEM ( )  RATIONAL_B_SPLINE_CURVE ( ( 1.000000000000000000, 0.9999245881713708650, 0.9999245881713708650, 1.000000000000000000 ) ) 
 REPRESENTATION_ITEM ( '' )  );
#57895 = CARTESIAN_POINT ( 'NONE',  ( -27.08429572838383947, -1.608131779585707299, -1.632445743623455847 ) ) ;
#57896 = CARTESIAN_POINT ( 'NONE',  ( 1.194176325881349587, -7.670099510969132339, 9.940715479868426740 ) ) ;
#57897 = CARTESIAN_POINT ( 'NONE',  ( -22.30986928587821438, -2.105440358094953002, -3.138878161034341474 ) ) ;
#57898 = VERTEX_POINT ( 'NONE', #3961 ) ;
#57899 = EDGE_CURVE ( 'NONE', #18117, #13538, #54168, .T. ) ;
#57900 = VERTEX_POINT ( 'NONE', #18280 ) ;
#57901 = ORIENTED_EDGE ( 'NONE', *, *, #34736, .T. ) ;
#57902 = CARTESIAN_POINT ( 'NONE',  ( 2.573738926104377267, 7.741646296020607387, 0.2352053552897726552 ) ) ;
#57903 = VECTOR ( 'NONE', #20718, 1000.000000000000000 ) ;
#57904 = DIRECTION ( 'NONE',  ( -0.000000000000000000, -0.000000000000000000, -1.000000000000000000 ) ) ;
#57905 = VERTEX_POINT ( 'NONE', #59169 ) ;
#57906 = DIRECTION ( 'NONE',  ( 0.000000000000000000, -0.01356324068817999114, 0.9999080150203989437 ) ) ;
#57907 = DIRECTION ( 'NONE',  ( 0.000000000000000000, -1.000000000000000000, 0.000000000000000000 ) ) ;
#57908 = ORIENTED_EDGE ( 'NONE', *, *, #29370, .F. ) ;
#57909 = CARTESIAN_POINT ( 'NONE',  ( -27.08421860617808363, -0.2990745872176354681, -2.271664812096785280 ) ) ;
#57910 = CARTESIAN_POINT ( 'NONE',  ( 2.276905613633651182, -2.759436818562446270, -7.130967020394719746 ) ) ;
#57911 = CARTESIAN_POINT ( 'NONE',  ( 2.249013661412873510, 7.134443398813564485, 2.724484898588741100 ) ) ;
#57912 = ORIENTED_EDGE ( 'NONE', *, *, #36858, .F. ) ;
#57913 = ORIENTED_EDGE ( 'NONE', *, *, #8650, .T. ) ;
#57914 = CARTESIAN_POINT ( 'NONE',  ( 0.2869720083484405548, 12.10169797402142677, -1.922200714744033645 ) ) ;
#57915 = VERTEX_POINT ( 'NONE', #13583 ) ;
#57916 = CARTESIAN_POINT ( 'NONE',  ( 3.152665057734120868, 6.378477742800529704, -4.725420687650643714 ) ) ;
#57917 = EDGE_CURVE ( 'NONE', #36458, #38941, #38047, .T. ) ;
#57918 = CARTESIAN_POINT ( 'NONE',  ( 37.00000000000000711, 4.705694406421931860E-17, -3.469127814946512892E-15 ) ) ;
#57919 = DIRECTION ( 'NONE',  ( 1.000000000000000000, 0.000000000000000000, -0.000000000000000000 ) ) ;
#57920 = CARTESIAN_POINT ( 'NONE',  ( 2.241509619876137727, -6.630717740088877932, 3.784042210004685103 ) ) ;
#57921 = DIRECTION ( 'NONE',  ( 1.000000000000000000, -0.000000000000000000, 0.000000000000000000 ) ) ;
#57922 = DIRECTION ( 'NONE',  ( 1.000000000000000000, 0.000000000000000000, 0.000000000000000000 ) ) ;
#57923 = DIRECTION ( 'NONE',  ( 0.000000000000000000, 0.8827602140260297769, -0.4698238015817396418 ) ) ;
#57924 = VERTEX_POINT ( 'NONE', #59479 ) ;
#57925 = ADVANCED_FACE ( 'NONE', ( #39185 ), #3660, .T. ) ;
#57926 = CYLINDRICAL_SURFACE ( 'NONE', #18460, 12.00000000000000000 ) ;
#57927 = CIRCLE ( 'NONE', #56885, 12.18649999999999878 ) ;
#57928 = ORIENTED_EDGE ( 'NONE', *, *, #19881, .F. ) ;
#57929 = CYLINDRICAL_SURFACE ( 'NONE', #46583, 4.999999999999999112 ) ;
#57930 = CARTESIAN_POINT ( 'NONE',  ( 2.247112776669942580, 6.670755883243522533, 3.716786765235448708 ) ) ;
#57931 = EDGE_CURVE ( 'NONE', #41192, #44052, #13595, .T. ) ;
#57932 = ORIENTED_EDGE ( 'NONE', *, *, #2965, .T. ) ;
#57933 = CARTESIAN_POINT ( 'NONE',  ( 2.556980015514017435, 7.348538402679566595, 2.429125721802398719 ) ) ;
#57934 = CARTESIAN_POINT ( 'NONE',  ( 0.000000000000000000, -0.08317740279936355896, 7.499538753794337431 ) ) ;
#57935 = CARTESIAN_POINT ( 'NONE',  ( 2.305787727787084407, -7.508843116234166004, 1.493241775258399073 ) ) ;
#57936 = CIRCLE ( 'NONE', #590, 12.74999999999999822 ) ;
#57937 = ORIENTED_EDGE ( 'NONE', *, *, #15696, .T. ) ;
#57938 = VERTEX_POINT ( 'NONE', #22942 ) ;
#57939 = CARTESIAN_POINT ( 'NONE',  ( -35.00000000000000000, 8.927548052241016663, -8.295159312811756891 ) ) ;
#57940 = EDGE_LOOP ( 'NONE', ( #32591, #32204, #41491, #2012 ) ) ;
#57941 = CARTESIAN_POINT ( 'NONE',  ( -35.00000000000000000, 10.63508530065528923, -4.986700593229593359 ) ) ;
#57942 = CARTESIAN_POINT ( 'NONE',  ( -47.00000000000000711, 0.000000000000000000, 0.000000000000000000 ) ) ;
#57943 = DIRECTION ( 'NONE',  ( 0.000000000000000000, 0.3807014730195152907, -0.9246979985058750851 ) ) ;
#57944 = CYLINDRICAL_SURFACE ( 'NONE', #62878, 6.936499999999988120 ) ;
#57945 = ORIENTED_EDGE ( 'NONE', *, *, #61213, .T. ) ;
#57946 = CARTESIAN_POINT ( 'NONE',  ( -22.27706485742869091, -3.358064672837095976, -1.508175983031630585 ) ) ;
#57947 = VECTOR ( 'NONE', #59171, 1000.000000000000000 ) ;
#57948 = EDGE_CURVE ( 'NONE', #57258, #49577, #46566, .T. ) ;
#57949 = EDGE_CURVE ( 'NONE', #8885, #62664, #31839, .T. ) ;
#57950 = CARTESIAN_POINT ( 'NONE',  ( -22.30625920655495165, -2.110841417170890466, -3.150098859949351571 ) ) ;
#57951 = LINE ( 'NONE', #31989, #13928 ) ;
#57952 = LINE ( 'NONE', #17381, #22437 ) ;
#57953 = CARTESIAN_POINT ( 'NONE',  ( 2.000000000000001776, -6.470132594555779271, -2.133363481234176628 ) ) ;
#57954 = B_SPLINE_CURVE_WITH_KNOTS ( 'NONE', 3,
 ( #50155, #58851, #23577, #24211, #33549, #18610, #3648 ),
 .UNSPECIFIED., .F., .F.,
 ( 4, 3, 4 ),
 ( 2.764715539838036307E-18, 6.607593386745461920E-05, 0.0001321430428584417424 ),
 .UNSPECIFIED. ) ;
#57955 = CARTESIAN_POINT ( 'NONE',  ( 5.514970785353741078, -0.003805873180274799410, -0.002796696073589726318 ) ) ;
#57956 = CARTESIAN_POINT ( 'NONE',  ( 2.244591118396555895, -5.779440292195805462, 4.989853642775300635 ) ) ;
#57957 = CARTESIAN_POINT ( 'NONE',  ( -22.29570301036918423, -2.696988360630593995, -2.586939527522312599 ) ) ;
#57958 = EDGE_CURVE ( 'NONE', #51664, #63220, #57212, .T. ) ;
#57959 = ORIENTED_EDGE ( 'NONE', *, *, #28234, .F. ) ;
#57960 = CARTESIAN_POINT ( 'NONE',  ( 2.242819959140646358, -0.1024002568249904599, 7.634209046698944512 ) ) ;
#57961 = CARTESIAN_POINT ( 'NONE',  ( 0.2706063244538045032, -12.24670371972917948, -0.1752385892653291755 ) ) ;
#57962 = AXIS2_PLACEMENT_3D ( 'NONE', #4287, #65436, #8950 ) ;
#57963 = ORIENTED_EDGE ( 'NONE', *, *, #21774, .T. ) ;
#57964 = CARTESIAN_POINT ( 'NONE',  ( -22.28121537037576871, 3.680034389105501624, -0.3168735205819583900 ) ) ;
#57965 = CARTESIAN_POINT ( 'NONE',  ( 36.00000000000000711, 12.57916205664484188, 2.080187960898426169 ) ) ;
#57966 = VERTEX_POINT ( 'NONE', #53187 ) ;
#57967 = CARTESIAN_POINT ( 'NONE',  ( 2.241526690369557429, 4.894066724724331685, -5.859443871526991643 ) ) ;
#57968 = ORIENTED_EDGE ( 'NONE', *, *, #42884, .T. ) ;
#57969 = EDGE_CURVE ( 'NONE', #62996, #41515, #45501, .T. ) ;
#57970 = PLANE ( 'NONE',  #13675 ) ;
#57971 = VERTEX_POINT ( 'NONE', #34197 ) ;
#57972 = EDGE_LOOP ( 'NONE', ( #56586, #65626, #58138, #20025 ) ) ;
#57973 = EDGE_CURVE ( 'NONE', #60414, #19006, #17939, .T. ) ;
#57974 = AXIS2_PLACEMENT_3D ( 'NONE', #46054, #40722, #26096 ) ;
#57975 = CARTESIAN_POINT ( 'NONE',  ( 2.263328370261528111, -7.131064289852361071, 2.746620058315270896 ) ) ;
#57976 = VERTEX_POINT ( 'NONE', #23250 ) ;
#57977 = CARTESIAN_POINT ( 'NONE',  ( -47.00000000000000711, 0.000000000000000000, 0.000000000000000000 ) ) ;
#57978 = CARTESIAN_POINT ( 'NONE',  ( 3.864517994186338790, 5.325084099531887993, 12.40733688370094256 ) ) ;
#57979 = CARTESIAN_POINT ( 'NONE',  ( 35.00000000000000000, -10.12742074351890764, 7.745827850123116143 ) ) ;
#57980 = CARTESIAN_POINT ( 'NONE',  ( 2.000000000000001776, 0.000000000000000000, 0.000000000000000000 ) ) ;
#57981 = ORIENTED_EDGE ( 'NONE', *, *, #323, .F. ) ;
#57982 = DIRECTION ( 'NONE',  ( -1.000000000000000000, 0.000000000000000000, 0.000000000000000000 ) ) ;
#57983 = CARTESIAN_POINT ( 'NONE',  ( -4.254071763051084254, -31.39562805149797597, 14.04524613008041811 ) ) ;
#57984 = DIRECTION ( 'NONE',  ( 0.000000000000000000, -0.4134677391718385997, -0.9105187689796011563 ) ) ;
#57986 = ORIENTED_EDGE ( 'NONE', *, *, #24742, .F. ) ;
#57985 = CARTESIAN_POINT ( 'NONE',  ( -24.54625327245882360, 6.852894237372495034, 9.860103603378655990 ) ) ;
#57987 = CARTESIAN_POINT ( 'NONE',  ( 1.452237505248552996, -12.08199618361515526, 3.767214359061084927 ) ) ;
#57988 = ORIENTED_EDGE ( 'NONE', *, *, #28770, .T. ) ;
#57989 = CYLINDRICAL_SURFACE ( 'NONE', #62473, 5.000000000000000888 ) ;
#57990 = VERTEX_POINT ( 'NONE', #29226 ) ;
#57991 = FACE_OUTER_BOUND ( 'NONE', #444, .T. ) ;
#57992 = CARTESIAN_POINT ( 'NONE',  ( 2.241451721903216843, -4.860585618235927718, -5.887257931662889909 ) ) ;
#57993 = EDGE_CURVE ( 'NONE', #22233, #10582, #33827, .T. ) ;
#57994 = CARTESIAN_POINT ( 'NONE',  ( 35.00000000000000000, 4.705694406421931860E-17, -3.469127814946512892E-15 ) ) ;
#57995 = EDGE_LOOP ( 'NONE', ( #64724, #44803, #17265, #23110 ) ) ;
#57996 = DIRECTION ( 'NONE',  ( -1.000000000000000000, 0.000000000000000000, -0.000000000000000000 ) ) ;
#57997 = CARTESIAN_POINT ( 'NONE',  ( 5.514970785353741078, -0.004324946436530173639, -0.001897634820904526036 ) ) ;
#57998 = CARTESIAN_POINT ( 'NONE',  ( -22.28415773361649954, -3.586804264761562333, -0.9182279841530253117 ) ) ;
#57999 = ORIENTED_EDGE ( 'NONE', *, *, #3971, .T. ) ;
#58000 = EDGE_CURVE ( 'NONE', #52203, #57900, #34849, .T. ) ;
#58001 = ORIENTED_EDGE ( 'NONE', *, *, #25207, .F. ) ;
#58002 = CARTESIAN_POINT ( 'NONE',  ( -28.67667724226168602, -1.574547667005685936, 1.049259427760459218 ) ) ;
#58003 = VERTEX_POINT ( 'NONE', #8288 ) ;
#58004 = EDGE_CURVE ( 'NONE', #11187, #21416, #42302, .T. ) ;
#58005 = VERTEX_POINT ( 'NONE', #43861 ) ;
#58006 = CARTESIAN_POINT ( 'NONE',  ( 2.000000000000001776, 0.4804830611970061227, 6.919838746524539452 ) ) ;
#58007 = CARTESIAN_POINT ( 'NONE',  ( -18.04845295627699286, -11.93556515273317942, 1.283449352624662199 ) ) ;
#58008 = DIRECTION ( 'NONE',  ( -1.000000000000000000, 0.000000000000000000, -0.000000000000000000 ) ) ;
#58009 = CARTESIAN_POINT ( 'NONE',  ( 5.530133899448235191, 0.01437126147332034622, -0.006998616117863649434 ) ) ;
#58010 = CARTESIAN_POINT ( 'NONE',  ( -37.00000000000000711, 7.971186206369601734, -9.217970097227642157 ) ) ;
#58011 = DIRECTION ( 'NONE',  ( 0.000000000000000000, -0.01356324068817998940, 0.9999080150203990547 ) ) ;
#58012 = EDGE_CURVE ( 'NONE', #35021, #58885, #5225, .T. ) ;
#58013 = VECTOR ( 'NONE', #15030, 1000.000000000000000 ) ;
#58014 = DIRECTION ( 'NONE',  ( 1.000000000000000000, 0.000000000000000000, 0.000000000000000000 ) ) ;
#58015 = AXIS2_PLACEMENT_3D ( 'NONE', #8455, #18774, #8135 ) ;
#58016 = VERTEX_POINT ( 'NONE', #9563 ) ;
#58017 = CARTESIAN_POINT ( 'NONE',  ( 47.00000000000000711, 4.705694406421931860E-17, -3.469127814946512892E-15 ) ) ;
#58018 = CARTESIAN_POINT ( 'NONE',  ( -22.28121537037576516, -3.028566507474731218, 2.114437713163338284 ) ) ;
#58019 = CARTESIAN_POINT ( 'NONE',  ( 0.2706063244538070012, 4.353289770698386185, -11.44820198696410962 ) ) ;
#58020 = CARTESIAN_POINT ( 'NONE',  ( 35.00000000000000000, 11.78977382767499549, -4.245927698352105928 ) ) ;
#58021 = DIRECTION ( 'NONE',  ( 0.000000000000000000, -0.01356324068817998940, 0.9999080150203990547 ) ) ;
#58022 = EDGE_CURVE ( 'NONE', #57602, #52645, #45823, .T. ) ;
#58023 = CARTESIAN_POINT ( 'NONE',  ( 0.2653141334712594834, 12.05242949860146595, -2.169900597054395863 ) ) ;
#58024 = DIRECTION ( 'NONE',  ( -0.000000000000000000, 0.000000000000000000, 1.000000000000000000 ) ) ;
#58025 = VERTEX_POINT ( 'NONE', #50813 ) ;
#58026 = CARTESIAN_POINT ( 'NONE',  ( -22.31328051695926007, 0.2528478350594092761, 3.781397440874584071 ) ) ;
#58027 = CARTESIAN_POINT ( 'NONE',  ( 0.3278977287071224711, -1.885359334311883961, -12.12129679591848763 ) ) ;
#58028 = FACE_OUTER_BOUND ( 'NONE', #8876, .T. ) ;
#58029 = CARTESIAN_POINT ( 'NONE',  ( 3.152665057736135701, -1.848755561854027452, -7.719888720907647439 ) ) ;
#58030 = EDGE_CURVE ( 'NONE', #15725, #40578, #15225, .T. ) ;
#58031 = CARTESIAN_POINT ( 'NONE',  ( 2.000000000000001776, -6.767909380267597363, 2.119450094687866049 ) ) ;
#58032 = CARTESIAN_POINT ( 'NONE',  ( -26.18760594837597822, -12.07028982502884418, 6.047005920582382288 ) ) ;
#58033 = VERTEX_POINT ( 'NONE', #60449 ) ;
#58034 = CARTESIAN_POINT ( 'NONE',  ( 3.152665057734040488, 0.000000000000000000, 0.000000000000000000 ) ) ;
#58035 = DIRECTION ( 'NONE',  ( -1.000000000000000000, 0.000000000000000000, 0.000000000000000000 ) ) ;
#58036 = CARTESIAN_POINT ( 'NONE',  ( -35.04660725145885891, -0.008800808525089999501, 0.008590646501115670186 ) ) ;
#58037 = ORIENTED_EDGE ( 'NONE', *, *, #58971, .T. ) ;
#58038 = CARTESIAN_POINT ( 'NONE',  ( 0.3006302518452041439, 2.350739146140591984, 12.03044280705495161 ) ) ;
#58039 = CARTESIAN_POINT ( 'NONE',  ( 35.00000000000000000, 4.705694406421931860E-17, -3.469127814946512892E-15 ) ) ;
#58040 = ORIENTED_EDGE ( 'NONE', *, *, #38198, .F. ) ;
#58041 = EDGE_CURVE ( 'NONE', #6845, #39606, #54072, .T. ) ;
#58042 = ORIENTED_EDGE ( 'NONE', *, *, #30996, .T. ) ;
#58043 = DIRECTION ( 'NONE',  ( 0.000000000000000000, 0.000000000000000000, 1.000000000000000000 ) ) ;
#58044 = EDGE_CURVE ( 'NONE', #29266, #58976, #4906, .T. ) ;
#58045 = AXIS2_PLACEMENT_3D ( 'NONE', #39300, #29020, #29334 ) ;
#58046 = CARTESIAN_POINT ( 'NONE',  ( 0.2801149460245132006, -4.374013318106476866, -11.44368419510490575 ) ) ;
#58047 = ORIENTED_EDGE ( 'NONE', *, *, #18199, .F. ) ;
#58048 = CARTESIAN_POINT ( 'NONE',  ( 2.000000000000001776, 5.097042323172456868, 5.501832381651453829 ) ) ;
#58049 = CARTESIAN_POINT ( 'NONE',  ( 0.000000000000000000, 4.409940824963509698, -5.354199675985237050 ) ) ;
#58050 = CARTESIAN_POINT ( 'NONE',  ( 2.241528039335009215, 7.521191296022435857, -1.310213701658512697 ) ) ;
#58051 = CARTESIAN_POINT ( 'NONE',  ( -3.167554099594523720, -12.87069030742389764, 4.088466244554556539 ) ) ;
#58052 = CARTESIAN_POINT ( 'NONE',  ( 2.305787727787084407, 3.682701754025606178, -6.711944854845784292 ) ) ;
#58053 = CARTESIAN_POINT ( 'NONE',  ( 0.2648978790185584908, 6.008231198268983775, 10.67083876753494032 ) ) ;
#58055 = ORIENTED_EDGE ( 'NONE', *, *, #33599, .F. ) ;
#58054 = CARTESIAN_POINT ( 'NONE',  ( 1.633930747250947890, 0.7186603069032649893, 12.68212725188713286 ) ) ;
#58056 = CARTESIAN_POINT ( 'NONE',  ( 8.979959331610965378, 5.149046574253878461, 12.48452308162177538 ) ) ;
#58057 = VERTEX_POINT ( 'NONE', #59812 ) ;
#58058 = CARTESIAN_POINT ( 'NONE',  ( 2.241509619876138171, -0.03828218718775380086, 7.634391113243450988 ) ) ;
#58059 = VERTEX_POINT ( 'NONE', #65110 ) ;
#58060 = B_SPLINE_CURVE_WITH_KNOTS ( 'NONE', 3,
 ( #40375, #59368, #3542, #60340, #34079, #3864, #55359, #50396, #59702, #29427, #4171, #60033, #30083, #35050, #28774, #64998, #54398, #4842, #14449 ),
 .UNSPECIFIED., .F., .F.,
 ( 4, 3, 3, 3, 3, 3, 4 ),
 ( 5.131381242747340533E-18, 2.825908398991825956E-05, 4.208813692703089221E-05, 5.591713747221501498E-05, 6.279584083538142171E-05, 9.105792820727961210E-05, 0.0001153131102486980953 ),
 .UNSPECIFIED. ) ;
#58061 = ORIENTED_EDGE ( 'NONE', *, *, #3584, .F. ) ;
#58062 = CONTEXT_DEPENDENT_SHAPE_REPRESENTATION ( #14912, #58416 ) ;
#58063 = CARTESIAN_POINT ( 'NONE',  ( 37.00000000000000711, 11.80185301892980654, -4.824807283154168402 ) ) ;
#58064 = CARTESIAN_POINT ( 'NONE',  ( -13.86128969992323334, -30.12619713135721611, 5.984278774111453814 ) ) ;
#58065 = ADVANCED_FACE ( 'NONE', ( #24890 ), #65744, .T. ) ;
#58066 = CARTESIAN_POINT ( 'NONE',  ( -4.046008612244236247, 9.338948392566903678, 7.538928574057408127 ) ) ;
#58067 = CARTESIAN_POINT ( 'NONE',  ( -37.00000000000000711, -12.15823808070322265, -0.8294751490780611913 ) ) ;
#58068 = LINE ( 'NONE', #47439, #26737 ) ;
#58069 = ORIENTED_EDGE ( 'NONE', *, *, #57463, .T. ) ;
#58070 =( BOUNDED_SURFACE ( )  B_SPLINE_SURFACE ( 3, 1, ( 
 ( #62405, #62737 ),
 ( #16869, #58104 ),
 ( #12516, #11876 ),
 ( #32149, #52473 ) ),
 .UNSPECIFIED., .F., .F., .F. ) 
 B_SPLINE_SURFACE_WITH_KNOTS ( ( 4, 4 ),
 ( 2, 2 ),
 ( 0.000000000000000000, 1.000000000000000000 ),
 ( 0.000000000000000000, 1.000000000000000000 ),
 .UNSPECIFIED. ) 
 GEOMETRIC_REPRESENTATION_ITEM ( )  RATIONAL_B_SPLINE_SURFACE ( (
 ( 1.000000000000000000, 1.000000000000000000),
 ( 0.8716676215708681896, 0.8964445200148164483),
 ( 0.8716676215708681896, 0.8964445200148164483),
 ( 1.000000000000000000, 1.000000000000000000) ) ) 
 REPRESENTATION_ITEM ( '' )  SURFACE ( )  );
#58071 = CARTESIAN_POINT ( 'NONE',  ( -22.27722019110237284, -0.6492757894141321096, -3.623957119342521516 ) ) ;
#58072 = CARTESIAN_POINT ( 'NONE',  ( 0.3675815128205894289, -3.951233083390547129, 11.62724744438064306 ) ) ;
#58074 = ORIENTED_EDGE ( 'NONE', *, *, #4374, .F. ) ;
#58073 = CARTESIAN_POINT ( 'NONE',  ( 0.2648978790185593790, 11.55204314799269305, -4.063980959784929681 ) ) ;
#58075 = EDGE_LOOP ( 'NONE', ( #62774, #4320, #18248, #41169 ) ) ;
#58076 = CARTESIAN_POINT ( 'NONE',  ( -10.00000000000000178, 0.000000000000000000, 0.000000000000000000 ) ) ;
#58077 = ORIENTED_EDGE ( 'NONE', *, *, #35653, .F. ) ;
#58078 = DIRECTION ( 'NONE',  ( 0.000000000000000000, -0.9985334138511232638, -0.05413890858542831641 ) ) ;
#58079 = LINE ( 'NONE', #16192, #31924 ) ;
#58080 = LINE ( 'NONE', #57763, #51166 ) ;
#58081 = CARTESIAN_POINT ( 'NONE',  ( -37.00000000000000711, 0.000000000000000000, 0.000000000000000000 ) ) ;
#58082 = EDGE_CURVE ( 'NONE', #8903, #13989, #40156, .T. ) ;
#58083 = DIRECTION ( 'NONE',  ( -1.000000000000000000, 0.000000000000000000, 0.000000000000000000 ) ) ;
#58084 = CARTESIAN_POINT ( 'NONE',  ( -29.68541646480307250, -0.9867458123558492389, 13.47080766332845592 ) ) ;
#58085 = DIRECTION ( 'NONE',  ( -1.000000000000000000, 0.000000000000000000, 0.000000000000000000 ) ) ;
#58086 = ORIENTED_EDGE ( 'NONE', *, *, #32199, .F. ) ;
#58087 = DIRECTION ( 'NONE',  ( 0.000000000000000000, 0.000000000000000000, 1.000000000000000000 ) ) ;
#58088 = ORIENTED_EDGE ( 'NONE', *, *, #61536, .F. ) ;
#58089 = CARTESIAN_POINT ( 'NONE',  ( 0.2651627923886317739, -6.199207987242170148, 10.56116046379971962 ) ) ;
#58090 = CARTESIAN_POINT ( 'NONE',  ( -8.019454758349086276, -9.419150639783058665, -9.692301608309891847 ) ) ;
#58091 = CARTESIAN_POINT ( 'NONE',  ( -37.00000000000000711, -11.95840593935199792, -2.346765782874564277 ) ) ;
#58092 = VECTOR ( 'NONE', #57250, 1000.000000000000000 ) ;
#58093 = CARTESIAN_POINT ( 'NONE',  ( 0.2648978790185602672, -11.55204314799261311, -4.063980959785162383 ) ) ;
#58094 = ORIENTED_EDGE ( 'NONE', *, *, #29193, .T. ) ;
#58095 = VERTEX_POINT ( 'NONE', #65429 ) ;
#58096 = CARTESIAN_POINT ( 'NONE',  ( 0.2655924914740778742, 11.52280271232870845, 4.147079829127291006 ) ) ;
#58097 = VECTOR ( 'NONE', #20012, 1000.000000000000000 ) ;
#58098 = ADVANCED_FACE ( 'NONE', ( #60789 ), #50499, .T. ) ;
#58099 = ORIENTED_EDGE ( 'NONE', *, *, #59433, .T. ) ;
#58100 = CARTESIAN_POINT ( 'NONE',  ( 35.00000000000000000, -11.30684963584392477, -4.545979934229371189 ) ) ;
#58101 = CARTESIAN_POINT ( 'NONE',  ( 2.000000000000001776, 3.786546189469178092, 5.663561025469147303 ) ) ;
#58102 = DIRECTION ( 'NONE',  ( 0.000000000000000000, 0.01356324068818000328, -0.9999080150203990547 ) ) ;
#58103 = EDGE_CURVE ( 'NONE', #29107, #49616, #19034, .T. ) ;
#58104 = CARTESIAN_POINT ( 'NONE',  ( -22.51237073810381517, 1.333315726166114823, 4.218051923713566076 ) ) ;
#58105 = EDGE_LOOP ( 'NONE', ( #28850, #7605, #43877, #33741 ) ) ;
#58106 = CARTESIAN_POINT ( 'NONE',  ( 0.2717059086739011531, 12.09156413799790464, 1.953280559502737157 ) ) ;
#58107 = LINE ( 'NONE', #18545, #59755 ) ;
#58108 = CARTESIAN_POINT ( 'NONE',  ( 2.491965175174627678, -1.130870800982672009, 7.634639040875272009 ) ) ;
#58109 = CARTESIAN_POINT ( 'NONE',  ( -43.79915462856099850, -1.187172983101275836, 16.56021102286109326 ) ) ;
#58110 = ADVANCED_FACE ( 'NONE', ( #9245 ), #62321, .F. ) ;
#58111 = DIRECTION ( 'NONE',  ( -1.000000000000000000, 0.000000000000000000, 0.000000000000000000 ) ) ;
#58112 = CARTESIAN_POINT ( 'NONE',  ( -35.00000000000000000, 9.430788938294162094, -7.718225330433707398 ) ) ;
#58113 = ORIENTED_EDGE ( 'NONE', *, *, #36328, .T. ) ;
#58114 = CARTESIAN_POINT ( 'NONE',  ( 145.1370849898475797, -13.49999999999996803, 0.000000000000000000 ) ) ;
#58115 = FACE_OUTER_BOUND ( 'NONE', #35196, .T. ) ;
#58116 = CARTESIAN_POINT ( 'NONE',  ( 5.515188684475870851, 0.001283816547385122813, 0.005194992164431777061 ) ) ;
#58117 = VERTEX_POINT ( 'NONE', #3198 ) ;
#58118 = CARTESIAN_POINT ( 'NONE',  ( -16.98800322446194855, 2.922502605998049674, -13.17987020110343543 ) ) ;
#58119 = CARTESIAN_POINT ( 'NONE',  ( 0.7446945582518111895, -8.243982823409156779, 9.270687147117351756 ) ) ;
#58120 = CARTESIAN_POINT ( 'NONE',  ( 2.406456491626289385, -10.14681500356121013, 2.427896847126302049 ) ) ;
#58121 = EDGE_CURVE ( 'NONE', #49587, #42390, #10516, .T. ) ;
#58122 = CARTESIAN_POINT ( 'NONE',  ( 35.00000000000000000, 2.216820770815085773, -11.53507381115584529 ) ) ;
#58123 = CARTESIAN_POINT ( 'NONE',  ( 3.423896178748678576, -10.94279856996580413, 7.910751437345123982 ) ) ;
#58124 = ORIENTED_EDGE ( 'NONE', *, *, #7201, .F. ) ;
#58125 = ORIENTED_EDGE ( 'NONE', *, *, #10018, .F. ) ;
#58126 = FACE_OUTER_BOUND ( 'NONE', #21919, .T. ) ;
#58127 = ORIENTED_EDGE ( 'NONE', *, *, #15156, .F. ) ;
#58128 = CARTESIAN_POINT ( 'NONE',  ( 2.316650205446322719, 2.457467282897404459, 11.75170002979209194 ) ) ;
#58129 = DIRECTION ( 'NONE',  ( -1.000000000000000000, 0.000000000000000000, 0.000000000000000000 ) ) ;
#58130 = CARTESIAN_POINT ( 'NONE',  ( 1.948354844646196460, 11.63671644762978197, -2.783443994772825114 ) ) ;
#58131 = CARTESIAN_POINT ( 'NONE',  ( 2.241509619876137283, 0.03828218718780714014, -7.634391113243452764 ) ) ;
#58132 = CARTESIAN_POINT ( 'NONE',  ( 2.844750968614003117, 7.828506085987995355, -0.3326424433124895996 ) ) ;
#58133 = CARTESIAN_POINT ( 'NONE',  ( 2.249013661412875287, 5.772355099775897891, 5.000301708457582706 ) ) ;
#58134 = CARTESIAN_POINT ( 'NONE',  ( -10.00000000000000178, 0.000000000000000000, 0.000000000000000000 ) ) ;
#58135 = ORIENTED_EDGE ( 'NONE', *, *, #60221, .F. ) ;
#58136 = ORIENTED_EDGE ( 'NONE', *, *, #20957, .F. ) ;
#58137 = CARTESIAN_POINT ( 'NONE',  ( -35.00000000000000000, 0.000000000000000000, 0.000000000000000000 ) ) ;
#58138 = ORIENTED_EDGE ( 'NONE', *, *, #49416, .T. ) ;
#58139 = VECTOR ( 'NONE', #24527, 1000.000000000000000 ) ;
#58140 = DIRECTION ( 'NONE',  ( 0.000000000000000000, 0.01356324068817998940, -0.9999080150203990547 ) ) ;
#58141 = CARTESIAN_POINT ( 'NONE',  ( 1.287602823388787066, 8.506034117236191960, -9.277923463523999104 ) ) ;
#58142 = AXIS2_PLACEMENT_3D ( 'NONE', #47029, #16093, #51698 ) ;
#58143 = CARTESIAN_POINT ( 'NONE',  ( -22.28121537037576871, -1.565596675942153571, 3.345440028056702264 ) ) ;
#58144 = ORIENTED_EDGE ( 'NONE', *, *, #37851, .F. ) ;
#58145 = DIRECTION ( 'NONE',  ( -1.000000000000000000, 0.000000000000000000, 0.000000000000000000 ) ) ;
#58146 = CARTESIAN_POINT ( 'NONE',  ( -13.86128969992320847, -30.12619713135532251, -5.984278774113396260 ) ) ;
#58147 = DIRECTION ( 'NONE',  ( 0.000000000000000000, -0.9999080150203989437, -0.01356324068819032662 ) ) ;
#58148 = EDGE_CURVE ( 'NONE', #57924, #48534, #62537, .T. ) ;
#58149 = ORIENTED_EDGE ( 'NONE', *, *, #18034, .T. ) ;
#58150 = EDGE_LOOP ( 'NONE', ( #8210, #27545, #29824, #60755 ) ) ;
#58151 = DIRECTION ( 'NONE',  ( 0.000000000000000000, 0.000000000000000000, 1.000000000000000000 ) ) ;
#58152 = ORIENTED_EDGE ( 'NONE', *, *, #32975, .T. ) ;
#58153 = ORIENTED_EDGE ( 'NONE', *, *, #60954, .T. ) ;
#58154 = CYLINDRICAL_SURFACE ( 'NONE', #38632, 5.000000000000000888 ) ;
#58155 = ORIENTED_EDGE ( 'NONE', *, *, #11229, .F. ) ;
#58156 = ORIENTED_EDGE ( 'NONE', *, *, #39840, .T. ) ;
#58157 = CARTESIAN_POINT ( 'NONE',  ( -22.27721056931765631, -2.768264578996974645, 2.427163553894365666 ) ) ;
#58158 = CARTESIAN_POINT ( 'NONE',  ( 0.3675815128205894289, 11.44679196252409348, 4.447030445008218535 ) ) ;
#58159 = EDGE_CURVE ( 'NONE', #60104, #35544, #44074, .T. ) ;
#58160 = CARTESIAN_POINT ( 'NONE',  ( -20.95894390668759044, -11.53024028107489585, -3.336574098666279742 ) ) ;
#58161 = LINE ( 'NONE', #12266, #55316 ) ;
#58162 = CARTESIAN_POINT ( 'NONE',  ( 37.00000000000000711, 12.66641127287627810, 1.457575200925408820 ) ) ;
#58163 = ORIENTED_EDGE ( 'NONE', *, *, #58670, .T. ) ;
#58164 = LINE ( 'NONE', #57856, #22180 ) ;
#58165 = CARTESIAN_POINT ( 'NONE',  ( -22.27721688985630522, 2.843753050855884368, -2.338410344701251642 ) ) ;
#58166 = CARTESIAN_POINT ( 'NONE',  ( 5.514624014163232779, 0.0008859786816842089114, -0.004045310349816142945 ) ) ;
#58167 = CARTESIAN_POINT ( 'NONE',  ( -37.00000000000000711, 0.000000000000000000, 0.000000000000000000 ) ) ;
#58168 = CYLINDRICAL_SURFACE ( 'NONE', #32873, 4.999999999999999112 ) ;
#58169 = FACE_OUTER_BOUND ( 'NONE', #59931, .T. ) ;
#58170 = CARTESIAN_POINT ( 'NONE',  ( 0.2671309869109498303, -11.56263543972755592, -4.036029264453098619 ) ) ;
#58171 = DIRECTION ( 'NONE',  ( 1.000000000000000000, 0.000000000000000000, 0.000000000000000000 ) ) ;
#58172 = CIRCLE ( 'NONE', #29472, 5.000000000000000888 ) ;
#58173 = EDGE_CURVE ( 'NONE', #46419, #29718, #58342, .T. ) ;
#58174 = ORIENTED_EDGE ( 'NONE', *, *, #1871, .T. ) ;
#58175 = CARTESIAN_POINT ( 'NONE',  ( -35.00000000000000000, -9.677500615117949678, 6.657191900728284928 ) ) ;
#58176 = CIRCLE ( 'NONE', #49726, 5.000000000000000888 ) ;
#58177 = ORIENTED_EDGE ( 'NONE', *, *, #40300, .F. ) ;
#58178 = EDGE_CURVE ( 'NONE', #45342, #51818, #11252, .T. ) ;
#58179 = CARTESIAN_POINT ( 'NONE',  ( 0.3474126878361830650, 10.75620725594716021, 5.911350916722074800 ) ) ;
#58180 = CARTESIAN_POINT ( 'NONE',  ( 2.241311220309555097, 5.907514893712990656, -4.835827934490959379 ) ) ;
#58181 = CARTESIAN_POINT ( 'NONE',  ( 12.44547025303417698, -13.08988633905116039, -3.306802340674645180 ) ) ;
#58182 = DIRECTION ( 'NONE',  ( 1.000000000000000000, 0.000000000000000000, 0.000000000000000000 ) ) ;
#58183 = ADVANCED_FACE ( 'NONE', ( #64996 ), #23463, .T. ) ;
#58184 = CARTESIAN_POINT ( 'NONE',  ( 3.031336079628654367, 7.839300734792826297, 0.9593005538809813437 ) ) ;
#58185 = ORIENTED_EDGE ( 'NONE', *, *, #16120, .F. ) ;
#58186 = DIRECTION ( 'NONE',  ( -1.000000000000000000, -0.000000000000000000, 0.000000000000000000 ) ) ;
#58187 = DIRECTION ( 'NONE',  ( 0.000000000000000000, -0.01356324068817998940, 0.9999080150203990547 ) ) ;
#58188 = CARTESIAN_POINT ( 'NONE',  ( 35.00000000000000000, -8.017674001891711200, 9.913596905230193101 ) ) ;
#58189 = VECTOR ( 'NONE', #17518, 1000.000000000000000 ) ;
#58190 = CARTESIAN_POINT ( 'NONE',  ( 0.2648978790185584908, -1.996248716311547433, -12.08224454301450734 ) ) ;
#58191 = AXIS2_PLACEMENT_3D ( 'NONE', #38007, #13081, #22742 ) ;
#58192 = EDGE_CURVE ( 'NONE', #43264, #6288, #23261, .T. ) ;
#58193 = CARTESIAN_POINT ( 'NONE',  ( 0.3675815128205894289, 10.76447900494948584, -5.910255304480332761 ) ) ;
#58194 = ORIENTED_EDGE ( 'NONE', *, *, #49065, .F. ) ;
#58195 = EDGE_CURVE ( 'NONE', #54568, #52675, #18152, .T. ) ;
#58196 = CARTESIAN_POINT ( 'NONE',  ( 2.406456491624854976, -4.662370073865575115, 9.333533259768456603 ) ) ;
#58197 = CARTESIAN_POINT ( 'NONE',  ( 3.780834652287974773, 8.352030633203074927, -8.616471685210672860 ) ) ;
#58198 = ORIENTED_EDGE ( 'NONE', *, *, #16648, .F. ) ;
#58200 = EDGE_CURVE ( 'NONE', #54327, #16429, #11569, .T. ) ;
#58199 = DIRECTION ( 'NONE',  ( -1.000000000000000000, 0.000000000000000000, 0.000000000000000000 ) ) ;
#58201 = EDGE_LOOP ( 'NONE', ( #867, #33840, #62658, #29185 ) ) ;
#58202 = CARTESIAN_POINT ( 'NONE',  ( 0.2638984909335716500, 10.50550771760519986, 6.295352574289022840 ) ) ;
#58203 = DIRECTION ( 'NONE',  ( 1.000000000000000000, 0.000000000000000000, 0.000000000000000000 ) ) ;
#58204 = FACE_OUTER_BOUND ( 'NONE', #1790, .T. ) ;
#58205 = CARTESIAN_POINT ( 'NONE',  ( 12.93723047338301058, 4.476360154859203355, 25.00000000000000000 ) ) ;
#58206 = EDGE_CURVE ( 'NONE', #6535, #24257, #58741, .T. ) ;
#58207 = CARTESIAN_POINT ( 'NONE',  ( -22.27706485742869091, -2.154081322712202873, -2.985151051101508468 ) ) ;
#58208 = ORIENTED_EDGE ( 'NONE', *, *, #4514, .F. ) ;
#58209 = ORIENTED_EDGE ( 'NONE', *, *, #6181, .F. ) ;
#58210 = ORIENTED_EDGE ( 'NONE', *, *, #17109, .F. ) ;
#58211 = CARTESIAN_POINT ( 'NONE',  ( -37.00000000000000711, 5.428340790341860789, -10.91072401419405402 ) ) ;
#58212 = AXIS2_PLACEMENT_3D ( 'NONE', #46536, #2312, #31254 ) ;
#58213 = CARTESIAN_POINT ( 'NONE',  ( 0.2655924914740778742, -2.083162675473693604, 12.06787830249864513 ) ) ;
#58214 = ORIENTED_EDGE ( 'NONE', *, *, #49745, .T. ) ;
#58215 = CARTESIAN_POINT ( 'NONE',  ( -35.00000000000000000, -5.672855678558757830, 10.28547182238005853 ) ) ;
#58216 = DIRECTION ( 'NONE',  ( 1.000000000000000000, 0.000000000000000000, 0.000000000000000000 ) ) ;
#58217 = EDGE_LOOP ( 'NONE', ( #5043, #29603, #2887, #50782 ) ) ;
#58218 = LINE ( 'NONE', #32918, #34341 ) ;
#58219 = CARTESIAN_POINT ( 'NONE',  ( 2.305787727787083519, -2.774453000917102230, -7.135468203930011910 ) ) ;
#58220 = DIRECTION ( 'NONE',  ( -1.000000000000000000, 0.000000000000000000, 0.000000000000000000 ) ) ;
#58221 = ORIENTED_EDGE ( 'NONE', *, *, #57016, .T. ) ;
#58222 = VERTEX_POINT ( 'NONE', #59059 ) ;
#58223 = AXIS2_PLACEMENT_3D ( 'NONE', #65267, #19732, #35320 ) ;
#58224 = CARTESIAN_POINT ( 'NONE',  ( 2.290907136833251201, 2.463690939638674582, 7.243397831411258814 ) ) ;
#58225 = VERTEX_POINT ( 'NONE', #53735 ) ;
#58226 = ORIENTED_EDGE ( 'NONE', *, *, #12443, .F. ) ;
#58227 = VECTOR ( 'NONE', #49364, 1000.000000000000000 ) ;
#58228 = CARTESIAN_POINT ( 'NONE',  ( 2.258463476536646475, 3.701774005560860115, 6.683417898966894199 ) ) ;
#58229 = DIRECTION ( 'NONE',  ( -1.000000000000000000, 0.000000000000000000, 0.000000000000000000 ) ) ;
#58230 = DIRECTION ( 'NONE',  ( 0.000000000000000000, -0.01356324068817991828, 0.9999080150203990547 ) ) ;
#58231 = EDGE_CURVE ( 'NONE', #31007, #23822, #64021, .T. ) ;
#58232 = CARTESIAN_POINT ( 'NONE',  ( -22.28546858134833286, 3.592117891549500452, 0.9133285433746399784 ) ) ;
#58233 = LINE ( 'NONE', #12654, #11779 ) ;
#58234 = FACE_OUTER_BOUND ( 'NONE', #22125, .T. ) ;
#58235 = DIRECTION ( 'NONE',  ( 1.000000000000000000, 0.000000000000000000, 0.000000000000000000 ) ) ;
#58236 = ORIENTED_EDGE ( 'NONE', *, *, #65090, .F. ) ;
#58237 = DIRECTION ( 'NONE',  ( 1.000000000000000000, 0.000000000000000000, -0.000000000000000000 ) ) ;
#58238 = ORIENTED_EDGE ( 'NONE', *, *, #59047, .F. ) ;
#58239 = LINE ( 'NONE', #2397, #31715 ) ;
#58240 = DIRECTION ( 'NONE',  ( 0.000000000000000000, -0.01356324068817999114, 0.9999080150203989437 ) ) ;
#58241 = ORIENTED_EDGE ( 'NONE', *, *, #40930, .F. ) ;
#58242 = EDGE_CURVE ( 'NONE', #28860, #14144, #56192, .T. ) ;
#58243 = LINE ( 'NONE', #64520, #34954 ) ;
#58244 = CARTESIAN_POINT ( 'NONE',  ( 0.2915757698887306848, 12.02962099476165569, -2.339174865979159357 ) ) ;
#58245 = DIRECTION ( 'NONE',  ( -0.000000000000000000, -1.000000000000000000, -0.000000000000000000 ) ) ;
#58246 = ORIENTED_EDGE ( 'NONE', *, *, #41255, .F. ) ;
#58247 = B_SPLINE_CURVE_WITH_KNOTS ( 'NONE', 3,
 ( #52643, #18033, #38297, #48629, #63562, #58274 ),
 .UNSPECIFIED., .F., .F.,
 ( 4, 2, 4 ),
 ( 0.0002637379172192655451, 0.0009975831966643378297, 0.001731428476109410277 ),
 .UNSPECIFIED. ) ;
#58248 = AXIS2_PLACEMENT_3D ( 'NONE', #23755, #29377, #24724 ) ;
#58249 = ADVANCED_FACE ( 'NONE', ( #55224 ), #33954, .T. ) ;
#58250 = VERTEX_POINT ( 'NONE', #34287 ) ;
#58251 = CARTESIAN_POINT ( 'NONE',  ( 2.305787727787084407, -6.711944854845797614, -3.682701754025583085 ) ) ;
#58252 = B_SPLINE_CURVE_WITH_KNOTS ( 'NONE', 3,
 ( #15768, #37373, #21782, #31084, #1157, #21439, #41051, #42032, #42339, #62626, #62312, #46067, #5507, #56347, #51395, #61657 ),
 .UNSPECIFIED., .F., .F.,
 ( 4, 3, 3, 3, 3, 4 ),
 ( 2.710505431213761085E-19, 0.0003017745587525266565, 0.0006035491769808777520, 0.0009053241094668224281, 0.001207275924539992148, 0.001510325902532976602 ),
 .UNSPECIFIED. ) ;
#58253 = CIRCLE ( 'NONE', #39100, 12.74999999999999822 ) ;
#58254 = ORIENTED_EDGE ( 'NONE', *, *, #57727, .T. ) ;
#58255 = DIRECTION ( 'NONE',  ( -1.000000000000000000, 0.000000000000000000, 0.000000000000000000 ) ) ;
#58256 = CARTESIAN_POINT ( 'NONE',  ( 2.241526690369557873, -1.342748965918832971, -7.515450538999847829 ) ) ;
#58257 = CARTESIAN_POINT ( 'NONE',  ( -3.547682422092472976, -11.41132889151838725, 7.222740821714795700 ) ) ;
#58258 = EDGE_CURVE ( 'NONE', #62820, #47648, #23296, .T. ) ;
#58259 = DIRECTION ( 'NONE',  ( -1.000000000000000000, -0.000000000000000000, 0.000000000000000000 ) ) ;
#58260 = ORIENTED_EDGE ( 'NONE', *, *, #4123, .T. ) ;
#58261 = DIRECTION ( 'NONE',  ( -1.000000000000000000, -0.000000000000000000, 0.000000000000000000 ) ) ;
#58262 = CIRCLE ( 'NONE', #46575, 5.000000000000000888 ) ;
#58263 = AXIS2_PLACEMENT_3D ( 'NONE', #14974, #31589, #20654 ) ;
#58264 = CIRCLE ( 'NONE', #45387, 12.18650000000000411 ) ;
#58265 = CARTESIAN_POINT ( 'NONE',  ( 12.54355452190762144, -28.27128177340750526, -13.14909765253698559 ) ) ;
#58266 =( BOUNDED_CURVE ( )  B_SPLINE_CURVE ( 3, ( #58197, #18637, #54187, #17640 ),
 .UNSPECIFIED., .F., .F. ) 
 B_SPLINE_CURVE_WITH_KNOTS ( ( 4, 4 ),
 ( 3.942573786070413977, 3.954312062358601221 ),
 .UNSPECIFIED. ) 
 CURVE ( )  GEOMETRIC_REPRESENTATION_ITEM ( )  RATIONAL_B_SPLINE_CURVE ( ( 1.000000000000000000, 0.9999885177721090646, 0.9999885177721090646, 1.000000000000000000 ) ) 
 REPRESENTATION_ITEM ( '' )  );
#58267 = EDGE_CURVE ( 'NONE', #41839, #9878, #48762, .T. ) ;
#58268 = CARTESIAN_POINT ( 'NONE',  ( 21.98157680265827452, 12.95962480054460819, -3.798644489114345824 ) ) ;
#58270 = VECTOR ( 'NONE', #1337, 1000.000000000000000 ) ;
#58269 = CARTESIAN_POINT ( 'NONE',  ( -27.08421723179412410, -0.6782017488087908053, 2.188590898430377685 ) ) ;
#58271 = EDGE_CURVE ( 'NONE', #22647, #48416, #46650, .T. ) ;
#58272 = FACE_OUTER_BOUND ( 'NONE', #34701, .T. ) ;
#58273 = CARTESIAN_POINT ( 'NONE',  ( 2.241317068080791230, -5.789053609344619211, 4.977030124433455605 ) ) ;
#58274 = CARTESIAN_POINT ( 'NONE',  ( -22.31328051695926007, -0.8849444482787947042, 3.685074213229300621 ) ) ;
#58275 = AXIS2_PLACEMENT_3D ( 'NONE', #43501, #64132, #65097 ) ;
#58276 = EDGE_CURVE ( 'NONE', #18784, #10110, #37254, .T. ) ;
#58277 = ORIENTED_EDGE ( 'NONE', *, *, #59384, .F. ) ;
#58278 = EDGE_CURVE ( 'NONE', #24195, #46588, #30212, .T. ) ;
#58279 = CARTESIAN_POINT ( 'NONE',  ( 12.17435499564740908, -9.235710332726100091, -7.670499671992002888 ) ) ;
#58280 = ORIENTED_EDGE ( 'NONE', *, *, #30358, .T. ) ;
#58281 = CARTESIAN_POINT ( 'NONE',  ( 35.00000000000000000, 11.47561260193577048, -5.556331110570448040 ) ) ;
#58282 = CARTESIAN_POINT ( 'NONE',  ( -22.27945548916780183, 3.673577025288763398, -0.3299677273100581343 ) ) ;
#58283 = DIRECTION ( 'NONE',  ( 0.000000000000000000, -0.01356324068817999114, 0.9999080150203989437 ) ) ;
#58284 = VERTEX_POINT ( 'NONE', #49599 ) ;
#58285 = EDGE_CURVE ( 'NONE', #53955, #5474, #42351, .T. ) ;
#58286 = UNCERTAINTY_MEASURE_WITH_UNIT (LENGTH_MEASURE( 1.000000000000000082E-05 ), #42479, 'distance_accuracy_value', 'NONE');
#58287 = DIRECTION ( 'NONE',  ( 0.000000000000000000, 0.1118654143051546479, 0.9937233664769768993 ) ) ;
#58288 = ORIENTED_EDGE ( 'NONE', *, *, #38401, .T. ) ;
#58289 = LINE ( 'NONE', #12706, #12618 ) ;
#58290 = VERTEX_POINT ( 'NONE', #34914 ) ;
#58291 = ORIENTED_EDGE ( 'NONE', *, *, #65228, .F. ) ;
#58292 = CARTESIAN_POINT ( 'NONE',  ( -10.48620311856347875, -9.720786832536937538, -7.036071585506805448 ) ) ;
#58293 = CARTESIAN_POINT ( 'NONE',  ( 2.273267844204865273, -7.130811676080292649, 2.756477528575274061 ) ) ;
#58294 = CIRCLE ( 'NONE', #27472, 12.74999999999999822 ) ;
#58295 = ORIENTED_EDGE ( 'NONE', *, *, #64345, .F. ) ;
#58296 = CARTESIAN_POINT ( 'NONE',  ( 3.152665057734128862, 5.761241965769081652, 5.461013642405580626 ) ) ;
#58297 = FACE_OUTER_BOUND ( 'NONE', #41032, .T. ) ;
#58298 = DIRECTION ( 'NONE',  ( 1.000000000000000000, -0.000000000000000000, 0.000000000000000000 ) ) ;
#58299 = CARTESIAN_POINT ( 'NONE',  ( -47.00000000000000711, 0.000000000000000000, 0.000000000000000000 ) ) ;
#58300 = VERTEX_POINT ( 'NONE', #50903 ) ;
#58301 = CARTESIAN_POINT ( 'NONE',  ( -37.00000000000000711, 0.000000000000000000, 0.000000000000000000 ) ) ;
#58302 = CARTESIAN_POINT ( 'NONE',  ( 11.77510182854060439, -29.30972061338670187, 6.669332763617590309 ) ) ;
#58303 = LINE ( 'NONE', #11739, #29205 ) ;
#58305 = ORIENTED_EDGE ( 'NONE', *, *, #61374, .T. ) ;
#58304 = CARTESIAN_POINT ( 'NONE',  ( 47.00000000000000711, 4.705694406421931860E-17, -3.469127814946512892E-15 ) ) ;
#58306 = CARTESIAN_POINT ( 'NONE',  ( -27.45775109278351067, 11.83395752356219077, -1.989333891161980894 ) ) ;
#58307 = ORIENTED_EDGE ( 'NONE', *, *, #1033, .T. ) ;
#58308 = CARTESIAN_POINT ( 'NONE',  ( -35.00000000000000000, -8.052525312709946093, 8.551552972817052733 ) ) ;
#58309 = ORIENTED_EDGE ( 'NONE', *, *, #41018, .F. ) ;
#58310 = DIRECTION ( 'NONE',  ( -1.000000000000000000, 0.000000000000000000, 0.000000000000000000 ) ) ;
#58311 = CARTESIAN_POINT ( 'NONE',  ( 35.00000000000000000, 1.285879139104720949E-14, 0.000000000000000000 ) ) ;
#58312 = AXIS2_PLACEMENT_3D ( 'NONE', #32814, #2266, #57804 ) ;
#58313 = DIRECTION ( 'NONE',  ( 0.000000000000000000, 0.000000000000000000, 1.000000000000000000 ) ) ;
#58314 = CARTESIAN_POINT ( 'NONE',  ( 0.3610902822527289335, -3.951920836718799457, 11.62472836966322731 ) ) ;
#58315 = EDGE_CURVE ( 'NONE', #28659, #25549, #10007, .T. ) ;
#58316 = CARTESIAN_POINT ( 'NONE',  ( 0.2915757698887286864, 9.524403232224875282, 7.711631695122881602 ) ) ;
#58317 = DIRECTION ( 'NONE',  ( 0.000000000000000000, -0.9903235168508535136, -0.1387779952735920808 ) ) ;
#58318 = CARTESIAN_POINT ( 'NONE',  ( 13.15812208069034384, 12.98105700980179833, -3.712867825188221449 ) ) ;
#58319 = VERTEX_POINT ( 'NONE', #41229 ) ;
#58320 = AXIS2_PLACEMENT_3D ( 'NONE', #35000, #18547, #33146 ) ;
#58321 = ORIENTED_EDGE ( 'NONE', *, *, #56338, .T. ) ;
#58322 = FACE_OUTER_BOUND ( 'NONE', #16539, .T. ) ;
#58323 = ORIENTED_EDGE ( 'NONE', *, *, #21566, .F. ) ;
#58324 = B_SPLINE_CURVE_WITH_KNOTS ( 'NONE', 3,
 ( #31742, #31436, #10165, #6180, #30444, #25799, #16482, #46092, #56373, #4872, #21116, #850, #25138, #41392, #36423, #56737, #51735, #53367, #32402, #33060, #37062, #27749, #7815, #62652 ),
 .UNSPECIFIED., .F., .F.,
 ( 4, 2, 2, 2, 2, 2, 2, 2, 2, 2, 2, 4 ),
 ( 0.000000000000000000, 0.001335873637788843014, 0.002671747275577686029, 0.004007620913366529043, 0.005343494551155374660, 0.008015241826733065025, 0.01068698910231075626, 0.01202286274009960361, 0.01335873637788844923, 0.01603048365346615087, 0.01870223092904384904, 0.02137397820462155415 ),
 .UNSPECIFIED. ) ;
#58325 = ORIENTED_EDGE ( 'NONE', *, *, #54179, .F. ) ;
#58326 = ADVANCED_FACE ( 'NONE', ( #25290 ), #41896, .T. ) ;
#58327 = DIRECTION ( 'NONE',  ( 1.000000000000000000, 0.000000000000000000, 0.000000000000000000 ) ) ;
#58328 = CARTESIAN_POINT ( 'NONE',  ( 2.000000000000001776, -6.906413915731192787, 0.6453518998147164121 ) ) ;
#58329 = AXIS2_PLACEMENT_3D ( 'NONE', #2497, #63304, #18099 ) ;
#58330 = FACE_OUTER_BOUND ( 'NONE', #43650, .T. ) ;
#58331 = CARTESIAN_POINT ( 'NONE',  ( -22.27756824490284515, 0.9472004376381394364, 3.558840239148765239 ) ) ;
#58332 = DIRECTION ( 'NONE',  ( 0.000000000000000000, 0.000000000000000000, 1.000000000000000000 ) ) ;
#58333 = CARTESIAN_POINT ( 'NONE',  ( 2.241506898688419014, -7.525229609709731093, -1.286963596520069864 ) ) ;
#58334 = CARTESIAN_POINT ( 'NONE',  ( 0.9232167919969126446, -10.99620217063211669, -5.871274944231814175 ) ) ;
#58335 = ORIENTED_EDGE ( 'NONE', *, *, #45056, .F. ) ;
#58336 = CARTESIAN_POINT ( 'NONE',  ( 2.241352910868909643, -5.794346703933810794, -4.970878533273820565 ) ) ;
#58337 = CARTESIAN_POINT ( 'NONE',  ( -35.04643116707788408, -0.01135624435144415301, -0.004425962698870883338 ) ) ;
#58338 = EDGE_CURVE ( 'NONE', #25841, #4330, #31275, .T. ) ;
#58339 = EDGE_CURVE ( 'NONE', #53221, #17893, #6276, .T. ) ;
#58340 = DIRECTION ( 'NONE',  ( -1.000000000000000000, 0.000000000000000000, 0.000000000000000000 ) ) ;
#58341 = DIRECTION ( 'NONE',  ( 1.000000000000000000, 0.000000000000000000, 0.000000000000000000 ) ) ;
#58342 = CIRCLE ( 'NONE', #12651, 12.73084802173761787 ) ;
#58343 = CIRCLE ( 'NONE', #60463, 7.499999999999988454 ) ;
#58344 = FACE_OUTER_BOUND ( 'NONE', #27587, .T. ) ;
#58345 = CARTESIAN_POINT ( 'NONE',  ( 5.520433897694421610, -0.004666464468077943101, -0.01432141647227068090 ) ) ;
#58346 = VERTEX_POINT ( 'NONE', #51891 ) ;
#58347 = FACE_OUTER_BOUND ( 'NONE', #29307, .T. ) ;
#58348 = CARTESIAN_POINT ( 'NONE',  ( 0.3053067050349179690, -1.901204202464590542, -12.11120005789973142 ) ) ;
#58349 = CARTESIAN_POINT ( 'NONE',  ( 1.452237505248555660, -8.579708443906683968, -9.303501428256112149 ) ) ;
#58350 = EDGE_CURVE ( 'NONE', #63668, #10675, #16635, .T. ) ;
#58351 = CIRCLE ( 'NONE', #63601, 11.99999999999999822 ) ;
#58352 = EDGE_CURVE ( 'NONE', #743, #18633, #60412, .T. ) ;
#58353 = DIRECTION ( 'NONE',  ( 0.000000000000000000, 0.6051742151937609115, 0.7960930657056469739 ) ) ;
#58354 = CARTESIAN_POINT ( 'NONE',  ( 5.536195898058073439, -0.008411485181668792652, 0.001224473329857563367 ) ) ;
#58355 = AXIS2_PLACEMENT_3D ( 'NONE', #26950, #7303, #58531 ) ;
#58356 = ORIENTED_EDGE ( 'NONE', *, *, #31015, .T. ) ;
#58357 = CARTESIAN_POINT ( 'NONE',  ( 47.00000000000000711, 4.705694406421931860E-17, -3.469127814946512892E-15 ) ) ;
#58358 = DIRECTION ( 'NONE',  ( -1.000000000000000000, 0.000000000000000000, -0.000000000000000000 ) ) ;
#58359 = CARTESIAN_POINT ( 'NONE',  ( 35.00000000000000000, -11.02904044024205987, 4.041347439435972966 ) ) ;
#58360 = CARTESIAN_POINT ( 'NONE',  ( 1.104777566491147001, -12.40974092093471093, -1.703053712365451222 ) ) ;
#58361 = ORIENTED_EDGE ( 'NONE', *, *, #34679, .T. ) ;
#58362 = EDGE_CURVE ( 'NONE', #4327, #30401, #13697, .T. ) ;
#58363 = CARTESIAN_POINT ( 'NONE',  ( -10.00000000000000178, 0.000000000000000000, 0.000000000000000000 ) ) ;
#58364 = CARTESIAN_POINT ( 'NONE',  ( 0.2650492594609233921, -4.084774262246008369, -11.54478160586241309 ) ) ;
#58365 = ORIENTED_EDGE ( 'NONE', *, *, #2214, .T. ) ;
#58366 = VERTEX_POINT ( 'NONE', #1353 ) ;
#58367 = CARTESIAN_POINT ( 'NONE',  ( -37.00000000000000711, 3.704519465651306742, 11.60979404548636218 ) ) ;
#58368 = EDGE_CURVE ( 'NONE', #18433, #42715, #11140, .T. ) ;
#58369 = CARTESIAN_POINT ( 'NONE',  ( 0.2739690278137290047, -4.360944092821376294, -11.44648082006009560 ) ) ;
#58370 = ORIENTED_EDGE ( 'NONE', *, *, #19413, .T. ) ;
#58371 = CIRCLE ( 'NONE', #30728, 4.999999999999999112 ) ;
#58372 = CARTESIAN_POINT ( 'NONE',  ( 2.000000000000001776, 4.409940824963425321, 5.354199675985255702 ) ) ;
#58373 = CARTESIAN_POINT ( 'NONE',  ( 0.3040950598368144520, -9.552450779732161834, 7.687624643091400145 ) ) ;
#58374 = CARTESIAN_POINT ( 'NONE',  ( 35.00000000000000000, 12.15823808070323508, 0.8294751490777961811 ) ) ;
#58375 = CARTESIAN_POINT ( 'NONE',  ( 2.256373768223414622, -7.545294827890042022, -1.195444820369755412 ) ) ;
#58376 = CARTESIAN_POINT ( 'NONE',  ( 2.491965175174396752, 3.673871285745645920, -6.787433375639467137 ) ) ;
#58377 = CARTESIAN_POINT ( 'NONE',  ( -37.00000000000000711, -11.26103545359858060, 3.340853584269496412 ) ) ;
#58379 = VERTEX_POINT ( 'NONE', #20304 ) ;
#58378 = CARTESIAN_POINT ( 'NONE',  ( -10.00000000000000178, 0.000000000000000000, 0.000000000000000000 ) ) ;
#58380 = CARTESIAN_POINT ( 'NONE',  ( 1.719304012341432264, 5.066286238787408358, -11.67935079956426847 ) ) ;
#58381 = ORIENTED_EDGE ( 'NONE', *, *, #26876, .F. ) ;
#58382 = CARTESIAN_POINT ( 'NONE',  ( 0.2648978790185584908, 10.67083876753500427, -6.008231198268870976 ) ) ;
#58383 = ORIENTED_EDGE ( 'NONE', *, *, #25284, .F. ) ;
#58384 = EDGE_LOOP ( 'NONE', ( #43489, #40740, #33903, #104 ) ) ;
#58385 = CONTEXT_DEPENDENT_SHAPE_REPRESENTATION ( #39991, #46151 ) ;
#58386 = CARTESIAN_POINT ( 'NONE',  ( -27.27855387000350262, 25.00000000000000000, 5.631341004100471892 ) ) ;
#58387 = CARTESIAN_POINT ( 'NONE',  ( -13.03183108261633549, -30.03462372422968940, 7.545134388564851413 ) ) ;
#58388 = CARTESIAN_POINT ( 'NONE',  ( -3.908294913248263835, 8.114081195363114674, 8.852078639661073112 ) ) ;
#58389 = AXIS2_PLACEMENT_3D ( 'NONE', #23169, #64374, #13819 ) ;
#58390 = AXIS2_PLACEMENT_3D ( 'NONE', #10889, #602, #30189 ) ;
#58391 = CARTESIAN_POINT ( 'NONE',  ( 35.00000000000000000, -8.854740511458901508, -7.717887834988215623 ) ) ;
#58392 = DIRECTION ( 'NONE',  ( 0.000000000000000000, 0.000000000000000000, 1.000000000000000000 ) ) ;
#58393 = VERTEX_POINT ( 'NONE', #51246 ) ;
#58394 = EDGE_CURVE ( 'NONE', #35661, #45163, #44502, .T. ) ;
#58395 = CARTESIAN_POINT ( 'NONE',  ( -25.29745827051326756, -10.31977495403786627, 6.126035789533863074 ) ) ;
#58396 = VECTOR ( 'NONE', #36487, 1000.000000000000000 ) ;
#58398 = B_SPLINE_CURVE_WITH_KNOTS ( 'NONE', 3,
 ( #62345, #27118, #37077, #47414, #1850, #18785, #63995, #8466, #38733, #3169, #23108, #58038, #27762, #63327, #53035, #54025, #12782, #17794, #28108, #52724, #43713, #33073 ),
 .UNSPECIFIED., .F., .F.,
 ( 4, 3, 3, 3, 3, 3, 3, 4 ),
 ( 1.318988870012550486E-18, 4.449119708436802246E-05, 6.626296329540413402E-05, 8.803456484962554629E-05, 0.0001098060367612792949, 0.0001315774408628498792, 0.0001760698110411158834, 0.0001829697163287818842 ),
 .UNSPECIFIED. ) ;
#58397 = CARTESIAN_POINT ( 'NONE',  ( -35.00000000000000000, -11.65554240571058031, 1.456211999474302798 ) ) ;
#58400 = VERTEX_POINT ( 'NONE', #40922 ) ;
#58399 = CARTESIAN_POINT ( 'NONE',  ( 1.719304012340733934, -12.20344780066092305, -3.626341562669774365 ) ) ;
#58401 = ORIENTED_EDGE ( 'NONE', *, *, #25043, .F. ) ;
#58402 = CARTESIAN_POINT ( 'NONE',  ( -37.00000000000000711, 10.23119532541083743, -7.608228585767615293 ) ) ;
#58403 = ORIENTED_EDGE ( 'NONE', *, *, #17114, .F. ) ;
#58404 = CARTESIAN_POINT ( 'NONE',  ( 35.00000000000000000, 3.916263239775349625, -11.07407352312214144 ) ) ;
#58405 = CARTESIAN_POINT ( 'NONE',  ( 1.719304012339844867, -10.62216384465586216, 7.017415949612814785 ) ) ;
#58406 = CARTESIAN_POINT ( 'NONE',  ( 2.000000000000001776, -3.786546189469212731, 5.663561025469122434 ) ) ;
#58408 = AXIS2_PLACEMENT_3D ( 'NONE', #21819, #62348, #1852 ) ;
#58407 = CARTESIAN_POINT ( 'NONE',  ( -37.00000000000000711, 6.265926637539497079, 11.10408318471061584 ) ) ;
#58409 = CARTESIAN_POINT ( 'NONE',  ( 35.00000000000000000, -3.511814412392203266, -11.66953048682398730 ) ) ;
#58410 = CARTESIAN_POINT ( 'NONE',  ( -29.57728396573499552, 0.08119487476310269236, 13.50144130734792292 ) ) ;
#58411 = DIRECTION ( 'NONE',  ( 0.000000000000000000, 0.000000000000000000, -1.000000000000000000 ) ) ;
#58412 = VECTOR ( 'NONE', #27592, 1000.000000000000000 ) ;
#58413 = ORIENTED_EDGE ( 'NONE', *, *, #31019, .T. ) ;
#58414 = CARTESIAN_POINT ( 'NONE',  ( -10.00000000000000178, 0.000000000000000000, 0.000000000000000000 ) ) ;
#58415 = ORIENTED_EDGE ( 'NONE', *, *, #32438, .T. ) ;
#58416 = PRODUCT_DEFINITION_SHAPE ( 'NONE', 'NONE',  #65811 ) ;
#58417 = B_SPLINE_CURVE_WITH_KNOTS ( 'NONE', 3,
 ( #22331, #12357, #62905, #28005, #17369, #32625, #7369, #38284, #33639, #37648, #42955, #53615, #3072, #47314, #63235, #48309, #2760, #23017 ),
 .UNSPECIFIED., .F., .F.,
 ( 4, 2, 2, 2, 2, 2, 2, 2, 4 ),
 ( 0.000000000000000000, 0.0009233824328804393286, 0.001385073649320658342, 0.001846764865760876922, 0.002770147298641318419, 0.003693529731521760350, 0.004616912164402201847, 0.005540294597282643778, 0.007387059463043525905 ),
 .UNSPECIFIED. ) ;
#58418 = EDGE_CURVE ( 'NONE', #63537, #17242, #50891, .T. ) ;
#58419 = CARTESIAN_POINT ( 'NONE',  ( 2.000000000000001776, -5.814643797626954935, 3.550179297009551149 ) ) ;
#58420 = ADVANCED_FACE ( 'NONE', ( #26602 ), #23697, .F. ) ;
#58421 = CARTESIAN_POINT ( 'NONE',  ( 2.290907136833251201, -3.965134647955939950, 6.543263131934282661 ) ) ;
#58422 = CIRCLE ( 'NONE', #1080, 5.000000000000000888 ) ;
#58423 = DIRECTION ( 'NONE',  ( 1.000000000000000000, 0.000000000000000000, -0.000000000000000000 ) ) ;
#58424 = ADVANCED_FACE ( 'NONE', ( #16312 ), #36588, .F. ) ;
#58425 = VERTEX_POINT ( 'NONE', #21635 ) ;
#58426 = DIRECTION ( 'NONE',  ( 0.000000000000000000, 0.000000000000000000, -1.000000000000000000 ) ) ;
#58427 = ORIENTED_EDGE ( 'NONE', *, *, #26123, .T. ) ;
#58428 = DIRECTION ( 'NONE',  ( 0.000000000000000000, 0.000000000000000000, 1.000000000000000000 ) ) ;
#58429 = CARTESIAN_POINT ( 'NONE',  ( 0.2646305136544065406, 11.55263159009964191, -4.064188116014433305 ) ) ;
#58430 = CARTESIAN_POINT ( 'NONE',  ( -27.10128162969864007, -2.102429195190290034, -1.032914450115358651 ) ) ;
#58431 = CARTESIAN_POINT ( 'NONE',  ( 2.284126774967658591, 1.483972655035312505, -7.503320429541866510 ) ) ;
#58432 = ORIENTED_EDGE ( 'NONE', *, *, #50921, .F. ) ;
#58433 = CARTESIAN_POINT ( 'NONE',  ( 2.770579946183322928, 2.384572752174086041, 7.437949029067695506 ) ) ;
#58434 = CARTESIAN_POINT ( 'NONE',  ( -22.71097035706202405, -0.4203397252017116448, 4.965150228107737540 ) ) ;
#58435 = CARTESIAN_POINT ( 'NONE',  ( 0.2653141334712559307, -10.62748186152493268, -6.084912053827449263 ) ) ;
#58436 = CARTESIAN_POINT ( 'NONE',  ( -40.19089168456216754, -1.800105668799816039, 19.87241647152734458 ) ) ;
#58437 = EDGE_CURVE ( 'NONE', #11101, #281, #35725, .T. ) ;
#58438 = AXIS2_PLACEMENT_3D ( 'NONE', #43595, #63885, #18364 ) ;
#58439 = CARTESIAN_POINT ( 'NONE',  ( 2.256373768223416842, -0.1329433694243792041, -7.638251659827605344 ) ) ;
#58440 = DIRECTION ( 'NONE',  ( -1.000000000000000000, 0.000000000000000000, -0.000000000000000000 ) ) ;
#58441 = ORIENTED_EDGE ( 'NONE', *, *, #30030, .T. ) ;
#58442 = DIRECTION ( 'NONE',  ( -1.000000000000000000, -0.000000000000000000, -0.000000000000000000 ) ) ;
#58443 = DIRECTION ( 'NONE',  ( 0.000000000000000000, 0.01356324068817998940, -0.9999080150203989437 ) ) ;
#58444 = CARTESIAN_POINT ( 'NONE',  ( -11.25859294448574666, -33.36858074101470351, -11.10377723166772768 ) ) ;
#58445 = ORIENTED_EDGE ( 'NONE', *, *, #14917, .T. ) ;
#58446 = CARTESIAN_POINT ( 'NONE',  ( -18.08686583997275221, 5.151216734910927464, -12.47858029384662970 ) ) ;
#58447 = CARTESIAN_POINT ( 'NONE',  ( 37.00000000000000711, -7.882940143791699050, 10.02106554660717030 ) ) ;
#58448 = CARTESIAN_POINT ( 'NONE',  ( 0.000000000000000000, 0.000000000000000000, 0.000000000000000000 ) ) ;
#58449 = B_SPLINE_CURVE_WITH_KNOTS ( 'NONE', 3,
 ( #2250, #32479, #28479, #48143, #32800, #63086, #42128, #42444, #13203, #7213 ),
 .UNSPECIFIED., .F., .F.,
 ( 4, 3, 3, 4 ),
 ( 5.401523115762181559E-05, 0.0008136511341527790341, 0.004068255670953091485, 0.005063778443040924809 ),
 .UNSPECIFIED. ) ;
#58450 = CARTESIAN_POINT ( 'NONE',  ( 1.937114397841932290, 11.53912442307263042, -5.620553190832856316 ) ) ;
#58451 = CARTESIAN_POINT ( 'NONE',  ( 0.2915757698887289640, -11.44067056871811516, 4.392559307431859850 ) ) ;
#58452 = EDGE_CURVE ( 'NONE', #9460, #56593, #31730, .T. ) ;
#58453 = ORIENTED_EDGE ( 'NONE', *, *, #43993, .T. ) ;
#58454 = DIRECTION ( 'NONE',  ( 0.000000000000000000, -0.01356324068817999114, 0.9999080150203990547 ) ) ;
#58455 = ORIENTED_EDGE ( 'NONE', *, *, #27331, .F. ) ;
#58456 = AXIS2_PLACEMENT_3D ( 'NONE', #29473, #6196, #4892 ) ;
#58457 = CARTESIAN_POINT ( 'NONE',  ( 5.516018279890452902, -0.005042957932159101465, -0.004525000489649917343 ) ) ;
#58459 = DIRECTION ( 'NONE',  ( -1.000000000000000000, 0.000000000000000000, 0.000000000000000000 ) ) ;
#58458 =( BOUNDED_CURVE ( )  B_SPLINE_CURVE ( 3, ( #7496, #882, #21154, #3192 ),
 .UNSPECIFIED., .F., .F. ) 
 B_SPLINE_CURVE_WITH_KNOTS ( ( 4, 4 ),
 ( 1.852694126892728388, 1.873650368502720598 ),
 .UNSPECIFIED. ) 
 CURVE ( )  GEOMETRIC_REPRESENTATION_ITEM ( )  RATIONAL_B_SPLINE_CURVE ( ( 1.000000000000000000, 0.9999634033296326274, 0.9999634033296326274, 1.000000000000000000 ) ) 
 REPRESENTATION_ITEM ( '' )  );
#58460 = CARTESIAN_POINT ( 'NONE',  ( 3.152665057734040488, 0.000000000000000000, 0.000000000000000000 ) ) ;
#58461 = CARTESIAN_POINT ( 'NONE',  ( 1.719304012341460908, 3.626341562669523011, -12.20344780066162649 ) ) ;
#58462 = DIRECTION ( 'NONE',  ( -1.000000000000000000, 0.000000000000000000, 0.000000000000000000 ) ) ;
#58463 = CARTESIAN_POINT ( 'NONE',  ( 2.251152103363642798, -1.202724109297136135, 7.542379262759451031 ) ) ;
#58464 = CYLINDRICAL_SURFACE ( 'NONE', #27624, 12.74999999999999822 ) ;
#58465 = ORIENTED_EDGE ( 'NONE', *, *, #64184, .T. ) ;
#58466 = ORIENTED_EDGE ( 'NONE', *, *, #22517, .F. ) ;
#58467 = CARTESIAN_POINT ( 'NONE',  ( 0.2655924914740778187, -10.62761259256421198, 6.084990060696473968 ) ) ;
#58468 = CIRCLE ( 'NONE', #1117, 12.74999999999999822 ) ;
#58469 = ORIENTED_EDGE ( 'NONE', *, *, #31472, .T. ) ;
#58470 =( LENGTH_UNIT ( ) NAMED_UNIT ( * ) SI_UNIT ( .MILLI., .METRE. ) );
#58471 = CARTESIAN_POINT ( 'NONE',  ( 2.000000000000001776, -5.769711778877344877, 4.791703871138500936 ) ) ;
#58472 = CARTESIAN_POINT ( 'NONE',  ( 2.990245332647814891, -8.130497889782889231, 2.413832934171158406 ) ) ;
#58473 = CARTESIAN_POINT ( 'NONE',  ( -28.67667724226168602, -0.8389685652161974483, 1.695959153103712369 ) ) ;
#58474 = VERTEX_POINT ( 'NONE', #11960 ) ;
#58475 = CARTESIAN_POINT ( 'NONE',  ( -37.00000000000000711, 12.12087942037211263, -1.262958560998631796 ) ) ;
#58476 = EDGE_CURVE ( 'NONE', #64903, #15913, #53192, .T. ) ;
#58477 = CARTESIAN_POINT ( 'NONE',  ( 2.257661810676415470, 6.547845034191149161, -3.936095962955222127 ) ) ;
#58478 = LINE ( 'NONE', #32198, #9538 ) ;
#58479 = ORIENTED_EDGE ( 'NONE', *, *, #20389, .F. ) ;
#58480 = ORIENTED_EDGE ( 'NONE', *, *, #30635, .F. ) ;
#58481 = DIRECTION ( 'NONE',  ( 1.000000000000000000, 0.000000000000000000, 0.000000000000000000 ) ) ;
#58482 = EDGE_CURVE ( 'NONE', #15892, #49980, #38143, .T. ) ;
#58483 = VECTOR ( 'NONE', #36775, 1000.000000000000000 ) ;
#58484 = ORIENTED_EDGE ( 'NONE', *, *, #38461, .F. ) ;
#58485 = DIRECTION ( 'NONE',  ( 0.000000000000000000, -0.9903235168508535136, -0.1387779952735920808 ) ) ;
#58486 = ORIENTED_EDGE ( 'NONE', *, *, #42431, .F. ) ;
#58487 = ORIENTED_EDGE ( 'NONE', *, *, #43169, .T. ) ;
#58488 = CARTESIAN_POINT ( 'NONE',  ( 0.3632410797595211904, 4.445654054452527149, 11.44577450250088546 ) ) ;
#58489 = CARTESIAN_POINT ( 'NONE',  ( -27.10719052120871098, -1.622102031466687189, 1.714424047991066846 ) ) ;
#58490 = AXIS2_PLACEMENT_3D ( 'NONE', #44846, #34211, #18934 ) ;
#58492 = VECTOR ( 'NONE', #55471, 1000.000000000000000 ) ;
#58491 = CARTESIAN_POINT ( 'NONE',  ( 2.000000000000001776, 0.000000000000000000, 0.000000000000000000 ) ) ;
#58494 = EDGE_CURVE ( 'NONE', #8357, #62996, #14728, .T. ) ;
#58493 = LINE ( 'NONE', #17269, #64 ) ;
#58495 = DIRECTION ( 'NONE',  ( -1.000000000000000000, 0.000000000000000000, 0.000000000000000000 ) ) ;
#58496 = CARTESIAN_POINT ( 'NONE',  ( 0.2648978790185602672, 11.55204314799263798, 4.063980959785085112 ) ) ;
#58497 = ORIENTED_EDGE ( 'NONE', *, *, #56106, .F. ) ;
#58498 = CARTESIAN_POINT ( 'NONE',  ( -35.00000000000000000, 0.000000000000000000, 0.000000000000000000 ) ) ;
#58499 = CARTESIAN_POINT ( 'NONE',  ( 2.573738926104314650, 4.796056562246174160, 6.081632213771376527 ) ) ;
#58500 = FACE_OUTER_BOUND ( 'NONE', #7025, .T. ) ;
#58501 = EDGE_CURVE ( 'NONE', #3623, #59877, #52557, .T. ) ;
#58503 = EDGE_CURVE ( 'NONE', #62889, #33447, #23029, .T. ) ;
#58502 = CARTESIAN_POINT ( 'NONE',  ( -22.27834755396593991, -3.434702243602655081, -1.338300169228714420 ) ) ;
#58504 = CARTESIAN_POINT ( 'NONE',  ( 35.00000000000000000, 11.32068061209303167, 5.865551165830956926 ) ) ;
#58505 = DIRECTION ( 'NONE',  ( 0.000000000000000000, 0.01356324068817998940, -0.9999080150203990547 ) ) ;
#58506 = CARTESIAN_POINT ( 'NONE',  ( -27.08416813689868263, 1.467601568343278595, 1.759517419957071782 ) ) ;
#58507 = DIRECTION ( 'NONE',  ( 1.000000000000000000, -0.000000000000000000, 0.000000000000000000 ) ) ;
#58508 = CARTESIAN_POINT ( 'NONE',  ( -27.01437459610461644, -10.69338818478079922, -8.240233560378637634 ) ) ;
#58509 = CIRCLE ( 'NONE', #29795, 5.000000000000000000 ) ;
#58510 = AXIS2_PLACEMENT_3D ( 'NONE', #9310, #29596, #28965 ) ;
#58511 = EDGE_LOOP ( 'NONE', ( #1898, #25594, #4812, #1568 ) ) ;
#58512 = CARTESIAN_POINT ( 'NONE',  ( -35.00000000000000000, -2.936739658819952581, 11.37311665002362560 ) ) ;
#58513 = CIRCLE ( 'NONE', #63739, 6.936499999999988120 ) ;
#58514 = AXIS2_PLACEMENT_3D ( 'NONE', #36632, #51293, #46941 ) ;
#58515 = ORIENTED_EDGE ( 'NONE', *, *, #12809, .T. ) ;
#58516 = DIRECTION ( 'NONE',  ( -1.000000000000000000, 0.000000000000000000, 0.000000000000000000 ) ) ;
#58517 = CARTESIAN_POINT ( 'NONE',  ( 2.276198483117257254, 5.955030244776342130, -4.795748742147450727 ) ) ;
#58518 = CARTESIAN_POINT ( 'NONE',  ( 11.34652066572562568, -13.36077880898726811, -1.937500768320442157 ) ) ;
#58519 = CIRCLE ( 'NONE', #54389, 7.499999999999988454 ) ;
#58520 = CARTESIAN_POINT ( 'NONE',  ( 2.491965175173322944, 7.634639040874793281, 1.130870800982929802 ) ) ;
#58521 = ORIENTED_EDGE ( 'NONE', *, *, #23439, .T. ) ;
#58522 = CARTESIAN_POINT ( 'NONE',  ( 2.000000000000001776, 0.000000000000000000, 0.000000000000000000 ) ) ;
#58524 = CIRCLE ( 'NONE', #9644, 5.000000000000000888 ) ;
#58523 = DIRECTION ( 'NONE',  ( -1.000000000000000000, 0.000000000000000000, 0.000000000000000000 ) ) ;
#58525 = B_SPLINE_CURVE_WITH_KNOTS ( 'NONE', 3,
 ( #56014, #10454, #5500, #36043, #25767, #26101, #20775, #31077, #51387, #46376, #819, #32681, #48020, #2476, #42333, #63289, #16452, #12413, #26746 ),
 .UNSPECIFIED., .F., .F.,
 ( 4, 3, 3, 3, 3, 3, 4 ),
 ( 8.475001095641158209E-18, 4.457896483014948957E-05, 6.639290541542329700E-05, 8.820687556479254565E-05, 0.0001100173248778965173, 0.0001545671401658162494, 0.0001830328308068602031 ),
 .UNSPECIFIED. ) ;
#58526 = CARTESIAN_POINT ( 'NONE',  ( -22.27706485742869091, -2.625261754997692876, 2.580541389029905819 ) ) ;
#58527 = DIRECTION ( 'NONE',  ( -1.000000000000000000, 0.000000000000000000, 0.000000000000000000 ) ) ;
#58528 = VECTOR ( 'NONE', #735, 1000.000000000000114 ) ;
#58529 = CARTESIAN_POINT ( 'NONE',  ( -22.49803948133826381, -2.073427785788362510, 3.817825231362851568 ) ) ;
#58530 = VERTEX_POINT ( 'NONE', #22947 ) ;
#58531 = DIRECTION ( 'NONE',  ( 0.000000000000000000, 0.000000000000000000, 1.000000000000000000 ) ) ;
#58532 = AXIS2_PLACEMENT_3D ( 'NONE', #11803, #32086, #36082 ) ;
#58533 = CARTESIAN_POINT ( 'NONE',  ( 0.8320506296491612108, -8.282532257448750102, -9.275353261146616290 ) ) ;
#58534 = CARTESIAN_POINT ( 'NONE',  ( 2.241317068080778352, -3.896159243838514641, -6.565357088387215434 ) ) ;
#58535 = EDGE_CURVE ( 'NONE', #35691, #26251, #13463, .T. ) ;
#58536 = EDGE_CURVE ( 'NONE', #32724, #54875, #49894, .T. ) ;
#58537 = AXIS2_PLACEMENT_3D ( 'NONE', #27754, #2161, #44040 ) ;
#58538 = AXIS2_PLACEMENT_3D ( 'NONE', #17777, #12765, #16474 ) ;
#58539 = B_SPLINE_CURVE_WITH_KNOTS ( 'NONE', 3,
 ( #10163, #55734, #55392, #40083, #40410, #45406, #4870, #56039, #30442, #25136, #45740, #21114, #60372, #65670, #20143, #50741 ),
 .UNSPECIFIED., .F., .F.,
 ( 4, 3, 3, 3, 3, 4 ),
 ( 0.000000000000000000, 0.0002176109881720239428, 0.0004352086762394612087, 0.0006528017811446903268, 0.0007615147961451737947, 0.0009453342004947317507 ),
 .UNSPECIFIED. ) ;
#58540 = CIRCLE ( 'NONE', #60612, 12.75000000000000178 ) ;
#58541 = ORIENTED_EDGE ( 'NONE', *, *, #20166, .F. ) ;
#58542 = CARTESIAN_POINT ( 'NONE',  ( -9.843269086711673665, 12.00503757583305742, -6.187402193203074496 ) ) ;
#58543 = ORIENTED_EDGE ( 'NONE', *, *, #46880, .T. ) ;
#58544 = CARTESIAN_POINT ( 'NONE',  ( 2.256373768223201015, 5.011614056001653772, 5.765785888499388001 ) ) ;
#58545 = DIRECTION ( 'NONE',  ( 0.000000000000000000, 0.9467777615094582488, 0.3218879778915939571 ) ) ;
#58546 = AXIS2_PLACEMENT_3D ( 'NONE', #14067, #53003, #27721 ) ;
#58547 = CARTESIAN_POINT ( 'NONE',  ( 47.00000000000000711, 4.705694406421931860E-17, -3.469127814946512892E-15 ) ) ;
#58548 = CARTESIAN_POINT ( 'NONE',  ( 35.00000000000000000, 11.38112321385050585, -2.905556151562669331 ) ) ;
#58549 = LINE ( 'NONE', #33255, #47769 ) ;
#58550 = ORIENTED_EDGE ( 'NONE', *, *, #19716, .T. ) ;
#58551 = ORIENTED_EDGE ( 'NONE', *, *, #821, .F. ) ;
#58552 = VERTEX_POINT ( 'NONE', #50172 ) ;
#58553 = CARTESIAN_POINT ( 'NONE',  ( 0.3040950598368152291, 11.43390362554258921, -4.428852722102617712 ) ) ;
#58554 = AXIS2_PLACEMENT_3D ( 'NONE', #18237, #48500, #2952 ) ;
#58555 = AXIS2_PLACEMENT_3D ( 'NONE', #46006, #464, #20730 ) ;
#58556 = CYLINDRICAL_SURFACE ( 'NONE', #29977, 10.70557198542813815 ) ;
#58557 = EDGE_CURVE ( 'NONE', #3064, #11516, #46705, .T. ) ;
#58558 = ORIENTED_EDGE ( 'NONE', *, *, #61031, .F. ) ;
#58559 = DIRECTION ( 'NONE',  ( 0.000000000000000000, 0.000000000000000000, 1.000000000000000000 ) ) ;
#58560 = VECTOR ( 'NONE', #7719, 1000.000000000000227 ) ;
#58561 = CARTESIAN_POINT ( 'NONE',  ( -22.29479313954897890, -0.2707859422896734536, -3.724550806388652546 ) ) ;
#58562 = ORIENTED_EDGE ( 'NONE', *, *, #63059, .T. ) ;
#58563 = FACE_OUTER_BOUND ( 'NONE', #7952, .T. ) ;
#58564 = EDGE_CURVE ( 'NONE', #58552, #56112, #56231, .T. ) ;
#58565 = CYLINDRICAL_SURFACE ( 'NONE', #13732, 6.936499999999988120 ) ;
#58566 = CARTESIAN_POINT ( 'NONE',  ( 2.000000000000001776, 5.585096664091945939, 4.113602740025928739 ) ) ;
#58567 = VERTEX_POINT ( 'NONE', #23595 ) ;
#58568 = EDGE_LOOP ( 'NONE', ( #15404, #62595, #38948, #21966 ) ) ;
#58569 = CARTESIAN_POINT ( 'NONE',  ( 10.75853767213705225, 7.830989516993144051, 9.092612561015865680 ) ) ;
#58570 = EDGE_CURVE ( 'NONE', #26022, #26770, #37102, .T. ) ;
#58571 = VERTEX_POINT ( 'NONE', #33877 ) ;
#58572 = CARTESIAN_POINT ( 'NONE',  ( -19.12691312516887265, 11.92229376959483211, -1.407263896924768387 ) ) ;
#58573 = ORIENTED_EDGE ( 'NONE', *, *, #38439, .F. ) ;
#58574 = AXIS2_PLACEMENT_3D ( 'NONE', #65087, #64748, #14223 ) ;
#58575 = CARTESIAN_POINT ( 'NONE',  ( 0.3040950598368144520, 0.2511348647277356072, -12.25911170648142523 ) ) ;
#58576 = LINE ( 'NONE', #57587, #34093 ) ;
#58577 = DIRECTION ( 'NONE',  ( 1.000000000000000000, 0.000000000000000000, -0.000000000000000000 ) ) ;
#58578 = DIRECTION ( 'NONE',  ( 0.000000000000000000, 0.1387779952735818667, -0.9903235168508549569 ) ) ;
#58580 = EDGE_CURVE ( 'NONE', #55881, #9403, #4222, .T. ) ;
#58579 = CARTESIAN_POINT ( 'NONE',  ( 1.194176325881335599, 11.61285876598812017, -4.773862381874613092 ) ) ;
#58581 = DIRECTION ( 'NONE',  ( 0.000000000000000000, -0.01356324068817991828, 0.9999080150203990547 ) ) ;
#58582 = CARTESIAN_POINT ( 'NONE',  ( -27.73981011261383856, -10.56186010129852093, -5.703782696336726410 ) ) ;
#58583 = ORIENTED_EDGE ( 'NONE', *, *, #51164, .T. ) ;
#58584 = CARTESIAN_POINT ( 'NONE',  ( 2.258463476536644254, -7.131741622455323615, -2.740340677911303757 ) ) ;
#58585 = CIRCLE ( 'NONE', #24566, 5.000000000000000000 ) ;
#58586 = VERTEX_POINT ( 'NONE', #8948 ) ;
#58587 = CARTESIAN_POINT ( 'NONE',  ( 2.253265082352432724, -2.732639326785855971, 7.132841660187154709 ) ) ;
#58588 = ADVANCED_FACE ( 'NONE', ( #49527 ), #43678, .F. ) ;
#58589 = LINE ( 'NONE', #37632, #31933 ) ;
#58590 = CIRCLE ( 'NONE', #25665, 12.18650000000000055 ) ;
#58591 = AXIS2_PLACEMENT_3D ( 'NONE', #5466, #31370, #61295 ) ;
#58592 = ORIENTED_EDGE ( 'NONE', *, *, #6546, .F. ) ;
#58593 = FACE_OUTER_BOUND ( 'NONE', #14660, .T. ) ;
#58594 = DIRECTION ( 'NONE',  ( -1.000000000000000000, 0.000000000000000000, 0.000000000000000000 ) ) ;
#58595 = CARTESIAN_POINT ( 'NONE',  ( 2.430348790456934527, -7.544199152378932460, 1.528169972228280660 ) ) ;
#58596 = VERTEX_POINT ( 'NONE', #33566 ) ;
#58597 = CIRCLE ( 'NONE', #28801, 2.899999999999996803 ) ;
#58598 = AXIS2_PLACEMENT_3D ( 'NONE', #48044, #22778, #43034 ) ;
#58599 = VECTOR ( 'NONE', #7375, 1000.000000000000114 ) ;
#58600 = ORIENTED_EDGE ( 'NONE', *, *, #20045, .T. ) ;
#58601 = DIRECTION ( 'NONE',  ( 0.000000000000000000, -0.5987040770935561085, 0.8009703041134255130 ) ) ;
#58602 = EDGE_CURVE ( 'NONE', #55347, #62855, #34945, .T. ) ;
#58603 = EDGE_LOOP ( 'NONE', ( #27210, #23656, #25166, #23590 ) ) ;
#58604 = CARTESIAN_POINT ( 'NONE',  ( -26.25036423639542349, -12.35650188709325015, 5.438569221978448276 ) ) ;
#58605 = CARTESIAN_POINT ( 'NONE',  ( 2.241537034860907163, -1.321063441155939433, -7.519304283075094020 ) ) ;
#58606 = CARTESIAN_POINT ( 'NONE',  ( 0.2706063244538038370, -9.268878137104346493, -8.006269958070696191 ) ) ;
#58607 = CARTESIAN_POINT ( 'NONE',  ( 0.2648978790185593790, 11.55204314799269305, -4.063980959784929681 ) ) ;
#58608 = ORIENTED_EDGE ( 'NONE', *, *, #49724, .T. ) ;
#58609 = DIRECTION ( 'NONE',  ( 0.000000000000000000, -0.1387779952735677669, 0.9903235168508569553 ) ) ;
#58610 = VECTOR ( 'NONE', #45061, 1000.000000000000000 ) ;
#58611 = AXIS2_PLACEMENT_3D ( 'NONE', #43451, #8223, #48801 ) ;
#58612 = AXIS2_PLACEMENT_3D ( 'NONE', #10815, #26122, #32066 ) ;
#58613 = CARTESIAN_POINT ( 'NONE',  ( 0.2648978790185602672, 6.237101853238547378, 10.53870023327865901 ) ) ;
#58614 = B_SPLINE_CURVE_WITH_KNOTS ( 'NONE', 3,
 ( #17284, #37564, #57864, #60128, #40152, #54823, #54502, #34194, #29853, #3658, #50164, #60446, #23922, #44180, #65422, #54166, #39842, #59167, #3311, #14550 ),
 .UNSPECIFIED., .F., .F.,
 ( 4, 2, 2, 2, 2, 2, 2, 2, 2, 4 ),
 ( 0.000000000000000000, 0.0008692636490269044875, 0.001738527298053808975, 0.002173159122567255852, 0.002607790947080702512, 0.003477054596107587159, 0.004346318245134472673, 0.005215581894161356452, 0.006084845543188241099, 0.006954109192215124878 ),
 .UNSPECIFIED. ) ;
#58615 = VECTOR ( 'NONE', #47025, 1000.000000000000000 ) ;
#58616 = CARTESIAN_POINT ( 'NONE',  ( -28.56473390530001311, 3.589939350442137300, 11.45074047018220753 ) ) ;
#58617 = CARTESIAN_POINT ( 'NONE',  ( -27.08421860617808008, -0.8768262158915691717, 2.116856729767842005 ) ) ;
#58618 = PLANE ( 'NONE',  #59642 ) ;
#58619 = CARTESIAN_POINT ( 'NONE',  ( 3.849043803728001922, -10.99600197132397206, -4.807418468138718204 ) ) ;
#58620 = CARTESIAN_POINT ( 'NONE',  ( -37.00000000000000711, 11.53507381115580444, 2.216820770815288721 ) ) ;
#58621 = CIRCLE ( 'NONE', #221, 12.75000000000000178 ) ;
#58622 = EDGE_CURVE ( 'NONE', #2448, #42463, #44549, .T. ) ;
#58623 = ORIENTED_EDGE ( 'NONE', *, *, #55311, .F. ) ;
#58624 = CARTESIAN_POINT ( 'NONE',  ( 2.249013661412229581, -0.1200550008339695413, 7.636012530783589547 ) ) ;
#58625 = CIRCLE ( 'NONE', #28891, 2.899999999999994138 ) ;
#58626 = ORIENTED_EDGE ( 'NONE', *, *, #62097, .F. ) ;
#58627 = CYLINDRICAL_SURFACE ( 'NONE', #50146, 5.000000000000000888 ) ;
#58628 = CARTESIAN_POINT ( 'NONE',  ( 0.000000000000000000, -7.203928197742102135, 2.086484728383119158 ) ) ;
#58629 = CARTESIAN_POINT ( 'NONE',  ( 0.6511581176972002227, -9.263557799003038440, -8.205008037407102606 ) ) ;
#58630 = ORIENTED_EDGE ( 'NONE', *, *, #61312, .T. ) ;
#58631 = CARTESIAN_POINT ( 'NONE',  ( 2.268878695254624489, 6.544222817597994180, 3.949362208798293583 ) ) ;
#58632 = VERTEX_POINT ( 'NONE', #4633 ) ;
#58633 = DIRECTION ( 'NONE',  ( -1.000000000000000000, 0.000000000000000000, 0.000000000000000000 ) ) ;
#58634 = ORIENTED_EDGE ( 'NONE', *, *, #40071, .T. ) ;
#58635 = ORIENTED_EDGE ( 'NONE', *, *, #25393, .F. ) ;
#58636 = CARTESIAN_POINT ( 'NONE',  ( -10.89043372599972059, -7.929194153844475679, -9.011149282957994444 ) ) ;
#58637 = VECTOR ( 'NONE', #12146, 1000.000000000000114 ) ;
#58638 = CARTESIAN_POINT ( 'NONE',  ( -22.29115169517546136, -3.355084543108104889, -1.614783311161204216 ) ) ;
#58639 = VECTOR ( 'NONE', #24398, 1000.000000000000000 ) ;
#58640 = EDGE_CURVE ( 'NONE', #17330, #36274, #32540, .T. ) ;
#58641 = ORIENTED_EDGE ( 'NONE', *, *, #18269, .F. ) ;
#58642 = CARTESIAN_POINT ( 'NONE',  ( 2.573738926104372382, 5.779258037547013949, 5.156412073069302160 ) ) ;
#58643 = CARTESIAN_POINT ( 'NONE',  ( 2.770579946183331810, -2.954332771348870512, 7.230573341413142785 ) ) ;
#58644 = DIRECTION ( 'NONE',  ( -1.000000000000000000, 0.000000000000000000, 0.000000000000000000 ) ) ;
#58645 = DIRECTION ( 'NONE',  ( 0.000000000000000000, 0.000000000000000000, 1.000000000000000000 ) ) ;
#58646 = ORIENTED_EDGE ( 'NONE', *, *, #9811, .T. ) ;
#58647 = CARTESIAN_POINT ( 'NONE',  ( 0.3474126878361793458, -7.689340002166794363, 9.566300984424369602 ) ) ;
#58648 = EDGE_CURVE ( 'NONE', #56217, #10610, #19586, .T. ) ;
#58649 = CARTESIAN_POINT ( 'NONE',  ( 18.88852658721791045, -28.93036277062534012, 6.677752214540050524 ) ) ;
#58650 = CARTESIAN_POINT ( 'NONE',  ( -29.68541646480313645, -1.416020129149148543, -11.91616074890925780 ) ) ;
#58652 = ORIENTED_EDGE ( 'NONE', *, *, #33838, .F. ) ;
#58651 = CARTESIAN_POINT ( 'NONE',  ( -25.15730131298249006, 10.22820549693168246, 6.278442145667771257 ) ) ;
#58653 = LINE ( 'NONE', #49338, #31990 ) ;
#58654 = EDGE_CURVE ( 'NONE', #3120, #45709, #19084, .T. ) ;
#58655 = VERTEX_POINT ( 'NONE', #9567 ) ;
#58656 = CARTESIAN_POINT ( 'NONE',  ( -19.74705739643458102, 13.27343858888937334, -2.482339776708336387 ) ) ;
#58657 = ORIENTED_EDGE ( 'NONE', *, *, #36555, .F. ) ;
#58658 = DIRECTION ( 'NONE',  ( 0.000000000000000000, -0.9346839223284580944, 0.3554799084908867868 ) ) ;
#58659 = CARTESIAN_POINT ( 'NONE',  ( -37.00000000000000711, -1.591260454995328866, 12.08216339958900321 ) ) ;
#58660 = FACE_OUTER_BOUND ( 'NONE', #30261, .T. ) ;
#58661 = DIRECTION ( 'NONE',  ( -1.000000000000000000, 0.000000000000000000, 0.000000000000000000 ) ) ;
#58662 = AXIS2_PLACEMENT_3D ( 'NONE', #54624, #9042, #40606 ) ;
#58663 = DIRECTION ( 'NONE',  ( 0.000000000000000000, 0.000000000000000000, 1.000000000000000000 ) ) ;
#58664 = DIRECTION ( 'NONE',  ( -1.000000000000000000, 0.000000000000000000, 0.000000000000000000 ) ) ;
#58665 = CARTESIAN_POINT ( 'NONE',  ( -22.28694879868232448, -3.597828382597544117, -0.9088670759108156139 ) ) ;
#58666 = CIRCLE ( 'NONE', #14977, 12.18650000000000055 ) ;
#58667 = ORIENTED_EDGE ( 'NONE', *, *, #64698, .T. ) ;
#58668 = DIRECTION ( 'NONE',  ( 0.000000000000000000, 0.8835120444460210498, 0.4684084406997938155 ) ) ;
#58669 = VERTEX_POINT ( 'NONE', #3965 ) ;
#58670 = EDGE_CURVE ( 'NONE', #42390, #6062, #24228, .T. ) ;
#58671 = CIRCLE ( 'NONE', #45880, 250.0000000000000000 ) ;
#58672 = EDGE_CURVE ( 'NONE', #59719, #55105, #54106, .T. ) ;
#58673 = ORIENTED_EDGE ( 'NONE', *, *, #18530, .T. ) ;
#58674 = CYLINDRICAL_SURFACE ( 'NONE', #39150, 7.499999999999988454 ) ;
#58675 = CARTESIAN_POINT ( 'NONE',  ( -18.36675263200364228, -11.99999999999999289, 0.3149281170547481579 ) ) ;
#58676 = CYLINDRICAL_SURFACE ( 'NONE', #59936, 4.999999999999999112 ) ;
#58677 = CARTESIAN_POINT ( 'NONE',  ( -22.29115169517546136, 2.098196790595542094, 3.075985640626778927 ) ) ;
#58678 = ADVANCED_FACE ( 'NONE', ( #21196 ), #50497, .F. ) ;
#58679 = DIRECTION ( 'NONE',  ( 0.000000000000000000, -1.000000000000000000, 0.000000000000000000 ) ) ;
#58680 = CARTESIAN_POINT ( 'NONE',  ( 0.3665391374699465965, 11.62960183138726933, 3.952034409876336252 ) ) ;
#58681 = CARTESIAN_POINT ( 'NONE',  ( 0.3675815128205894289, -10.76447900494936327, -5.910255304480558358 ) ) ;
#58682 = EDGE_CURVE ( 'NONE', #44984, #2788, #47753, .T. ) ;
#58683 = VECTOR ( 'NONE', #56439, 1000.000000000000000 ) ;
#58684 =( BOUNDED_SURFACE ( )  B_SPLINE_SURFACE ( 3, 1, ( 
 ( #21621, #41885 ),
 ( #16625, #36895 ),
 ( #57195, #11620 ),
 ( #12589, #52211 ) ),
 .UNSPECIFIED., .F., .F., .F. ) 
 B_SPLINE_SURFACE_WITH_KNOTS ( ( 4, 4 ),
 ( 2, 2 ),
 ( 0.000000000000000000, 1.000000000000000000 ),
 ( 0.000000000000000000, 1.000000000000000000 ),
 .UNSPECIFIED. ) 
 GEOMETRIC_REPRESENTATION_ITEM ( )  RATIONAL_B_SPLINE_SURFACE ( (
 ( 1.000000000000000000, 1.000000000000000000),
 ( 0.9942764183789327692, 0.8450855930916585379),
 ( 0.9942764183789327692, 0.8450855930916585379),
 ( 1.000000000000000000, 1.000000000000000000) ) ) 
 REPRESENTATION_ITEM ( '' )  SURFACE ( )  );
#58685 = ORIENTED_EDGE ( 'NONE', *, *, #387, .T. ) ;
#58686 = CARTESIAN_POINT ( 'NONE',  ( 3.152665057733930798, -5.761241965769118067, -5.461013642405381674 ) ) ;
#58687 = ADVANCED_FACE ( 'NONE', ( #10238 ), #5266, .T. ) ;
#58688 = CARTESIAN_POINT ( 'NONE',  ( 2.258463476536646475, -5.764393264552599483, -5.014277205346519217 ) ) ;
#58689 = AXIS2_PLACEMENT_3D ( 'NONE', #22973, #47575, #2024 ) ;
#58690 = VECTOR ( 'NONE', #39715, 1000.000000000000000 ) ;
#58691 = CARTESIAN_POINT ( 'NONE',  ( -18.04458733766117362, -11.34280559204704097, 3.916728392552376370 ) ) ;
#58692 = DIRECTION ( 'NONE',  ( 0.000000000000000000, 0.5155538571770172940, 0.8568571761675919385 ) ) ;
#58693 = AXIS2_PLACEMENT_3D ( 'NONE', #18616, #38870, #43855 ) ;
#58694 = DIRECTION ( 'NONE',  ( -1.000000000000000000, 0.000000000000000000, 0.000000000000000000 ) ) ;
#58695 = CARTESIAN_POINT ( 'NONE',  ( 42.50000000000000000, -2.710505431213761085E-17, 1.201363017033314212E-18 ) ) ;
#58696 = ORIENTED_EDGE ( 'NONE', *, *, #54836, .F. ) ;
#58697 = CARTESIAN_POINT ( 'NONE',  ( -37.00000000000000711, -10.14408668126209001, -5.921969905510467314 ) ) ;
#58698 = CARTESIAN_POINT ( 'NONE',  ( 5.516018279890452902, 0.005331956019561467572, 0.004180585980734550546 ) ) ;
#58699 = DIRECTION ( 'NONE',  ( -1.000000000000000000, 0.000000000000000000, 0.000000000000000000 ) ) ;
#58700 = AXIS2_PLACEMENT_3D ( 'NONE', #20833, #35464, #40448 ) ;
#58701 = CIRCLE ( 'NONE', #2446, 12.18650000000000055 ) ;
#58702 = EDGE_CURVE ( 'NONE', #62401, #11425, #10564, .T. ) ;
#58703 = CYLINDRICAL_SURFACE ( 'NONE', #15031, 12.00000000000000000 ) ;
#58704 = CARTESIAN_POINT ( 'NONE',  ( 2.034671305879989234, -0.7032348381693109829, 11.65517003033966681 ) ) ;
#58705 = AXIS2_PLACEMENT_3D ( 'NONE', #65156, #19630, #39889 ) ;
#58706 = EDGE_LOOP ( 'NONE', ( #33602, #43563, #26979, #46027 ) ) ;
#58707 = DIRECTION ( 'NONE',  ( -1.000000000000000000, 0.000000000000000000, 0.000000000000000000 ) ) ;
#58708 = CARTESIAN_POINT ( 'NONE',  ( 0.3002738374340845895, 9.243462099800829890, 8.050654058169905980 ) ) ;
#58709 = CIRCLE ( 'NONE', #32082, 12.74999999999999822 ) ;
#58710 = DIRECTION ( 'NONE',  ( 0.000000000000000000, -0.01356324068817991828, 0.9999080150203990547 ) ) ;
#58711 = VERTEX_POINT ( 'NONE', #56457 ) ;
#58712 = DIRECTION ( 'NONE',  ( -1.000000000000000000, 0.000000000000000000, 0.000000000000000000 ) ) ;
#58713 = DIRECTION ( 'NONE',  ( -1.000000000000000000, 0.000000000000000000, 0.000000000000000000 ) ) ;
#58714 = VERTEX_POINT ( 'NONE', #15230 ) ;
#58715 = EDGE_CURVE ( 'NONE', #13694, #3037, #57292, .T. ) ;
#58716 = ORIENTED_EDGE ( 'NONE', *, *, #54500, .F. ) ;
#58717 = FACE_OUTER_BOUND ( 'NONE', #14121, .T. ) ;
#58718 = ADVANCED_FACE ( 'NONE', ( #10902 ), #40842, .T. ) ;
#58719 = ORIENTED_EDGE ( 'NONE', *, *, #16087, .T. ) ;
#58720 = CARTESIAN_POINT ( 'NONE',  ( 1.719304012339893939, -12.38166659046436457, -2.961219984258754767 ) ) ;
#58721 = CIRCLE ( 'NONE', #36391, 2.899999999999995470 ) ;
#58722 = CARTESIAN_POINT ( 'NONE',  ( 0.2646305136544065406, -9.465888453933013480, 7.770320294339142286 ) ) ;
#58723 = CARTESIAN_POINT ( 'NONE',  ( -47.00000000000000711, 0.000000000000000000, 0.000000000000000000 ) ) ;
#58724 = DIRECTION ( 'NONE',  ( -1.000000000000000000, 0.000000000000000000, 0.000000000000000000 ) ) ;
#58725 = CARTESIAN_POINT ( 'NONE',  ( -27.71501699605894231, 10.41584495806773880, -5.966219686924770116 ) ) ;
#58726 = CARTESIAN_POINT ( 'NONE',  ( 37.00000000000000711, 4.705694406421931860E-17, -3.469127814946512892E-15 ) ) ;
#58728 = ORIENTED_EDGE ( 'NONE', *, *, #3034, .F. ) ;
#58727 = DIRECTION ( 'NONE',  ( -1.000000000000000000, 0.000000000000000000, 0.000000000000000000 ) ) ;
#58729 = CARTESIAN_POINT ( 'NONE',  ( 35.00000000000000000, 9.512294188640899151, -6.891188680298859559 ) ) ;
#58730 = EDGE_CURVE ( 'NONE', #23561, #51119, #15553, .T. ) ;
#58731 = ORIENTED_EDGE ( 'NONE', *, *, #50598, .F. ) ;
#58732 = CIRCLE ( 'NONE', #42891, 6.936499999999989896 ) ;
#58733 = DIRECTION ( 'NONE',  ( 0.000000000000000000, -0.5987040770935737610, 0.8009703041134123014 ) ) ;
#58734 = ORIENTED_EDGE ( 'NONE', *, *, #11541, .T. ) ;
#58735 = ORIENTED_EDGE ( 'NONE', *, *, #46809, .F. ) ;
#58736 = CARTESIAN_POINT ( 'NONE',  ( -25.50214104994386233, 8.498208897971778697, 10.49406410904484765 ) ) ;
#58737 = CARTESIAN_POINT ( 'NONE',  ( -0.4456450841876061775, -28.11949765475245400, 13.91469577634640231 ) ) ;
#58739 = CARTESIAN_POINT ( 'NONE',  ( 47.00000000000000711, 4.705694406421931860E-17, -3.469127814946512892E-15 ) ) ;
#58738 = AXIS2_PLACEMENT_3D ( 'NONE', #56461, #26520, #46805 ) ;
#58740 = VECTOR ( 'NONE', #17393, 1000.000000000000000 ) ;
#58741 = LINE ( 'NONE', #13161, #16890 ) ;
#58742 = DIRECTION ( 'NONE',  ( 0.000000000000000000, 0.9346839223284527653, -0.3554799084909000539 ) ) ;
#58743 = PLANE ( 'NONE',  #16094 ) ;
#58744 = EDGE_LOOP ( 'NONE', ( #20395, #24751, #26819, #56004 ) ) ;
#58745 = CARTESIAN_POINT ( 'NONE',  ( -22.27722019094931127, -0.6491642780571716953, -3.623977093944210637 ) ) ;
#58746 = CARTESIAN_POINT ( 'NONE',  ( 2.280717697723838810, 5.756537207046756421, -5.034569468898497213 ) ) ;
#58747 = DIRECTION ( 'NONE',  ( 0.000000000000000000, -0.01356324068817999114, 0.9999080150203989437 ) ) ;
#58748 = ORIENTED_EDGE ( 'NONE', *, *, #24185, .F. ) ;
#58749 = CARTESIAN_POINT ( 'NONE',  ( 5.530133899448235191, -0.01536822665454943594, -0.004396748047611565534 ) ) ;
#58750 = ORIENTED_EDGE ( 'NONE', *, *, #58934, .T. ) ;
#58751 = AXIS2_PLACEMENT_3D ( 'NONE', #20308, #15325, #50590 ) ;
#58752 = DIRECTION ( 'NONE',  ( -0.000000000000000000, -0.000000000000000000, -1.000000000000000000 ) ) ;
#58753 = CARTESIAN_POINT ( 'NONE',  ( 2.903928887688355331, -7.316175791235651538, 4.835706109686327636 ) ) ;
#58754 = EDGE_CURVE ( 'NONE', #50843, #19597, #15872, .T. ) ;
#58755 = DIRECTION ( 'NONE',  ( 1.000000000000000000, 0.000000000000000000, -0.000000000000000000 ) ) ;
#58756 = CIRCLE ( 'NONE', #10983, 1.500000000000000444 ) ;
#58757 = CARTESIAN_POINT ( 'NONE',  ( -37.25000000000002132, -27.32965888902625196, 3.759436751556509915 ) ) ;
#58758 = DIRECTION ( 'NONE',  ( 0.000000000000000000, 0.9246979985058736418, 0.3807014730195186214 ) ) ;
#58759 = EDGE_CURVE ( 'NONE', #38324, #52526, #45483, .T. ) ;
#58760 = CARTESIAN_POINT ( 'NONE',  ( -9.197602943758386829, 12.97439165539572592, -3.730917860933687269 ) ) ;
#58761 = ORIENTED_EDGE ( 'NONE', *, *, #21396, .F. ) ;
#58762 = CARTESIAN_POINT ( 'NONE',  ( -19.69476066079020171, -4.201994156881551312, 25.00000000000000000 ) ) ;
#58763 = ORIENTED_EDGE ( 'NONE', *, *, #24522, .F. ) ;
#58764 = CONICAL_SURFACE ( 'NONE', #60875, 7.938172270156617749, 1.280189991382167047 ) ;
#58765 = EDGE_CURVE ( 'NONE', #16970, #45562, #50826, .T. ) ;
#58766 = DIRECTION ( 'NONE',  ( -1.000000000000000000, -0.000000000000000000, 0.000000000000000000 ) ) ;
#58767 = CARTESIAN_POINT ( 'NONE',  ( 2.717984159219948737, 4.788867404453592158, -6.148373979319133653 ) ) ;
#58768 = CARTESIAN_POINT ( 'NONE',  ( -22.00000000000000711, -20.00000000000000000, -1.499999999999998002 ) ) ;
#58769 = CARTESIAN_POINT ( 'NONE',  ( 0.000000000000000000, 0.000000000000000000, 0.000000000000000000 ) ) ;
#58770 = AXIS2_PLACEMENT_3D ( 'NONE', #3886, #44743, #49120 ) ;
#58771 = CARTESIAN_POINT ( 'NONE',  ( 0.3665391374699467075, 11.44911061034386357, 4.447929964102883993 ) ) ;
#58772 = ORIENTED_EDGE ( 'NONE', *, *, #14940, .F. ) ;
#58773 = CYLINDRICAL_SURFACE ( 'NONE', #61682, 2.899999999999994582 ) ;
#58774 = CARTESIAN_POINT ( 'NONE',  ( 8.909527563550417639, 6.491711137615684635, 10.09430667957289174 ) ) ;
#58775 = CARTESIAN_POINT ( 'NONE',  ( 2.273267844204864385, 1.476347988307471715, 7.501135923490785729 ) ) ;
#58776 = FACE_OUTER_BOUND ( 'NONE', #1616, .T. ) ;
#58777 = VERTEX_POINT ( 'NONE', #7542 ) ;
#58778 = VECTOR ( 'NONE', #49232, 1000.000000000000227 ) ;
#58779 = DIRECTION ( 'NONE',  ( 0.000000000000000000, 0.8696919319575167062, 0.4935949184179292404 ) ) ;
#58780 = DIRECTION ( 'NONE',  ( -1.000000000000000000, 0.000000000000000000, 0.000000000000000000 ) ) ;
#58781 = AXIS2_PLACEMENT_3D ( 'NONE', #23069, #49008, #44309 ) ;
#58782 = CARTESIAN_POINT ( 'NONE',  ( 0.2648978790185619880, -10.67083876753487637, -6.008231198269095685 ) ) ;
#58783 = FACE_OUTER_BOUND ( 'NONE', #62726, .T. ) ;
#58784 = AXIS2_PLACEMENT_3D ( 'NONE', #44037, #38044, #54014 ) ;
#58785 = EDGE_CURVE ( 'NONE', #25246, #45531, #22525, .T. ) ;
#58786 = CARTESIAN_POINT ( 'NONE',  ( -27.08418179957658367, -0.4604195552868174390, -2.244544746853593065 ) ) ;
#58787 = EDGE_CURVE ( 'NONE', #21888, #44528, #33928, .T. ) ;
#58788 = DIRECTION ( 'NONE',  ( -1.000000000000000000, 0.000000000000000000, -0.000000000000000000 ) ) ;
#58789 = ORIENTED_EDGE ( 'NONE', *, *, #25184, .F. ) ;
#58790 = CARTESIAN_POINT ( 'NONE',  ( -27.08419797710328325, 1.803546201758821743, -1.413289504316735501 ) ) ;
#58791 = DIRECTION ( 'NONE',  ( -0.000000000000000000, -1.000000000000000000, -0.000000000000000000 ) ) ;
#58792 = AXIS2_PLACEMENT_3D ( 'NONE', #41889, #15312, #41221 ) ;
#58793 = CARTESIAN_POINT ( 'NONE',  ( -3.416103270178013407, -31.26314776370590209, -14.19449313401761081 ) ) ;
#58794 = ORIENTED_EDGE ( 'NONE', *, *, #6617, .T. ) ;
#58795 = CARTESIAN_POINT ( 'NONE',  ( -17.71459495912815996, 3.737299794473689651, -12.97394593183730116 ) ) ;
#58796 = CARTESIAN_POINT ( 'NONE',  ( 2.889800649504073782, -5.267262008933692563, 3.118861721612547377 ) ) ;
#58797 = DIRECTION ( 'NONE',  ( -1.000000000000000000, -0.000000000000000000, 0.000000000000000000 ) ) ;
#58798 = CIRCLE ( 'NONE', #35400, 4.999999999999999112 ) ;
#58799 = EDGE_CURVE ( 'NONE', #16694, #32172, #23865, .T. ) ;
#58800 = DIRECTION ( 'NONE',  ( 0.000000000000000000, -0.01356324068817999114, 0.9999080150203989437 ) ) ;
#58801 = CARTESIAN_POINT ( 'NONE',  ( 0.3341166715381274632, -11.44035855572978733, 4.432780143632454539 ) ) ;
#58802 = ORIENTED_EDGE ( 'NONE', *, *, #36752, .T. ) ;
#58803 = DIRECTION ( 'NONE',  ( -1.000000000000000000, 0.000000000000000000, 0.000000000000000000 ) ) ;
#58804 = ORIENTED_EDGE ( 'NONE', *, *, #34120, .F. ) ;
#58805 = CARTESIAN_POINT ( 'NONE',  ( 2.241352910868909643, -7.202080440908757986, 2.532612177304417678 ) ) ;
#58806 = CARTESIAN_POINT ( 'NONE',  ( 36.00000000000000711, 12.21925492305367200, 3.640372113593418835 ) ) ;
#58807 = CARTESIAN_POINT ( 'NONE',  ( 2.931247277082684288, 7.508560300462436388, -2.338794445044915626 ) ) ;
#58808 = DIRECTION ( 'NONE',  ( -1.000000000000000000, 0.000000000000000000, 0.000000000000000000 ) ) ;
#58809 = DIRECTION ( 'NONE',  ( 1.000000000000000000, 0.000000000000000000, 0.000000000000000000 ) ) ;
#58810 = CARTESIAN_POINT ( 'NONE',  ( -35.00000000000000000, -11.73555825188280011, 4.983891302653540301 ) ) ;
#58811 = AXIS2_PLACEMENT_3D ( 'NONE', #26581, #47532, #41877 ) ;
#58812 = CARTESIAN_POINT ( 'NONE',  ( 2.245754705088792491, 5.777230445737854048, 4.993005209688604396 ) ) ;
#58813 = FACE_OUTER_BOUND ( 'NONE', #25037, .T. ) ;
#58814 = ORIENTED_EDGE ( 'NONE', *, *, #39099, .F. ) ;
#58815 = ADVANCED_FACE ( 'NONE', ( #28169 ), #27834, .T. ) ;
#58816 = EDGE_CURVE ( 'NONE', #47920, #28421, #62691, .T. ) ;
#58817 = ORIENTED_EDGE ( 'NONE', *, *, #30449, .T. ) ;
#58818 = CARTESIAN_POINT ( 'NONE',  ( 35.00000000000000000, 8.146229107149526527, 9.063649021438864750 ) ) ;
#58819 = ORIENTED_EDGE ( 'NONE', *, *, #29435, .T. ) ;
#58820 = EDGE_CURVE ( 'NONE', #62620, #33705, #52134, .T. ) ;
#58821 = DIRECTION ( 'NONE',  ( -0.3865475372811021382, 0.4442537292684497485, -0.8082200352954570510 ) ) ;
#58822 = DIRECTION ( 'NONE',  ( -1.000000000000000000, 0.000000000000000000, 0.000000000000000000 ) ) ;
#58823 = AXIS2_PLACEMENT_3D ( 'NONE', #19937, #25249, #5309 ) ;
#58824 = CARTESIAN_POINT ( 'NONE',  ( 35.00000000000000000, -3.093009498343839869, 11.78745411414842437 ) ) ;
#58825 = VERTEX_POINT ( 'NONE', #37808 ) ;
#58826 = DIRECTION ( 'NONE',  ( -1.000000000000000000, 0.000000000000000000, 0.000000000000000000 ) ) ;
#58827 = CARTESIAN_POINT ( 'NONE',  ( 2.247112776671465362, 6.554209700764031865, -3.918650674719026394 ) ) ;
#58828 = FACE_OUTER_BOUND ( 'NONE', #13421, .T. ) ;
#58829 = ORIENTED_EDGE ( 'NONE', *, *, #41723, .F. ) ;
#58830 = ORIENTED_EDGE ( 'NONE', *, *, #39399, .F. ) ;
#58831 = DIRECTION ( 'NONE',  ( 0.000000000000000000, 0.000000000000000000, 1.000000000000000000 ) ) ;
#58832 = EDGE_LOOP ( 'NONE', ( #40344, #60507, #33910, #33452 ) ) ;
#58834 = CARTESIAN_POINT ( 'NONE',  ( 5.516018279890452902, -0.006440244342253398716, 0.002104829434641079973 ) ) ;
#58833 = AXIS2_PLACEMENT_3D ( 'NONE', #28723, #40249, #60216 ) ;
#58835 = VERTEX_POINT ( 'NONE', #22862 ) ;
#58836 = ORIENTED_EDGE ( 'NONE', *, *, #51801, .T. ) ;
#58837 = DIRECTION ( 'NONE',  ( 1.000000000000000000, 0.000000000000000000, -0.000000000000000000 ) ) ;
#58838 = EDGE_CURVE ( 'NONE', #25850, #8080, #13745, .T. ) ;
#58839 = DIRECTION ( 'NONE',  ( -0.9688695217174484453, 0.000000000000000000, 0.2475719085175105139 ) ) ;
#58840 = AXIS2_PLACEMENT_3D ( 'NONE', #24320, #34929, #34616 ) ;
#58841 = CARTESIAN_POINT ( 'NONE',  ( -27.09364415740217424, -2.313349100776211920, 0.1694361397562745286 ) ) ;
#58842 = CARTESIAN_POINT ( 'NONE',  ( 0.3002738374340851446, 8.050654058169996574, -9.243462099800746401 ) ) ;
#58843 = DIRECTION ( 'NONE',  ( 0.000000000000000000, 0.7617968321374855023, 0.6478160128811972784 ) ) ;
#58844 = ADVANCED_FACE ( 'NONE', ( #42124 ), #58070, .F. ) ;
#58845 = CARTESIAN_POINT ( 'NONE',  ( 0.2872850955227719272, 11.58431228138438662, 3.994021792079137878 ) ) ;
#58846 = ORIENTED_EDGE ( 'NONE', *, *, #21244, .F. ) ;
#58847 = AXIS2_PLACEMENT_3D ( 'NONE', #51740, #46731, #1192 ) ;
#58848 = DIRECTION ( 'NONE',  ( 1.000000000000000000, 1.685093406416449860E-16, -1.011030131491573426E-17 ) ) ;
#58850 = CARTESIAN_POINT ( 'NONE',  ( -17.15625955527509916, 7.251550614233345016, 9.562613488379174242 ) ) ;
#58849 = AXIS2_PLACEMENT_3D ( 'NONE', #20868, #16551, #46468 ) ;
#58851 = CARTESIAN_POINT ( 'NONE',  ( 0.2650492594609232810, -0.1101156276917609755, 12.24562116224018560 ) ) ;
#58852 = CARTESIAN_POINT ( 'NONE',  ( 2.889800649504073782, -1.129261637821570075, -6.016320774579819286 ) ) ;
#58853 = CARTESIAN_POINT ( 'NONE',  ( -22.39032720737626647, 2.746561316202170921, -2.936932155721168503 ) ) ;
#58854 = CIRCLE ( 'NONE', #22705, 2.899999999999994582 ) ;
#58855 = CARTESIAN_POINT ( 'NONE',  ( 2.000000000000001776, 4.962980376314068742, 4.846014654777798469 ) ) ;
#58856 = CARTESIAN_POINT ( 'NONE',  ( -27.08429572838383947, 1.608131779585724619, 1.632445743623414325 ) ) ;
#58857 = CARTESIAN_POINT ( 'NONE',  ( -28.56462394502010937, 3.589878760083829334, -13.01421318288084095 ) ) ;
#58858 = CARTESIAN_POINT ( 'NONE',  ( 0.5572780756279106518, 5.905274004878355854, 10.83930267798883484 ) ) ;
#58859 = AXIS2_PLACEMENT_3D ( 'NONE', #5477, #31382, #11418 ) ;
#58860 = VERTEX_POINT ( 'NONE', #27179 ) ;
#58861 = CARTESIAN_POINT ( 'NONE',  ( 2.639814597422735609, -7.207158938903925005, -2.896050884406603743 ) ) ;
#58862 = ORIENTED_EDGE ( 'NONE', *, *, #22220, .F. ) ;
#58863 = DIRECTION ( 'NONE',  ( 0.000000000000000000, 0.000000000000000000, 1.000000000000000000 ) ) ;
#58864 = CARTESIAN_POINT ( 'NONE',  ( 2.245754705088394587, 5.920355780195151851, -4.822435078157686128 ) ) ;
#58865 = CIRCLE ( 'NONE', #25893, 1.750000000000000000 ) ;
#58866 = CARTESIAN_POINT ( 'NONE',  ( 12.19141456596091011, -11.13119688865502255, -7.646933030662562025 ) ) ;
#58867 = CARTESIAN_POINT ( 'NONE',  ( -37.00000000000000711, -1.113475361586400814, -12.70128625845194215 ) ) ;
#58868 = DIRECTION ( 'NONE',  ( 0.000000000000000000, -0.8169148498130339719, 0.5767582926624881257 ) ) ;
#58869 = ORIENTED_EDGE ( 'NONE', *, *, #19856, .F. ) ;
#58870 = CARTESIAN_POINT ( 'NONE',  ( 1.547277799339725091, 10.62321481610081086, -6.911346840320961249 ) ) ;
#58871 = DIRECTION ( 'NONE',  ( 1.000000000000000000, 0.000000000000000000, 0.000000000000000000 ) ) ;
#58872 = CARTESIAN_POINT ( 'NONE',  ( -37.00000000000000711, 0.000000000000000000, 0.000000000000000000 ) ) ;
#58873 = CARTESIAN_POINT ( 'NONE',  ( -35.00000000000000000, -11.59095880812009582, 1.903127969211145132 ) ) ;
#58874 = EDGE_CURVE ( 'NONE', #26482, #8029, #14780, .T. ) ;
#58875 = CARTESIAN_POINT ( 'NONE',  ( 35.00000000000000000, 7.608228585767871976, 10.23119532541064203 ) ) ;
#58876 =( BOUNDED_SURFACE ( )  B_SPLINE_SURFACE ( 3, 1, ( 
 ( #43380, #58722 ),
 ( #33736, #38067 ),
 ( #24102, #58373 ),
 ( #12797, #33085 ) ),
 .UNSPECIFIED., .F., .F., .F. ) 
 B_SPLINE_SURFACE_WITH_KNOTS ( ( 4, 4 ),
 ( 2, 2 ),
 ( 0.000000000000000000, 1.000000000000000000 ),
 ( 0.000000000000000000, 1.000000000000000000 ),
 .UNSPECIFIED. ) 
 GEOMETRIC_REPRESENTATION_ITEM ( )  RATIONAL_B_SPLINE_SURFACE ( (
 ( 1.000000000000000000, 1.000000000000000000),
 ( 0.9942764183789327692, 0.8450855930916580938),
 ( 0.9942764183789327692, 0.8450855930916580938),
 ( 1.000000000000000000, 1.000000000000000000) ) ) 
 REPRESENTATION_ITEM ( '' )  SURFACE ( )  );
#58877 = ORIENTED_EDGE ( 'NONE', *, *, #61672, .F. ) ;
#58878 = CARTESIAN_POINT ( 'NONE',  ( 2.969415267404130532, -0.3878973768016590884, -7.867532449842983944 ) ) ;
#58879 = CARTESIAN_POINT ( 'NONE',  ( 2.969415267403965331, 5.777543886622456881, -5.354299007565090029 ) ) ;
#58880 = CARTESIAN_POINT ( 'NONE',  ( 37.00000000000000711, 0.000000000000000000, 0.000000000000000000 ) ) ;
#58881 = VECTOR ( 'NONE', #6990, 1000.000000000000000 ) ;
#58882 = AXIS2_PLACEMENT_3D ( 'NONE', #61245, #2962, #11041 ) ;
#58883 = EDGE_CURVE ( 'NONE', #18517, #20299, #27722, .T. ) ;
#58884 = ORIENTED_EDGE ( 'NONE', *, *, #36334, .T. ) ;
#58885 = VERTEX_POINT ( 'NONE', #8859 ) ;
#58886 = CARTESIAN_POINT ( 'NONE',  ( -7.489022030332961322, 8.034049540753141372, -10.84914964302385521 ) ) ;
#58887 = ORIENTED_EDGE ( 'NONE', *, *, #18599, .T. ) ;
#58888 = DIRECTION ( 'NONE',  ( 1.000000000000000000, 0.000000000000000000, 0.000000000000000000 ) ) ;
#58889 = CARTESIAN_POINT ( 'NONE',  ( 2.941278708680199916, -0.9331242451664579773, -6.068329152486386491 ) ) ;
#58890 = CARTESIAN_POINT ( 'NONE',  ( -36.00000000000000711, -9.076753354954062658, 8.954052073409570767 ) ) ;
#58891 = DIRECTION ( 'NONE',  ( 0.000000000000000000, -0.9796553971857763221, -0.2006870767258792099 ) ) ;
#58892 = CARTESIAN_POINT ( 'NONE',  ( 1.452237505248555660, -10.06489946308196970, -7.672309600508799399 ) ) ;
#58893 = VERTEX_POINT ( 'NONE', #49452 ) ;
#58894 = EDGE_CURVE ( 'NONE', #10423, #15438, #24385, .T. ) ;
#58895 = CIRCLE ( 'NONE', #7896, 5.000000000000000888 ) ;
#58896 = VERTEX_POINT ( 'NONE', #24466 ) ;
#58897 = ORIENTED_EDGE ( 'NONE', *, *, #61080, .F. ) ;
#58898 = CARTESIAN_POINT ( 'NONE',  ( 2.241352910868909643, 7.202080440908774861, -2.532612177304371048 ) ) ;
#58899 = EDGE_CURVE ( 'NONE', #2111, #6900, #22254, .T. ) ;
#58900 = VECTOR ( 'NONE', #36189, 1000.000000000000000 ) ;
#58901 = DIRECTION ( 'NONE',  ( 0.000000000000000000, 0.6478160128811947249, -0.7617968321374878338 ) ) ;
#58902 = EDGE_LOOP ( 'NONE', ( #47665, #43346, #36998, #46913 ) ) ;
#58903 = FACE_OUTER_BOUND ( 'NONE', #5196, .T. ) ;
#58904 = CARTESIAN_POINT ( 'NONE',  ( 2.350038591458109227, -9.502240128958682419, 4.746773736939463362 ) ) ;
#58905 = ORIENTED_EDGE ( 'NONE', *, *, #37883, .F. ) ;
#58906 = CARTESIAN_POINT ( 'NONE',  ( 2.963017218115626239, 7.259628195185936939, 3.051711603120559335 ) ) ;
#58907 = CARTESIAN_POINT ( 'NONE',  ( -37.00000000000000711, 5.300372733891804522, -11.59605747147781152 ) ) ;
#58908 = DIRECTION ( 'NONE',  ( -0.000000000000000000, -0.000000000000000000, -1.000000000000000000 ) ) ;
#58909 = ORIENTED_EDGE ( 'NONE', *, *, #56323, .F. ) ;
#58910 = ORIENTED_EDGE ( 'NONE', *, *, #45906, .T. ) ;
#58911 = DIRECTION ( 'NONE',  ( 0.000000000000000000, -0.6943713148249535116, 0.7196168960969895334 ) ) ;
#58912 = ORIENTED_EDGE ( 'NONE', *, *, #34242, .F. ) ;
#58913 = DIRECTION ( 'NONE',  ( 1.000000000000000000, 0.000000000000000000, 0.000000000000000000 ) ) ;
#58914 = VERTEX_POINT ( 'NONE', #19499 ) ;
#58915 = CARTESIAN_POINT ( 'NONE',  ( 0.2653519789438754106, -4.167744179923992931, 11.51519617080779945 ) ) ;
#58916 = CYLINDRICAL_SURFACE ( 'NONE', #47883, 5.000000000000000888 ) ;
#58917 = ADVANCED_FACE ( 'NONE', ( #2909 ), #59398, .T. ) ;
#58918 = CARTESIAN_POINT ( 'NONE',  ( 2.241352910868908310, -5.901537464758421336, -4.843133558968188979 ) ) ;
#58919 = CIRCLE ( 'NONE', #16406, 5.000000000000001776 ) ;
#58920 = CARTESIAN_POINT ( 'NONE',  ( -22.27706485742869091, 3.547445275915927176, 0.9832726768967369191 ) ) ;
#58921 = CARTESIAN_POINT ( 'NONE',  ( 1.633930747254533244, 11.67150509329711028, -5.012862767615578363 ) ) ;
#58922 = CARTESIAN_POINT ( 'NONE',  ( 1.375507693218991134, -0.5913006932463059639, 12.60244951981753481 ) ) ;
#58923 = ORIENTED_EDGE ( 'NONE', *, *, #36311, .T. ) ;
#58924 = CARTESIAN_POINT ( 'NONE',  ( 2.241352910868908310, -7.145045428366559648, -2.689314586382423045 ) ) ;
#58925 = EDGE_LOOP ( 'NONE', ( #14670, #19116, #43707, #44129 ) ) ;
#58926 = CARTESIAN_POINT ( 'NONE',  ( 2.290907136833252089, -2.768669624188737632, 7.132394668149376393 ) ) ;
#58927 = CARTESIAN_POINT ( 'NONE',  ( 5.520433897694421610, 0.004666464468078041980, 0.01432141647227064968 ) ) ;
#58928 = CONICAL_SURFACE ( 'NONE', #27042, 7.938172270156617749, 1.280189991382167047 ) ;
#58929 = VERTEX_POINT ( 'NONE', #19159 ) ;
#58930 = CARTESIAN_POINT ( 'NONE',  ( 47.00000000000000711, 4.705694406421931860E-17, -3.469127814946512892E-15 ) ) ;
#58931 = FACE_OUTER_BOUND ( 'NONE', #42309, .T. ) ;
#58932 = CARTESIAN_POINT ( 'NONE',  ( 0.2767916011545376032, -2.313848297676370347, -12.02950149294536430 ) ) ;
#58934 = EDGE_CURVE ( 'NONE', #61089, #9977, #30740, .T. ) ;
#58933 = VERTEX_POINT ( 'NONE', #44746 ) ;
#58935 = ORIENTED_EDGE ( 'NONE', *, *, #23576, .F. ) ;
#58936 = CARTESIAN_POINT ( 'NONE',  ( 2.430348790457596664, -6.761480562106405579, -3.678671624790093464 ) ) ;
#58937 = ORIENTED_EDGE ( 'NONE', *, *, #54120, .F. ) ;
#58938 = CARTESIAN_POINT ( 'NONE',  ( -24.95335564517041149, -11.81240985965305512, 6.538156315917978745 ) ) ;
#58939 = CARTESIAN_POINT ( 'NONE',  ( -4.045980568306387859, -9.337516854300243807, 7.540689691057082200 ) ) ;
#58940 = DIRECTION ( 'NONE',  ( 0.000000000000000000, 0.000000000000000000, 1.000000000000000000 ) ) ;
#58941 = CARTESIAN_POINT ( 'NONE',  ( 37.00000000000000711, 5.636262487437473823, 10.80478261802175233 ) ) ;
#58942 = CARTESIAN_POINT ( 'NONE',  ( -35.00000000000000000, 11.60979404548639948, -3.704519465651187282 ) ) ;
#58943 = AXIS2_PLACEMENT_3D ( 'NONE', #5674, #35573, #55867 ) ;
#58944 = ORIENTED_EDGE ( 'NONE', *, *, #44600, .F. ) ;
#58945 = CYLINDRICAL_SURFACE ( 'NONE', #14651, 4.999999999999999112 ) ;
#58946 = CIRCLE ( 'NONE', #44020, 4.999999999999999112 ) ;
#58947 = EDGE_CURVE ( 'NONE', #64141, #34055, #11623, .T. ) ;
#58948 = CARTESIAN_POINT ( 'NONE',  ( 2.000000000000001776, 2.562706407243739992, -6.312399813420325856 ) ) ;
#58949 = LINE ( 'NONE', #52637, #58599 ) ;
#58950 = CARTESIAN_POINT ( 'NONE',  ( -27.08423923533013422, -0.8983804370399710582, 2.107995711831558872 ) ) ;
#58951 = ADVANCED_FACE ( 'NONE', ( #53771 ), #59733, .T. ) ;
#58952 = FACE_OUTER_BOUND ( 'NONE', #34881, .T. ) ;
#58953 = LINE ( 'NONE', #23689, #13419 ) ;
#58954 = CARTESIAN_POINT ( 'NONE',  ( -36.00000000000000711, -0.4871980014162358152, 12.74068829017553739 ) ) ;
#58955 = ADVANCED_FACE ( 'NONE', ( #18193 ), #64057, .T. ) ;
#58956 = VERTEX_POINT ( 'NONE', #38463 ) ;
#58957 = CARTESIAN_POINT ( 'NONE',  ( -22.71097035706202760, 2.118550233809425087, 4.510116093748266053 ) ) ;
#58958 = ORIENTED_EDGE ( 'NONE', *, *, #62800, .F. ) ;
#58959 = CARTESIAN_POINT ( 'NONE',  ( 0.2915757698887304072, 1.916267336493336693, -12.10419100255477076 ) ) ;
#58960 = CARTESIAN_POINT ( 'NONE',  ( -28.66013792860432119, -1.770123732198272570, -0.4872053345172134842 ) ) ;
#58961 = CARTESIAN_POINT ( 'NONE',  ( 8.937200413559443390, 4.476360154859203355, -12.73625532737111143 ) ) ;
#58962 = ORIENTED_EDGE ( 'NONE', *, *, #64914, .F. ) ;
#58963 = CARTESIAN_POINT ( 'NONE',  ( 22.88594695219327235, 3.421158645304719137, -13.05931366970166962 ) ) ;
#58964 = ORIENTED_EDGE ( 'NONE', *, *, #52622, .F. ) ;
#58965 = PRESENTATION_LAYER_ASSIGNMENT (  '', '', ( #48331 ) ) ;
#58966 = ORIENTED_EDGE ( 'NONE', *, *, #61952, .F. ) ;
#58967 = VERTEX_POINT ( 'NONE', #44407 ) ;
#58968 = CARTESIAN_POINT ( 'NONE',  ( 29.73149305502989392, -9.424759817252279959, 9.675963828540520950 ) ) ;
#58969 = CARTESIAN_POINT ( 'NONE',  ( -22.29677679919927868, -3.364642266483117705, -1.633785040807715250 ) ) ;
#58970 = ORIENTED_EDGE ( 'NONE', *, *, #4211, .T. ) ;
#58971 = EDGE_CURVE ( 'NONE', #63621, #31648, #55146, .T. ) ;
#58972 = DIRECTION ( 'NONE',  ( -1.000000000000000000, -0.000000000000000000, 0.000000000000000000 ) ) ;
#58973 = CARTESIAN_POINT ( 'NONE',  ( 2.705197763288547108, -2.925192046931958778, 7.218866228162280407 ) ) ;
#58974 = CARTESIAN_POINT ( 'NONE',  ( -35.00000000000000000, 4.946702696913171771, 11.13736569743276306 ) ) ;
#58975 = CARTESIAN_POINT ( 'NONE',  ( 17.38697840126492622, 10.06593862365382464, 6.600811317301616299 ) ) ;
#58976 = VERTEX_POINT ( 'NONE', #14160 ) ;
#58977 = CIRCLE ( 'NONE', #23936, 12.18649999999999700 ) ;
#58978 = CYLINDRICAL_SURFACE ( 'NONE', #21391, 5.000000000000000888 ) ;
#58979 = CARTESIAN_POINT ( 'NONE',  ( 35.00000000000000000, 4.705694406421931860E-17, -3.469127814946512892E-15 ) ) ;
#58980 = DIRECTION ( 'NONE',  ( -1.000000000000000000, 0.000000000000000000, 0.000000000000000000 ) ) ;
#58982 = VERTEX_POINT ( 'NONE', #55057 ) ;
#58981 = CARTESIAN_POINT ( 'NONE',  ( 1.000000000000000888, -6.997684042076877553, -2.698595569414293127 ) ) ;
#58983 = CARTESIAN_POINT ( 'NONE',  ( -35.00000000000000000, 8.295159312811854591, 8.927548052240926069 ) ) ;
#58984 = ORIENTED_EDGE ( 'NONE', *, *, #33870, .F. ) ;
#58985 = CARTESIAN_POINT ( 'NONE',  ( 0.2647959493198543401, -6.249846955854195585, -10.53111783886897612 ) ) ;
#58986 = ORIENTED_EDGE ( 'NONE', *, *, #65525, .T. ) ;
#58987 = CARTESIAN_POINT ( 'NONE',  ( 37.00000000000000711, -7.094637218249427946, -10.59380114696467778 ) ) ;
#58988 = CARTESIAN_POINT ( 'NONE',  ( 0.2767916011545388244, 4.010899340181579120, -11.57477803659169169 ) ) ;
#58989 = AXIS2_PLACEMENT_3D ( 'NONE', #55611, #60921, #14674 ) ;
#58990 = CARTESIAN_POINT ( 'NONE',  ( 5.516018279890452902, 0.002104829434641014487, 0.006440244342253419532 ) ) ;
#58991 = DIRECTION ( 'NONE',  ( -1.000000000000000000, -0.000000000000000000, 0.000000000000000000 ) ) ;
#58992 = CARTESIAN_POINT ( 'NONE',  ( 0.3675815128205894289, 9.574637318041965273, 7.689697408877307794 ) ) ;
#58993 = CARTESIAN_POINT ( 'NONE',  ( -10.39032328888078105, -5.036169502593281777, -12.53141698666758685 ) ) ;
#58994 = CARTESIAN_POINT ( 'NONE',  ( 0.000000000000000000, -3.073484823194374993, 6.841322316745024779 ) ) ;
#58995 = ORIENTED_EDGE ( 'NONE', *, *, #9556, .T. ) ;
#58996 = DIRECTION ( 'NONE',  ( 0.000000000000000000, 0.01356324068817998940, -0.9999080150203989437 ) ) ;
#58997 = ORIENTED_EDGE ( 'NONE', *, *, #44146, .F. ) ;
#58998 = VERTEX_POINT ( 'NONE', #44106 ) ;
#58999 = CARTESIAN_POINT ( 'NONE',  ( -35.00000000000000000, -6.303578524886872536, -10.42955799785326576 ) ) ;
#59000 = CARTESIAN_POINT ( 'NONE',  ( -17.54726996257253191, -11.36053454945672136, 3.865003848717349033 ) ) ;
#59001 = CARTESIAN_POINT ( 'NONE',  ( 2.941278708680199916, 0.1348063076486946399, 6.138172921908581436 ) ) ;
#59002 = FACE_OUTER_BOUND ( 'NONE', #12003, .T. ) ;
#59003 = EDGE_CURVE ( 'NONE', #65768, #11428, #26474, .T. ) ;
#59004 = CYLINDRICAL_SURFACE ( 'NONE', #10685, 5.000000000000000888 ) ;
#59005 = AXIS2_PLACEMENT_3D ( 'NONE', #11071, #12033, #56629 ) ;
#59006 = B_SPLINE_CURVE_WITH_KNOTS ( 'NONE', 3,
 ( #48654, #58975, #23717, #13068, #8740, #8089, #43641, #29022, #42990, #28356, #28042, #63266, #13386, #33671 ),
 .UNSPECIFIED., .F., .F.,
 ( 4, 2, 2, 2, 2, 2, 4 ),
 ( 1.701886623846052835E-17, 0.002810228430025432916, 0.004215342645038138748, 0.005620456860050845882, 0.007025571075063551281, 0.008430685290076256680, 0.01124091372010166921 ),
 .UNSPECIFIED. ) ;
#59007 = FACE_OUTER_BOUND ( 'NONE', #22984, .T. ) ;
#59008 = VERTEX_POINT ( 'NONE', #8520 ) ;
#59009 = CARTESIAN_POINT ( 'NONE',  ( 35.00000000000000000, -5.246972444133939817, 10.99909370905162298 ) ) ;
#59010 = CARTESIAN_POINT ( 'NONE',  ( 2.268878695253356614, -5.759001817705827975, -5.025754889199108177 ) ) ;
#59011 = DIRECTION ( 'NONE',  ( 0.000000000000000000, -0.01356324068817998940, 0.9999080150203990547 ) ) ;
#59012 = CARTESIAN_POINT ( 'NONE',  ( 3.152665057734040488, 0.000000000000000000, 0.000000000000000000 ) ) ;
#59013 = CARTESIAN_POINT ( 'NONE',  ( 2.080613030138688480, 5.400000000000000355, -1.000000000000000000 ) ) ;
#59014 = ADVANCED_FACE ( 'NONE', ( #58776 ), #28475, .T. ) ;
#59015 = AXIS2_PLACEMENT_3D ( 'NONE', #50425, #60713, #9831 ) ;
#59016 = CARTESIAN_POINT ( 'NONE',  ( -9.053705415859559125, -2.444157173645027381, 13.27951883727767246 ) ) ;
#59017 = ADVANCED_FACE ( 'NONE', ( #39105 ), #34108, .T. ) ;
#59018 = CARTESIAN_POINT ( 'NONE',  ( -9.443643884643755371, -3.548096057925545388, 13.02630244985499353 ) ) ;
#59019 = ADVANCED_FACE ( 'NONE', ( #26046 ), #1167, .F. ) ;
#59020 = ORIENTED_EDGE ( 'NONE', *, *, #22438, .F. ) ;
#59021 = DIRECTION ( 'NONE',  ( 0.3865475372811021382, -0.4778122177792148983, 0.7888450329201692757 ) ) ;
#59022 = LINE ( 'NONE', #13434, #28285 ) ;
#59023 = DIRECTION ( 'NONE',  ( 1.000000000000000000, -0.000000000000000000, 0.000000000000000000 ) ) ;
#59024 = EDGE_CURVE ( 'NONE', #56049, #51886, #57283, .T. ) ;
#59025 = CARTESIAN_POINT ( 'NONE',  ( -36.00000000000000711, -10.84030624090602046, -6.711949091238257559 ) ) ;
#59026 = CARTESIAN_POINT ( 'NONE',  ( -37.00000000000000711, 11.65150730582932503, 1.488153103997165605 ) ) ;
#59027 = ORIENTED_EDGE ( 'NONE', *, *, #15319, .F. ) ;
#59028 = CARTESIAN_POINT ( 'NONE',  ( 0.2646305136544065406, -10.67138229758233692, 6.008537389229378967 ) ) ;
#59029 = EDGE_CURVE ( 'NONE', #50088, #32109, #39405, .T. ) ;
#59030 = CARTESIAN_POINT ( 'NONE',  ( -9.603270190229855174, -9.180294942608449915, -7.739257472663321202 ) ) ;
#59031 = DIRECTION ( 'NONE',  ( -1.000000000000000000, -0.000000000000000000, -0.000000000000000000 ) ) ;
#59032 = ORIENTED_EDGE ( 'NONE', *, *, #60632, .F. ) ;
#59033 = CARTESIAN_POINT ( 'NONE',  ( -10.48620311856347875, -9.720786832536937538, 9.367833439828908482 ) ) ;
#59034 = CARTESIAN_POINT ( 'NONE',  ( 5.536195898058073439, 0.005656495196970996904, 0.006344799443924045018 ) ) ;
#59035 = EDGE_LOOP ( 'NONE', ( #7780, #55776, #608, #56980 ) ) ;
#59036 = ORIENTED_EDGE ( 'NONE', *, *, #57655, .F. ) ;
#59037 = CARTESIAN_POINT ( 'NONE',  ( -37.00000000000000711, -11.24036214326516436, -6.018036132182280618 ) ) ;
#59038 = EDGE_CURVE ( 'NONE', #15001, #11288, #49872, .T. ) ;
#59039 = AXIS2_PLACEMENT_3D ( 'NONE', #38793, #43778, #53446 ) ;
#59040 = ORIENTED_EDGE ( 'NONE', *, *, #22270, .F. ) ;
#59041 = EDGE_CURVE ( 'NONE', #2269, #34549, #11660, .T. ) ;
#59042 = CARTESIAN_POINT ( 'NONE',  ( -37.00000000000000711, 0.000000000000000000, 0.000000000000000000 ) ) ;
#59043 = CARTESIAN_POINT ( 'NONE',  ( 0.2651627923886339944, 6.199207987242239426, -10.56116046379966811 ) ) ;
#59045 = FACE_OUTER_BOUND ( 'NONE', #22487, .T. ) ;
#59044 =( BOUNDED_CURVE ( )  B_SPLINE_CURVE ( 3, ( #7720, #12680, #47956, #62562 ),
 .UNSPECIFIED., .F., .F. ) 
 B_SPLINE_CURVE_WITH_KNOTS ( ( 4, 4 ),
 ( 0.4415372860933093335, 0.5130637748270454601 ),
 .UNSPECIFIED. ) 
 CURVE ( )  GEOMETRIC_REPRESENTATION_ITEM ( )  RATIONAL_B_SPLINE_CURVE ( ( 1.000000000000000000, 0.9995737088895612077, 0.9995737088895612077, 1.000000000000000000 ) ) 
 REPRESENTATION_ITEM ( '' )  );
#59046 = DIRECTION ( 'NONE',  ( 1.000000000000000000, 0.000000000000000000, -0.000000000000000000 ) ) ;
#59047 = EDGE_CURVE ( 'NONE', #30510, #23409, #51972, .T. ) ;
#59048 = FACE_OUTER_BOUND ( 'NONE', #48944, .T. ) ;
#59050 = ORIENTED_EDGE ( 'NONE', *, *, #20872, .F. ) ;
#59049 = DIRECTION ( 'NONE',  ( 0.4826047536471247956, 0.8758382566188793739, -0.000000000000000000 ) ) ;
#59051 = CARTESIAN_POINT ( 'NONE',  ( 5.515539859299206427, -0.005924322247675101009, 0.001241880655086994309 ) ) ;
#59052 = ORIENTED_EDGE ( 'NONE', *, *, #23266, .F. ) ;
#59053 = CARTESIAN_POINT ( 'NONE',  ( 0.2653141334712571520, 10.58342934917120637, -6.161213243425151198 ) ) ;
#59054 = VERTEX_POINT ( 'NONE', #21372 ) ;
#59055 = ORIENTED_EDGE ( 'NONE', *, *, #60548, .F. ) ;
#59056 = CARTESIAN_POINT ( 'NONE',  ( -18.58686583997218378, 5.410928820688530649, 12.37136992127100932 ) ) ;
#59057 = CARTESIAN_POINT ( 'NONE',  ( -13.72965000697191584, -28.58137455677819361, 12.42479717943507822 ) ) ;
#59058 = CARTESIAN_POINT ( 'NONE',  ( -24.38047113150638268, 9.758145127762370308, 9.337300561328881088 ) ) ;
#59059 = CARTESIAN_POINT ( 'NONE',  ( -37.00000000000000711, 12.54989509947650994, 2.250029553613800637 ) ) ;
#59060 = AXIS2_PLACEMENT_3D ( 'NONE', #46610, #1407, #37623 ) ;
#59061 = CARTESIAN_POINT ( 'NONE',  ( 2.305787727787083519, -7.135468203930003028, 2.774453000917123990 ) ) ;
#59062 = DIRECTION ( 'NONE',  ( -1.000000000000000000, -0.000000000000000000, 0.000000000000000000 ) ) ;
#59063 = VERTEX_POINT ( 'NONE', #24811 ) ;
#59064 = CARTESIAN_POINT ( 'NONE',  ( -22.27711653538342773, 0.4190680140413665655, 3.657713416444722920 ) ) ;
#59065 =( BOUNDED_SURFACE ( )  B_SPLINE_SURFACE ( 3, 1, ( 
 ( #65746, #34529 ),
 ( #4629, #5264 ),
 ( #65431, #25532 ),
 ( #30513, #54508 ) ),
 .UNSPECIFIED., .F., .F., .F. ) 
 B_SPLINE_SURFACE_WITH_KNOTS ( ( 4, 4 ),
 ( 2, 2 ),
 ( 0.000000000000000000, 1.000000000000000000 ),
 ( 0.000000000000000000, 1.000000000000000000 ),
 .UNSPECIFIED. ) 
 GEOMETRIC_REPRESENTATION_ITEM ( )  RATIONAL_B_SPLINE_SURFACE ( (
 ( 1.000000000000000000, 1.000000000000000000),
 ( 0.6933888150995267674, 0.9895912004443193632),
 ( 0.6933888150995267674, 0.9895912004443193632),
 ( 1.000000000000000000, 1.000000000000000000) ) ) 
 REPRESENTATION_ITEM ( '' )  SURFACE ( )  );
#59066 = CARTESIAN_POINT ( 'NONE',  ( 35.00000000000000000, -11.65150730582935523, -1.488153103996925797 ) ) ;
#59067 = CARTESIAN_POINT ( 'NONE',  ( -35.00000000000000000, -12.15823808070322087, -0.8294751490780611913 ) ) ;
#59068 = ORIENTED_EDGE ( 'NONE', *, *, #10484, .F. ) ;
#59069 = DIRECTION ( 'NONE',  ( -1.000000000000000000, 0.000000000000000000, 0.000000000000000000 ) ) ;
#59070 = VERTEX_POINT ( 'NONE', #35985 ) ;
#59071 = CARTESIAN_POINT ( 'NONE',  ( 2.305787727787084407, -7.508843116234166004, 1.493241775258399073 ) ) ;
#59072 = CARTESIAN_POINT ( 'NONE',  ( 0.2706063244538025603, -10.51833723927417807, -6.275112929891721869 ) ) ;
#59073 = CARTESIAN_POINT ( 'NONE',  ( 35.00000000000000000, 7.971186206369472060, -9.217970097227754067 ) ) ;
#59074 = AXIS2_PLACEMENT_3D ( 'NONE', #16754, #37027, #58317 ) ;
#59075 = CARTESIAN_POINT ( 'NONE',  ( -22.28023996335807411, 3.022323476748291604, -2.118259050016077616 ) ) ;
#59076 = EDGE_CURVE ( 'NONE', #36481, #34717, #20725, .T. ) ;
#59077 = CARTESIAN_POINT ( 'NONE',  ( -37.25000000000000711, -27.21021009056489248, -4.500000000000000888 ) ) ;
#59078 = DIRECTION ( 'NONE',  ( 0.000000000000000000, -0.8169148498130338609, 0.5767582926624880146 ) ) ;
#59079 = CARTESIAN_POINT ( 'NONE',  ( -7.489022030332961322, -8.034049540753116503, -10.84914964302385521 ) ) ;
#59080 = ORIENTED_EDGE ( 'NONE', *, *, #1062, .T. ) ;
#59081 = ORIENTED_EDGE ( 'NONE', *, *, #28374, .T. ) ;
#59082 = CARTESIAN_POINT ( 'NONE',  ( 0.8375941296792225321, 3.890418817178149524, 11.81283813871825750 ) ) ;
#59083 = CYLINDRICAL_SURFACE ( 'NONE', #24432, 5.000000000000000888 ) ;
#59084 = ADVANCED_FACE ( 'NONE', ( #41310 ), #27023, .T. ) ;
#59085 = CARTESIAN_POINT ( 'NONE',  ( 0.2652384529303135619, -11.53005674806959746, -4.126283314267688240 ) ) ;
#59086 = CARTESIAN_POINT ( 'NONE',  ( -18.10791796330941850, -9.538085361946238905, -7.283445145555471179 ) ) ;
#59087 = ADVANCED_FACE ( 'NONE', ( #61278 ), #3314, .F. ) ;
#59089 = B_SPLINE_CURVE_WITH_KNOTS ( 'NONE', 3,
 ( #29446, #34102, #54081, #23163, #38790, #53764, #49445 ),
 .UNSPECIFIED., .F., .F.,
 ( 4, 3, 4 ),
 ( 0.000000000000000000, 0.001700533616330539939, 0.005002426799371323396 ),
 .UNSPECIFIED. ) ;
#59088 = CARTESIAN_POINT ( 'NONE',  ( -37.00000000000000711, 12.74613886779085448, -0.3137578094507852411 ) ) ;
#59090 = CARTESIAN_POINT ( 'NONE',  ( -47.00000000000000711, 0.000000000000000000, 0.000000000000000000 ) ) ;
#59091 = LINE ( 'NONE', #27831, #56770 ) ;
#59092 = DIRECTION ( 'NONE',  ( 0.000000000000000000, 0.000000000000000000, 1.000000000000000000 ) ) ;
#59093 = CARTESIAN_POINT ( 'NONE',  ( -37.00000000000000711, 0.000000000000000000, 0.000000000000000000 ) ) ;
#59094 = EDGE_CURVE ( 'NONE', #15359, #61567, #38233, .T. ) ;
#59095 = ORIENTED_EDGE ( 'NONE', *, *, #6692, .T. ) ;
#59096 = CARTESIAN_POINT ( 'NONE',  ( 0.2648978790185584908, 12.03635331166812250, 2.256510822326184940 ) ) ;
#59097 = CARTESIAN_POINT ( 'NONE',  ( 19.09841239469957941, 7.043214802939539609, 11.53926296509304450 ) ) ;
#59098 = CARTESIAN_POINT ( 'NONE',  ( 37.00000000000000711, 0.3025107581131208367, -11.74226168163341555 ) ) ;
#59099 = LINE ( 'NONE', #15065, #29571 ) ;
#59100 = AXIS2_PLACEMENT_3D ( 'NONE', #50032, #14432, #20421 ) ;
#59101 = DIRECTION ( 'NONE',  ( -1.000000000000000000, 0.000000000000000000, 0.000000000000000000 ) ) ;
#59102 = CARTESIAN_POINT ( 'NONE',  ( -27.67949680227653175, -8.923181436745910133, -8.045965622785404392 ) ) ;
#59103 = CIRCLE ( 'NONE', #44225, 5.000000000000000888 ) ;
#59104 = ORIENTED_EDGE ( 'NONE', *, *, #42947, .F. ) ;
#59105 = CARTESIAN_POINT ( 'NONE',  ( 2.266490820343225021, -2.476945027124318521, 7.230273269342697873 ) ) ;
#59106 = CARTESIAN_POINT ( 'NONE',  ( 0.3665391374699465965, 10.76665847464312442, 5.911453292029641204 ) ) ;
#59107 = EDGE_CURVE ( 'NONE', #37744, #35944, #7373, .T. ) ;
#59108 = CARTESIAN_POINT ( 'NONE',  ( -4.254071763051084254, -31.39562805149797597, -14.04524613008041811 ) ) ;
#59109 = ORIENTED_EDGE ( 'NONE', *, *, #40335, .F. ) ;
#59110 = CARTESIAN_POINT ( 'NONE',  ( 1.000000000000000888, -4.472310526050796931, 6.020667617347345235 ) ) ;
#59111 = DIRECTION ( 'NONE',  ( 0.000000000000000000, -0.01356324068817998940, 0.9999080150203990547 ) ) ;
#59112 = LINE ( 'NONE', #23524, #56354 ) ;
#59113 = ADVANCED_FACE ( 'NONE', ( #38291 ), #48315, .T. ) ;
#59114 = CARTESIAN_POINT ( 'NONE',  ( 0.3106921474978429076, -8.060345844326345599, 9.239619355094122355 ) ) ;
#59115 = CARTESIAN_POINT ( 'NONE',  ( -9.351388602708162523, -12.99278190472486827, -3.665735721005250358 ) ) ;
#59116 = EDGE_CURVE ( 'NONE', #45883, #12635, #5444, .T. ) ;
#59117 = CARTESIAN_POINT ( 'NONE',  ( 2.000000000000001776, 4.962980376314141573, -4.846014654777754060 ) ) ;
#59118 = EDGE_CURVE ( 'NONE', #7370, #62374, #65738, .T. ) ;
#59119 = ORIENTED_EDGE ( 'NONE', *, *, #9835, .T. ) ;
#59120 = DIRECTION ( 'NONE',  ( -1.000000000000000000, 0.000000000000000000, 0.000000000000000000 ) ) ;
#59121 = LINE ( 'NONE', #44131, #31920 ) ;
#59122 = CARTESIAN_POINT ( 'NONE',  ( 3.152665057734040488, 0.000000000000000000, 0.000000000000000000 ) ) ;
#59123 = DIRECTION ( 'NONE',  ( 0.000000000000000000, -0.4198891015602717602, 0.9075754196709537869 ) ) ;
#59124 = CARTESIAN_POINT ( 'NONE',  ( 2.941278708680199916, 2.952340773940109298, 5.383216837018951040 ) ) ;
#59125 = CARTESIAN_POINT ( 'NONE',  ( 2.241506898688419458, -3.783130304541474587, 6.631235260227153816 ) ) ;
#59126 = EDGE_CURVE ( 'NONE', #16453, #33841, #5323, .T. ) ;
#59127 = CARTESIAN_POINT ( 'NONE',  ( -22.71097035706202405, 4.089776368546564456, 2.846599994298306679 ) ) ;
#59128 = FACE_OUTER_BOUND ( 'NONE', #62971, .T. ) ;
#59129 = VERTEX_POINT ( 'NONE', #58613 ) ;
#59130 = ORIENTED_EDGE ( 'NONE', *, *, #43211, .F. ) ;
#59131 = ORIENTED_EDGE ( 'NONE', *, *, #30281, .T. ) ;
#59132 =( NAMED_UNIT ( * ) PLANE_ANGLE_UNIT ( ) SI_UNIT ( $, .RADIAN. ) );
#59133 = CARTESIAN_POINT ( 'NONE',  ( -27.10719052120871098, -0.1538293304135310291, -2.355164825213519109 ) ) ;
#59134 = CARTESIAN_POINT ( 'NONE',  ( 2.827825597296806492, -8.650999012440189873, 2.568788224597731595 ) ) ;
#59135 = CARTESIAN_POINT ( 'NONE',  ( -35.00000000000000000, -4.237174932027140350, -12.02534193257725548 ) ) ;
#59136 = ORIENTED_EDGE ( 'NONE', *, *, #62219, .F. ) ;
#59137 = DIRECTION ( 'NONE',  ( -1.000000000000000000, 0.000000000000000000, -0.000000000000000000 ) ) ;
#59138 = CARTESIAN_POINT ( 'NONE',  ( 2.242418902651939661, 6.561482094363304540, -3.903399295463767515 ) ) ;
#59139 = CARTESIAN_POINT ( 'NONE',  ( 2.297017764050237165, -5.044319338147413845, -5.755222757172084869 ) ) ;
#59140 = ORIENTED_EDGE ( 'NONE', *, *, #64446, .F. ) ;
#59141 = VERTEX_POINT ( 'NONE', #32967 ) ;
#59142 = FACE_BOUND ( 'NONE', #49732, .T. ) ;
#59143 = CARTESIAN_POINT ( 'NONE',  ( -35.00000000000000000, 10.64792938439755332, 5.927257550915355999 ) ) ;
#59144 = EDGE_LOOP ( 'NONE', ( #7097, #46316, #39653, #23883, #24069, #63649, #13860, #60327, #64967, #32358, #52109, #9026 ) ) ;
#59145 = VECTOR ( 'NONE', #31954, 1000.000000000000000 ) ;
#59146 = ORIENTED_EDGE ( 'NONE', *, *, #53397, .T. ) ;
#59147 = CARTESIAN_POINT ( 'NONE',  ( 5.514970785353741078, 0.004233694591582952416, 0.002093325033903827709 ) ) ;
#59148 = CARTESIAN_POINT ( 'NONE',  ( -27.08776759928997180, -1.611072893085645275, 1.644157618165822621 ) ) ;
#59149 = EDGE_CURVE ( 'NONE', #9981, #14466, #5489, .T. ) ;
#59150 = CARTESIAN_POINT ( 'NONE',  ( 0.3610902822527243816, 10.49957835860572430, -6.364812822043059981 ) ) ;
#59151 = DIRECTION ( 'NONE',  ( 0.000000000000000000, 0.4698238015817303159, 0.8827602140260348840 ) ) ;
#59152 = FACE_OUTER_BOUND ( 'NONE', #18107, .T. ) ;
#59153 = DIRECTION ( 'NONE',  ( -1.000000000000000000, -0.000000000000000000, -0.000000000000000000 ) ) ;
#59154 = EDGE_CURVE ( 'NONE', #41809, #56943, #28657, .T. ) ;
#59155 = EDGE_LOOP ( 'NONE', ( #33313, #49538, #55921, #19096 ) ) ;
#59156 = CARTESIAN_POINT ( 'NONE',  ( 2.251139882113958102, -1.448366094935465531, 7.499076289418100671 ) ) ;
#59157 = CARTESIAN_POINT ( 'NONE',  ( -37.00000000000000711, 9.821084925794570708, 7.215058775251291578 ) ) ;
#59158 = CARTESIAN_POINT ( 'NONE',  ( 0.2651627682582933243, -9.324228491541576958, 7.938957913267723931 ) ) ;
#59159 = CARTESIAN_POINT ( 'NONE',  ( 37.00000000000000711, -11.44858830469738109, 2.627174906297032209 ) ) ;
#59160 = CARTESIAN_POINT ( 'NONE',  ( 2.000000000000001776, 0.000000000000000000, 0.000000000000000000 ) ) ;
#59161 = CARTESIAN_POINT ( 'NONE',  ( -27.09030469827931853, 1.608164674722576848, -1.657623467486017299 ) ) ;
#59162 = LINE ( 'NONE', #49194, #2213 ) ;
#59163 = FACE_OUTER_BOUND ( 'NONE', #2067, .T. ) ;
#59164 = ADVANCED_FACE ( 'NONE', ( #14979 ), #34612, .F. ) ;
#59165 = DIRECTION ( 'NONE',  ( -0.5244426074294280538, 0.000000000000000000, 0.8514458006899926490 ) ) ;
#59166 = ORIENTED_EDGE ( 'NONE', *, *, #1748, .T. ) ;
#59167 = CARTESIAN_POINT ( 'NONE',  ( -18.55539683905438864, 5.671985714705006565, -10.57868011600847602 ) ) ;
#59168 = VERTEX_POINT ( 'NONE', #14642 ) ;
#59169 = CARTESIAN_POINT ( 'NONE',  ( 0.000000000000000000, 7.248432822490286753, -1.926193556692960440 ) ) ;
#59170 = CARTESIAN_POINT ( 'NONE',  ( -35.00000000000000000, 0.000000000000000000, 0.000000000000000000 ) ) ;
#59171 = DIRECTION ( 'NONE',  ( 1.000000000000000000, -0.000000000000000000, -0.000000000000000000 ) ) ;
#59172 = DIRECTION ( 'NONE',  ( 0.000000000000000000, 0.01356324068817998940, -0.9999080150203990547 ) ) ;
#59173 = CARTESIAN_POINT ( 'NONE',  ( 2.305787727787083519, -6.711944854845849129, 3.682701754025489826 ) ) ;
#59174 = EDGE_CURVE ( 'NONE', #25143, #10126, #44586, .T. ) ;
#59175 = ORIENTED_EDGE ( 'NONE', *, *, #48045, .T. ) ;
#59176 = CARTESIAN_POINT ( 'NONE',  ( -37.00000000000000711, 3.033604067594749765, -12.38385022362078836 ) ) ;
#59177 = DIRECTION ( 'NONE',  ( -1.000000000000000000, -1.836970198721029688E-16, 0.000000000000000000 ) ) ;
#59178 = FACE_OUTER_BOUND ( 'NONE', #38559, .T. ) ;
#59179 = CARTESIAN_POINT ( 'NONE',  ( -22.29018399051993882, 2.675685774027749986, 2.585196332786354301 ) ) ;
#59180 = ADVANCED_FACE ( 'NONE', ( #4046 ), #25297, .T. ) ;
#59181 = DIRECTION ( 'NONE',  ( 0.000000000000000000, 0.000000000000000000, 1.000000000000000000 ) ) ;
#59182 = ORIENTED_EDGE ( 'NONE', *, *, #6500, .T. ) ;
#59183 = DIRECTION ( 'NONE',  ( 1.000000000000000000, -0.000000000000000000, 0.000000000000000000 ) ) ;
#59184 = ORIENTED_EDGE ( 'NONE', *, *, #8057, .F. ) ;
#59185 = CARTESIAN_POINT ( 'NONE',  ( 0.9232167919969141989, -8.324955738482405110, -9.278116382137454821 ) ) ;
#59186 = CARTESIAN_POINT ( 'NONE',  ( -0.4601472316358399817, -30.53649492335484439, 15.30974548841791183 ) ) ;
#59187 = CIRCLE ( 'NONE', #7139, 12.74999999999999822 ) ;
#59188 = CARTESIAN_POINT ( 'NONE',  ( 36.00000000000000711, 3.307597835713413481, 12.31350058095519273 ) ) ;
#59189 = EDGE_CURVE ( 'NONE', #62456, #14132, #53882, .T. ) ;
#59190 = ORIENTED_EDGE ( 'NONE', *, *, #47562, .F. ) ;
#59191 = VERTEX_POINT ( 'NONE', #49299 ) ;
#59192 = CARTESIAN_POINT ( 'NONE',  ( 35.00000000000000000, -8.551552972817137999, -8.052525312709853722 ) ) ;
#59193 = EDGE_CURVE ( 'NONE', #26426, #55701, #19424, .T. ) ;
#59194 = CARTESIAN_POINT ( 'NONE',  ( 2.244591118396413343, 4.989853642774898290, 5.779440292196087015 ) ) ;
#59195 = CARTESIAN_POINT ( 'NONE',  ( 2.573738926104375047, -3.667129335223154207, -6.822065037112471586 ) ) ;
#59196 = CARTESIAN_POINT ( 'NONE',  ( 0.3278977287071228597, 12.26453627383315848, 0.2481246099268475946 ) ) ;
#59197 = CARTESIAN_POINT ( 'NONE',  ( 0.3164563675027631806, 9.237806174449874064, -8.065346584422156795 ) ) ;
#59198 = ADVANCED_FACE ( 'NONE', ( #46905 ), #62190, .T. ) ;
#59199 = CYLINDRICAL_SURFACE ( 'NONE', #63638, 2.899999999999994582 ) ;
#59200 = ORIENTED_EDGE ( 'NONE', *, *, #44290, .T. ) ;
#59201 = VERTEX_POINT ( 'NONE', #702 ) ;
#59202 = ORIENTED_EDGE ( 'NONE', *, *, #55323, .F. ) ;
#59203 = CARTESIAN_POINT ( 'NONE',  ( 2.251139882113958990, 7.218573619021379173, -2.495216312514809687 ) ) ;
#59204 = CARTESIAN_POINT ( 'NONE',  ( -35.00000000000000000, 0.000000000000000000, 0.000000000000000000 ) ) ;
#59206 = EDGE_CURVE ( 'NONE', #30137, #30073, #10329, .T. ) ;
#59205 = ORIENTED_EDGE ( 'NONE', *, *, #45799, .T. ) ;
#59207 = CYLINDRICAL_SURFACE ( 'NONE', #8150, 2.899999999999994582 ) ;
#59208 = CARTESIAN_POINT ( 'NONE',  ( 2.242819959140645469, -7.536009875295344607, 1.224821922055950418 ) ) ;
#59209 = ORIENTED_EDGE ( 'NONE', *, *, #52025, .T. ) ;
#59210 = CARTESIAN_POINT ( 'NONE',  ( 2.241509619876138171, 6.630717740088905465, -3.784042210004639806 ) ) ;
#59211 = CARTESIAN_POINT ( 'NONE',  ( -27.10719052120871098, 1.622102031466687189, -1.714424047991080613 ) ) ;
#59212 = LINE ( 'NONE', #48275, #31376 ) ;
#59213 = ORIENTED_EDGE ( 'NONE', *, *, #32021, .T. ) ;
#59214 = ORIENTED_EDGE ( 'NONE', *, *, #15811, .F. ) ;
#59215 = CARTESIAN_POINT ( 'NONE',  ( 2.276198483117258586, 2.469789406312234092, 7.236140649716372941 ) ) ;
#59216 = ORIENTED_EDGE ( 'NONE', *, *, #17851, .T. ) ;
#59217 = CARTESIAN_POINT ( 'NONE',  ( 8.437200413559441614, 4.476360154859202467, -12.73625532737110966 ) ) ;
#59218 = ORIENTED_EDGE ( 'NONE', *, *, #35408, .F. ) ;
#59219 = ORIENTED_EDGE ( 'NONE', *, *, #19577, .F. ) ;
#59220 = CARTESIAN_POINT ( 'NONE',  ( 5.515188684475870851, 0.003709313826050237434, 0.003857086913166458270 ) ) ;
#59221 = FACE_OUTER_BOUND ( 'NONE', #17823, .T. ) ;
#59222 = CARTESIAN_POINT ( 'NONE',  ( -11.92921645562753064, -32.88698380610600935, -11.67323352594349650 ) ) ;
#59223 = CARTESIAN_POINT ( 'NONE',  ( -22.27710395300133683, 3.549456197028686866, 0.9764373854728822799 ) ) ;
#59224 = DIRECTION ( 'NONE',  ( 0.000000000000000000, 0.000000000000000000, 1.000000000000000000 ) ) ;
#59225 = DIRECTION ( 'NONE',  ( -1.000000000000000000, 0.000000000000000000, 0.000000000000000000 ) ) ;
#59226 = ORIENTED_EDGE ( 'NONE', *, *, #57349, .F. ) ;
#59227 = DIRECTION ( 'NONE',  ( 1.000000000000000000, 0.000000000000000000, 0.000000000000000000 ) ) ;
#59228 = ADVANCED_FACE ( 'NONE', ( #25975 ), #41236, .T. ) ;
#59229 = ORIENTED_EDGE ( 'NONE', *, *, #64253, .F. ) ;
#59230 = CARTESIAN_POINT ( 'NONE',  ( 35.00000000000000000, 4.705694406421931860E-17, -3.469127814946512892E-15 ) ) ;
#59231 = DIRECTION ( 'NONE',  ( 0.000000000000000000, 0.000000000000000000, 1.000000000000000000 ) ) ;
#59232 = ORIENTED_EDGE ( 'NONE', *, *, #60369, .F. ) ;
#59233 = CARTESIAN_POINT ( 'NONE',  ( -15.66545752291940019, 8.441064718611558604, 8.529329405872159597 ) ) ;
#59234 = DIRECTION ( 'NONE',  ( 0.000000000000000000, 0.000000000000000000, 1.000000000000000000 ) ) ;
#59235 = LINE ( 'NONE', #7707, #40802 ) ;
#59236 = B_SPLINE_CURVE_WITH_KNOTS ( 'NONE', 3,
 ( #30119, #24464, #65025, #23844, #65667, #54751, #3573, #59396, #44104, #40406 ),
 .UNSPECIFIED., .F., .F.,
 ( 4, 3, 3, 4 ),
 ( 1.226634733346699349E-18, 6.607638129004494304E-05, 9.911389841680424680E-05, 0.0001667630577588614710 ),
 .UNSPECIFIED. ) ;
#59237 = AXIS2_PLACEMENT_3D ( 'NONE', #40389, #60693, #34737 ) ;
#59238 = ORIENTED_EDGE ( 'NONE', *, *, #38849, .F. ) ;
#59239 = VERTEX_POINT ( 'NONE', #1362 ) ;
#59240 = VECTOR ( 'NONE', #25336, 1000.000000000000000 ) ;
#59241 = CARTESIAN_POINT ( 'NONE',  ( 2.244591118396559448, -7.634724215899725941, 0.1074970442783885205 ) ) ;
#59242 =( BOUNDED_CURVE ( )  B_SPLINE_CURVE ( 3, ( #352, #50571, #15616, #20631 ),
 .UNSPECIFIED., .F., .F. ) 
 B_SPLINE_CURVE_WITH_KNOTS ( ( 4, 4 ),
 ( 1.759007296960887645, 1.789005565290672672 ),
 .UNSPECIFIED. ) 
 CURVE ( )  GEOMETRIC_REPRESENTATION_ITEM ( )  RATIONAL_B_SPLINE_CURVE ( ( 1.000000000000000000, 0.9999250100640160177, 0.9999250100640160177, 1.000000000000000000 ) ) 
 REPRESENTATION_ITEM ( '' )  );
#59243 = ORIENTED_EDGE ( 'NONE', *, *, #55857, .T. ) ;
#59244 = DIRECTION ( 'NONE',  ( -1.000000000000000000, 0.000000000000000000, 0.000000000000000000 ) ) ;
#59245 = CARTESIAN_POINT ( 'NONE',  ( -3.979081881654057629, -10.13347235061305796, 6.442799153484752850 ) ) ;
#59246 = CARTESIAN_POINT ( 'NONE',  ( -27.08416781016246588, 2.158663327075696081, 0.7680651426971605300 ) ) ;
#59247 = DIRECTION ( 'NONE',  ( -1.000000000000000000, -0.000000000000000000, 0.000000000000000000 ) ) ;
#59248 = CARTESIAN_POINT ( 'NONE',  ( 1.459561108993331358, -9.267924853468697322, 8.601340491611225048 ) ) ;
#59249 = ADVANCED_FACE ( 'NONE', ( #5704 ), #26211, .F. ) ;
#59250 = ORIENTED_EDGE ( 'NONE', *, *, #59862, .T. ) ;
#59251 = CARTESIAN_POINT ( 'NONE',  ( 0.3665391374699465965, -9.237363111276819083, 8.095513416941198415 ) ) ;
#59252 = CARTESIAN_POINT ( 'NONE',  ( 37.00000000000000711, -4.725891942574827809, -10.75351884295726101 ) ) ;
#59253 = EDGE_CURVE ( 'NONE', #15087, #27683, #40326, .T. ) ;
#59254 = CARTESIAN_POINT ( 'NONE',  ( -35.00000000000000000, 11.74226168163341555, 0.3025107581131598611 ) ) ;
#59255 = CARTESIAN_POINT ( 'NONE',  ( -18.12051508114042164, -4.789732380985432414, 11.00348193257416973 ) ) ;
#59256 = DIRECTION ( 'NONE',  ( -1.000000000000000000, 0.000000000000000000, 0.000000000000000000 ) ) ;
#59257 = FACE_OUTER_BOUND ( 'NONE', #61483, .T. ) ;
#59258 = CYLINDRICAL_SURFACE ( 'NONE', #2827, 5.000000000000000888 ) ;
#59259 = DIRECTION ( 'NONE',  ( 0.000000000000000000, 0.01356324068817998940, -0.9999080150203990547 ) ) ;
#59260 = EDGE_CURVE ( 'NONE', #19597, #33743, #61521, .T. ) ;
#59261 = VECTOR ( 'NONE', #53743, 1000.000000000000000 ) ;
#59262 = ORIENTED_EDGE ( 'NONE', *, *, #55857, .F. ) ;
#59263 = CARTESIAN_POINT ( 'NONE',  ( 12.42313808479329218, -9.574587216605449314, -7.236090607063219160 ) ) ;
#59264 = B_SPLINE_CURVE_WITH_KNOTS ( 'NONE', 3,
 ( #58924, #38262, #54238, #8347, #8038, #64835, #49269, #19314, #59885, #58584, #39586, #48931, #54884, #3725, #14307, #34585, #44244, #9306, #54577 ),
 .UNSPECIFIED., .F., .F.,
 ( 4, 3, 3, 3, 3, 3, 4 ),
 ( 0.000000000000000000, 2.831840207499539448E-05, 4.217266859840335547E-05, 5.602024318395820929E-05, 6.290810167968980229E-05, 9.120440630945211011E-05, 0.0001153103026479757780 ),
 .UNSPECIFIED. ) ;
#59265 = VECTOR ( 'NONE', #48337, 1000.000000000000000 ) ;
#59266 = ORIENTED_EDGE ( 'NONE', *, *, #36005, .T. ) ;
#59267 = CARTESIAN_POINT ( 'NONE',  ( 2.000000000000001776, 0.000000000000000000, 0.000000000000000000 ) ) ;
#59268 = CARTESIAN_POINT ( 'NONE',  ( -22.27722015946438816, -3.628085906632222635, 0.6262261846986550973 ) ) ;
#59269 = CARTESIAN_POINT ( 'NONE',  ( 0.2653141617321009282, 6.084921229689422617, 10.62747662594933296 ) ) ;
#59270 = CARTESIAN_POINT ( 'NONE',  ( -35.00000000000000000, 5.300372733891805410, -11.59605747147781152 ) ) ;
#59271 = ORIENTED_EDGE ( 'NONE', *, *, #59189, .F. ) ;
#59272 = ORIENTED_EDGE ( 'NONE', *, *, #1389, .F. ) ;
#59273 = ORIENTED_EDGE ( 'NONE', *, *, #60717, .F. ) ;
#59274 = CARTESIAN_POINT ( 'NONE',  ( 0.3278977287071230817, -7.693417476735460170, -9.554671284920370766 ) ) ;
#59275 = EDGE_CURVE ( 'NONE', #34346, #58095, #41968, .T. ) ;
#59276 = ORIENTED_EDGE ( 'NONE', *, *, #12744, .F. ) ;
#59277 = CARTESIAN_POINT ( 'NONE',  ( -22.27719412087655471, -2.283949229175425533, -2.887588494201234202 ) ) ;
#59278 = CARTESIAN_POINT ( 'NONE',  ( 2.305787727787085295, 5.756228004061457959, 5.047606869483074910 ) ) ;
#59279 = CARTESIAN_POINT ( 'NONE',  ( 0.3002738374340835348, 10.50101454678644686, 6.323236184341160637 ) ) ;
#59280 = CARTESIAN_POINT ( 'NONE',  ( -15.27729454824424948, 5.151216734910788908, 25.00000000000000000 ) ) ;
#59281 = ORIENTED_EDGE ( 'NONE', *, *, #27319, .F. ) ;
#59282 = CARTESIAN_POINT ( 'NONE',  ( 35.00000000000000000, -6.753013023069642351, 10.14433819232440825 ) ) ;
#59283 = CARTESIAN_POINT ( 'NONE',  ( 12.59130566666910944, -33.86016745060436506, 10.02644098062840960 ) ) ;
#59284 = CARTESIAN_POINT ( 'NONE',  ( 2.266490820343228574, -1.470039317404115309, -7.500072841116513622 ) ) ;
#59286 = ORIENTED_EDGE ( 'NONE', *, *, #65327, .F. ) ;
#59285 = FACE_OUTER_BOUND ( 'NONE', #48196, .T. ) ;
#59287 = CARTESIAN_POINT ( 'NONE',  ( 5.514970785353741078, 0.003415090918276138254, -0.003262412238248725994 ) ) ;
#59288 = ORIENTED_EDGE ( 'NONE', *, *, #65767, .F. ) ;
#59289 = CARTESIAN_POINT ( 'NONE',  ( 35.00000000000000000, -10.59380114696464581, 7.094637218249467026 ) ) ;
#59290 = ORIENTED_EDGE ( 'NONE', *, *, #39939, .T. ) ;
#59291 = CARTESIAN_POINT ( 'NONE',  ( 3.152665057734128862, 2.258875078502223133, 7.609997527621164437 ) ) ;
#59292 = CARTESIAN_POINT ( 'NONE',  ( 0.3057689695767515925, 3.975296631252121404, -11.59726335252429230 ) ) ;
#59293 = DIRECTION ( 'NONE',  ( 0.000000000000000000, 0.01356324068817998940, -0.9999080150203990547 ) ) ;
#59294 = CARTESIAN_POINT ( 'NONE',  ( 0.3223008802179286869, -3.964361764750254924, 11.60682919296350946 ) ) ;
#59295 = CARTESIAN_POINT ( 'NONE',  ( 0.2648978790185619880, -11.46165506714231341, 4.312320170909196726 ) ) ;
#59296 = CARTESIAN_POINT ( 'NONE',  ( -10.22413763068411541, -4.688135402597775503, -12.66488886014959725 ) ) ;
#59297 = CARTESIAN_POINT ( 'NONE',  ( 37.00000000000000711, -3.645068577059948911, 11.16627499335658413 ) ) ;
#59298 = EDGE_CURVE ( 'NONE', #43145, #26931, #36596, .T. ) ;
#59299 = EDGE_LOOP ( 'NONE', ( #39074, #30075, #36345, #4026 ) ) ;
#59300 = AXIS2_PLACEMENT_3D ( 'NONE', #25504, #4919, #35789 ) ;
#59301 = DIRECTION ( 'NONE',  ( 0.000000000000000000, -0.01356324068817998940, 0.9999080150203990547 ) ) ;
#59302 = ORIENTED_EDGE ( 'NONE', *, *, #30597, .T. ) ;
#59303 = EDGE_CURVE ( 'NONE', #48610, #26353, #53111, .T. ) ;
#59304 = ORIENTED_EDGE ( 'NONE', *, *, #1109, .F. ) ;
#59305 = CARTESIAN_POINT ( 'NONE',  ( 2.000000000000001776, -7.493043167941588756, -0.3229614270520431152 ) ) ;
#59306 = DIRECTION ( 'NONE',  ( 0.000000000000000000, -0.9987865678893272925, 0.04924826701375684818 ) ) ;
#59307 = CARTESIAN_POINT ( 'NONE',  ( 0.000000000000000000, 3.979254915827449945, -5.681598592373734213 ) ) ;
#59308 = CARTESIAN_POINT ( 'NONE',  ( -22.29479313954897890, 2.096782908204907869, 3.090162644873513997 ) ) ;
#59309 = CIRCLE ( 'NONE', #17863, 12.75000000000000178 ) ;
#59310 = CARTESIAN_POINT ( 'NONE',  ( -37.00000000000000711, 1.171570255487447643, 11.68758509253248867 ) ) ;
#59311 = EDGE_CURVE ( 'NONE', #8578, #8085, #21257, .T. ) ;
#59312 = CARTESIAN_POINT ( 'NONE',  ( 0.6473888112830253894, -10.87693551365366673, -5.898884566269122942 ) ) ;
#59313 = CIRCLE ( 'NONE', #43345, 3.552075659825890241 ) ;
#59314 = AXIS2_PLACEMENT_3D ( 'NONE', #59358, #54388, #53400 ) ;
#59315 = ORIENTED_EDGE ( 'NONE', *, *, #17715, .T. ) ;
#59316 = CARTESIAN_POINT ( 'NONE',  ( 35.00000000000000000, 11.65150730582934635, 1.488153103997001514 ) ) ;
#59317 = DIRECTION ( 'NONE',  ( 0.000000000000000000, -0.7617968321374946061, -0.6478160128811869534 ) ) ;
#59318 = AXIS2_PLACEMENT_3D ( 'NONE', #14619, #40907, #44904 ) ;
#59319 = CARTESIAN_POINT ( 'NONE',  ( 2.941278708680199916, -1.198640839021267723, -6.021511413163973536 ) ) ;
#59320 = EDGE_CURVE ( 'NONE', #57170, #63179, #39284, .T. ) ;
#59321 = VERTEX_POINT ( 'NONE', #58193 ) ;
#59322 = AXIS2_PLACEMENT_3D ( 'NONE', #25517, #45809, #271 ) ;
#59323 = CARTESIAN_POINT ( 'NONE',  ( -8.519593703685796271, -2.053853521695917728, 13.34350279803584449 ) ) ;
#59324 = LINE ( 'NONE', #63311, #34178 ) ;
#59325 = ORIENTED_EDGE ( 'NONE', *, *, #11134, .T. ) ;
#59326 = FACE_OUTER_BOUND ( 'NONE', #21043, .T. ) ;
#59327 = CARTESIAN_POINT ( 'NONE',  ( 5.515539859299206427, 0.005142293699651638746, 0.003193223631738825990 ) ) ;
#59328 = CARTESIAN_POINT ( 'NONE',  ( 2.506442445385721474, 1.822928711644228761, 11.86634058133937053 ) ) ;
#59329 = CIRCLE ( 'NONE', #7299, 16.73205080756888563 ) ;
#59330 = CYLINDRICAL_SURFACE ( 'NONE', #63925, 12.75000000000000178 ) ;
#59331 = CARTESIAN_POINT ( 'NONE',  ( 1.719304012338199517, 0.000000000000000000, 0.000000000000000000 ) ) ;
#59332 = ORIENTED_EDGE ( 'NONE', *, *, #49272, .F. ) ;
#59333 = AXIS2_PLACEMENT_3D ( 'NONE', #2817, #49019, #34352 ) ;
#59334 = CARTESIAN_POINT ( 'NONE',  ( 5.516018279890452902, 0.0002248006052446666569, -0.006771744149385742172 ) ) ;
#59335 = B_SPLINE_CURVE_WITH_KNOTS ( 'NONE', 3,
 ( #37701, #47674, #46368, #16444, #6458, #810, #27377, #26092, #26740, #21077, #36710, #5832, #31068, #57010, #11433, #31703, #47032, #1490, #21767 ),
 .UNSPECIFIED., .F., .F.,
 ( 4, 3, 3, 3, 3, 3, 4 ),
 ( 0.000000000000000000, 2.831840207499292453E-05, 4.217266859840086181E-05, 5.602024318395534971E-05, 6.290810167968737638E-05, 9.120440630944575398E-05, 0.0001153103026479753850 ),
 .UNSPECIFIED. ) ;
#59336 = CARTESIAN_POINT ( 'NONE',  ( 0.3002738374340856442, -12.10874171309340142, 1.906042098268977636 ) ) ;
#59337 = CARTESIAN_POINT ( 'NONE',  ( -18.48144388550085182, 4.313438978693093340, -11.19870530402159226 ) ) ;
#59338 = ORIENTED_EDGE ( 'NONE', *, *, #3399, .T. ) ;
#59339 = CARTESIAN_POINT ( 'NONE',  ( 2.000000000000001776, 0.08317740279932192560, 7.499538753794337431 ) ) ;
#59340 = CARTESIAN_POINT ( 'NONE',  ( -27.20164183316783024, -1.232966507052636329, 2.339520810540414164 ) ) ;
#59341 = ORIENTED_EDGE ( 'NONE', *, *, #24377, .T. ) ;
#59342 = VERTEX_POINT ( 'NONE', #58875 ) ;
#59343 = CARTESIAN_POINT ( 'NONE',  ( -22.30625920655495165, -0.2529928606556531290, -3.783486345733990674 ) ) ;
#59344 = AXIS2_PLACEMENT_3D ( 'NONE', #65461, #7748, #39550 ) ;
#59345 = EDGE_CURVE ( 'NONE', #30591, #44042, #22954, .T. ) ;
#59346 = VERTEX_POINT ( 'NONE', #57879 ) ;
#59347 = FACE_OUTER_BOUND ( 'NONE', #49017, .T. ) ;
#59348 = FACE_OUTER_BOUND ( 'NONE', #26009, .T. ) ;
#59349 = AXIS2_PLACEMENT_3D ( 'NONE', #30298, #14980, #24989 ) ;
#59350 = DIRECTION ( 'NONE',  ( -1.000000000000000000, 0.000000000000000000, 0.000000000000000000 ) ) ;
#59351 = CARTESIAN_POINT ( 'NONE',  ( 2.000000000000001776, -3.230174184210014232, -5.998318953995379843 ) ) ;
#59352 = CARTESIAN_POINT ( 'NONE',  ( 3.152665057734087117, 7.886634106564184954, -0.9030954876737516956 ) ) ;
#59354 = EDGE_LOOP ( 'NONE', ( #33187, #51011, #60202, #64525 ) ) ;
#59353 = DIRECTION ( 'NONE',  ( -1.000000000000000000, -0.000000000000000000, 0.000000000000000000 ) ) ;
#59355 = AXIS2_PLACEMENT_3D ( 'NONE', #50152, #24209, #44475 ) ;
#59356 = DIRECTION ( 'NONE',  ( -1.000000000000000000, -0.000000000000000000, 0.000000000000000000 ) ) ;
#59357 = ORIENTED_EDGE ( 'NONE', *, *, #42829, .F. ) ;
#59358 = CARTESIAN_POINT ( 'NONE',  ( 35.00000000000000000, 4.705694406421931860E-17, -3.469127814946512892E-15 ) ) ;
#59359 = VERTEX_POINT ( 'NONE', #18293 ) ;
#59360 = AXIS2_PLACEMENT_3D ( 'NONE', #56027, #10468, #29759 ) ;
#59361 = ORIENTED_EDGE ( 'NONE', *, *, #58004, .F. ) ;
#59362 = CARTESIAN_POINT ( 'NONE',  ( -35.00000000000000000, 0.06441628369853458214, -12.18632975068353019 ) ) ;
#59363 = CARTESIAN_POINT ( 'NONE',  ( -9.369086346424605694, -29.24458096581515321, 11.21746676166726786 ) ) ;
#59364 = CARTESIAN_POINT ( 'NONE',  ( -24.38798772506720169, 11.02001175613503925, 7.800463590741535391 ) ) ;
#59365 = ADVANCED_FACE ( 'NONE', ( #8301 ), #21958, .T. ) ;
#59366 = CARTESIAN_POINT ( 'NONE',  ( 24.17751860031820144, -2.141477541963367592, 11.80861164620684711 ) ) ;
#59367 = CARTESIAN_POINT ( 'NONE',  ( 0.2648978790185619880, -11.46165506714231341, 4.312320170909196726 ) ) ;
#59368 = CARTESIAN_POINT ( 'NONE',  ( 2.297017764049618993, 5.967068736726843348, 4.791851130936075620 ) ) ;
#59369 = VERTEX_POINT ( 'NONE', #2002 ) ;
#59370 = ORIENTED_EDGE ( 'NONE', *, *, #6994, .F. ) ;
#59371 = EDGE_CURVE ( 'NONE', #35410, #25804, #36088, .T. ) ;
#59372 = DIRECTION ( 'NONE',  ( 0.000000000000000000, 0.01356324068817998940, -0.9999080150203990547 ) ) ;
#59373 = LINE ( 'NONE', #26333, #65079 ) ;
#59374 = EDGE_CURVE ( 'NONE', #4778, #37616, #14818, .T. ) ;
#59375 = VERTEX_POINT ( 'NONE', #53861 ) ;
#59376 = CARTESIAN_POINT ( 'NONE',  ( 2.241449424704145876, -1.265244293929138841, 7.528892370271786483 ) ) ;
#59377 = CARTESIAN_POINT ( 'NONE',  ( 0.2759803524722184154, -10.51260004517008717, -6.288205958087898395 ) ) ;
#59378 = CARTESIAN_POINT ( 'NONE',  ( 37.00000000000000711, -5.921969905510278132, 10.14408668126219304 ) ) ;
#59379 = CARTESIAN_POINT ( 'NONE',  ( -22.28482751661422867, 3.048214341614492451, -2.105139449411404851 ) ) ;
#59380 = DIRECTION ( 'NONE',  ( 0.000000000000000000, -0.01356324068817998940, 0.9999080150203990547 ) ) ;
#59381 = EDGE_CURVE ( 'NONE', #60329, #53266, #24431, .T. ) ;
#59382 = ORIENTED_EDGE ( 'NONE', *, *, #50996, .T. ) ;
#59383 = AXIS2_PLACEMENT_3D ( 'NONE', #63221, #11057, #17691 ) ;
#59384 = EDGE_CURVE ( 'NONE', #40797, #24451, #4275, .T. ) ;
#59385 = EDGE_LOOP ( 'NONE', ( #59618, #60047, #27893, #49248 ) ) ;
#59386 = DIRECTION ( 'NONE',  ( -1.000000000000000000, 0.000000000000000000, 0.000000000000000000 ) ) ;
#59387 = CARTESIAN_POINT ( 'NONE',  ( 2.305787727787084407, 4.792270232040973355, -5.970480882365174047 ) ) ;
#59388 = DIRECTION ( 'NONE',  ( -1.000000000000000000, 0.000000000000000000, 0.000000000000000000 ) ) ;
#59389 = AXIS2_PLACEMENT_3D ( 'NONE', #48802, #44124, #38139 ) ;
#59390 = AXIS2_PLACEMENT_3D ( 'NONE', #3908, #39127, #60077 ) ;
#59391 = CARTESIAN_POINT ( 'NONE',  ( -17.83419946441818027, -9.720786832536937538, -7.036071585506806336 ) ) ;
#59392 = DIRECTION ( 'NONE',  ( -1.000000000000000000, 0.000000000000000000, 0.000000000000000000 ) ) ;
#59393 = EDGE_CURVE ( 'NONE', #34255, #29292, #38802, .T. ) ;
#59394 = AXIS2_PLACEMENT_3D ( 'NONE', #17554, #26866, #47169 ) ;
#59395 = CARTESIAN_POINT ( 'NONE',  ( -7.200201640635544464, -1.899635279488593120, -11.84901858051199142 ) ) ;
#59396 = CARTESIAN_POINT ( 'NONE',  ( 2.241509619876138171, 5.872890204493088184, -4.877966158328247204 ) ) ;
#59397 = CARTESIAN_POINT ( 'NONE',  ( 2.305787727787084407, 1.493241775258423720, 7.508843116234161563 ) ) ;
#59398 = PLANE ( 'NONE',  #51980 ) ;
#59399 = ORIENTED_EDGE ( 'NONE', *, *, #57835, .T. ) ;
#59400 = CARTESIAN_POINT ( 'NONE',  ( 0.2650492594609241692, 12.04046128294318052, 2.234872523101219866 ) ) ;
#59401 = CARTESIAN_POINT ( 'NONE',  ( -23.18047892478189453, -0.4043282704081303525, 4.776019214182007921 ) ) ;
#59402 = CARTESIAN_POINT ( 'NONE',  ( 2.177405672431210970, -7.702458780351562062, -8.129711416440695615 ) ) ;
#59403 = CIRCLE ( 'NONE', #54142, 7.499999999999988454 ) ;
#59404 = AXIS2_PLACEMENT_3D ( 'NONE', #14956, #64216, #49906 ) ;
#59405 = CARTESIAN_POINT ( 'NONE',  ( 2.259025283528088401, -0.1366755880739185802, -7.639069972920481177 ) ) ;
#59406 = CARTESIAN_POINT ( 'NONE',  ( 2.261269890822071638, -5.942064862945643178, 4.803890999604306877 ) ) ;
#59407 = ORIENTED_EDGE ( 'NONE', *, *, #24598, .F. ) ;
#59408 = FACE_OUTER_BOUND ( 'NONE', #57158, .T. ) ;
#59409 = CARTESIAN_POINT ( 'NONE',  ( 2.241352910868908754, 7.145045428366577411, 2.689314586382375527 ) ) ;
#59410 = CARTESIAN_POINT ( 'NONE',  ( 3.024435290549866817, -27.93754772256033903, -12.30283293119135202 ) ) ;
#59411 = ORIENTED_EDGE ( 'NONE', *, *, #16070, .T. ) ;
#59412 = CARTESIAN_POINT ( 'NONE',  ( -9.367105207800477729, -2.739720568162369307, -13.21991852363683506 ) ) ;
#59413 = DIRECTION ( 'NONE',  ( 0.000000000000000000, -0.01356324068817992175, 0.9999080150203990547 ) ) ;
#59414 = CARTESIAN_POINT ( 'NONE',  ( 17.00162812139343416, -11.45156432714296635, 7.188684627388551185 ) ) ;
#59415 = DIRECTION ( 'NONE',  ( -1.000000000000000000, 0.000000000000000000, 0.000000000000000000 ) ) ;
#59416 = CARTESIAN_POINT ( 'NONE',  ( -9.502270498702225510, -12.89234730350994340, -4.021714702740394110 ) ) ;
#59417 = ADVANCED_FACE ( 'NONE', ( #27266 ), #2345, .T. ) ;
#59418 = AXIS2_PLACEMENT_3D ( 'NONE', #48866, #9249, #58868 ) ;
#59419 = CARTESIAN_POINT ( 'NONE',  ( 2.000000000000001776, -6.796153407501424049, -1.388283512725909219 ) ) ;
#59420 = ORIENTED_EDGE ( 'NONE', *, *, #16120, .T. ) ;
#59421 = DIRECTION ( 'NONE',  ( 0.000000000000000000, -0.01356324068817991828, 0.9999080150203990547 ) ) ;
#59422 = CARTESIAN_POINT ( 'NONE',  ( 0.3040950598368144520, 10.74226959800799719, -5.912066680610498892 ) ) ;
#59423 = DIRECTION ( 'NONE',  ( -1.000000000000000000, 0.000000000000000000, 0.000000000000000000 ) ) ;
#59424 = CARTESIAN_POINT ( 'NONE',  ( 37.00000000000000711, 7.817610399097634222, 8.766823244861901898 ) ) ;
#59425 =( BOUNDED_SURFACE ( )  B_SPLINE_SURFACE ( 3, 1, ( 
 ( #41485, #63096 ),
 ( #42138, #52796 ),
 ( #37497, #16885 ),
 ( #26217, #12224 ) ),
 .UNSPECIFIED., .F., .F., .F. ) 
 B_SPLINE_SURFACE_WITH_KNOTS ( ( 4, 4 ),
 ( 2, 2 ),
 ( 0.000000000000000000, 1.000000000000000000 ),
 ( 0.000000000000000000, 1.000000000000000000 ),
 .UNSPECIFIED. ) 
 GEOMETRIC_REPRESENTATION_ITEM ( )  RATIONAL_B_SPLINE_SURFACE ( (
 ( 1.000000000000000000, 1.000000000000000000),
 ( 0.9856612449720755231, 0.9999558406602322425),
 ( 0.9856612449720755231, 0.9999558406602322425),
 ( 1.000000000000000000, 1.000000000000000000) ) ) 
 REPRESENTATION_ITEM ( '' )  SURFACE ( )  );
#59426 = DIRECTION ( 'NONE',  ( -1.000000000000000000, 0.000000000000000000, -0.000000000000000000 ) ) ;
#59428 = CARTESIAN_POINT ( 'NONE',  ( -22.71097035706202405, -4.089776368546547580, -2.846599994298351977 ) ) ;
#59427 = AXIS2_PLACEMENT_3D ( 'NONE', #32621, #16698, #42952 ) ;
#59429 = CARTESIAN_POINT ( 'NONE',  ( -30.04249239712260788, 0.3851321492415041847, -12.00220082160331891 ) ) ;
#59430 = CARTESIAN_POINT ( 'NONE',  ( 2.251152103361941492, 1.202724109300151500, -7.542379262758394987 ) ) ;
#59431 = ORIENTED_EDGE ( 'NONE', *, *, #60715, .F. ) ;
#59432 = VERTEX_POINT ( 'NONE', #12957 ) ;
#59433 = EDGE_CURVE ( 'NONE', #57314, #38680, #60192, .T. ) ;
#59434 = CARTESIAN_POINT ( 'NONE',  ( -17.74424199868676766, -6.571554700141313710, -10.04532163134672551 ) ) ;
#59435 = ORIENTED_EDGE ( 'NONE', *, *, #3512, .T. ) ;
#59436 =( NAMED_UNIT ( * ) PLANE_ANGLE_UNIT ( ) SI_UNIT ( $, .RADIAN. ) );
#59437 = AXIS2_PLACEMENT_3D ( 'NONE', #10668, #61534, #716 ) ;
#59438 = CARTESIAN_POINT ( 'NONE',  ( -35.00000000000000000, -5.636262487437237567, -10.80478261802188023 ) ) ;
#59439 = EDGE_CURVE ( 'NONE', #14466, #64767, #22288, .T. ) ;
#59440 = CARTESIAN_POINT ( 'NONE',  ( 35.00000000000000000, -11.56998259273180274, -3.827046518385039064 ) ) ;
#59442 = ORIENTED_EDGE ( 'NONE', *, *, #44345, .T. ) ;
#59441 = CIRCLE ( 'NONE', #2102, 4.999999999999999112 ) ;
#59443 = LINE ( 'NONE', #38504, #63058 ) ;
#59444 = CARTESIAN_POINT ( 'NONE',  ( 2.266490820343221024, 6.544980046121079198, -3.946561086901401172 ) ) ;
#59445 = ADVANCED_FACE ( 'NONE', ( #53201 ), #43529, .T. ) ;
#59446 = CARTESIAN_POINT ( 'NONE',  ( 2.257661810676955927, -5.013319178751810767, -5.764872664104216504 ) ) ;
#59447 = ORIENTED_EDGE ( 'NONE', *, *, #31166, .T. ) ;
#59448 = ORIENTED_EDGE ( 'NONE', *, *, #63752, .F. ) ;
#59449 = CARTESIAN_POINT ( 'NONE',  ( 0.000000000000000000, 0.000000000000000000, 0.000000000000000000 ) ) ;
#59450 = ADVANCED_FACE ( 'NONE', ( #22271 ), #53549, .T. ) ;
#59451 = CARTESIAN_POINT ( 'NONE',  ( 5.520433897694421610, -0.01120198501134877893, 0.01006947824912462000 ) ) ;
#59452 = EDGE_LOOP ( 'NONE', ( #10594, #29138, #4308, #47643 ) ) ;
#59453 = ORIENTED_EDGE ( 'NONE', *, *, #49553, .T. ) ;
#59454 = DIRECTION ( 'NONE',  ( 1.000000000000000000, 0.000000000000000000, 0.000000000000000000 ) ) ;
#59455 = DIRECTION ( 'NONE',  ( -1.000000000000000000, -0.000000000000000000, 0.000000000000000000 ) ) ;
#59456 = CARTESIAN_POINT ( 'NONE',  ( 0.2834382757448002943, 10.50792790568177182, -6.300836243950055149 ) ) ;
#59457 = CARTESIAN_POINT ( 'NONE',  ( -7.489022030332961322, 8.034049540753141372, -10.84914964302385521 ) ) ;
#59458 = FACE_OUTER_BOUND ( 'NONE', #31678, .T. ) ;
#59459 = CARTESIAN_POINT ( 'NONE',  ( 2.827825597296801163, 5.372687261161280148, 7.250702617666018313 ) ) ;
#59460 = ORIENTED_EDGE ( 'NONE', *, *, #11757, .F. ) ;
#59461 = CARTESIAN_POINT ( 'NONE',  ( 2.350038591458109227, -2.471682575235262025, 10.33030559206112997 ) ) ;
#59462 = ADVANCED_FACE ( 'NONE', ( #47557 ), #49843, .T. ) ;
#59463 = CARTESIAN_POINT ( 'NONE',  ( -16.80243436552160574, 7.513500008141047459, 9.356964553287092201 ) ) ;
#59464 = CARTESIAN_POINT ( 'NONE',  ( 0.2653141334712589838, -9.352759824582554060, 7.905403790036936940 ) ) ;
#59465 = EDGE_CURVE ( 'NONE', #51290, #27983, #1095, .T. ) ;
#59466 = DIRECTION ( 'NONE',  ( -0.3939253465568943735, -0.1691689424289704313, -0.9034404741085569901 ) ) ;
#59467 = CARTESIAN_POINT ( 'NONE',  ( 0.3632410797595244656, -8.092233745354578289, -9.235006602299437262 ) ) ;
#59468 = CARTESIAN_POINT ( 'NONE',  ( -27.08850691366518504, 1.609738257842381559, -1.648570643966305260 ) ) ;
#59469 = CARTESIAN_POINT ( 'NONE',  ( -27.08426571771018132, 1.357728109767524005, 1.845988025802319132 ) ) ;
#59470 = CARTESIAN_POINT ( 'NONE',  ( 2.000000000000001776, -2.562706407243680928, 6.312399813420318750 ) ) ;
#59471 = CARTESIAN_POINT ( 'NONE',  ( 1.462291587748370647, 5.766456054324373248, 11.25382118863233316 ) ) ;
#59472 = EDGE_CURVE ( 'NONE', #64505, #6215, #24235, .T. ) ;
#59473 = AXIS2_PLACEMENT_3D ( 'NONE', #32249, #32558, #48551 ) ;
#59474 = ORIENTED_EDGE ( 'NONE', *, *, #11007, .T. ) ;
#59475 = DIRECTION ( 'NONE',  ( -1.000000000000000000, 0.000000000000000000, 0.000000000000000000 ) ) ;
#59476 = EDGE_CURVE ( 'NONE', #14064, #43917, #55238, .T. ) ;
#59477 = EDGE_CURVE ( 'NONE', #44848, #3064, #3196, .T. ) ;
#59478 = ORIENTED_EDGE ( 'NONE', *, *, #24598, .T. ) ;
#59479 = CARTESIAN_POINT ( 'NONE',  ( 37.00000000000000711, -12.74068829017554094, -0.4871980014161064743 ) ) ;
#59480 = CARTESIAN_POINT ( 'NONE',  ( 35.00000000000000000, 4.705694406421931860E-17, -3.469127814946512892E-15 ) ) ;
#59481 = CARTESIAN_POINT ( 'NONE',  ( 0.3665391374699464300, 11.44911061034386179, 4.447929964102885769 ) ) ;
#59482 = EDGE_CURVE ( 'NONE', #29583, #57508, #24903, .T. ) ;
#59483 = CARTESIAN_POINT ( 'NONE',  ( 0.2653519890518169499, 9.381137101569672510, 7.871697161810723209 ) ) ;
#59484 = CARTESIAN_POINT ( 'NONE',  ( -35.00000000000000000, -6.036400161834495570, -10.07641281632183983 ) ) ;
#59485 = ORIENTED_EDGE ( 'NONE', *, *, #6262, .F. ) ;
#59486 = CARTESIAN_POINT ( 'NONE',  ( 0.3665391374699472626, 7.691255657244420618, -9.576575648338943481 ) ) ;
#59487 = DIRECTION ( 'NONE',  ( 0.000000000000000000, -1.000000000000000000, 0.000000000000000000 ) ) ;
#59488 = CARTESIAN_POINT ( 'NONE',  ( 12.52750123246316072, 0.4973700281276248192, 11.98968819674307618 ) ) ;
#59489 = CARTESIAN_POINT ( 'NONE',  ( -22.28415773361649954, 2.647149619609392879, 2.588610893123033829 ) ) ;
#59490 = AXIS2_PLACEMENT_3D ( 'NONE', #29811, #4576, #60404 ) ;
#59491 = AXIS2_PLACEMENT_3D ( 'NONE', #44128, #18566, #35104 ) ;
#59492 = CARTESIAN_POINT ( 'NONE',  ( 2.000000000000001776, -6.643843315911796665, -1.507714007300762660 ) ) ;
#59493 = EDGE_LOOP ( 'NONE', ( #8521, #22548, #12622, #49570 ) ) ;
#59494 = CARTESIAN_POINT ( 'NONE',  ( 0.2655924914740778187, -6.161287456391757011, 10.58356227062107457 ) ) ;
#59495 = VERTEX_POINT ( 'NONE', #9256 ) ;
#59496 = CARTESIAN_POINT ( 'NONE',  ( 2.305787727787083519, 5.756228004061526349, -5.047606869482997638 ) ) ;
#59497 = CARTESIAN_POINT ( 'NONE',  ( 35.00000000000000000, 4.705694406421931860E-17, -3.469127814946512892E-15 ) ) ;
#59498 = CIRCLE ( 'NONE', #36116, 4.999999999999999112 ) ;
#59499 = FACE_OUTER_BOUND ( 'NONE', #61609, .T. ) ;
#59500 = DIRECTION ( 'NONE',  ( 0.000000000000000000, 0.01356324068817998940, -0.9999080150203990547 ) ) ;
#59501 = EDGE_CURVE ( 'NONE', #34799, #64644, #35044, .T. ) ;
#59502 = ORIENTED_EDGE ( 'NONE', *, *, #16801, .T. ) ;
#59503 = ORIENTED_EDGE ( 'NONE', *, *, #9296, .T. ) ;
#59504 = DIRECTION ( 'NONE',  ( 1.000000000000000000, 0.000000000000000000, 0.000000000000000000 ) ) ;
#59505 = AXIS2_PLACEMENT_3D ( 'NONE', #249, #4587, #24857 ) ;
#59506 = DIRECTION ( 'NONE',  ( -0.9854502544271372955, 0.000000000000000000, -0.1699641022377680610 ) ) ;
#59507 = DIRECTION ( 'NONE',  ( 0.3939253465568944290, 0.009718094113439539050, -0.9190910618577644575 ) ) ;
#59508 = CARTESIAN_POINT ( 'NONE',  ( 35.00000000000000000, 10.99909370905164430, 5.246972444133898072 ) ) ;
#59509 = CARTESIAN_POINT ( 'NONE',  ( 2.907497136251136816, 6.617189382231139838, -4.235253383576361053 ) ) ;
#59510 = CARTESIAN_POINT ( 'NONE',  ( 1.020182472822753317, -12.48987306958581556, -0.4462553704985335323 ) ) ;
#59511 = ORIENTED_EDGE ( 'NONE', *, *, #16723, .F. ) ;
#59512 = VECTOR ( 'NONE', #58724, 1000.000000000000000 ) ;
#59513 = ADVANCED_FACE ( 'NONE', ( #45177 ), #24567, .T. ) ;
#59514 = ORIENTED_EDGE ( 'NONE', *, *, #64446, .T. ) ;
#59515 = ORIENTED_EDGE ( 'NONE', *, *, #1550, .F. ) ;
#59516 = DIRECTION ( 'NONE',  ( 0.000000000000000000, 0.000000000000000000, -1.000000000000000000 ) ) ;
#59518 = FACE_OUTER_BOUND ( 'NONE', #35279, .T. ) ;
#59517 = AXIS2_PLACEMENT_3D ( 'NONE', #6918, #58788, #37490 ) ;
#59519 = AXIS2_PLACEMENT_3D ( 'NONE', #8699, #29303, #14324 ) ;
#59520 = CIRCLE ( 'NONE', #15861, 5.000000000000001776 ) ;
#59521 = AXIS2_PLACEMENT_3D ( 'NONE', #40523, #10584, #60154 ) ;
#59522 = VERTEX_POINT ( 'NONE', #65124 ) ;
#59523 = CARTESIAN_POINT ( 'NONE',  ( 2.000000000000001776, 6.164400007374783108, 2.900694413976516728 ) ) ;
#59524 = CARTESIAN_POINT ( 'NONE',  ( -35.00000000000000000, -9.700295462048607931, -7.376655759824990000 ) ) ;
#59525 = ORIENTED_EDGE ( 'NONE', *, *, #3625, .T. ) ;
#59526 = CARTESIAN_POINT ( 'NONE',  ( 2.770579946183333142, 7.230573341413149002, 2.954332771348846087 ) ) ;
#59527 = DIRECTION ( 'NONE',  ( 0.000000000000000000, -0.01356324068817998940, 0.9999080150203990547 ) ) ;
#59528 = CYLINDRICAL_SURFACE ( 'NONE', #33522, 8.549672981451799103 ) ;
#59529 = ORIENTED_EDGE ( 'NONE', *, *, #43699, .F. ) ;
#59530 = ORIENTED_EDGE ( 'NONE', *, *, #59477, .F. ) ;
#59531 = CARTESIAN_POINT ( 'NONE',  ( 2.941278708680199916, 6.021511413163961990, 1.198640839021329452 ) ) ;
#59532 = EDGE_CURVE ( 'NONE', #1460, #42144, #23403, .T. ) ;
#59533 = ORIENTED_EDGE ( 'NONE', *, *, #14342, .F. ) ;
#59534 = CARTESIAN_POINT ( 'NONE',  ( 0.000000000000000000, 3.805198749487436416, 5.799611601383225512 ) ) ;
#59535 = ORIENTED_EDGE ( 'NONE', *, *, #51506, .T. ) ;
#59536 = ORIENTED_EDGE ( 'NONE', *, *, #50996, .F. ) ;
#59537 = ORIENTED_EDGE ( 'NONE', *, *, #41849, .F. ) ;
#59538 = CIRCLE ( 'NONE', #62693, 5.000000000000001776 ) ;
#59539 = CARTESIAN_POINT ( 'NONE',  ( 0.2650492433740059273, 11.54478237753292014, 4.084772052580635915 ) ) ;
#59540 = CARTESIAN_POINT ( 'NONE',  ( -3.683412895348672667, -30.77133338175875465, -15.02788192792846189 ) ) ;
#59541 = DIRECTION ( 'NONE',  ( 0.000000000000000000, -0.01356324068817998940, 0.9999080150203990547 ) ) ;
#59542 = DIRECTION ( 'NONE',  ( -1.000000000000000000, -0.000000000000000000, -0.000000000000000000 ) ) ;
#59543 = CARTESIAN_POINT ( 'NONE',  ( -35.00000000000000000, -7.817610399097453922, -8.766823244862070652 ) ) ;
#59544 = EDGE_LOOP ( 'NONE', ( #6248, #49522, #51678, #13582 ) ) ;
#59545 = AXIS2_PLACEMENT_3D ( 'NONE', #28467, #2233, #32465 ) ;
#59546 = CARTESIAN_POINT ( 'NONE',  ( 0.9232167919969114234, 10.99620217063216465, 5.871274944231739568 ) ) ;
#59547 = ORIENTED_EDGE ( 'NONE', *, *, #15999, .T. ) ;
#59548 = CYLINDRICAL_SURFACE ( 'NONE', #31664, 2.899999999999994582 ) ;
#59549 = CARTESIAN_POINT ( 'NONE',  ( -18.07087328174625895, -5.729890374228451044, -12.22671232969771715 ) ) ;
#59550 = VERTEX_POINT ( 'NONE', #54181 ) ;
#59551 = DIRECTION ( 'NONE',  ( 0.000000000000000000, 0.7196168960969766548, 0.6943713148249667233 ) ) ;
#59552 = DIRECTION ( 'NONE',  ( 0.3865475372811021382, -0.8598319252293120663, -0.3335716741247219952 ) ) ;
#59553 = AXIS2_PLACEMENT_3D ( 'NONE', #63212, #59542, #54233 ) ;
#59554 = CARTESIAN_POINT ( 'NONE',  ( 2.000000000000001776, -6.997684042076874000, -2.698595569414309114 ) ) ;
#59555 = EDGE_CURVE ( 'NONE', #31409, #30664, #36137, .T. ) ;
#59556 = ORIENTED_EDGE ( 'NONE', *, *, #31916, .T. ) ;
#59557 = ORIENTED_EDGE ( 'NONE', *, *, #52799, .F. ) ;
#59558 = CARTESIAN_POINT ( 'NONE',  ( -25.00000000000000355, -30.00000000000000000, 1.530808498934191521E-15 ) ) ;
#59559 = EDGE_CURVE ( 'NONE', #26907, #32446, #65442, .T. ) ;
#59560 = VECTOR ( 'NONE', #54569, 1000.000000000000000 ) ;
#59561 = VERTEX_POINT ( 'NONE', #43873 ) ;
#59562 = CARTESIAN_POINT ( 'NONE',  ( -26.80268169419326085, -12.44861804319972265, 5.223704780996759389 ) ) ;
#59563 = CARTESIAN_POINT ( 'NONE',  ( -37.00000000000000711, 1.771820996347319710, -11.61175578952784448 ) ) ;
#59564 = CARTESIAN_POINT ( 'NONE',  ( -30.18541646480390384, -1.416020129149325513, 13.42553116244798517 ) ) ;
#59565 = ADVANCED_FACE ( 'NONE', ( #64782 ), #29871, .T. ) ;
#59567 = VECTOR ( 'NONE', #57378, 1000.000000000000000 ) ;
#59566 = CARTESIAN_POINT ( 'NONE',  ( -2.924554904731178961, 11.04673857066214815, 4.702770982435475311 ) ) ;
#59568 = CARTESIAN_POINT ( 'NONE',  ( 13.10189188732837628, 9.774122605474259373, -6.975859618942914508 ) ) ;
#59569 = ORIENTED_EDGE ( 'NONE', *, *, #56543, .F. ) ;
#59570 = CARTESIAN_POINT ( 'NONE',  ( -35.05175862995318425, -0.01212835938694395432, 0.003331684148533478607 ) ) ;
#59571 = CARTESIAN_POINT ( 'NONE',  ( 1.287602823386241324, 1.639728374786390663, 12.47973441446148257 ) ) ;
#59572 = AXIS2_PLACEMENT_3D ( 'NONE', #18115, #3505, #9416 ) ;
#59573 = CIRCLE ( 'NONE', #30880, 2.899999999999995914 ) ;
#59574 = CARTESIAN_POINT ( 'NONE',  ( -25.00000000000000355, -30.00000000000000000, 1.530808498934191521E-15 ) ) ;
#59575 = CIRCLE ( 'NONE', #9667, 25.00000000000000000 ) ;
#59576 = CARTESIAN_POINT ( 'NONE',  ( 2.440552418640496768, -5.099602138956240260, 5.770332237304425682 ) ) ;
#59577 = DIRECTION ( 'NONE',  ( -0.000000000000000000, -1.000000000000000000, -0.000000000000000000 ) ) ;
#59578 = DIRECTION ( 'NONE',  ( 1.000000000000000000, 0.000000000000000000, 0.000000000000000000 ) ) ;
#59579 = CARTESIAN_POINT ( 'NONE',  ( 2.000000000000001776, 0.000000000000000000, 0.000000000000000000 ) ) ;
#59580 = AXIS2_PLACEMENT_3D ( 'NONE', #57493, #47512, #41513 ) ;
#59581 = CIRCLE ( 'NONE', #54279, 12.74999999999999822 ) ;
#59582 = EDGE_CURVE ( 'NONE', #2444, #65068, #17030, .T. ) ;
#59583 = ORIENTED_EDGE ( 'NONE', *, *, #50001, .T. ) ;
#59584 = CARTESIAN_POINT ( 'NONE',  ( 37.00000000000000711, 1.488153103996963100, -11.65150730582935523 ) ) ;
#59585 = CIRCLE ( 'NONE', #30905, 4.999999999999999112 ) ;
#59586 = CIRCLE ( 'NONE', #24550, 11.99999999999998579 ) ;
#59587 = ADVANCED_FACE ( 'NONE', ( #39197 ), #19906, .T. ) ;
#59588 = ORIENTED_EDGE ( 'NONE', *, *, #24116, .T. ) ;
#59589 = CARTESIAN_POINT ( 'NONE',  ( 0.2647959493198558945, 1.981611532097707240, -12.08462848595693018 ) ) ;
#59590 = CARTESIAN_POINT ( 'NONE',  ( 2.000000000000001776, 4.570217215903443986, -5.218059682435596258 ) ) ;
#59591 = CARTESIAN_POINT ( 'NONE',  ( 2.705197763288546664, -7.410249563424439856, 2.399370654839244832 ) ) ;
#59592 = DIRECTION ( 'NONE',  ( 1.000000000000000000, 0.000000000000000000, 0.000000000000000000 ) ) ;
#59593 = ORIENTED_EDGE ( 'NONE', *, *, #32560, .T. ) ;
#59594 = AXIS2_PLACEMENT_3D ( 'NONE', #22838, #22500, #7518 ) ;
#59595 = EDGE_CURVE ( 'NONE', #52466, #54224, #46793, .T. ) ;
#59596 = VERTEX_POINT ( 'NONE', #55486 ) ;
#59597 = VERTEX_POINT ( 'NONE', #14564 ) ;
#59598 = B_SPLINE_CURVE_WITH_KNOTS ( 'NONE', 3,
 ( #10145, #23905, #18602, #28538, #65650, #44164, #23231, #59456, #45715, #34175, #54485, #43493, #38857, #48843, #50404, #25118, #3291, #4849, #59150, #45383, #13561, #40385 ),
 .UNSPECIFIED., .F., .F.,
 ( 4, 3, 3, 3, 3, 3, 3, 4 ),
 ( 8.940560153363745023E-19, 4.449119708436977073E-05, 6.626296329540607203E-05, 8.803456484962844653E-05, 0.0001098060367612834013, 0.0001315774408628557881, 0.0001760698110411249636, 0.0001829697163287847303 ),
 .UNSPECIFIED. ) ;
#59599 = CARTESIAN_POINT ( 'NONE',  ( 0.3053067050349173583, -7.702091166065946126, -9.538004819224426001 ) ) ;
#59600 = ORIENTED_EDGE ( 'NONE', *, *, #45104, .T. ) ;
#59601 = CARTESIAN_POINT ( 'NONE',  ( 35.00000000000000000, -7.251710744571640888, -9.240395740215610942 ) ) ;
#59602 = CYLINDRICAL_SURFACE ( 'NONE', #35745, 5.000000000000000888 ) ;
#59603 = CARTESIAN_POINT ( 'NONE',  ( 0.3474126878361814552, -9.233692382639425489, 8.085727498271742419 ) ) ;
#59604 = AXIS2_PLACEMENT_3D ( 'NONE', #30981, #46606, #10364 ) ;
#59605 = CARTESIAN_POINT ( 'NONE',  ( -47.00000000000000711, 0.000000000000000000, 0.000000000000000000 ) ) ;
#59606 = ORIENTED_EDGE ( 'NONE', *, *, #46278, .T. ) ;
#59607 = DIRECTION ( 'NONE',  ( 0.000000000000000000, -0.8989688749565202253, -0.4380125133593882336 ) ) ;
#59608 = CARTESIAN_POINT ( 'NONE',  ( 0.9290584433855355595, -28.11997881881914196, -13.91374373156083166 ) ) ;
#59609 = DIRECTION ( 'NONE',  ( -1.000000000000000000, 0.000000000000000000, 0.000000000000000000 ) ) ;
#59611 = EDGE_LOOP ( 'NONE', ( #22986, #27886, #13279, #38311 ) ) ;
#59610 = CARTESIAN_POINT ( 'NONE',  ( 37.00000000000000711, -9.926225166346981155, 6.280308599560240346 ) ) ;
#59613 = VECTOR ( 'NONE', #21130, 1000.000000000000000 ) ;
#59612 = CARTESIAN_POINT ( 'NONE',  ( 0.3665391374699472626, 5.911453292029753115, -10.76665847464306403 ) ) ;
#59614 = EDGE_CURVE ( 'NONE', #21230, #28220, #14258, .T. ) ;
#59615 = EDGE_CURVE ( 'NONE', #12134, #36790, #40170, .T. ) ;
#59616 = ORIENTED_EDGE ( 'NONE', *, *, #561, .F. ) ;
#59617 = DIRECTION ( 'NONE',  ( 0.000000000000000000, -0.01356324068817998940, 0.9999080150203990547 ) ) ;
#59618 = ORIENTED_EDGE ( 'NONE', *, *, #19827, .F. ) ;
#59619 = CARTESIAN_POINT ( 'NONE',  ( 37.00000000000000711, -4.603882218679472338, 10.80631716521671493 ) ) ;
#59620 = CARTESIAN_POINT ( 'NONE',  ( -35.05012975565874456, 0.01323209221895734096, 0.004360246756757623493 ) ) ;
#59621 = ADVANCED_FACE ( 'NONE', ( #25545 ), #45837, .T. ) ;
#59622 = DIRECTION ( 'NONE',  ( 1.000000000000000000, -0.000000000000000000, 0.000000000000000000 ) ) ;
#59623 = DIRECTION ( 'NONE',  ( 0.000000000000000000, 0.000000000000000000, 1.000000000000000000 ) ) ;
#59624 = VECTOR ( 'NONE', #39206, 1000.000000000000000 ) ;
#59625 = AXIS2_PLACEMENT_3D ( 'NONE', #6829, #12433, #32396 ) ;
#59626 = CARTESIAN_POINT ( 'NONE',  ( 0.2834382757448019041, 9.514772331577425746, 7.719209397492011071 ) ) ;
#59627 = DIRECTION ( 'NONE',  ( -1.000000000000000000, 0.000000000000000000, -0.000000000000000000 ) ) ;
#59628 = DIRECTION ( 'NONE',  ( 1.000000000000000000, 0.000000000000000000, 0.000000000000000000 ) ) ;
#59630 = ORIENTED_EDGE ( 'NONE', *, *, #51300, .F. ) ;
#59629 = DIRECTION ( 'NONE',  ( -1.000000000000000000, 0.000000000000000000, 0.000000000000000000 ) ) ;
#59631 =( BOUNDED_SURFACE ( )  B_SPLINE_SURFACE ( 3, 1, ( 
 ( #33320, #53623 ),
 ( #3081, #23342 ),
 ( #55485, #4953 ),
 ( #30845, #295 ) ),
 .UNSPECIFIED., .F., .F., .F. ) 
 B_SPLINE_SURFACE_WITH_KNOTS ( ( 4, 4 ),
 ( 2, 2 ),
 ( 0.000000000000000000, 1.000000000000000000 ),
 ( 0.000000000000000000, 1.000000000000000000 ),
 .UNSPECIFIED. ) 
 GEOMETRIC_REPRESENTATION_ITEM ( )  RATIONAL_B_SPLINE_SURFACE ( (
 ( 1.000000000000000000, 1.000000000000000000),
 ( 0.6933888150995267674, 0.9895912004443193632),
 ( 0.6933888150995267674, 0.9895912004443193632),
 ( 1.000000000000000000, 1.000000000000000000) ) ) 
 REPRESENTATION_ITEM ( '' )  SURFACE ( )  );
#59632 = ORIENTED_EDGE ( 'NONE', *, *, #5528, .F. ) ;
#59633 = CARTESIAN_POINT ( 'NONE',  ( 36.00000000000000711, 8.624332853796058629, -9.390600770288022758 ) ) ;
#59634 = ORIENTED_EDGE ( 'NONE', *, *, #53569, .T. ) ;
#59635 = ORIENTED_EDGE ( 'NONE', *, *, #36975, .F. ) ;
#59636 = CARTESIAN_POINT ( 'NONE',  ( 5.514970785353741078, 0.0003039746380528286578, 0.004713149585127535644 ) ) ;
#59637 = DIRECTION ( 'NONE',  ( 1.000000000000000000, 0.000000000000000000, -0.000000000000000000 ) ) ;
#59638 = CARTESIAN_POINT ( 'NONE',  ( 0.2739690278137234536, -10.51531306167491486, 6.282352088166227588 ) ) ;
#59640 = AXIS2_PLACEMENT_3D ( 'NONE', #44708, #44076, #14130 ) ;
#59639 = CARTESIAN_POINT ( 'NONE',  ( -22.31099767395441091, 1.667781795950537882, -3.395517675085595766 ) ) ;
#59641 = ADVANCED_FACE ( 'NONE', ( #56125 ), #61774, .T. ) ;
#59642 = AXIS2_PLACEMENT_3D ( 'NONE', #23345, #39281, #3084 ) ;
#59643 = CARTESIAN_POINT ( 'NONE',  ( 0.2833330754217378566, 10.71034013638387528, -5.950193237802298363 ) ) ;
#59644 = CYLINDRICAL_SURFACE ( 'NONE', #40826, 4.999999999999999112 ) ;
#59645 = AXIS2_PLACEMENT_3D ( 'NONE', #13283, #54510, #28897 ) ;
#59646 = EDGE_CURVE ( 'NONE', #19021, #53819, #20228, .T. ) ;
#59647 = VERTEX_POINT ( 'NONE', #30524 ) ;
#59648 = FACE_BOUND ( 'NONE', #53835, .T. ) ;
#59649 = AXIS2_PLACEMENT_3D ( 'NONE', #4159, #50039, #24768 ) ;
#59650 = DIRECTION ( 'NONE',  ( 1.000000000000000000, 0.000000000000000000, 0.000000000000000000 ) ) ;
#59651 = CARTESIAN_POINT ( 'NONE',  ( -22.27218376572352554, 2.099017427146268044, 3.026314224080933091 ) ) ;
#59652 = ORIENTED_EDGE ( 'NONE', *, *, #51653, .F. ) ;
#59653 = CIRCLE ( 'NONE', #49039, 12.18649999999999878 ) ;
#59654 = CARTESIAN_POINT ( 'NONE',  ( -7.952749643240611732, -1.708398112507050204, 13.39193977470096542 ) ) ;
#59655 = DIRECTION ( 'NONE',  ( -1.000000000000000000, 0.000000000000000000, 0.000000000000000000 ) ) ;
#59656 = CIRCLE ( 'NONE', #34009, 12.18650000000000233 ) ;
#59657 = AXIS2_PLACEMENT_3D ( 'NONE', #955, #30232, #51187 ) ;
#59658 = ORIENTED_EDGE ( 'NONE', *, *, #14786, .F. ) ;
#59659 = PLANE ( 'NONE',  #19240 ) ;
#59660 = CARTESIAN_POINT ( 'NONE',  ( 29.03457606387295087, 4.854210015632069997, 10.97436308512422265 ) ) ;
#59661 = CARTESIAN_POINT ( 'NONE',  ( -37.00000000000000711, 11.02904044024209185, -4.041347439435899247 ) ) ;
#59662 = VECTOR ( 'NONE', #32730, 1000.000000000000000 ) ;
#59663 = CIRCLE ( 'NONE', #1242, 12.18649999999999700 ) ;
#59664 = AXIS2_PLACEMENT_3D ( 'NONE', #64311, #39042, #18114 ) ;
#59665 = DIRECTION ( 'NONE',  ( 0.000000000000000000, 0.01356324068817991828, -0.9999080150203990547 ) ) ;
#59666 = CARTESIAN_POINT ( 'NONE',  ( 35.00000000000000000, 8.295159312811978936, 8.927548052240801724 ) ) ;
#59667 = EDGE_CURVE ( 'NONE', #6215, #44872, #51507, .T. ) ;
#59668 = ORIENTED_EDGE ( 'NONE', *, *, #44516, .F. ) ;
#59669 = CARTESIAN_POINT ( 'NONE',  ( -35.04709527796842394, -0.005220632201001842998, -0.01120703303053409428 ) ) ;
#59670 = DIRECTION ( 'NONE',  ( 0.000000000000000000, 0.9999080150203989437, 0.01356324068818338426 ) ) ;
#59671 = DIRECTION ( 'NONE',  ( 0.8405098440481681976, 0.000000000000000000, -0.5417962735734934698 ) ) ;
#59672 = VERTEX_POINT ( 'NONE', #16566 ) ;
#59673 = CYLINDRICAL_SURFACE ( 'NONE', #14870, 4.999999999999999112 ) ;
#59674 = CARTESIAN_POINT ( 'NONE',  ( 2.241451721903215066, 6.581017239736967284, 3.869794645251144694 ) ) ;
#59675 = ORIENTED_EDGE ( 'NONE', *, *, #34046, .T. ) ;
#59676 = ORIENTED_EDGE ( 'NONE', *, *, #14707, .F. ) ;
#59677 = LINE ( 'NONE', #39374, #36343 ) ;
#59678 = VECTOR ( 'NONE', #65263, 1000.000000000000000 ) ;
#59679 = EDGE_CURVE ( 'NONE', #58379, #58530, #60228, .T. ) ;
#59680 = EDGE_LOOP ( 'NONE', ( #41627, #19540, #6771, #36307 ) ) ;
#59681 = AXIS2_PLACEMENT_3D ( 'NONE', #24077, #45659, #35345 ) ;
#59682 = DIRECTION ( 'NONE',  ( 0.000000000000000000, 0.000000000000000000, 1.000000000000000000 ) ) ;
#59683 = DIRECTION ( 'NONE',  ( 0.000000000000000000, -0.8696919319575239227, -0.4935949184179166394 ) ) ;
#59684 = CARTESIAN_POINT ( 'NONE',  ( -17.54726996257253191, 25.00000000000000000, 3.865003848717349033 ) ) ;
#59685 = CARTESIAN_POINT ( 'NONE',  ( -47.00000000000000711, 0.000000000000000000, 0.000000000000000000 ) ) ;
#59686 = VECTOR ( 'NONE', #29994, 1000.000000000000000 ) ;
#59687 = CARTESIAN_POINT ( 'NONE',  ( -22.30625920655495165, -3.403091720605013748, -1.672644928563079780 ) ) ;
#59689 = ORIENTED_EDGE ( 'NONE', *, *, #51535, .F. ) ;
#59688 = DIRECTION ( 'NONE',  ( -0.8758382566188793739, 0.4826047536471247956, 0.000000000000000000 ) ) ;
#59690 = DIRECTION ( 'NONE',  ( 0.000000000000000000, 0.000000000000000000, 1.000000000000000000 ) ) ;
#59691 = VERTEX_POINT ( 'NONE', #25891 ) ;
#59692 = CARTESIAN_POINT ( 'NONE',  ( -22.71097035706202405, -2.846599994298329328, 4.089776368546542251 ) ) ;
#59693 = VECTOR ( 'NONE', #10226, 1000.000000000000000 ) ;
#59694 = ORIENTED_EDGE ( 'NONE', *, *, #56882, .T. ) ;
#59695 = VERTEX_POINT ( 'NONE', #51167 ) ;
#59696 = DIRECTION ( 'NONE',  ( -0.9854502544271372955, 0.000000000000000000, -0.1699641022377680610 ) ) ;
#59697 = B_SPLINE_CURVE_WITH_KNOTS ( 'NONE', 3,
 ( #55826, #60467, #14892, #35184, #44508, #39534, #10251, #30531, #65763, #20233 ),
 .UNSPECIFIED., .F., .F.,
 ( 4, 3, 3, 4 ),
 ( 5.401523115762577292E-05, 0.0008136511341527794677, 0.004068255670953088016, 0.005063778443040924809 ),
 .UNSPECIFIED. ) ;
#59698 = CARTESIAN_POINT ( 'NONE',  ( -7.454036404615679956, -28.85515183291106212, 12.27947133142187219 ) ) ;
#59699 = CARTESIAN_POINT ( 'NONE',  ( -24.75879207840611684, 11.63908045720823736, 6.841945026260960461 ) ) ;
#59700 = CARTESIAN_POINT ( 'NONE',  ( 22.86323487647331021, 2.804901635794770254, 11.66983792800902542 ) ) ;
#59701 = FACE_OUTER_BOUND ( 'NONE', #4321, .T. ) ;
#59702 = CARTESIAN_POINT ( 'NONE',  ( 2.263328370259782840, 5.944174889969469078, 4.802372801875639752 ) ) ;
#59703 = ORIENTED_EDGE ( 'NONE', *, *, #64347, .F. ) ;
#59704 = AXIS2_PLACEMENT_3D ( 'NONE', #29434, #13800, #34088 ) ;
#59705 = ORIENTED_EDGE ( 'NONE', *, *, #61789, .T. ) ;
#59706 = DIRECTION ( 'NONE',  ( -1.000000000000000000, 0.000000000000000000, 0.000000000000000000 ) ) ;
#59707 = ORIENTED_EDGE ( 'NONE', *, *, #43434, .T. ) ;
#59709 = AXIS2_PLACEMENT_3D ( 'NONE', #53049, #37759, #32740 ) ;
#59708 = DIRECTION ( 'NONE',  ( 0.000000000000000000, 0.000000000000000000, 1.000000000000000000 ) ) ;
#59710 = CARTESIAN_POINT ( 'NONE',  ( -10.48620311856347875, -9.720786832536937538, 7.036071585506805448 ) ) ;
#59711 = CARTESIAN_POINT ( 'NONE',  ( 0.000000000000000000, -1.754183803416586196, 6.711026108862235162 ) ) ;
#59712 = DIRECTION ( 'NONE',  ( 0.000000000000000000, -0.01356324068817992175, 0.9999080150203990547 ) ) ;
#59713 = EDGE_CURVE ( 'NONE', #50166, #21169, #35, .T. ) ;
#59714 = CIRCLE ( 'NONE', #31030, 12.75000000000000178 ) ;
#59715 = DIRECTION ( 'NONE',  ( 0.000000000000000000, -0.01356324068818000848, 0.9999080150203990547 ) ) ;
#59716 = VECTOR ( 'NONE', #62662, 1000.000000000000000 ) ;
#59717 = CARTESIAN_POINT ( 'NONE',  ( 37.00000000000000711, -8.534258022646033837, 8.699265615723071221 ) ) ;
#59718 = ORIENTED_EDGE ( 'NONE', *, *, #39032, .T. ) ;
#59719 = VERTEX_POINT ( 'NONE', #40506 ) ;
#59720 = CARTESIAN_POINT ( 'NONE',  ( -35.00000000000000000, 0.000000000000000000, 0.000000000000000000 ) ) ;
#59721 = DIRECTION ( 'NONE',  ( 0.000000000000000000, -0.01356324068817991828, 0.9999080150203990547 ) ) ;
#59722 = LINE ( 'NONE', #54421, #42560 ) ;
#59723 = AXIS2_PLACEMENT_3D ( 'NONE', #1561, #17494, #42394 ) ;
#59724 = EDGE_CURVE ( 'NONE', #12098, #60025, #25217, .T. ) ;
#59725 = CIRCLE ( 'NONE', #39539, 12.18649999999999878 ) ;
#59726 = DIRECTION ( 'NONE',  ( 0.000000000000000000, 0.01356324068817998940, -0.9999080150203990547 ) ) ;
#59727 = DIRECTION ( 'NONE',  ( 0.000000000000000000, -0.01356324068817992175, 0.9999080150203990547 ) ) ;
#59728 = CIRCLE ( 'NONE', #267, 6.936499999999991672 ) ;
#59729 = CARTESIAN_POINT ( 'NONE',  ( -10.66166322600637173, -5.805694913916275901, -10.50405896137098161 ) ) ;
#59730 = DIRECTION ( 'NONE',  ( -1.000000000000000000, 0.000000000000000000, 0.000000000000000000 ) ) ;
#59731 = AXIS2_PLACEMENT_3D ( 'NONE', #54139, #58481, #27890 ) ;
#59732 = CARTESIAN_POINT ( 'NONE',  ( 35.00000000000000000, 6.415447294506860132, 11.01837265713066039 ) ) ;
#59733 = CYLINDRICAL_SURFACE ( 'NONE', #58389, 4.999999999999999112 ) ;
#59734 = ORIENTED_EDGE ( 'NONE', *, *, #56617, .F. ) ;
#59735 = CARTESIAN_POINT ( 'NONE',  ( -36.00000000000000711, -12.38385022362079724, -3.033604067594711129 ) ) ;
#59736 = CARTESIAN_POINT ( 'NONE',  ( -35.00000000000000000, -2.346765782874520312, 11.95840593935200680 ) ) ;
#59737 = CYLINDRICAL_SURFACE ( 'NONE', #33327, 4.999999999999998224 ) ;
#59738 = CARTESIAN_POINT ( 'NONE',  ( 2.507146904658100084, -6.577532285019736413, -4.047319006787544637 ) ) ;
#59739 = AXIS2_PLACEMENT_3D ( 'NONE', #64755, #34516, #39503 ) ;
#59740 = CARTESIAN_POINT ( 'NONE',  ( -27.45775109278351067, -8.499184579339635448, -8.471355351200609007 ) ) ;
#59741 = EDGE_CURVE ( 'NONE', #35230, #15987, #46486, .T. ) ;
#59742 = ORIENTED_EDGE ( 'NONE', *, *, #97, .T. ) ;
#59743 = CARTESIAN_POINT ( 'NONE',  ( 2.251152103363645018, -2.494172441821545405, 7.218942724308482717 ) ) ;
#59744 = CARTESIAN_POINT ( 'NONE',  ( 37.00000000000000711, -11.70009620280412399, -1.039216533672868481 ) ) ;
#59745 = CARTESIAN_POINT ( 'NONE',  ( -10.20982488791560883, -26.83227745022078992, -13.82162602233992565 ) ) ;
#59746 = ORIENTED_EDGE ( 'NONE', *, *, #57144, .F. ) ;
#59747 = EDGE_CURVE ( 'NONE', #6336, #21047, #4954, .T. ) ;
#59748 = CARTESIAN_POINT ( 'NONE',  ( 1.287602823385640693, -6.765713844064606519, 10.61402828236298213 ) ) ;
#59749 = CARTESIAN_POINT ( 'NONE',  ( -28.24693446298985577, -12.60603044485271873, -4.840642766324885216 ) ) ;
#59750 = DIRECTION ( 'NONE',  ( 1.000000000000000000, 0.000000000000000000, 0.000000000000000000 ) ) ;
#59751 = AXIS2_PLACEMENT_3D ( 'NONE', #20078, #15078, #35358 ) ;
#59752 = AXIS2_PLACEMENT_3D ( 'NONE', #59204, #3026, #13621 ) ;
#59753 = DIRECTION ( 'NONE',  ( -0.000000000000000000, -1.000000000000000000, -0.000000000000000000 ) ) ;
#59754 = CARTESIAN_POINT ( 'NONE',  ( -7.971167194659495969, -8.542028475013285771, -10.47297933864158104 ) ) ;
#59755 = VECTOR ( 'NONE', #43438, 1000.000000000000114 ) ;
#59756 = EDGE_CURVE ( 'NONE', #11939, #26744, #26525, .T. ) ;
#59757 = CARTESIAN_POINT ( 'NONE',  ( 1.459561108995800272, 12.32692860927524769, -2.815016945601904297 ) ) ;
#59758 = ORIENTED_EDGE ( 'NONE', *, *, #24873, .F. ) ;
#59759 = CARTESIAN_POINT ( 'NONE',  ( 2.305787727787085295, -7.249469779319927198, 2.461236246751046242 ) ) ;
#59760 = CARTESIAN_POINT ( 'NONE',  ( 35.00000000000000000, 3.093009498343925134, -11.78745411414841016 ) ) ;
#59761 = DIRECTION ( 'NONE',  ( 0.000000000000000000, 0.7790879021242487212, -0.6269146997508011632 ) ) ;
#59762 = CARTESIAN_POINT ( 'NONE',  ( 2.653899356900494055, -4.792827201941008752, 6.118160465319252062 ) ) ;
#59763 = CARTESIAN_POINT ( 'NONE',  ( 2.242819959140645025, 7.536009875295354377, -1.224821922055896906 ) ) ;
#59764 = CARTESIAN_POINT ( 'NONE',  ( 2.241352910868909643, -3.744764251557037849, 6.652881166698498383 ) ) ;
#59765 = EDGE_CURVE ( 'NONE', #48378, #37589, #54603, .T. ) ;
#59766 = CARTESIAN_POINT ( 'NONE',  ( -30.18541646480307961, -1.416020129149133888, -11.91616074890920807 ) ) ;
#59767 = CARTESIAN_POINT ( 'NONE',  ( 2.244591118395375062, 1.219892024453471890, -7.537402265770549725 ) ) ;
#59768 = ORIENTED_EDGE ( 'NONE', *, *, #57948, .F. ) ;
#59769 = ORIENTED_EDGE ( 'NONE', *, *, #55307, .F. ) ;
#59770 = CARTESIAN_POINT ( 'NONE',  ( -18.25006854224444908, -9.443202773001939221, -7.404452808139720510 ) ) ;
#59771 = CIRCLE ( 'NONE', #8793, 12.18650000000000233 ) ;
#59772 = ORIENTED_EDGE ( 'NONE', *, *, #35210, .T. ) ;
#59773 = AXIS2_PLACEMENT_3D ( 'NONE', #25312, #50925, #50281 ) ;
#59774 = CARTESIAN_POINT ( 'NONE',  ( 1.719304012339881282, -12.20344780066076318, 3.626341562669963992 ) ) ;
#59775 = EDGE_CURVE ( 'NONE', #49587, #24086, #1144, .T. ) ;
#59776 = CARTESIAN_POINT ( 'NONE',  ( -18.10941110424452916, -9.537088721069792996, 9.555689318548472144 ) ) ;
#59777 = VERTEX_POINT ( 'NONE', #6595 ) ;
#59778 = CARTESIAN_POINT ( 'NONE',  ( 0.000000000000000000, 0.000000000000000000, 0.000000000000000000 ) ) ;
#59779 = DIRECTION ( 'NONE',  ( 1.000000000000000000, 0.000000000000000000, -0.000000000000000000 ) ) ;
#59780 = DIRECTION ( 'NONE',  ( 1.000000000000000000, 0.000000000000000000, 0.000000000000000000 ) ) ;
#59781 = VERTEX_POINT ( 'NONE', #58112 ) ;
#59782 = ORIENTED_EDGE ( 'NONE', *, *, #15337, .T. ) ;
#59783 = CARTESIAN_POINT ( 'NONE',  ( 2.263328370261528555, -7.228205514767154227, -2.479726736363712103 ) ) ;
#59784 = LINE ( 'NONE', #38514, #40761 ) ;
#59785 = ORIENTED_EDGE ( 'NONE', *, *, #46244, .F. ) ;
#59786 = CARTESIAN_POINT ( 'NONE',  ( -27.65870282641429867, -11.28224200227462859, -4.098090116028304308 ) ) ;
#59787 = ORIENTED_EDGE ( 'NONE', *, *, #4406, .T. ) ;
#59788 = CARTESIAN_POINT ( 'NONE',  ( -19.55198024779261345, -3.902068674853249153, -11.34897822738861883 ) ) ;
#59789 = CYLINDRICAL_SURFACE ( 'NONE', #11410, 6.095312090839646757 ) ;
#59790 = CARTESIAN_POINT ( 'NONE',  ( 2.305787727787085295, -3.971363876084009537, 6.545285700970515208 ) ) ;
#59791 = PLANE ( 'NONE',  #9336 ) ;
#59792 = DIRECTION ( 'NONE',  ( 0.000000000000000000, 0.000000000000000000, 1.000000000000000000 ) ) ;
#59793 = ORIENTED_EDGE ( 'NONE', *, *, #55556, .T. ) ;
#59794 = CARTESIAN_POINT ( 'NONE',  ( 2.290907136833255198, -1.488079974904993996, 7.504812001538600619 ) ) ;
#59795 = CARTESIAN_POINT ( 'NONE',  ( 0.2653519890518161728, 7.871697161810815579, -9.381137101569592573 ) ) ;
#59796 = CARTESIAN_POINT ( 'NONE',  ( 0.2650492594609250574, -9.451471004987384461, 7.786980091309421148 ) ) ;
#59797 = FACE_OUTER_BOUND ( 'NONE', #51677, .T. ) ;
#59799 = CARTESIAN_POINT ( 'NONE',  ( 1.000000000000000888, -6.936109781200700652, 2.853135311045000400 ) ) ;
#59798 = AXIS2_PLACEMENT_3D ( 'NONE', #60479, #4313, #29894 ) ;
#59800 = CARTESIAN_POINT ( 'NONE',  ( 1.198791140420486290, 0.5160125886334614442, -12.54673713002939195 ) ) ;
#59801 = CARTESIAN_POINT ( 'NONE',  ( -27.32337605527166247, 2.988381643048321212, 0.3676050637290654288 ) ) ;
#59802 = DIRECTION ( 'NONE',  ( -1.000000000000000000, 0.000000000000000000, 0.000000000000000000 ) ) ;
#59803 = CIRCLE ( 'NONE', #51327, 7.499999999999988454 ) ;
#59804 = CARTESIAN_POINT ( 'NONE',  ( 35.00000000000000000, 4.705694406421931860E-17, -3.469127814946512892E-15 ) ) ;
#59805 = AXIS2_PLACEMENT_3D ( 'NONE', #19991, #29623, #9672 ) ;
#59806 = EDGE_CURVE ( 'NONE', #8415, #35879, #47851, .T. ) ;
#59807 = AXIS2_PLACEMENT_3D ( 'NONE', #58548, #12973, #33590 ) ;
#59808 = ORIENTED_EDGE ( 'NONE', *, *, #43628, .F. ) ;
#59809 = CARTESIAN_POINT ( 'NONE',  ( 37.00000000000000711, -4.018060380616318206, 11.50504120060946533 ) ) ;
#59810 =( BOUNDED_SURFACE ( )  B_SPLINE_SURFACE ( 3, 1, ( 
 ( #22831, #43087 ),
 ( #17511, #18163 ),
 ( #58749, #52757 ),
 ( #17829, #37782 ) ),
 .UNSPECIFIED., .F., .F., .F. ) 
 B_SPLINE_SURFACE_WITH_KNOTS ( ( 4, 4 ),
 ( 2, 2 ),
 ( 0.000000000000000000, 1.000000000000000000 ),
 ( 0.000000000000000000, 1.000000000000000000 ),
 .UNSPECIFIED. ) 
 GEOMETRIC_REPRESENTATION_ITEM ( )  RATIONAL_B_SPLINE_SURFACE ( (
 ( 1.000000000000000000, 1.000000000000000000),
 ( 0.6933888150995267674, 0.9895912004443193632),
 ( 0.6933888150995267674, 0.9895912004443193632),
 ( 1.000000000000000000, 1.000000000000000000) ) ) 
 REPRESENTATION_ITEM ( '' )  SURFACE ( )  );
#59811 = ORIENTED_EDGE ( 'NONE', *, *, #52170, .F. ) ;
#59812 = CARTESIAN_POINT ( 'NONE',  ( -30.18541646480307961, -1.416020129149133888, -11.91616074890920807 ) ) ;
#59813 = CARTESIAN_POINT ( 'NONE',  ( 2.241311220309555541, -7.501736494813736833, -1.417008678104561659 ) ) ;
#59814 = FACE_OUTER_BOUND ( 'NONE', #24136, .T. ) ;
#59815 = AXIS2_PLACEMENT_3D ( 'NONE', #46969, #21707, #41960 ) ;
#59816 = B_SPLINE_CURVE_WITH_KNOTS ( 'NONE', 3,
 ( #61165, #25250, #65791, #30559, #20263, #50863, #20608, #5656, #9616, #35557, #14597, #19938, #55852, #40544, #40886, #15595, #35859, #29913, #34877, #65475 ),
 .UNSPECIFIED., .F., .F.,
 ( 4, 2, 2, 2, 2, 2, 2, 2, 2, 4 ),
 ( 0.000000000000000000, 0.001138311071655714055, 0.002276622143311428110, 0.003414933214967142382, 0.004553244286622856220, 0.005691555358278570058, 0.006829866429934284763, 0.007399021965762139948, 0.007968177501589996867, 0.009106488573245712440 ),
 .UNSPECIFIED. ) ;
#59817 = CARTESIAN_POINT ( 'NONE',  ( -35.04660725145885891, 0.001288602543501626970, 0.01223081933018644978 ) ) ;
#59818 = CARTESIAN_POINT ( 'NONE',  ( 3.152665057736164123, 5.461013642407259283, 5.761241965767907480 ) ) ;
#59819 = VERTEX_POINT ( 'NONE', #22191 ) ;
#59820 = DIRECTION ( 'NONE',  ( -1.000000000000000000, -1.836970198721029688E-16, 0.000000000000000000 ) ) ;
#59821 = CARTESIAN_POINT ( 'NONE',  ( 3.152665057736245391, 2.258875078500370837, -7.609997527622033076 ) ) ;
#59822 = CARTESIAN_POINT ( 'NONE',  ( 9.270078297875276263, 2.860737070136182059, 11.65636294989809407 ) ) ;
#59823 = CARTESIAN_POINT ( 'NONE',  ( 0.8320506296491596565, 2.535206712041455202, 12.17395768195218331 ) ) ;
#59824 = B_SPLINE_CURVE_WITH_KNOTS ( 'NONE', 3,
 ( #34939, #40267, #35616, #24329, #45938, #40944, #29634, #61224, #39955, #64884, #5373, #60236, #54629, #4400, #20325, #19362, #55909, #40609, #59930 ),
 .UNSPECIFIED., .F., .F.,
 ( 4, 3, 3, 3, 3, 3, 4 ),
 ( 0.000000000000000000, 2.831840207624787838E-05, 4.217266860011569017E-05, 5.602024318565227519E-05, 6.290810168137421878E-05, 9.120440631109840335E-05, 0.0001153103026478316740 ),
 .UNSPECIFIED. ) ;
#59825 = VECTOR ( 'NONE', #24173, 1000.000000000000000 ) ;
#59826 = EDGE_CURVE ( 'NONE', #4955, #29543, #9607, .T. ) ;
#59827 = DIRECTION ( 'NONE',  ( 0.000000000000000000, -1.000000000000000000, 0.000000000000000000 ) ) ;
#59828 = CIRCLE ( 'NONE', #44960, 2.899999999999995914 ) ;
#59829 = VERTEX_POINT ( 'NONE', #48470 ) ;
#59830 = EDGE_CURVE ( 'NONE', #37175, #58284, #35085, .T. ) ;
#59831 = AXIS2_PLACEMENT_3D ( 'NONE', #24961, #45233, #65491 ) ;
#59832 = CARTESIAN_POINT ( 'NONE',  ( 35.00000000000000000, -5.556331110570486231, -11.47561260193575272 ) ) ;
#59833 = ORIENTED_EDGE ( 'NONE', *, *, #42402, .F. ) ;
#59834 = EDGE_CURVE ( 'NONE', #5900, #6107, #6459, .T. ) ;
#59835 = CARTESIAN_POINT ( 'NONE',  ( -2.532614230583026593, 7.965877694534055031, 10.89930238848911337 ) ) ;
#59836 = CARTESIAN_POINT ( 'NONE',  ( 35.00000000000000000, 7.561043153948098450, 9.557269938331469206 ) ) ;
#59837 = CARTESIAN_POINT ( 'NONE',  ( 2.350038591457886739, 7.305692696276214093, -7.710465783964237652 ) ) ;
#59838 = CARTESIAN_POINT ( 'NONE',  ( -37.00000000000000711, -4.041347439435779343, -11.02904044024213270 ) ) ;
#59839 = VECTOR ( 'NONE', #49972, 1000.000000000000000 ) ;
#59840 = ORIENTED_EDGE ( 'NONE', *, *, #27825, .T. ) ;
#59842 = VERTEX_POINT ( 'NONE', #26862 ) ;
#59841 = ADVANCED_FACE ( 'NONE', ( #27844 ), #32805, .T. ) ;
#59843 = CARTESIAN_POINT ( 'NONE',  ( 37.00000000000000711, -11.56998259273180274, -3.827046518385039064 ) ) ;
#59844 = DIRECTION ( 'NONE',  ( -1.000000000000000000, 0.000000000000000000, 0.000000000000000000 ) ) ;
#59845 = LINE ( 'NONE', #34553, #53430 ) ;
#59846 = CARTESIAN_POINT ( 'NONE',  ( 2.258463476537674097, 6.547539277367620869, 3.937122681833869375 ) ) ;
#59847 = CARTESIAN_POINT ( 'NONE',  ( 0.3675815128205894289, 12.27743992903066150, 0.2638082659428850896 ) ) ;
#59848 = CARTESIAN_POINT ( 'NONE',  ( 2.717984159220097062, 6.602931111513763440, -4.139692542159497890 ) ) ;
#59849 = ADVANCED_FACE ( 'NONE', ( #17218 ), #63089, .T. ) ;
#59850 = DIRECTION ( 'NONE',  ( 1.000000000000000000, -0.000000000000000000, -0.000000000000000000 ) ) ;
#59851 = LINE ( 'NONE', #14279, #23324 ) ;
#59852 = ORIENTED_EDGE ( 'NONE', *, *, #23660, .F. ) ;
#59853 = AXIS2_PLACEMENT_3D ( 'NONE', #63627, #38373, #58692 ) ;
#59854 = VERTEX_POINT ( 'NONE', #48148 ) ;
#59855 = ORIENTED_EDGE ( 'NONE', *, *, #28699, .T. ) ;
#59856 = CARTESIAN_POINT ( 'NONE',  ( 1.104777566491140783, -2.644034362100612601, -12.24382064406182735 ) ) ;
#59857 = EDGE_CURVE ( 'NONE', #44559, #62520, #16878, .T. ) ;
#59858 = AXIS2_PLACEMENT_3D ( 'NONE', #13684, #33964, #48965 ) ;
#59859 = FACE_OUTER_BOUND ( 'NONE', #51012, .T. ) ;
#59860 = VERTEX_POINT ( 'NONE', #22870 ) ;
#59861 = LINE ( 'NONE', #15189, #45353 ) ;
#59862 = EDGE_CURVE ( 'NONE', #19519, #18553, #30825, .T. ) ;
#59863 = CYLINDRICAL_SURFACE ( 'NONE', #58705, 11.99999999999999289 ) ;
#59864 = EDGE_LOOP ( 'NONE', ( #37441, #42776, #59990, #28352 ) ) ;
#59865 = CARTESIAN_POINT ( 'NONE',  ( -37.00000000000000711, 1.457575200925721237, -12.66641127287624435 ) ) ;
#59866 = DIRECTION ( 'NONE',  ( 0.000000000000000000, -0.9987865678893271815, 0.04924826701375695226 ) ) ;
#59867 = CARTESIAN_POINT ( 'NONE',  ( -27.08935880048752765, -2.235999130317592343, -0.5666837974575801296 ) ) ;
#59868 = ORIENTED_EDGE ( 'NONE', *, *, #9927, .F. ) ;
#59869 = CIRCLE ( 'NONE', #38638, 12.18649999999999878 ) ;
#59871 = EDGE_CURVE ( 'NONE', #433, #23887, #7218, .T. ) ;
#59870 = VERTEX_POINT ( 'NONE', #42797 ) ;
#59872 = CARTESIAN_POINT ( 'NONE',  ( 35.00000000000000000, 4.705694406421931860E-17, -3.469127814946512892E-15 ) ) ;
#59873 = ORIENTED_EDGE ( 'NONE', *, *, #37572, .F. ) ;
#59874 = CARTESIAN_POINT ( 'NONE',  ( 10.57567362079633355, 8.112553359107785411, 10.79197710481157557 ) ) ;
#59875 = ORIENTED_EDGE ( 'NONE', *, *, #29951, .F. ) ;
#59876 = AXIS2_PLACEMENT_3D ( 'NONE', #1840, #12129, #7457 ) ;
#59877 = VERTEX_POINT ( 'NONE', #63397 ) ;
#59878 = EDGE_LOOP ( 'NONE', ( #31928, #12242, #11202, #40973 ) ) ;
#59879 = CARTESIAN_POINT ( 'NONE',  ( 0.2652384770603662401, 11.48486213386625820, 4.250454630553602620 ) ) ;
#59880 = CIRCLE ( 'NONE', #3602, 12.74999999999999822 ) ;
#59881 = LINE ( 'NONE', #13644, #48557 ) ;
#59882 = CARTESIAN_POINT ( 'NONE',  ( -35.00000000000000000, 3.704519465651306742, 11.60979404548636218 ) ) ;
#59883 = CARTESIAN_POINT ( 'NONE',  ( 1.109979610370801506, -0.4797593171729975792, 12.51859925746135538 ) ) ;
#59884 = VERTEX_POINT ( 'NONE', #47166 ) ;
#59885 = CARTESIAN_POINT ( 'NONE',  ( 2.255723233588950549, -7.132203433012270999, -2.736592204236721670 ) ) ;
#59886 = ORIENTED_EDGE ( 'NONE', *, *, #14548, .F. ) ;
#59887 = CARTESIAN_POINT ( 'NONE',  ( -35.00000000000000000, -0.1414404973751245964, -12.74921544981111055 ) ) ;
#59888 = VECTOR ( 'NONE', #64434, 1000.000000000000000 ) ;
#59889 = FACE_OUTER_BOUND ( 'NONE', #22911, .T. ) ;
#59890 = ORIENTED_EDGE ( 'NONE', *, *, #15319, .T. ) ;
#59891 = CARTESIAN_POINT ( 'NONE',  ( 1.198791140420805812, 9.943044756149616248, -7.669598593074792525 ) ) ;
#59892 = CARTESIAN_POINT ( 'NONE',  ( -35.00000000000000000, 0.000000000000000000, 0.000000000000000000 ) ) ;
#59893 = LINE ( 'NONE', #19967, #8954 ) ;
#59894 = ORIENTED_EDGE ( 'NONE', *, *, #14604, .F. ) ;
#59895 = EDGE_CURVE ( 'NONE', #23681, #65266, #19165, .T. ) ;
#59896 = EDGE_CURVE ( 'NONE', #22857, #45822, #17550, .T. ) ;
#59897 = VECTOR ( 'NONE', #31235, 1000.000000000000000 ) ;
#59898 = ORIENTED_EDGE ( 'NONE', *, *, #62834, .T. ) ;
#59899 = DIRECTION ( 'NONE',  ( 0.000000000000000000, 0.000000000000000000, 1.000000000000000000 ) ) ;
#59900 = ORIENTED_EDGE ( 'NONE', *, *, #35965, .T. ) ;
#59901 = DIRECTION ( 'NONE',  ( -1.000000000000000000, 0.000000000000000000, 0.000000000000000000 ) ) ;
#59902 = CARTESIAN_POINT ( 'NONE',  ( 0.3675815128205894289, 9.574637318041965273, 7.689697408877307794 ) ) ;
#59903 = CARTESIAN_POINT ( 'NONE',  ( 35.00000000000000000, 1.286231064351314624, -12.68495603654572257 ) ) ;
#59904 = DIRECTION ( 'NONE',  ( -1.000000000000000000, 0.000000000000000000, 0.000000000000000000 ) ) ;
#59905 = CARTESIAN_POINT ( 'NONE',  ( 13.33628443002342046, 11.16462474940892236, -4.404581277556346208 ) ) ;
#59906 = ORIENTED_EDGE ( 'NONE', *, *, #12218, .T. ) ;
#59907 = CIRCLE ( 'NONE', #3631, 4.999999999999997335 ) ;
#59908 = EDGE_CURVE ( 'NONE', #26907, #20276, #32964, .T. ) ;
#59909 = AXIS2_PLACEMENT_3D ( 'NONE', #56599, #26012, #2650 ) ;
#59910 = CARTESIAN_POINT ( 'NONE',  ( -35.00000000000000000, -11.72195762423409349, -0.7536123767499773862 ) ) ;
#59911 = CARTESIAN_POINT ( 'NONE',  ( 1.948354844646766448, -10.70340528294945770, -5.347695345041388215 ) ) ;
#59912 = AXIS2_PLACEMENT_3D ( 'NONE', #60234, #9683, #4740 ) ;
#59913 = EDGE_CURVE ( 'NONE', #62432, #11383, #22535, .T. ) ;
#59914 = DIRECTION ( 'NONE',  ( 1.000000000000000000, -0.000000000000000000, 0.000000000000000000 ) ) ;
#59915 = CIRCLE ( 'NONE', #33318, 12.75000000000000178 ) ;
#59916 = CARTESIAN_POINT ( 'NONE',  ( 2.305787727787084407, -5.047606869483094449, 5.756228004061441084 ) ) ;
#59917 = EDGE_CURVE ( 'NONE', #52994, #55534, #6412, .T. ) ;
#59918 = FACE_OUTER_BOUND ( 'NONE', #9971, .T. ) ;
#59919 = CARTESIAN_POINT ( 'NONE',  ( -35.00000000000000000, 0.000000000000000000, 0.000000000000000000 ) ) ;
#59920 = DIRECTION ( 'NONE',  ( 0.000000000000000000, 0.8827602140260332186, -0.4698238015817334245 ) ) ;
#59921 = AXIS2_PLACEMENT_3D ( 'NONE', #43846, #28547, #3300 ) ;
#59922 = ORIENTED_EDGE ( 'NONE', *, *, #4121, .T. ) ;
#59923 = CARTESIAN_POINT ( 'NONE',  ( 37.00000000000000711, 3.287724142101414504, -11.73463472867577373 ) ) ;
#59924 = ORIENTED_EDGE ( 'NONE', *, *, #30170, .F. ) ;
#59925 = CARTESIAN_POINT ( 'NONE',  ( -14.23149639848878678, 7.941839253138335941, -8.998400932456027235 ) ) ;
#59926 = CARTESIAN_POINT ( 'NONE',  ( -22.27706485742869091, -3.662257305743835012, 0.3729136217356029959 ) ) ;
#59927 = CARTESIAN_POINT ( 'NONE',  ( 0.2653519789438769649, 6.142177718873936598, 10.59450269107735565 ) ) ;
#59928 = AXIS2_PLACEMENT_3D ( 'NONE', #25652, #10345, #24675 ) ;
#59929 = EDGE_CURVE ( 'NONE', #58896, #49993, #19023, .T. ) ;
#59930 = CARTESIAN_POINT ( 'NONE',  ( 2.305787727787084407, -1.164987321564681100, -7.566723232958083578 ) ) ;
#59931 = EDGE_LOOP ( 'NONE', ( #11574, #13514, #42039, #56873 ) ) ;
#59932 = EDGE_LOOP ( 'NONE', ( #24972, #36264, #23712, #59175 ) ) ;
#59933 = ORIENTED_EDGE ( 'NONE', *, *, #48893, .T. ) ;
#59934 = CARTESIAN_POINT ( 'NONE',  ( 2.705197763288550217, 2.925192046932006740, -7.218866228162253762 ) ) ;
#59935 = EDGE_CURVE ( 'NONE', #9125, #36890, #12215, .T. ) ;
#59936 = AXIS2_PLACEMENT_3D ( 'NONE', #29677, #30020, #39996 ) ;
#59937 = DIRECTION ( 'NONE',  ( -1.000000000000000000, 0.000000000000000000, 0.000000000000000000 ) ) ;
#59938 = ORIENTED_EDGE ( 'NONE', *, *, #59003, .F. ) ;
#59939 = ADVANCED_FACE ( 'NONE', ( #42132 ), #45101, .T. ) ;
#59940 = CARTESIAN_POINT ( 'NONE',  ( 3.152665057736049103, -0.4801242025610908959, -7.923639299008895520 ) ) ;
#59941 = CARTESIAN_POINT ( 'NONE',  ( 0.000000000000000000, -4.570217215903394248, 5.218059682435592705 ) ) ;
#59942 = CARTESIAN_POINT ( 'NONE',  ( 0.2767916011545360488, -9.260929738915292475, 8.018602152763836699 ) ) ;
#59943 = CARTESIAN_POINT ( 'NONE',  ( 0.000000000000000000, -5.662015959325143122, -4.918493191654053298 ) ) ;
#59944 = EDGE_LOOP ( 'NONE', ( #31141, #51992, #17471, #28202 ) ) ;
#59945 = CARTESIAN_POINT ( 'NONE',  ( 2.000000000000001776, 0.4129979343798200753, -6.800241778083709221 ) ) ;
#59946 = CARTESIAN_POINT ( 'NONE',  ( -2.264138978095799448, -30.62783502483855358, -15.20150737401304575 ) ) ;
#59947 = CARTESIAN_POINT ( 'NONE',  ( -29.92777678363736626, -3.750539801530011985, 11.39883551934754635 ) ) ;
#59949 = ORIENTED_EDGE ( 'NONE', *, *, #42375, .T. ) ;
#59948 = FACE_OUTER_BOUND ( 'NONE', #40475, .T. ) ;
#59950 = EDGE_CURVE ( 'NONE', #65174, #44673, #9182, .T. ) ;
#59951 = CARTESIAN_POINT ( 'NONE',  ( 5.516018279890452902, -0.006629829924290480368, 0.001397286410094396563 ) ) ;
#59952 = ORIENTED_EDGE ( 'NONE', *, *, #13883, .F. ) ;
#59953 = AXIS2_PLACEMENT_3D ( 'NONE', #9777, #25402, #45682 ) ;
#59954 = CARTESIAN_POINT ( 'NONE',  ( 1.020182472822861230, -9.854645283130160749, 7.686484208904955651 ) ) ;
#59955 = ORIENTED_EDGE ( 'NONE', *, *, #12914, .F. ) ;
#59956 = CARTESIAN_POINT ( 'NONE',  ( 11.74548640120467979, 25.00000000000000000, -8.184666801472349817 ) ) ;
#59957 = CARTESIAN_POINT ( 'NONE',  ( 12.34777221413211912, -11.79052471001755009, -2.240005522967919216 ) ) ;
#59958 = CARTESIAN_POINT ( 'NONE',  ( 5.520433897694421610, -0.01006947824912458184, -0.01120198501134881015 ) ) ;
#59959 = CYLINDRICAL_SURFACE ( 'NONE', #2527, 12.18649999999999878 ) ;
#59960 = CYLINDRICAL_SURFACE ( 'NONE', #21883, 2.899999999999994582 ) ;
#59961 = CARTESIAN_POINT ( 'NONE',  ( -35.00000000000000000, 0.000000000000000000, 0.000000000000000000 ) ) ;
#59962 = CARTESIAN_POINT ( 'NONE',  ( 0.2706063244538032819, -4.023948952279190472, -11.56807224179757121 ) ) ;
#59964 = VERTEX_POINT ( 'NONE', #29460 ) ;
#59963 = LINE ( 'NONE', #49654, #33133 ) ;
#59965 = CLOSED_SHELL ( 'NONE', ( #9093, #56754, #3711, #7648, #44018, #59565, #18113, #37833, #56438, #17463, #31951, #56031, #35434, #22845, #10397, #53300, #28649, #10695, #29400, #62683, #51979, #56861, #27937, #26951, #20956, #14402, #42012, #24843, #53147, #44392, #50982, #6142, #59450, #13703, #27233, #50347, #62671, #44718, #28255, #65576, #52582, #42575, #9871, #31968, #44629, #26507, #45244, #51494, #61258, #3786, #45176, #4303, #21165, #15671, #9439, #35132, #41336, #49403, #7070, #42303, #45115, #10565, #36319, #2743, #48618, #37472, #32920, #19352, #19987, #47946, #44162, #3997, #20604, #26413, #47661, #39609, #46445, #34673, #63326, #17521, #38344, #18692, #14023, #61433, #54872, #14057, #745, #2957, #9067, #36656, #38898, #9965, #31410, #7617, #24780, #52927, #65285, #55414, #35993, #61444, #4457, #1784, #19081, #46545, #20133, #12580, #5602, #41306, #58183, #18046, #45075, #56374, #46649, #8386, #51681, #39825, #21705, #46471, #37369, #8411, #62151, #64414, #2696, #45649, #33483, #16100, #15309, #53012, #25215, #10614, #23841, #16373, #62661, #4234, #48437, #22526, #32865, #13238, #23511, #59417, #61128, #64031, #11856, #59017, #52944, #5175, #43583, #31096, #7999, #19132, #59445, #59084, #15376, #61049, #31079, #33966, #45364, #59113, #41474, #19760, #21079, #20469, #18325, #30427, #38598, #47607, #35834, #45816, #16476, #10301, #17562, #15327, #26224, #28441, #12350, #8777, #1444, #11367, #47521, #55793, #57623, #55289, #16969, #13917, #52217, #34437, #19683, #34511, #31594, #6231, #56643, #64242, #46942, #59462, #23651, #969, #1598, #10783, #50902, #25280, #51241, #13916, #44365, #61277, #12729, #21654, #58326, #7590, #4221, #3757, #60645, #51075, #22077, #60096, #36083, #34599, #21780, #11415, #60761, #11949, #44794, #42046, #45794, #4449, #26885, #2496, #15873, #11663, #33329, #24633, #4148, #44857, #61233, #6393, #9936, #34934, #2425, #55720, #31145, #59513, #29950, #35041, #59849, #64300, #24602, #40322, #57058, #60833, #57249, #2187, #51584, #33946, #41888, #61574, #46979, #63781, #33316, #903, #65064, #50070, #16282, #57367, #19238, #5017, #58420, #41005, #25432, #62379, #61352, #17425, #26264, #35887, #23710, #59087, #29290, #22599, #52111, #46910, #53626, #17161, #48816, #25461, #2047, #53356, #43514, #47154, #47326, #33978, #59019, #33942, #24382, #12510, #44941, #3039, #58844, #33424, #45652, #319, #4685, #47288, #47849, #9754, #36484, #36704, #35600, #63495, #20788, #39617, #5059 ) ) ;
#59966 = EDGE_LOOP ( 'NONE', ( #22520, #59020 ) ) ;
#59967 = DIRECTION ( 'NONE',  ( -1.000000000000000000, 0.000000000000000000, 0.000000000000000000 ) ) ;
#59968 = ORIENTED_EDGE ( 'NONE', *, *, #34360, .T. ) ;
#59969 = EDGE_LOOP ( 'NONE', ( #27496, #47533, #43198, #58370 ) ) ;
#59970 = FACE_OUTER_BOUND ( 'NONE', #40268, .T. ) ;
#59971 = DIRECTION ( 'NONE',  ( -1.000000000000000000, -0.000000000000000000, 0.000000000000000000 ) ) ;
#59972 = CARTESIAN_POINT ( 'NONE',  ( -27.08702828306176258, -2.216258174335476561, 0.6138566972905330488 ) ) ;
#59973 = CARTESIAN_POINT ( 'NONE',  ( 36.00000000000000711, 8.017674001891782254, -9.913596905230145140 ) ) ;
#59974 = DIRECTION ( 'NONE',  ( 1.000000000000000000, -0.000000000000000000, 0.000000000000000000 ) ) ;
#59975 = VECTOR ( 'NONE', #44366, 1000.000000000000000 ) ;
#59976 = CARTESIAN_POINT ( 'NONE',  ( 0.2956976708475454463, 10.72256944221094699, -5.936640677855251624 ) ) ;
#59977 = EDGE_CURVE ( 'NONE', #32302, #54991, #31597, .T. ) ;
#59978 = CARTESIAN_POINT ( 'NONE',  ( 35.00000000000000000, 3.805206332242470513, -12.16893194857551386 ) ) ;
#59979 = EDGE_CURVE ( 'NONE', #2869, #35192, #4668, .T. ) ;
#59980 = ORIENTED_EDGE ( 'NONE', *, *, #44345, .F. ) ;
#59981 = CARTESIAN_POINT ( 'NONE',  ( -14.11589373245165469, 8.250315036047107142, 10.68561190601526611 ) ) ;
#59982 = CARTESIAN_POINT ( 'NONE',  ( -10.00000000000000178, 0.000000000000000000, 0.000000000000000000 ) ) ;
#59983 = CARTESIAN_POINT ( 'NONE',  ( 0.000000000000000000, -35.00000000000000000, 0.000000000000000000 ) ) ;
#59984 = ORIENTED_EDGE ( 'NONE', *, *, #44574, .T. ) ;
#59985 = EDGE_CURVE ( 'NONE', #57610, #52011, #25823, .T. ) ;
#59986 = CIRCLE ( 'NONE', #7919, 12.74999999999999822 ) ;
#59987 = CARTESIAN_POINT ( 'NONE',  ( 42.06985574703970343, -1.486553742990792681, -18.28338660486113909 ) ) ;
#59988 = CARTESIAN_POINT ( 'NONE',  ( -8.073144562555491177, -2.358972950292971049, 13.29271665687120674 ) ) ;
#59990 = ORIENTED_EDGE ( 'NONE', *, *, #31651, .T. ) ;
#59989 = EDGE_CURVE ( 'NONE', #31716, #16864, #28418, .T. ) ;
#59991 = CARTESIAN_POINT ( 'NONE',  ( 2.245754705088395919, 6.667819336165991650, -3.721112460996948368 ) ) ;
#59992 = DIRECTION ( 'NONE',  ( -1.000000000000000000, 0.000000000000000000, 0.000000000000000000 ) ) ;
#59993 = CARTESIAN_POINT ( 'NONE',  ( 2.889800649504073782, 4.732281052280313816, 3.882893708502064278 ) ) ;
#59994 = EDGE_CURVE ( 'NONE', #11634, #30317, #12790, .T. ) ;
#59995 = CARTESIAN_POINT ( 'NONE',  ( 36.00000000000000711, -12.60630747491661374, 1.908798535168511057 ) ) ;
#59996 = CARTESIAN_POINT ( 'NONE',  ( 35.00000000000000000, 4.705694406421931860E-17, -3.469127814946512892E-15 ) ) ;
#59997 = ORIENTED_EDGE ( 'NONE', *, *, #11476, .F. ) ;
#59998 = CARTESIAN_POINT ( 'NONE',  ( 2.276905613633651182, 0.1540880535620979541, 7.644700064315450128 ) ) ;
#59999 = CARTESIAN_POINT ( 'NONE',  ( -22.27706485742869091, 3.547445275915927176, 0.9832726768967369191 ) ) ;
#60000 = CARTESIAN_POINT ( 'NONE',  ( -37.00000000000000711, -4.400442035671033203, 11.96656215839367654 ) ) ;
#60001 = ORIENTED_EDGE ( 'NONE', *, *, #64995, .T. ) ;
#60002 = CARTESIAN_POINT ( 'NONE',  ( 35.00000000000000000, 6.891188680298960811, 9.512294188640820991 ) ) ;
#60003 = DIRECTION ( 'NONE',  ( -0.8405098440481674205, 0.000000000000000000, -0.5417962735734949131 ) ) ;
#60004 = VERTEX_POINT ( 'NONE', #10826 ) ;
#60005 = ORIENTED_EDGE ( 'NONE', *, *, #7443, .T. ) ;
#60006 = VERTEX_POINT ( 'NONE', #20808 ) ;
#60007 = CARTESIAN_POINT ( 'NONE',  ( 37.00000000000000711, -6.753013023069642351, 10.14433819232440825 ) ) ;
#60008 = ADVANCED_FACE ( 'NONE', ( #15152 ), #32586, .F. ) ;
#60009 = ORIENTED_EDGE ( 'NONE', *, *, #5249, .T. ) ;
#60010 = ADVANCED_FACE ( 'NONE', ( #16147 ), #50431, .T. ) ;
#60011 = DIRECTION ( 'NONE',  ( 1.000000000000000000, -0.000000000000000000, -0.000000000000000000 ) ) ;
#60012 = CYLINDRICAL_SURFACE ( 'NONE', #4939, 12.18650000000000055 ) ;
#60013 = CARTESIAN_POINT ( 'NONE',  ( 0.3218525148189785301, -6.342972338926866627, 10.49750909897050555 ) ) ;
#60014 = DIRECTION ( 'NONE',  ( -1.000000000000000000, 0.000000000000000000, 0.000000000000000000 ) ) ;
#60015 =( BOUNDED_SURFACE ( )  B_SPLINE_SURFACE ( 3, 1, ( 
 ( #56213, #49609 ),
 ( #49928, #55897 ),
 ( #39940, #55235 ),
 ( #19989, #10331 ) ),
 .UNSPECIFIED., .F., .F., .F. ) 
 B_SPLINE_SURFACE_WITH_KNOTS ( ( 4, 4 ),
 ( 2, 2 ),
 ( 0.000000000000000000, 1.000000000000000000 ),
 ( 0.000000000000000000, 1.000000000000000000 ),
 .UNSPECIFIED. ) 
 GEOMETRIC_REPRESENTATION_ITEM ( )  RATIONAL_B_SPLINE_SURFACE ( (
 ( 1.000000000000000000, 1.000000000000000000),
 ( 0.6933888150995267674, 0.9895912004443193632),
 ( 0.6933888150995267674, 0.9895912004443193632),
 ( 1.000000000000000000, 1.000000000000000000) ) ) 
 REPRESENTATION_ITEM ( '' )  SURFACE ( )  );
#60016 = CARTESIAN_POINT ( 'NONE',  ( -11.38801898431830040, -29.26006678106075753, 7.242958320504926384 ) ) ;
#60017 = CARTESIAN_POINT ( 'NONE',  ( -35.00000000000000000, -5.246972444134095248, 10.99909370905155370 ) ) ;
#60019 = ORIENTED_EDGE ( 'NONE', *, *, #45281, .F. ) ;
#60018 = CARTESIAN_POINT ( 'NONE',  ( 2.241352910868908310, -7.633946224498474820, 0.08337961031701579540 ) ) ;
#60020 = ADVANCED_FACE ( 'NONE', ( #10169 ), #41076, .T. ) ;
#60021 = DIRECTION ( 'NONE',  ( -0.000000000000000000, -0.000000000000000000, -1.000000000000000000 ) ) ;
#60022 = EDGE_LOOP ( 'NONE', ( #44357, #55249, #28038, #42024 ) ) ;
#60023 = CARTESIAN_POINT ( 'NONE',  ( 2.000000000000001776, -6.250523986463956128, -3.007653927006670003 ) ) ;
#60024 = VERTEX_POINT ( 'NONE', #852 ) ;
#60025 = VERTEX_POINT ( 'NONE', #40766 ) ;
#60026 = CARTESIAN_POINT ( 'NONE',  ( -27.20102706715913143, 1.966718264078106682, 1.765193291701696143 ) ) ;
#60027 = CARTESIAN_POINT ( 'NONE',  ( 16.93571557946443562, -34.49999999976442666, 4.804977935187394245 ) ) ;
#60028 = DIRECTION ( 'NONE',  ( -1.000000000000000000, 0.000000000000000000, 0.000000000000000000 ) ) ;
#60029 = VECTOR ( 'NONE', #604, 1000.000000000000114 ) ;
#60030 = DIRECTION ( 'NONE',  ( -1.000000000000000000, 0.000000000000000000, -0.000000000000000000 ) ) ;
#60031 = EDGE_CURVE ( 'NONE', #40020, #23561, #1486, .T. ) ;
#60032 = CARTESIAN_POINT ( 'NONE',  ( 37.00000000000000711, -4.309077947445731027, -10.92721691015454510 ) ) ;
#60033 = CARTESIAN_POINT ( 'NONE',  ( 2.257661810674660874, 5.938215228160625969, 4.806737555286991537 ) ) ;
#60034 = ORIENTED_EDGE ( 'NONE', *, *, #21921, .T. ) ;
#60035 = VERTEX_POINT ( 'NONE', #15794 ) ;
#60036 = CARTESIAN_POINT ( 'NONE',  ( 0.3665391374699467075, 1.872534962004800851, 12.13918562134719359 ) ) ;
#60037 = VERTEX_POINT ( 'NONE', #60720 ) ;
#60038 = MECHANICAL_DESIGN_GEOMETRIC_PRESENTATION_REPRESENTATION (  '', ( #63205 ), #17559 ) ;
#60039 = VERTEX_POINT ( 'NONE', #30762 ) ;
#60040 = DIRECTION ( 'NONE',  ( 0.000000000000000000, 1.000000000000000000, 0.000000000000000000 ) ) ;
#60041 = CARTESIAN_POINT ( 'NONE',  ( 0.2648978790185584908, 0.1321385342564118659, -12.24533305150758089 ) ) ;
#60042 = CARTESIAN_POINT ( 'NONE',  ( 2.000000000000001776, 1.956810415765184219, 6.654767106875543625 ) ) ;
#60043 = CARTESIAN_POINT ( 'NONE',  ( 2.284126774967663476, 7.647017279602157380, 0.1584898568958162390 ) ) ;
#60044 = LINE ( 'NONE', #34738, #1273 ) ;
#60045 = DIRECTION ( 'NONE',  ( 0.000000000000000000, 0.01356324068817998073, -0.9999080150203990547 ) ) ;
#60046 = EDGE_CURVE ( 'NONE', #19066, #49868, #46844, .T. ) ;
#60047 = ORIENTED_EDGE ( 'NONE', *, *, #17508, .F. ) ;
#60048 = AXIS2_PLACEMENT_3D ( 'NONE', #46253, #40588, #10641 ) ;
#60049 = EDGE_LOOP ( 'NONE', ( #14935, #31874, #46430, #9005 ) ) ;
#60050 = FACE_OUTER_BOUND ( 'NONE', #50223, .T. ) ;
#60051 = CARTESIAN_POINT ( 'NONE',  ( 3.031336079629687319, 4.750429016921711600, -6.309383307296628551 ) ) ;
#60052 = CARTESIAN_POINT ( 'NONE',  ( -35.00000000000000000, 0.000000000000000000, 0.000000000000000000 ) ) ;
#60053 = CIRCLE ( 'NONE', #28206, 5.000000000000001776 ) ;
#60054 = DIRECTION ( 'NONE',  ( 1.000000000000000000, -0.000000000000000000, -0.000000000000000000 ) ) ;
#60055 = FACE_OUTER_BOUND ( 'NONE', #43615, .T. ) ;
#60056 = CARTESIAN_POINT ( 'NONE',  ( -10.90165637462999726, -7.183754052287492975, -9.621202272021861290 ) ) ;
#60057 = CARTESIAN_POINT ( 'NONE',  ( 3.152665057734040488, 0.000000000000000000, 0.000000000000000000 ) ) ;
#60058 = CARTESIAN_POINT ( 'NONE',  ( 2.781367136451863509, 6.179587792204241481, 4.783057651000522270 ) ) ;
#60059 = CARTESIAN_POINT ( 'NONE',  ( 2.491965175174582381, -5.121563073453708093, -5.773748672882058841 ) ) ;
#60060 = EDGE_CURVE ( 'NONE', #20098, #46347, #44683, .T. ) ;
#60061 = ORIENTED_EDGE ( 'NONE', *, *, #22692, .F. ) ;
#60062 = PLANE ( 'NONE',  #54780 ) ;
#60063 = CARTESIAN_POINT ( 'NONE',  ( 0.2646305136544065406, 10.53923716745255490, -6.237419468586969273 ) ) ;
#60064 = DIRECTION ( 'NONE',  ( 0.000000000000000000, -0.01356324068817999114, 0.9999080150203989437 ) ) ;
#60065 = EDGE_CURVE ( 'NONE', #14286, #55534, #51425, .T. ) ;
#60066 = CIRCLE ( 'NONE', #39886, 12.18649999999999878 ) ;
#60067 = CARTESIAN_POINT ( 'NONE',  ( -5.596759081085386889, -31.66776075797297096, -13.71641508080218230 ) ) ;
#60068 = CARTESIAN_POINT ( 'NONE',  ( -17.87891481078358069, -12.92455976930239814, 3.899497271525862896 ) ) ;
#60069 = ORIENTED_EDGE ( 'NONE', *, *, #40231, .T. ) ;
#60070 = DIRECTION ( 'NONE',  ( -1.000000000000000000, 0.000000000000000000, -0.000000000000000000 ) ) ;
#60071 = CARTESIAN_POINT ( 'NONE',  ( 27.73674564613515514, 12.76067307604452417, 4.417293456390572359 ) ) ;
#60072 = CARTESIAN_POINT ( 'NONE',  ( 0.8805962972398277966, -27.81433265277922828, -12.58259205804047021 ) ) ;
#60073 = ORIENTED_EDGE ( 'NONE', *, *, #16671, .F. ) ;
#60074 = DIRECTION ( 'NONE',  ( -1.000000000000000000, 0.000000000000000000, 0.000000000000000000 ) ) ;
#60075 = CARTESIAN_POINT ( 'NONE',  ( -28.08468344552528606, -11.68084827141784565, -6.774767069026986555 ) ) ;
#60076 = CARTESIAN_POINT ( 'NONE',  ( -22.29770266787582500, -1.047554374660435439, -3.593535545924356089 ) ) ;
#60077 = DIRECTION ( 'NONE',  ( 0.000000000000000000, -0.01356324068817998940, 0.9999080150203990547 ) ) ;
#60078 = CARTESIAN_POINT ( 'NONE',  ( 0.3610902822527181644, -11.44530431865296016, 4.444884365376562840 ) ) ;
#60079 = ADVANCED_FACE ( 'NONE', ( #46096 ), #543, .T. ) ;
#60080 = CYLINDRICAL_SURFACE ( 'NONE', #38261, 5.000000000000000888 ) ;
#60081 = VERTEX_POINT ( 'NONE', #5874 ) ;
#60082 = CARTESIAN_POINT ( 'NONE',  ( 3.780834652287974773, 8.352030633203074927, -8.616471685210672860 ) ) ;
#60084 = AXIS2_PLACEMENT_3D ( 'NONE', #57705, #22432, #16480 ) ;
#60083 = DIRECTION ( 'NONE',  ( 1.000000000000000000, -0.000000000000000000, 0.000000000000000000 ) ) ;
#60085 = DIRECTION ( 'NONE',  ( 1.000000000000000000, -0.000000000000000000, 0.000000000000000000 ) ) ;
#60086 = CARTESIAN_POINT ( 'NONE',  ( 2.249013661412230913, 7.540851674528681770, -1.207748565003158081 ) ) ;
#60087 = DIRECTION ( 'NONE',  ( 1.000000000000000000, -0.000000000000000000, 0.000000000000000000 ) ) ;
#60088 = FACE_OUTER_BOUND ( 'NONE', #40878, .T. ) ;
#60089 = CYLINDRICAL_SURFACE ( 'NONE', #42460, 12.18650000000000055 ) ;
#60090 = ORIENTED_EDGE ( 'NONE', *, *, #35610, .T. ) ;
#60091 = ORIENTED_EDGE ( 'NONE', *, *, #41651, .F. ) ;
#60092 = CARTESIAN_POINT ( 'NONE',  ( -18.01363938508876927, -9.088990878694016118, -7.856193784715579831 ) ) ;
#60093 = VERTEX_POINT ( 'NONE', #26130 ) ;
#60094 =( LENGTH_UNIT ( ) NAMED_UNIT ( * ) SI_UNIT ( .MILLI., .METRE. ) );
#60095 = CIRCLE ( 'NONE', #18725, 5.000000000000000000 ) ;
#60096 = ADVANCED_FACE ( 'NONE', ( #46407 ), #42704, .T. ) ;
#60097 = DIRECTION ( 'NONE',  ( -1.000000000000000000, 0.000000000000000000, 0.000000000000000000 ) ) ;
#60098 = CARTESIAN_POINT ( 'NONE',  ( -19.69476066079020171, -4.201994156881551312, 11.24025111398909615 ) ) ;
#60099 = ORIENTED_EDGE ( 'NONE', *, *, #1635, .T. ) ;
#60100 = CARTESIAN_POINT ( 'NONE',  ( -35.00000000000000000, 0.000000000000000000, 0.000000000000000000 ) ) ;
#60101 = DIRECTION ( 'NONE',  ( 0.000000000000000000, 0.000000000000000000, 1.000000000000000000 ) ) ;
#60102 = CARTESIAN_POINT ( 'NONE',  ( 23.98498522125079191, 2.278584884918189779, 13.31001393690969969 ) ) ;
#60103 = EDGE_LOOP ( 'NONE', ( #29852, #38693, #37359, #42092 ) ) ;
#60104 = VERTEX_POINT ( 'NONE', #43043 ) ;
#60105 = CARTESIAN_POINT ( 'NONE',  ( 2.639814597422740050, 0.2564041122426181651, -7.763021810282384472 ) ) ;
#60106 = ORIENTED_EDGE ( 'NONE', *, *, #48253, .T. ) ;
#60107 = DIRECTION ( 'NONE',  ( -1.000000000000000000, 0.000000000000000000, 0.000000000000000000 ) ) ;
#60108 = VERTEX_POINT ( 'NONE', #17788 ) ;
#60109 = DIRECTION ( 'NONE',  ( 0.000000000000000000, -0.9651210252299822212, -0.2618041379715531636 ) ) ;
#60110 = CARTESIAN_POINT ( 'NONE',  ( -29.25216940168754931, 1.557237388845396753, 11.90587590551118424 ) ) ;
#60111 = FACE_OUTER_BOUND ( 'NONE', #4286, .T. ) ;
#60112 = CARTESIAN_POINT ( 'NONE',  ( 0.2652384770603669617, -10.63836422907228396, 6.065775245581129127 ) ) ;
#60113 = DIRECTION ( 'NONE',  ( 0.9582930651793755139, 0.01979360193296375928, 0.2851010602429189245 ) ) ;
#60114 = EDGE_CURVE ( 'NONE', #65638, #983, #63318, .T. ) ;
#60115 = EDGE_LOOP ( 'NONE', ( #37567, #31292, #33632, #24274 ) ) ;
#60116 = CARTESIAN_POINT ( 'NONE',  ( 2.000000000000001776, -1.754183803416492493, -6.711026108862277795 ) ) ;
#60117 = CARTESIAN_POINT ( 'NONE',  ( 2.034671305879536263, 2.716450156984552944, -11.35598636043548204 ) ) ;
#60118 = ADVANCED_FACE ( 'NONE', ( #16791 ), #46596, .F. ) ;
#60119 = DIRECTION ( 'NONE',  ( 1.000000000000000000, 0.000000000000000000, 0.000000000000000000 ) ) ;
#60120 = DIRECTION ( 'NONE',  ( 0.000000000000000000, 0.01356324068817991828, -0.9999080150203990547 ) ) ;
#60121 = CARTESIAN_POINT ( 'NONE',  ( 2.241509619876139503, -7.525055189891911134, 1.287997509666546803 ) ) ;
#60122 = CARTESIAN_POINT ( 'NONE',  ( 24.08205593069842365, 1.039322572775280618, 13.46392217257402635 ) ) ;
#60123 = FACE_OUTER_BOUND ( 'NONE', #46304, .T. ) ;
#60124 = CARTESIAN_POINT ( 'NONE',  ( 35.00000000000000000, -7.561043153948031836, -9.557269938331533154 ) ) ;
#60125 = LINE ( 'NONE', #14866, #5569 ) ;
#60126 = ORIENTED_EDGE ( 'NONE', *, *, #11029, .F. ) ;
#60127 = EDGE_CURVE ( 'NONE', #46634, #10568, #92, .T. ) ;
#60128 = CARTESIAN_POINT ( 'NONE',  ( -15.23244606078242214, 8.473308435344804934, -8.497338976891521511 ) ) ;
#60129 = VECTOR ( 'NONE', #48318, 1000.000000000000000 ) ;
#60130 = ORIENTED_EDGE ( 'NONE', *, *, #59275, .F. ) ;
#60131 = DIRECTION ( 'NONE',  ( -1.000000000000000000, -1.836970198721029688E-16, -0.000000000000000000 ) ) ;
#60132 = DIRECTION ( 'NONE',  ( 1.000000000000000000, 0.000000000000000000, -0.000000000000000000 ) ) ;
#60133 = DIRECTION ( 'NONE',  ( 1.000000000000000000, 0.000000000000000000, -0.000000000000000000 ) ) ;
#60134 = CYLINDRICAL_SURFACE ( 'NONE', #45820, 2.899999999999994582 ) ;
#60135 = CARTESIAN_POINT ( 'NONE',  ( 5.514970785353741078, -0.001117786416802142449, 0.004588761610584822515 ) ) ;
#60136 = EDGE_CURVE ( 'NONE', #44008, #32797, #65574, .T. ) ;
#60137 = EDGE_LOOP ( 'NONE', ( #17564, #48086, #42799, #45863 ) ) ;
#60138 = CARTESIAN_POINT ( 'NONE',  ( 35.00000000000000000, -9.896810808925339487, 7.110831038798382409 ) ) ;
#60139 = CARTESIAN_POINT ( 'NONE',  ( 2.244591118396556784, -3.724266936773029890, 6.665613643996593396 ) ) ;
#60140 = CARTESIAN_POINT ( 'NONE',  ( 12.27748271067557617, 0.5231152287652744981, 11.98862020473568002 ) ) ;
#60141 = CARTESIAN_POINT ( 'NONE',  ( 0.4613984246114880006, 2.415907815801404457, 12.07219521825821040 ) ) ;
#60142 = DIRECTION ( 'NONE',  ( 0.000000000000000000, 0.000000000000000000, -1.000000000000000000 ) ) ;
#60143 = ORIENTED_EDGE ( 'NONE', *, *, #47328, .F. ) ;
#60144 = CARTESIAN_POINT ( 'NONE',  ( -35.00000000000000000, 0.000000000000000000, 0.000000000000000000 ) ) ;
#60145 = ORIENTED_EDGE ( 'NONE', *, *, #60890, .T. ) ;
#60146 = CARTESIAN_POINT ( 'NONE',  ( -4.975205859172449507, -1.416020129149132778, 13.42553116244733680 ) ) ;
#60147 = DIRECTION ( 'NONE',  ( -1.000000000000000000, 0.000000000000000000, 0.000000000000000000 ) ) ;
#60148 = CARTESIAN_POINT ( 'NONE',  ( 3.152665057734128862, 5.461013642405629476, -5.761241965769021256 ) ) ;
#60149 = DIRECTION ( 'NONE',  ( -1.000000000000000000, -0.000000000000000000, 0.000000000000000000 ) ) ;
#60150 = ORIENTED_EDGE ( 'NONE', *, *, #34251, .T. ) ;
#60151 = VERTEX_POINT ( 'NONE', #52055 ) ;
#60152 = DIRECTION ( 'NONE',  ( -1.000000000000000000, 0.000000000000000000, 0.000000000000000000 ) ) ;
#60153 = ORIENTED_EDGE ( 'NONE', *, *, #62031, .T. ) ;
#60154 = DIRECTION ( 'NONE',  ( 0.000000000000000000, 0.01356324068817998940, -0.9999080150203990547 ) ) ;
#60155 = DIRECTION ( 'NONE',  ( 0.000000000000000000, 0.9467777615094560284, 0.3218879778916007850 ) ) ;
#60156 = FACE_OUTER_BOUND ( 'NONE', #20292, .T. ) ;
#60157 = CARTESIAN_POINT ( 'NONE',  ( 1.719304012338398246, 7.581471372739840398, 10.22720798541364395 ) ) ;
#60158 = CARTESIAN_POINT ( 'NONE',  ( 1.283627346226907218, 9.278077665801971463, -8.503905436512024352 ) ) ;
#60159 = DIRECTION ( 'NONE',  ( -1.000000000000000000, -0.000000000000000000, -0.000000000000000000 ) ) ;
#60160 = CARTESIAN_POINT ( 'NONE',  ( 2.000000000000001776, -7.484036900328550956, 0.4890722589968952150 ) ) ;
#60161 = ORIENTED_EDGE ( 'NONE', *, *, #55953, .T. ) ;
#60163 = ORIENTED_EDGE ( 'NONE', *, *, #209, .T. ) ;
#60162 = CARTESIAN_POINT ( 'NONE',  ( -37.00000000000000711, 0.000000000000000000, 0.000000000000000000 ) ) ;
#60164 = ORIENTED_EDGE ( 'NONE', *, *, #7281, .T. ) ;
#60165 = VECTOR ( 'NONE', #22991, 1000.000000000000000 ) ;
#60166 = LINE ( 'NONE', #39885, #22415 ) ;
#60167 = EDGE_CURVE ( 'NONE', #1326, #31517, #9662, .T. ) ;
#60168 = CARTESIAN_POINT ( 'NONE',  ( 1.948354844648341411, 11.94326855455022240, -0.7204626209688785865 ) ) ;
#60169 = ORIENTED_EDGE ( 'NONE', *, *, #30102, .T. ) ;
#60170 = AXIS2_PLACEMENT_3D ( 'NONE', #42306, #52337, #16734 ) ;
#60171 = CARTESIAN_POINT ( 'NONE',  ( 35.00000000000000000, 4.545979934229410269, -11.30684963584391234 ) ) ;
#60172 = ORIENTED_EDGE ( 'NONE', *, *, #14239, .T. ) ;
#60173 = DIRECTION ( 'NONE',  ( -1.000000000000000000, -0.000000000000000000, 0.000000000000000000 ) ) ;
#60174 = CARTESIAN_POINT ( 'NONE',  ( -35.00000000000000000, 1.738225594539995589, 12.63095688309029541 ) ) ;
#60175 = DIRECTION ( 'NONE',  ( 1.000000000000000000, 0.000000000000000000, 0.000000000000000000 ) ) ;
#60176 = CARTESIAN_POINT ( 'NONE',  ( -27.10113028276028757, -2.276991616286371478, -0.5479825692854007890 ) ) ;
#60177 = ORIENTED_EDGE ( 'NONE', *, *, #59260, .T. ) ;
#60178 = VERTEX_POINT ( 'NONE', #32406 ) ;
#60179 = DIRECTION ( 'NONE',  ( 1.000000000000000000, -0.000000000000000000, 0.000000000000000000 ) ) ;
#60180 = ORIENTED_EDGE ( 'NONE', *, *, #40771, .F. ) ;
#60181 = DIRECTION ( 'NONE',  ( 1.000000000000000000, 0.000000000000000000, -0.000000000000000000 ) ) ;
#60182 = ORIENTED_EDGE ( 'NONE', *, *, #29680, .T. ) ;
#60183 = ORIENTED_EDGE ( 'NONE', *, *, #28156, .F. ) ;
#60184 = VERTEX_POINT ( 'NONE', #22109 ) ;
#60185 = DIRECTION ( 'NONE',  ( -1.000000000000000000, 0.000000000000000000, -0.000000000000000000 ) ) ;
#60186 = CARTESIAN_POINT ( 'NONE',  ( -36.00000000000000711, -8.624332853796127907, 9.390600770287960586 ) ) ;
#60187 = ADVANCED_FACE ( 'NONE', ( #37737 ), #53027, .T. ) ;
#60188 = CARTESIAN_POINT ( 'NONE',  ( -37.00000000000000711, -11.78977382767499194, 4.245927698352017110 ) ) ;
#60189 = CARTESIAN_POINT ( 'NONE',  ( -35.00000000000000000, -9.821084925794513865, -7.215058775251364409 ) ) ;
#60190 = ORIENTED_EDGE ( 'NONE', *, *, #29485, .T. ) ;
#60191 = DIRECTION ( 'NONE',  ( 0.000000000000000000, 0.3554799084908899509, 0.9346839223284567622 ) ) ;
#60192 =( BOUNDED_CURVE ( )  B_SPLINE_CURVE ( 3, ( #23263, #12612, #28258, #32890 ),
 .UNSPECIFIED., .F., .F. ) 
 B_SPLINE_CURVE_WITH_KNOTS ( ( 4, 4 ),
 ( 1.638716093112601024, 1.675879999089879613 ),
 .UNSPECIFIED. ) 
 CURVE ( )  GEOMETRIC_REPRESENTATION_ITEM ( )  RATIONAL_B_SPLINE_CURVE ( ( 1.000000000000000000, 0.9998849069861288630, 0.9998849069861288630, 1.000000000000000000 ) ) 
 REPRESENTATION_ITEM ( '' )  );
#60193 = ORIENTED_EDGE ( 'NONE', *, *, #34790, .T. ) ;
#60194 = CARTESIAN_POINT ( 'NONE',  ( 0.2851083653049504285, -0.4107471485392698018, 25.00000000000000000 ) ) ;
#60195 = EDGE_CURVE ( 'NONE', #49313, #7701, #57434, .T. ) ;
#60196 = CARTESIAN_POINT ( 'NONE',  ( -19.42992534460779908, -4.328069792619975154, -12.78809649950834171 ) ) ;
#60197 = ADVANCED_FACE ( 'NONE', ( #27419 ), #47717, .T. ) ;
#60198 = ORIENTED_EDGE ( 'NONE', *, *, #52590, .T. ) ;
#60199 = CARTESIAN_POINT ( 'NONE',  ( 5.516018279890452902, 0.003191189039764837348, 0.005976902763919047894 ) ) ;
#60200 = CARTESIAN_POINT ( 'NONE',  ( 0.2759803524722208024, 4.011137970318948476, 11.57441428600633770 ) ) ;
#60201 = CARTESIAN_POINT ( 'NONE',  ( 2.256373768223409737, -6.681391662621552818, -3.703993494727584324 ) ) ;
#60202 = ORIENTED_EDGE ( 'NONE', *, *, #33303, .F. ) ;
#60203 = ORIENTED_EDGE ( 'NONE', *, *, #47263, .F. ) ;
#60204 = EDGE_CURVE ( 'NONE', #13349, #39026, #24528, .T. ) ;
#60205 = CARTESIAN_POINT ( 'NONE',  ( 2.241317068080781905, -7.633845645378816158, 0.09149433816013313736 ) ) ;
#60206 = AXIS2_PLACEMENT_3D ( 'NONE', #13097, #53676, #32380 ) ;
#60207 = ORIENTED_EDGE ( 'NONE', *, *, #33644, .T. ) ;
#60208 = EDGE_CURVE ( 'NONE', #15944, #63155, #14094, .T. ) ;
#60209 = CARTESIAN_POINT ( 'NONE',  ( 0.2739690278137231760, 10.69833303470765884, 5.965352196073636648 ) ) ;
#60210 = CARTESIAN_POINT ( 'NONE',  ( 1.547277799337567483, 10.12789507952265566, 7.618736734813758460 ) ) ;
#60211 = CARTESIAN_POINT ( 'NONE',  ( -47.00000000000000711, 0.000000000000000000, 0.000000000000000000 ) ) ;
#60212 = CARTESIAN_POINT ( 'NONE',  ( -47.00000000000000711, 0.000000000000000000, 0.000000000000000000 ) ) ;
#60213 = CARTESIAN_POINT ( 'NONE',  ( -37.00000000000000711, 0.000000000000000000, 0.000000000000000000 ) ) ;
#60214 = ORIENTED_EDGE ( 'NONE', *, *, #36659, .F. ) ;
#60215 = DIRECTION ( 'NONE',  ( 0.000000000000000000, 0.01356324068817992175, -0.9999080150203990547 ) ) ;
#60216 = DIRECTION ( 'NONE',  ( 0.000000000000000000, -0.01356324068817992175, 0.9999080150203990547 ) ) ;
#60217 = CARTESIAN_POINT ( 'NONE',  ( 35.00000000000000000, 4.705694406421931860E-17, -3.469127814946512892E-15 ) ) ;
#60218 = AXIS2_PLACEMENT_3D ( 'NONE', #41871, #47527, #1658 ) ;
#60219 = CARTESIAN_POINT ( 'NONE',  ( 2.655192694323885050, -8.589732161579133773, -4.290256727312194762 ) ) ;
#60220 = AXIS2_PLACEMENT_3D ( 'NONE', #31147, #26164, #39559 ) ;
#60221 = EDGE_CURVE ( 'NONE', #59432, #8976, #43706, .T. ) ;
#60222 = CARTESIAN_POINT ( 'NONE',  ( -16.12286248669608213, -29.23548504417002647, -10.48934106169928704 ) ) ;
#60223 = ADVANCED_FACE ( 'NONE', ( #44347 ), #63987, .T. ) ;
#60224 = DIRECTION ( 'NONE',  ( 0.000000000000000000, 0.4380125133593912312, -0.8989688749565187820 ) ) ;
#60225 = CARTESIAN_POINT ( 'NONE',  ( 2.273267844204862165, -5.952585402747270216, -4.797225296800606387 ) ) ;
#60226 = DIRECTION ( 'NONE',  ( 0.000000000000000000, 0.01356324068818000328, -0.9999080150203990547 ) ) ;
#60227 = CARTESIAN_POINT ( 'NONE',  ( -19.69476066079020171, -4.201994156881551312, -12.82938989607585789 ) ) ;
#60228 = B_SPLINE_CURVE_WITH_KNOTS ( 'NONE', 3,
 ( #50829, #16231, #56467, #31514, #36513, #31202, #5275, #11559, #41825, #61435, #5954, #20572, #51816, #6266, #30847, #26210, #297, #46814, #40852 ),
 .UNSPECIFIED., .F., .F.,
 ( 4, 3, 3, 3, 3, 3, 4 ),
 ( 7.230905111020012517E-18, 2.825908398831274927E-05, 4.208813692483992291E-05, 5.591713746943835966E-05, 6.279584083231888939E-05, 9.105792820296731993E-05, 0.0001153131102488850796 ),
 .UNSPECIFIED. ) ;
#60229 = EDGE_LOOP ( 'NONE', ( #43477, #12860, #53848, #37334 ) ) ;
#60230 = CARTESIAN_POINT ( 'NONE',  ( -30.18541646480307250, -2.218019889705987957, 11.82085758638470629 ) ) ;
#60231 = ORIENTED_EDGE ( 'NONE', *, *, #28748, .F. ) ;
#60232 = LINE ( 'NONE', #45272, #63947 ) ;
#60233 = B_SPLINE_CURVE_WITH_KNOTS ( 'NONE', 3,
 ( #64527, #34600, #54894, #25282, #18997, #34907, #23995, #9319, #38950, #45560, #24639, #5019, #65196, #12, #39922, #59241, #19331, #60205, #55559 ),
 .UNSPECIFIED., .F., .F.,
 ( 4, 3, 3, 3, 3, 3, 4 ),
 ( 6.759600587344757484E-18, 2.825908398830985241E-05, 4.208813692483710399E-05, 5.591713746943576435E-05, 6.279584083231437640E-05, 9.105792820296104511E-05, 0.0001153131102488857436 ),
 .UNSPECIFIED. ) ;
#60234 = CARTESIAN_POINT ( 'NONE',  ( -37.00000000000000711, 5.391785509270962784, 10.43555801961477236 ) ) ;
#60235 = CARTESIAN_POINT ( 'NONE',  ( 0.2653519991613836893, 6.104031847945017297, 10.61652626436030111 ) ) ;
#60236 = CARTESIAN_POINT ( 'NONE',  ( 2.261269890823172091, -1.189259211194653609, -7.547924622048553189 ) ) ;
#60237 = ORIENTED_EDGE ( 'NONE', *, *, #28228, .F. ) ;
#60238 = ORIENTED_EDGE ( 'NONE', *, *, #18836, .F. ) ;
#60239 = ORIENTED_EDGE ( 'NONE', *, *, #64237, .T. ) ;
#60240 = CARTESIAN_POINT ( 'NONE',  ( -2.952869152607111136, -4.384817011589735358, 11.17020052527586138 ) ) ;
#60241 = CIRCLE ( 'NONE', #37031, 7.499999999999988454 ) ;
#60242 = EDGE_CURVE ( 'NONE', #924, #5805, #54265, .T. ) ;
#60243 = CARTESIAN_POINT ( 'NONE',  ( 2.653899356900220941, 3.657605971842848636, -6.857477569908583703 ) ) ;
#60244 = ORIENTED_EDGE ( 'NONE', *, *, #42118, .F. ) ;
#60245 = CARTESIAN_POINT ( 'NONE',  ( -35.00000000000000000, 6.307491713049167004, -9.908974237959577991 ) ) ;
#60246 = LINE ( 'NONE', #30323, #60820 ) ;
#60247 = ORIENTED_EDGE ( 'NONE', *, *, #28382, .T. ) ;
#60248 = DIRECTION ( 'NONE',  ( 1.000000000000000000, 0.000000000000000000, -0.000000000000000000 ) ) ;
#60249 = CARTESIAN_POINT ( 'NONE',  ( -0.4456450841876022362, -28.11949765475245400, -13.91469577634640231 ) ) ;
#60250 = CARTESIAN_POINT ( 'NONE',  ( -4.989057617119011745, -0.9162120371760335003, 25.00000000000000000 ) ) ;
#60252 = VERTEX_POINT ( 'NONE', #28409 ) ;
#60251 = DIRECTION ( 'NONE',  ( -1.000000000000000000, -0.000000000000000000, -0.000000000000000000 ) ) ;
#60253 = FACE_OUTER_BOUND ( 'NONE', #36707, .T. ) ;
#60254 = ORIENTED_EDGE ( 'NONE', *, *, #23363, .F. ) ;
#60255 = LINE ( 'NONE', #14680, #60380 ) ;
#60256 = EDGE_CURVE ( 'NONE', #19077, #2801, #19219, .T. ) ;
#60257 = B_SPLINE_CURVE_WITH_KNOTS ( 'NONE', 3,
 ( #34926, #5361, #11323, #11000, #46906, #62191, #16643, #56561, #11645, #30604 ),
 .UNSPECIFIED., .F., .F.,
 ( 4, 3, 3, 4 ),
 ( 4.336808689942017736E-19, 6.607638129004463133E-05, 9.911389841680550718E-05, 0.0001667630577588626365 ),
 .UNSPECIFIED. ) ;
#60258 = EDGE_LOOP ( 'NONE', ( #56664, #25726, #45632, #19385 ) ) ;
#60259 = VECTOR ( 'NONE', #34089, 1000.000000000000000 ) ;
#60260 = FACE_OUTER_BOUND ( 'NONE', #8822, .T. ) ;
#60261 = CARTESIAN_POINT ( 'NONE',  ( 12.57979501679909440, -8.984612513102003817, -7.965368934693056069 ) ) ;
#60262 = CARTESIAN_POINT ( 'NONE',  ( -35.00000000000000000, 0.000000000000000000, 0.000000000000000000 ) ) ;
#60263 = CYLINDRICAL_SURFACE ( 'NONE', #11005, 6.936499999999988120 ) ;
#60264 = CARTESIAN_POINT ( 'NONE',  ( -22.27722019117890895, -0.6493872998088024984, -3.623937139367951588 ) ) ;
#60265 = LINE ( 'NONE', #50956, #34617 ) ;
#60266 = EDGE_CURVE ( 'NONE', #29257, #59691, #49053, .T. ) ;
#60267 = CARTESIAN_POINT ( 'NONE',  ( -35.00000000000000000, 11.56998259273177787, 3.827046518385122553 ) ) ;
#60268 = CARTESIAN_POINT ( 'NONE',  ( 0.000000000000000000, 6.664893814313728626, 3.439359016433498173 ) ) ;
#60269 = CARTESIAN_POINT ( 'NONE',  ( 2.000000000000001776, -4.409940824963459960, 5.354199675985231721 ) ) ;
#60271 = ORIENTED_EDGE ( 'NONE', *, *, #33644, .F. ) ;
#60270 = CARTESIAN_POINT ( 'NONE',  ( -27.32343372485685862, -2.674948176236188413, 1.382463360572558475 ) ) ;
#60272 = EDGE_LOOP ( 'NONE', ( #64792, #62752, #20431, #11854 ) ) ;
#60273 = CARTESIAN_POINT ( 'NONE',  ( 12.68490744323399433, -13.22581700042956498, -2.713934262790095087 ) ) ;
#60274 = ORIENTED_EDGE ( 'NONE', *, *, #17938, .T. ) ;
#60275 = EDGE_CURVE ( 'NONE', #35410, #26477, #4381, .T. ) ;
#60276 = VERTEX_POINT ( 'NONE', #49687 ) ;
#60277 = CARTESIAN_POINT ( 'NONE',  ( 1.283627346226615895, -12.57362488724973915, 0.5505361391623344591 ) ) ;
#60278 = DIRECTION ( 'NONE',  ( 0.9486832985018465170, 3.872673197958691324E-17, 0.3162277646628396943 ) ) ;
#60279 = CARTESIAN_POINT ( 'NONE',  ( 5.515188684475870851, 0.004893136156457998653, -0.002166413411657814019 ) ) ;
#60280 = CARTESIAN_POINT ( 'NONE',  ( -22.28939870658739864, 1.608176106660567983, -3.352428181135929997 ) ) ;
#60281 = CARTESIAN_POINT ( 'NONE',  ( 2.260457164925434359, 7.226149053011227785, 2.482766715768787158 ) ) ;
#60282 = CARTESIAN_POINT ( 'NONE',  ( -37.00000000000000711, 11.17622378668011685, -3.614449339633368119 ) ) ;
#60283 = VERTEX_POINT ( 'NONE', #34044 ) ;
#60284 = EDGE_CURVE ( 'NONE', #10035, #6763, #16024, .T. ) ;
#60285 = CARTESIAN_POINT ( 'NONE',  ( 2.305787727787084407, -5.970480882365253983, 4.792270232040873879 ) ) ;
#60286 = CYLINDRICAL_SURFACE ( 'NONE', #36614, 2.899999999999994582 ) ;
#60287 = CARTESIAN_POINT ( 'NONE',  ( -19.17656007471153146, -3.894919239584830439, 12.92680134493071797 ) ) ;
#60288 = EDGE_CURVE ( 'NONE', #29095, #11102, #5297, .T. ) ;
#60289 = ORIENTED_EDGE ( 'NONE', *, *, #13, .F. ) ;
#60290 = EDGE_CURVE ( 'NONE', #3684, #20446, #29831, .T. ) ;
#60291 = AXIS2_PLACEMENT_3D ( 'NONE', #64027, #18513, #14133 ) ;
#60292 = EDGE_CURVE ( 'NONE', #44595, #36164, #2235, .T. ) ;
#60293 = ADVANCED_FACE ( 'NONE', ( #38725 ), #14918, .T. ) ;
#60294 = CONICAL_SURFACE ( 'NONE', #20982, 7.938172270156617749, 1.280189991382167047 ) ;
#60295 = CARTESIAN_POINT ( 'NONE',  ( 46.63605190621407104, -0.6629852496305267406, -12.55202432522571421 ) ) ;
#60296 = EDGE_CURVE ( 'NONE', #38332, #8899, #37240, .T. ) ;
#60297 = CARTESIAN_POINT ( 'NONE',  ( -7.539837441135050611, -2.057183563332125154, 13.34261549860323015 ) ) ;
#60299 = AXIS2_PLACEMENT_3D ( 'NONE', #45379, #20449, #10790 ) ;
#60298 = CARTESIAN_POINT ( 'NONE',  ( -43.82484328533829654, -1.182663722159860376, -16.53294353590084143 ) ) ;
#60300 = VERTEX_POINT ( 'NONE', #49389 ) ;
#60301 = DIRECTION ( 'NONE',  ( 1.000000000000000000, 0.000000000000000000, 0.000000000000000000 ) ) ;
#60302 = CYLINDRICAL_SURFACE ( 'NONE', #24017, 2.899999999999994582 ) ;
#60303 = CARTESIAN_POINT ( 'NONE',  ( 3.848109687703774817, 8.028244186201112242, 8.930321068435377541 ) ) ;
#60304 = AXIS2_PLACEMENT_3D ( 'NONE', #33701, #18090, #23401 ) ;
#60305 = AXIS2_PLACEMENT_3D ( 'NONE', #4247, #40806, #581 ) ;
#60306 = LINE ( 'NONE', #14093, #40518 ) ;
#60307 = DIRECTION ( 'NONE',  ( -1.000000000000000000, -1.836970198721029688E-16, 0.000000000000000000 ) ) ;
#60308 = ORIENTED_EDGE ( 'NONE', *, *, #59615, .T. ) ;
#60309 = CARTESIAN_POINT ( 'NONE',  ( 2.241352910868908310, 0.08337961031704246850, 7.633946224498473931 ) ) ;
#60310 = DIRECTION ( 'NONE',  ( 1.000000000000000000, 0.000000000000000000, 0.000000000000000000 ) ) ;
#60311 = CARTESIAN_POINT ( 'NONE',  ( -36.00000000000000711, 10.68873102412852560, -6.950793414699682593 ) ) ;
#60312 = ORIENTED_EDGE ( 'NONE', *, *, #18876, .F. ) ;
#60313 = CARTESIAN_POINT ( 'NONE',  ( 11.39082382910284785, 0.2412655231989612459, 13.49807518737375744 ) ) ;
#60314 = CARTESIAN_POINT ( 'NONE',  ( 1.719304012338199517, 0.000000000000000000, 0.000000000000000000 ) ) ;
#60315 = ORIENTED_EDGE ( 'NONE', *, *, #47646, .F. ) ;
#60316 = EDGE_LOOP ( 'NONE', ( #27228, #20274, #746, #5562 ) ) ;
#60317 = ORIENTED_EDGE ( 'NONE', *, *, #7516, .T. ) ;
#60318 = EDGE_CURVE ( 'NONE', #21025, #17610, #4132, .T. ) ;
#60319 = ORIENTED_EDGE ( 'NONE', *, *, #56127, .T. ) ;
#60320 = DIRECTION ( 'NONE',  ( -1.000000000000000000, 0.000000000000000000, -0.000000000000000000 ) ) ;
#60321 = DIRECTION ( 'NONE',  ( 1.000000000000000000, 0.000000000000000000, 0.000000000000000000 ) ) ;
#60322 = DIRECTION ( 'NONE',  ( 1.000000000000000000, 0.000000000000000000, 0.000000000000000000 ) ) ;
#60323 = CARTESIAN_POINT ( 'NONE',  ( -3.740102306720532788, 25.00000000000000000, -6.044082642436763742 ) ) ;
#60324 = CARTESIAN_POINT ( 'NONE',  ( -12.85491158824215141, -29.00000000000000711, 3.284771503683518556 ) ) ;
#60325 = DIRECTION ( 'NONE',  ( -1.000000000000000000, 0.000000000000000000, 0.000000000000000000 ) ) ;
#60327 = ORIENTED_EDGE ( 'NONE', *, *, #26594, .F. ) ;
#60326 = CARTESIAN_POINT ( 'NONE',  ( -28.85619398320021745, 3.750539801530000439, 25.00000000000000000 ) ) ;
#60328 = CYLINDRICAL_SURFACE ( 'NONE', #60685, 12.74999999999999822 ) ;
#60329 = VERTEX_POINT ( 'NONE', #64622 ) ;
#60330 = CARTESIAN_POINT ( 'NONE',  ( 2.941278708680199916, 4.048809123187934844, 4.615461433467269003 ) ) ;
#60331 = ORIENTED_EDGE ( 'NONE', *, *, #44334, .F. ) ;
#60332 = EDGE_CURVE ( 'NONE', #22711, #9287, #52122, .T. ) ;
#60333 = ORIENTED_EDGE ( 'NONE', *, *, #51322, .T. ) ;
#60334 = DIRECTION ( 'NONE',  ( 0.000000000000000000, 0.000000000000000000, 1.000000000000000000 ) ) ;
#60335 = CARTESIAN_POINT ( 'NONE',  ( 13.40144019692491995, -30.08877117594913742, 6.927253557473016521 ) ) ;
#60336 = VECTOR ( 'NONE', #38522, 1000.000000000000000 ) ;
#60337 = CARTESIAN_POINT ( 'NONE',  ( 2.903928887688582705, 7.046356840275206146, 5.221047506680442929 ) ) ;
#60338 = CARTESIAN_POINT ( 'NONE',  ( 3.047904605210433271, 7.845751380824992793, -0.9519317672905968086 ) ) ;
#60339 = DIRECTION ( 'NONE',  ( 1.000000000000000000, 0.000000000000000000, 0.000000000000000000 ) ) ;
#60340 = CARTESIAN_POINT ( 'NONE',  ( 2.280717697722505655, 5.957695241724533908, 4.794838658391401331 ) ) ;
#60341 = VERTEX_POINT ( 'NONE', #53704 ) ;
#60342 = AXIS2_PLACEMENT_3D ( 'NONE', #40365, #40044, #55016 ) ;
#60343 = ORIENTED_EDGE ( 'NONE', *, *, #43276, .T. ) ;
#60344 = FACE_OUTER_BOUND ( 'NONE', #22321, .T. ) ;
#60345 = VERTEX_POINT ( 'NONE', #34384 ) ;
#60346 = EDGE_CURVE ( 'NONE', #58059, #35179, #54689, .T. ) ;
#60347 = EDGE_LOOP ( 'NONE', ( #3715, #3769, #21084, #11478 ) ) ;
#60348 = CARTESIAN_POINT ( 'NONE',  ( 35.00000000000000000, 1.262958560998929558, 12.12087942037208066 ) ) ;
#60349 = AXIS2_PLACEMENT_3D ( 'NONE', #44819, #34817, #49820 ) ;
#60350 = CARTESIAN_POINT ( 'NONE',  ( 2.241537034860906275, 1.321063441155988949, 7.519304283075082473 ) ) ;
#60351 = CARTESIAN_POINT ( 'NONE',  ( 17.10287315442671030, -9.289536693978741155, 7.615149052798787288 ) ) ;
#60352 = EDGE_CURVE ( 'NONE', #58929, #30664, #23440, .T. ) ;
#60353 = CARTESIAN_POINT ( 'NONE',  ( -22.27709082389155171, 1.005749854561714507, -3.541295940224341354 ) ) ;
#60354 = CARTESIAN_POINT ( 'NONE',  ( -10.87643784907710298, -4.898157848850412499, -10.96305477394234273 ) ) ;
#60355 = DIRECTION ( 'NONE',  ( 1.000000000000000000, -0.000000000000000000, 0.000000000000000000 ) ) ;
#60356 = ORIENTED_EDGE ( 'NONE', *, *, #51785, .F. ) ;
#60357 = ORIENTED_EDGE ( 'NONE', *, *, #21113, .F. ) ;
#60358 = CARTESIAN_POINT ( 'NONE',  ( 1.000000000000000888, -2.315790869867103474, 7.133520354428079635 ) ) ;
#60359 = FACE_OUTER_BOUND ( 'NONE', #5393, .T. ) ;
#60360 = DIRECTION ( 'NONE',  ( 0.000000000000000000, -0.01356324068817998940, 0.9999080150203990547 ) ) ;
#60361 = EDGE_CURVE ( 'NONE', #8080, #42619, #25573, .T. ) ;
#60362 = CARTESIAN_POINT ( 'NONE',  ( -35.00000000000000000, -11.50504120060940316, -4.018060380616521599 ) ) ;
#60363 = AXIS2_PLACEMENT_3D ( 'NONE', #63468, #12945, #8943 ) ;
#60364 = CARTESIAN_POINT ( 'NONE',  ( 37.00000000000000711, 4.705694406421931860E-17, -3.469127814946512892E-15 ) ) ;
#60365 = ADVANCED_FACE ( 'NONE', ( #10744 ), #50998, .T. ) ;
#60366 = CIRCLE ( 'NONE', #34859, 12.18649999999999878 ) ;
#60367 = CARTESIAN_POINT ( 'NONE',  ( 6.812204945636112896, -4.138731716409435712, -12.84993773446340803 ) ) ;
#60368 = DIRECTION ( 'NONE',  ( 0.000000000000000000, 1.000000000000000000, -0.000000000000000000 ) ) ;
#60369 = EDGE_CURVE ( 'NONE', #15685, #6304, #11750, .T. ) ;
#60370 = CARTESIAN_POINT ( 'NONE',  ( 2.000000000000001776, 6.906413915731199005, -0.6453518998146886565 ) ) ;
#60371 = EDGE_LOOP ( 'NONE', ( #13942, #18686, #20618, #52779 ) ) ;
#60372 = CARTESIAN_POINT ( 'NONE',  ( 2.994568964204213035, -0.3996732855055282752, 7.875338388187476113 ) ) ;
#60373 = CARTESIAN_POINT ( 'NONE',  ( 2.000000000000001776, 6.812627895098307462, -0.04423456934727655609 ) ) ;
#60374 = DIRECTION ( 'NONE',  ( 1.000000000000000000, 0.000000000000000000, -0.000000000000000000 ) ) ;
#60375 = AXIS2_PLACEMENT_3D ( 'NONE', #12380, #32650, #9276 ) ;
#60376 = EDGE_CURVE ( 'NONE', #49890, #7383, #55319, .T. ) ;
#60377 = CARTESIAN_POINT ( 'NONE',  ( -2.195494320951781653, -31.13300424730296001, -14.33890400575618074 ) ) ;
#60378 = CARTESIAN_POINT ( 'NONE',  ( 35.00000000000000000, 7.146664589317909488, -9.321877890560465119 ) ) ;
#60379 = TOROIDAL_SURFACE ( 'NONE', #15795, 20.19615242270663558, 4.000000000000000000 ) ;
#60380 = VECTOR ( 'NONE', #60925, 1000.000000000000114 ) ;
#60381 =( BOUNDED_SURFACE ( )  B_SPLINE_SURFACE ( 3, 1, ( 
 ( #36453, #31769 ),
 ( #11500, #11186 ),
 ( #41763, #56069 ),
 ( #26802, #40796 ) ),
 .UNSPECIFIED., .F., .F., .F. ) 
 B_SPLINE_SURFACE_WITH_KNOTS ( ( 4, 4 ),
 ( 2, 2 ),
 ( 0.000000000000000000, 1.000000000000000000 ),
 ( 0.000000000000000000, 1.000000000000000000 ),
 .UNSPECIFIED. ) 
 GEOMETRIC_REPRESENTATION_ITEM ( )  RATIONAL_B_SPLINE_SURFACE ( (
 ( 1.000000000000000000, 1.000000000000000000),
 ( 0.9856612449720755231, 0.9999558406602322425),
 ( 0.9856612449720755231, 0.9999558406602322425),
 ( 1.000000000000000000, 1.000000000000000000) ) ) 
 REPRESENTATION_ITEM ( '' )  SURFACE ( )  );
#60382 = VERTEX_POINT ( 'NONE', #45667 ) ;
#60383 = CARTESIAN_POINT ( 'NONE',  ( 2.269879328256730666, -2.474479066008269168, 7.232310762824155859 ) ) ;
#60384 = CARTESIAN_POINT ( 'NONE',  ( 27.08585833250204900, 12.95103964514429684, 3.823327208526503984 ) ) ;
#60385 = CARTESIAN_POINT ( 'NONE',  ( 11.12775972613914099, -27.03492176219597454, -13.41779706364883396 ) ) ;
#60386 = ORIENTED_EDGE ( 'NONE', *, *, #36424, .T. ) ;
#60387 = VECTOR ( 'NONE', #57260, 1000.000000000000000 ) ;
#60388 = CARTESIAN_POINT ( 'NONE',  ( 0.8375941296792348556, -6.548446001455606513, 10.57337970710551822 ) ) ;
#60389 = CYLINDRICAL_SURFACE ( 'NONE', #1309, 12.74999999999999822 ) ;
#60390 = CARTESIAN_POINT ( 'NONE',  ( 5.514624014163232779, 0.004045310349816153353, -0.0008859786816847026571 ) ) ;
#60392 = ORIENTED_EDGE ( 'NONE', *, *, #60114, .F. ) ;
#60391 = CARTESIAN_POINT ( 'NONE',  ( 0.2833330754217411318, -8.029341648258412789, 9.254504746325759257 ) ) ;
#60393 = CARTESIAN_POINT ( 'NONE',  ( -14.23149639848878678, 7.941839253138341270, 8.998400932456021906 ) ) ;
#60394 = CARTESIAN_POINT ( 'NONE',  ( 37.00000000000000711, -10.02106554660713833, -7.882940143791743459 ) ) ;
#60395 = ORIENTED_EDGE ( 'NONE', *, *, #54218, .F. ) ;
#60396 = DIRECTION ( 'NONE',  ( -1.000000000000000000, 0.000000000000000000, 0.000000000000000000 ) ) ;
#60397 = EDGE_CURVE ( 'NONE', #43263, #18227, #5425, .T. ) ;
#60398 = DIRECTION ( 'NONE',  ( -1.000000000000000000, -0.000000000000000000, 0.000000000000000000 ) ) ;
#60399 = CARTESIAN_POINT ( 'NONE',  ( -14.37821012703996892, 8.339393263347453455, -10.61631806211926587 ) ) ;
#60400 = DIRECTION ( 'NONE',  ( 1.000000000000000000, 0.000000000000000000, 0.000000000000000000 ) ) ;
#60401 = FACE_OUTER_BOUND ( 'NONE', #63823, .T. ) ;
#60402 = B_SPLINE_CURVE_WITH_KNOTS ( 'NONE', 3,
 ( #49825, #56104, #24546, #44825, #12451, #43047, #3166, #48398, #58708, #23431, #27115, #43709, #52721, #12137, #47722, #37406, #38390, #63006, #2166 ),
 .UNSPECIFIED., .F., .F.,
 ( 4, 3, 3, 3, 3, 3, 4 ),
 ( 1.158841720744533638E-17, 4.457896483014492915E-05, 6.639290541541691376E-05, 8.820687556478305888E-05, 0.0001100173248778826531, 0.0001545671401658026156, 0.0001830328308068575197 ),
 .UNSPECIFIED. ) ;
#60403 = CYLINDRICAL_SURFACE ( 'NONE', #55695, 5.000000000000000888 ) ;
#60404 = DIRECTION ( 'NONE',  ( 0.000000000000000000, -0.8515178078024813191, 0.5243256840888652626 ) ) ;
#60405 = ORIENTED_EDGE ( 'NONE', *, *, #31424, .T. ) ;
#60406 = ORIENTED_EDGE ( 'NONE', *, *, #17020, .F. ) ;
#60407 = CARTESIAN_POINT ( 'NONE',  ( 2.290907136833254309, -5.041121061899943356, 5.755317856506266594 ) ) ;
#60408 = EDGE_LOOP ( 'NONE', ( #65771, #19650, #3022, #61635 ) ) ;
#60409 = ADVANCED_FACE ( 'NONE', ( #65296 ), #47891, .T. ) ;
#60410 = SURFACE_STYLE_USAGE ( .BOTH. , #39142 ) ;
#60411 = CARTESIAN_POINT ( 'NONE',  ( 2.000000000000001776, 3.979254915827366901, 5.681598592373755530 ) ) ;
#60412 = CIRCLE ( 'NONE', #49842, 12.74999999999999822 ) ;
#60413 = DIRECTION ( 'NONE',  ( 0.3865475372811021382, 0.2971585806051794676, 0.8730852074079769043 ) ) ;
#60414 = VERTEX_POINT ( 'NONE', #40019 ) ;
#60415 = CARTESIAN_POINT ( 'NONE',  ( 37.00000000000000711, -5.246972444133939817, 10.99909370905162298 ) ) ;
#60416 = CARTESIAN_POINT ( 'NONE',  ( 10.88441259213023393, 11.89247429979993242, -1.605920490876132867 ) ) ;
#60417 = CIRCLE ( 'NONE', #42311, 6.936499999999992561 ) ;
#60418 = DIRECTION ( 'NONE',  ( -1.000000000000000000, -0.000000000000000000, 0.000000000000000000 ) ) ;
#60419 = EDGE_LOOP ( 'NONE', ( #26143, #45889, #65129, #33209 ) ) ;
#60420 = ORIENTED_EDGE ( 'NONE', *, *, #269, .F. ) ;
#60421 = FACE_OUTER_BOUND ( 'NONE', #10754, .T. ) ;
#60422 = EDGE_CURVE ( 'NONE', #30330, #47727, #3340, .T. ) ;
#60423 = EDGE_CURVE ( 'NONE', #7557, #24932, #29882, .T. ) ;
#60424 = ORIENTED_EDGE ( 'NONE', *, *, #28499, .T. ) ;
#60425 = FACE_OUTER_BOUND ( 'NONE', #16019, .T. ) ;
#60426 = ORIENTED_EDGE ( 'NONE', *, *, #26044, .F. ) ;
#60427 = CARTESIAN_POINT ( 'NONE',  ( 0.000000000000000000, -1.754183803416492493, -6.711026108862277795 ) ) ;
#60428 = AXIS2_PLACEMENT_3D ( 'NONE', #27852, #2616, #43129 ) ;
#60429 = ADVANCED_FACE ( 'NONE', ( #24745 ), #64070, .F. ) ;
#60431 = CIRCLE ( 'NONE', #31744, 5.000000000000000000 ) ;
#60430 = CARTESIAN_POINT ( 'NONE',  ( -29.68541646480307605, -1.201201861335963628, 11.94168801375079703 ) ) ;
#60432 = CARTESIAN_POINT ( 'NONE',  ( 2.963017218115616913, -4.265970453343964408, 6.619413971958201692 ) ) ;
#60433 = CARTESIAN_POINT ( 'NONE',  ( 0.000000000000000000, 4.570217215903371155, 5.218059682435623792 ) ) ;
#60434 = CARTESIAN_POINT ( 'NONE',  ( 35.00000000000000000, 10.25474254703961918, 6.584150480049438592 ) ) ;
#60435 = ORIENTED_EDGE ( 'NONE', *, *, #34238, .F. ) ;
#60436 = CARTESIAN_POINT ( 'NONE',  ( 2.242418902651939661, 7.634109827927225922, -0.09970190380435364763 ) ) ;
#60437 = DIRECTION ( 'NONE',  ( 0.000000000000000000, 0.01356324068817992175, -0.9999080150203990547 ) ) ;
#60438 = CARTESIAN_POINT ( 'NONE',  ( 2.241536586108912932, 5.852386772940070259, 4.902521014023349721 ) ) ;
#60439 = CARTESIAN_POINT ( 'NONE',  ( 12.73595680732062085, 12.88342186531470546, -4.037885783516507843 ) ) ;
#60440 = CARTESIAN_POINT ( 'NONE',  ( 3.031336079629145530, -3.088871717871215505, -7.268683861177180461 ) ) ;
#60441 = CARTESIAN_POINT ( 'NONE',  ( 3.152665057734040488, 0.000000000000000000, 0.000000000000000000 ) ) ;
#60442 = LINE ( 'NONE', #25196, #15349 ) ;
#60443 = CARTESIAN_POINT ( 'NONE',  ( 0.000000000000000000, 1.779948802829816490, 6.576141558201244131 ) ) ;
#60444 = EDGE_CURVE ( 'NONE', #14488, #37865, #24577, .T. ) ;
#60445 = VERTEX_POINT ( 'NONE', #470 ) ;
#60446 = CARTESIAN_POINT ( 'NONE',  ( -17.49774675589618411, 7.618938804295157574, -9.273320750912958488 ) ) ;
#60447 = EDGE_CURVE ( 'NONE', #46217, #51182, #21181, .T. ) ;
#60448 = ORIENTED_EDGE ( 'NONE', *, *, #48952, .F. ) ;
#60449 = CARTESIAN_POINT ( 'NONE',  ( 35.00000000000000000, -1.030638227056475120, 12.14284015767850811 ) ) ;
#60450 = CARTESIAN_POINT ( 'NONE',  ( -22.28236030719477512, -3.683993210674363361, 0.3108070568283768376 ) ) ;
#60451 = CARTESIAN_POINT ( 'NONE',  ( -18.08686583997217667, 5.372364593331139915, -12.38728941600954769 ) ) ;
#60452 = CARTESIAN_POINT ( 'NONE',  ( 35.00000000000000000, 9.557269938331552694, -7.561043153948004303 ) ) ;
#60453 = CARTESIAN_POINT ( 'NONE',  ( 2.260457164926975349, 2.482766715767231069, -7.226149053012312251 ) ) ;
#60454 = ORIENTED_EDGE ( 'NONE', *, *, #18332, .T. ) ;
#60455 = CARTESIAN_POINT ( 'NONE',  ( -35.00000000000000000, -10.02106554660702820, -7.882940143791882903 ) ) ;
#60456 = CARTESIAN_POINT ( 'NONE',  ( 2.907497136250260628, 2.346692756478441666, -7.497839665536633724 ) ) ;
#60457 = CARTESIAN_POINT ( 'NONE',  ( 35.00000000000000000, 4.705694406421931860E-17, -3.469127814946512892E-15 ) ) ;
#60458 = CARTESIAN_POINT ( 'NONE',  ( 47.00000000000000711, 4.705694406421931860E-17, -3.469127814946512892E-15 ) ) ;
#60459 = B_SPLINE_CURVE_WITH_KNOTS ( 'NONE', 3,
 ( #10587, #40526, #36533, #65775, #41173, #61452 ),
 .UNSPECIFIED., .F., .F.,
 ( 4, 2, 4 ),
 ( 0.0001654224980408285247, 0.0006219428995476449255, 0.001078463301054461299 ),
 .UNSPECIFIED. ) ;
#60460 = CARTESIAN_POINT ( 'NONE',  ( -18.87003134133906102, -4.090855072109758517, 11.28365501786238490 ) ) ;
#60461 = CARTESIAN_POINT ( 'NONE',  ( 2.889800649504073782, 0.06738247734058958049, -6.121013568931505944 ) ) ;
#60462 = ORIENTED_EDGE ( 'NONE', *, *, #65175, .T. ) ;
#60463 = AXIS2_PLACEMENT_3D ( 'NONE', #23662, #63871, #53915 ) ;
#60464 = CARTESIAN_POINT ( 'NONE',  ( 5.514970785353741078, 0.004233694591582517000, -0.002093325033904037177 ) ) ;
#60465 = ORIENTED_EDGE ( 'NONE', *, *, #1512, .T. ) ;
#60466 = CARTESIAN_POINT ( 'NONE',  ( 0.2650492594609233366, 12.24562116224018382, 0.1101156276917182181 ) ) ;
#60467 = CARTESIAN_POINT ( 'NONE',  ( -22.94572469358970679, -4.424217216616509241, 2.078200699019450148 ) ) ;
#60468 = CARTESIAN_POINT ( 'NONE',  ( -37.00000000000000711, 0.000000000000000000, -1.750000000000000000 ) ) ;
#60469 = CARTESIAN_POINT ( 'NONE',  ( 2.000000000000001776, 1.865193240757184290, -6.552473556515182374 ) ) ;
#60470 = VERTEX_POINT ( 'NONE', #45021 ) ;
#60471 = ORIENTED_EDGE ( 'NONE', *, *, #8980, .T. ) ;
#60472 = DIRECTION ( 'NONE',  ( 0.000000000000000000, 1.000000000000000000, 0.000000000000000000 ) ) ;
#60473 = ORIENTED_EDGE ( 'NONE', *, *, #39388, .T. ) ;
#60474 = AXIS2_PLACEMENT_3D ( 'NONE', #25729, #5124, #46020 ) ;
#60475 = EDGE_CURVE ( 'NONE', #14035, #12068, #39423, .T. ) ;
#60476 = CARTESIAN_POINT ( 'NONE',  ( 2.655192694323992519, 5.293797899975493770, 8.010337395398677174 ) ) ;
#60477 = CYLINDRICAL_SURFACE ( 'NONE', #3502, 4.999999999999999112 ) ;
#60478 = DIRECTION ( 'NONE',  ( 1.000000000000000000, 0.000000000000000000, 0.000000000000000000 ) ) ;
#60479 = CARTESIAN_POINT ( 'NONE',  ( 35.00000000000000000, -11.16627499335657703, -3.645068577059991988 ) ) ;
#60480 = CARTESIAN_POINT ( 'NONE',  ( 2.241352910868908754, 3.889181972941450738, 6.569501556381455387 ) ) ;
#60481 = LINE ( 'NONE', #64800, #19010 ) ;
#60482 = DIRECTION ( 'NONE',  ( 0.000000000000000000, -0.01356324068817998073, 0.9999080150203990547 ) ) ;
#60483 = ORIENTED_EDGE ( 'NONE', *, *, #25601, .F. ) ;
#60485 = ORIENTED_EDGE ( 'NONE', *, *, #31911, .T. ) ;
#60484 = CARTESIAN_POINT ( 'NONE',  ( 2.931247277082690061, -2.338794445044939163, -7.508560300462427506 ) ) ;
#60486 = VECTOR ( 'NONE', #63512, 1000.000000000000000 ) ;
#60487 = ORIENTED_EDGE ( 'NONE', *, *, #23547, .T. ) ;
#60488 = DIRECTION ( 'NONE',  ( 0.000000000000000000, 0.04924826701373889726, 0.9987865678893281807 ) ) ;
#60489 = DIRECTION ( 'NONE',  ( 1.000000000000000000, 1.685093406416449860E-16, -1.011030131491581592E-17 ) ) ;
#60490 = EDGE_CURVE ( 'NONE', #35533, #36952, #56654, .T. ) ;
#60491 = ORIENTED_EDGE ( 'NONE', *, *, #5447, .T. ) ;
#60492 = DIRECTION ( 'NONE',  ( 1.000000000000000000, -0.000000000000000000, 0.000000000000000000 ) ) ;
#60493 = ORIENTED_EDGE ( 'NONE', *, *, #9920, .F. ) ;
#60494 = CARTESIAN_POINT ( 'NONE',  ( 36.00000000000000711, 1.286231064351314624, -12.68495603654572257 ) ) ;
#60495 = CARTESIAN_POINT ( 'NONE',  ( 1.937114397841935398, 10.63710405811943716, -7.182898292393653961 ) ) ;
#60496 = CARTESIAN_POINT ( 'NONE',  ( 35.00000000000000000, -11.72397916322011824, 0.7214809346829776926 ) ) ;
#60497 = CARTESIAN_POINT ( 'NONE',  ( 4.365482547053908924, -10.79959492482372241, 5.234344269312817488 ) ) ;
#60498 = ORIENTED_EDGE ( 'NONE', *, *, #55475, .T. ) ;
#60499 = VERTEX_POINT ( 'NONE', #56974 ) ;
#60500 = CARTESIAN_POINT ( 'NONE',  ( 2.000000000000001776, 0.000000000000000000, 0.000000000000000000 ) ) ;
#60501 = VERTEX_POINT ( 'NONE', #46653 ) ;
#60502 = EDGE_CURVE ( 'NONE', #52979, #54859, #50533, .T. ) ;
#60503 = ADVANCED_FACE ( 'NONE', ( #12372 ), #62581, .T. ) ;
#60504 = DIRECTION ( 'NONE',  ( -1.000000000000000000, 0.000000000000000000, -0.000000000000000000 ) ) ;
#60505 = ORIENTED_EDGE ( 'NONE', *, *, #47778, .F. ) ;
#60506 = VERTEX_POINT ( 'NONE', #52647 ) ;
#60507 = ORIENTED_EDGE ( 'NONE', *, *, #26048, .T. ) ;
#60508 = CARTESIAN_POINT ( 'NONE',  ( 2.430348790456883901, -5.769383131055034752, 5.095533593439705022 ) ) ;
#60509 = CARTESIAN_POINT ( 'NONE',  ( 0.8375941296786605372, 11.54987202580242389, 4.612912274495619691 ) ) ;
#60510 = AXIS2_PLACEMENT_3D ( 'NONE', #13036, #27333, #18372 ) ;
#60512 = AXIS2_PLACEMENT_3D ( 'NONE', #63150, #27566, #6657 ) ;
#60511 = CARTESIAN_POINT ( 'NONE',  ( 35.00000000000000000, 4.705694406421931860E-17, -3.469127814946512892E-15 ) ) ;
#60513 = CYLINDRICAL_SURFACE ( 'NONE', #46821, 7.115568257478080305 ) ;
#60514 = CYLINDRICAL_SURFACE ( 'NONE', #54700, 1.500000000000000444 ) ;
#60515 = VERTEX_POINT ( 'NONE', #26700 ) ;
#60516 = CARTESIAN_POINT ( 'NONE',  ( 2.249013661412014642, -2.498855301843467380, -7.216565855998053891 ) ) ;
#60517 = VERTEX_POINT ( 'NONE', #1107 ) ;
#60518 = AXIS2_PLACEMENT_3D ( 'NONE', #2063, #37959, #22327 ) ;
#60519 = FACE_OUTER_BOUND ( 'NONE', #4208, .T. ) ;
#60520 = CARTESIAN_POINT ( 'NONE',  ( 35.00000000000000000, 4.705694406421931860E-17, -3.469127814946512892E-15 ) ) ;
#60521 = ORIENTED_EDGE ( 'NONE', *, *, #30760, .T. ) ;
#60522 = CARTESIAN_POINT ( 'NONE',  ( 0.2911222467163514516, -10.71854909364322772, 5.940753417478891407 ) ) ;
#60523 = CARTESIAN_POINT ( 'NONE',  ( 26.83124887464803976, 11.22347478894700679, 4.259285346550930385 ) ) ;
#60524 = CARTESIAN_POINT ( 'NONE',  ( 2.273267844204860832, -6.695181685739923338, -3.690689057641690418 ) ) ;
#60525 = CIRCLE ( 'NONE', #46761, 12.74999999999999822 ) ;
#60526 = VERTEX_POINT ( 'NONE', #47638 ) ;
#60527 = DIRECTION ( 'NONE',  ( 1.000000000000000000, 0.000000000000000000, -0.000000000000000000 ) ) ;
#60528 = AXIS2_PLACEMENT_3D ( 'NONE', #22124, #47732, #62675 ) ;
#60529 = ORIENTED_EDGE ( 'NONE', *, *, #59917, .F. ) ;
#60530 = CARTESIAN_POINT ( 'NONE',  ( -10.64440273086534816, -9.782391350870085489, -6.950960968970274934 ) ) ;
#60531 = DIRECTION ( 'NONE',  ( 0.000000000000000000, 0.2960891610144441022, 0.9551603052523501836 ) ) ;
#60532 = CARTESIAN_POINT ( 'NONE',  ( 2.573738926104375935, 6.822065037112484909, -3.667129335223129782 ) ) ;
#60533 = CYLINDRICAL_SURFACE ( 'NONE', #20285, 12.18650000000000055 ) ;
#60534 = CARTESIAN_POINT ( 'NONE',  ( 13.41118187415329643, 10.79912113741252178, -5.237416537976061548 ) ) ;
#60535 = ORIENTED_EDGE ( 'NONE', *, *, #23340, .T. ) ;
#60536 = EDGE_CURVE ( 'NONE', #52831, #47834, #16409, .T. ) ;
#60537 = CYLINDRICAL_SURFACE ( 'NONE', #38783, 4.999999999999999112 ) ;
#60539 = CIRCLE ( 'NONE', #48839, 4.999999999999999112 ) ;
#60538 = CARTESIAN_POINT ( 'NONE',  ( 36.00000000000000711, -12.68495603654572612, -1.286231064351273989 ) ) ;
#60540 = DIRECTION ( 'NONE',  ( 0.3939253465568944290, -0.8008152550167628725, 0.4511294145502680597 ) ) ;
#60541 = CARTESIAN_POINT ( 'NONE',  ( 3.100650473569583010, 3.562766772868595222, 7.074394303868141165 ) ) ;
#60542 = EDGE_CURVE ( 'NONE', #27686, #62900, #50078, .T. ) ;
#60543 = CARTESIAN_POINT ( 'NONE',  ( -19.56743653832046803, -30.00000000000000000, -5.000000000000000888 ) ) ;
#60544 = CARTESIAN_POINT ( 'NONE',  ( -22.30625920655495165, 2.610366806364701642, -2.750410778797873323 ) ) ;
#60545 = CARTESIAN_POINT ( 'NONE',  ( -7.489022030332961322, -5.127957880411574187, -10.84914964302385521 ) ) ;
#60546 = CARTESIAN_POINT ( 'NONE',  ( 2.241352910868908754, 1.243507963608094347, 7.532448145350512547 ) ) ;
#60547 = AXIS2_PLACEMENT_3D ( 'NONE', #3672, #44196, #29540 ) ;
#60548 = EDGE_CURVE ( 'NONE', #62086, #7910, #46901, .T. ) ;
#60549 = VECTOR ( 'NONE', #51721, 1000.000000000000000 ) ;
#60550 = ORIENTED_EDGE ( 'NONE', *, *, #21227, .F. ) ;
#60551 = CARTESIAN_POINT ( 'NONE',  ( -27.10128162969864007, -1.304299867635194232, -1.945744751331073497 ) ) ;
#60553 = EDGE_LOOP ( 'NONE', ( #61256, #32810, #45151, #54031 ) ) ;
#60552 = EDGE_CURVE ( 'NONE', #61981, #21190, #38384, .T. ) ;
#60554 = DIRECTION ( 'NONE',  ( -0.9748757316300199482, 0.000000000000000000, 0.2227494284590502138 ) ) ;
#60555 = EDGE_CURVE ( 'NONE', #25882, #16541, #10756, .T. ) ;
#60556 = FACE_OUTER_BOUND ( 'NONE', #24737, .T. ) ;
#60557 = CARTESIAN_POINT ( 'NONE',  ( 3.152665057734040488, 0.000000000000000000, 0.000000000000000000 ) ) ;
#60558 = CARTESIAN_POINT ( 'NONE',  ( 2.241352910868908754, 3.889181972941450738, 6.569501556381455387 ) ) ;
#60559 = EDGE_CURVE ( 'NONE', #56061, #15944, #53710, .T. ) ;
#60560 = ORIENTED_EDGE ( 'NONE', *, *, #4631, .T. ) ;
#60561 = ORIENTED_EDGE ( 'NONE', *, *, #64246, .T. ) ;
#60562 = VERTEX_POINT ( 'NONE', #19914 ) ;
#60563 = CARTESIAN_POINT ( 'NONE',  ( 28.90977330190072792, -10.36490708579996678, 6.051299003903356954 ) ) ;
#60564 = AXIS2_PLACEMENT_3D ( 'NONE', #58304, #57318, #22380 ) ;
#60565 = FACE_OUTER_BOUND ( 'NONE', #51991, .T. ) ;
#60566 = EDGE_CURVE ( 'NONE', #49238, #4915, #51369, .T. ) ;
#60567 = ORIENTED_EDGE ( 'NONE', *, *, #22048, .F. ) ;
#60568 = CARTESIAN_POINT ( 'NONE',  ( 2.406456491625824867, -0.6290357040720556681, -10.41426194695600671 ) ) ;
#60569 = DIRECTION ( 'NONE',  ( -1.000000000000000000, 0.000000000000000000, 0.000000000000000000 ) ) ;
#60570 = VECTOR ( 'NONE', #42429, 1000.000000000000000 ) ;
#60571 = DIRECTION ( 'NONE',  ( -1.000000000000000000, 0.000000000000000000, 0.000000000000000000 ) ) ;
#60572 = EDGE_LOOP ( 'NONE', ( #65398, #31305, #24298, #15766 ) ) ;
#60573 =( BOUNDED_SURFACE ( )  B_SPLINE_SURFACE ( 3, 1, ( 
 ( #53789, #8222 ),
 ( #28493, #3250 ),
 ( #23522, #64077 ),
 ( #38811, #33801 ) ),
 .UNSPECIFIED., .F., .F., .F. ) 
 B_SPLINE_SURFACE_WITH_KNOTS ( ( 4, 4 ),
 ( 2, 2 ),
 ( 0.000000000000000000, 1.000000000000000000 ),
 ( 0.000000000000000000, 1.000000000000000000 ),
 .UNSPECIFIED. ) 
 GEOMETRIC_REPRESENTATION_ITEM ( )  RATIONAL_B_SPLINE_SURFACE ( (
 ( 1.000000000000000000, 1.000000000000000000),
 ( 0.9856612449720755231, 0.9999558406602322425),
 ( 0.9856612449720755231, 0.9999558406602322425),
 ( 1.000000000000000000, 1.000000000000000000) ) ) 
 REPRESENTATION_ITEM ( '' )  SURFACE ( )  );
#60574 = CARTESIAN_POINT ( 'NONE',  ( -22.31099767395441091, 0.2534174342804221824, 3.774495463598458223 ) ) ;
#60575 = EDGE_CURVE ( 'NONE', #49787, #46103, #39867, .T. ) ;
#60576 = CARTESIAN_POINT ( 'NONE',  ( -7.529925403076002333, -31.54078451673387917, -13.99923386364710609 ) ) ;
#60577 = FACE_OUTER_BOUND ( 'NONE', #60817, .T. ) ;
#60579 = ORIENTED_EDGE ( 'NONE', *, *, #42785, .F. ) ;
#60578 = CARTESIAN_POINT ( 'NONE',  ( -27.10512513516316702, 1.709353012333669319, 1.618446180706308635 ) ) ;
#60580 = DIRECTION ( 'NONE',  ( -1.000000000000000000, 0.000000000000000000, -0.000000000000000000 ) ) ;
#60581 = VERTEX_POINT ( 'NONE', #30223 ) ;
#60582 = DIRECTION ( 'NONE',  ( 0.000000000000000000, 0.7621620551276376831, -0.6473862847818260269 ) ) ;
#60583 = AXIS2_PLACEMENT_3D ( 'NONE', #1067, #7032, #21336 ) ;
#60584 = ORIENTED_EDGE ( 'NONE', *, *, #26258, .F. ) ;
#60585 = DIRECTION ( 'NONE',  ( -1.000000000000000000, 0.000000000000000000, 0.000000000000000000 ) ) ;
#60586 = DIRECTION ( 'NONE',  ( -1.000000000000000000, 0.000000000000000000, 0.000000000000000000 ) ) ;
#60587 = DIRECTION ( 'NONE',  ( 0.000000000000000000, 0.01356324068817300540, -0.9999080150203989437 ) ) ;
#60588 = CARTESIAN_POINT ( 'NONE',  ( 1.194176325881346035, -6.717888447700763876, -10.60746084433563041 ) ) ;
#60589 = CARTESIAN_POINT ( 'NONE',  ( 35.00000000000000000, -2.250029553613672295, 12.54989509947652770 ) ) ;
#60590 = FACE_OUTER_BOUND ( 'NONE', #3634, .T. ) ;
#60591 = B_SPLINE_CURVE_WITH_KNOTS ( 'NONE', 3,
 ( #20795, #35420, #20135, #5859, #51065, #45087, #41063, #35073, #46080, #40402, #24805, #40746, #50733, #41383, #10471, #40076, #61340, #46392, #20470, #30748, #840, #55726, #10157, #19817 ),
 .UNSPECIFIED., .F., .F.,
 ( 4, 2, 2, 2, 2, 2, 2, 2, 2, 2, 2, 4 ),
 ( 2.602085213965210642E-18, 0.001217752653192586071, 0.001826628979788878782, 0.002435505306385171709, 0.003044381632981464636, 0.003653257959577757129, 0.004871010612770343418, 0.006088763265962928405, 0.007306515919155514259, 0.008524268572348100981, 0.009133144898944393908, 0.009742021225540686835 ),
 .UNSPECIFIED. ) ;
#60592 = CARTESIAN_POINT ( 'NONE',  ( 12.19547418290646590, 0.02891602860409012848, 11.99999999999999467 ) ) ;
#60593 = DIRECTION ( 'NONE',  ( 0.000000000000000000, 0.01356324068817998767, -0.9999080150203990547 ) ) ;
#60594 = DIRECTION ( 'NONE',  ( 0.000000000000000000, 0.5155538571770231782, -0.8568571761675882748 ) ) ;
#60596 = ORIENTED_EDGE ( 'NONE', *, *, #24083, .F. ) ;
#60595 = CARTESIAN_POINT ( 'NONE',  ( 4.884421565153296285, -10.53113076414237703, 8.448016786630551778 ) ) ;
#60597 = B_SPLINE_CURVE_WITH_KNOTS ( 'NONE', 3,
 ( #3906, #49139, #59414, #3598, #18211, #39449, #34131, #38479, #64709, #23864 ),
 .UNSPECIFIED., .F., .F.,
 ( 4, 2, 2, 2, 4 ),
 ( 1.163687884334659274E-17, 0.002301662762293088353, 0.004603325524586164563, 0.006904988286879240773, 0.009206651049172318718 ),
 .UNSPECIFIED. ) ;
#60598 = EDGE_CURVE ( 'NONE', #57759, #57723, #18233, .T. ) ;
#60599 = CARTESIAN_POINT ( 'NONE',  ( 36.00000000000000711, -12.08151691381187298, 4.074242145636130630 ) ) ;
#60600 = AXIS2_PLACEMENT_3D ( 'NONE', #43655, #22744, #43007 ) ;
#60601 = VERTEX_POINT ( 'NONE', #8631 ) ;
#60602 = CARTESIAN_POINT ( 'NONE',  ( 12.89830783111085566, -13.14232582968774388, -3.093048059426170227 ) ) ;
#60603 = VERTEX_POINT ( 'NONE', #3681 ) ;
#60604 = VERTEX_POINT ( 'NONE', #24912 ) ;
#60605 = DIRECTION ( 'NONE',  ( -1.000000000000000000, -0.000000000000000000, 0.000000000000000000 ) ) ;
#60606 = DIRECTION ( 'NONE',  ( 0.000000000000000000, 0.01356324068817991828, -0.9999080150203990547 ) ) ;
#60607 = CARTESIAN_POINT ( 'NONE',  ( -27.32337605527165891, -1.175835497774981198, -2.771816950947483704 ) ) ;
#60608 = CARTESIAN_POINT ( 'NONE',  ( -22.27706485742869091, 1.508175983031630585, -3.358064672837109743 ) ) ;
#60609 = FACE_OUTER_BOUND ( 'NONE', #45993, .T. ) ;
#60610 = AXIS2_PLACEMENT_3D ( 'NONE', #10411, #15076, #25386 ) ;
#60611 = AXIS2_PLACEMENT_3D ( 'NONE', #36237, #365, #35899 ) ;
#60612 = AXIS2_PLACEMENT_3D ( 'NONE', #49474, #7924, #38490 ) ;
#60613 = PLANE ( 'NONE',  #18389 ) ;
#60614 = AXIS2_PLACEMENT_3D ( 'NONE', #22493, #57415, #11845 ) ;
#60615 = ORIENTED_EDGE ( 'NONE', *, *, #61996, .T. ) ;
#60616 = CARTESIAN_POINT ( 'NONE',  ( -22.27384469013076185, 0.9835229356382479970, -3.548341908721023952 ) ) ;
#60617 = FACE_OUTER_BOUND ( 'NONE', #20867, .T. ) ;
#60618 = CARTESIAN_POINT ( 'NONE',  ( 0.8375941296789963797, 12.17542732751272183, 2.537217542321736463 ) ) ;
#60619 = ORIENTED_EDGE ( 'NONE', *, *, #48074, .T. ) ;
#60620 = VECTOR ( 'NONE', #12906, 1000.000000000000114 ) ;
#60621 = EDGE_CURVE ( 'NONE', #57809, #63687, #17124, .T. ) ;
#60622 = AXIS2_PLACEMENT_3D ( 'NONE', #18990, #4703, #45237 ) ;
#60623 = CARTESIAN_POINT ( 'NONE',  ( -35.00000000000000000, -3.511814412392038953, -11.66953048682403171 ) ) ;
#60624 = AXIS2_PLACEMENT_3D ( 'NONE', #8744, #63269, #64568 ) ;
#60625 = CARTESIAN_POINT ( 'NONE',  ( -10.82482511535300773, -8.491786248805359705, -10.49748912556531621 ) ) ;
#60626 = CARTESIAN_POINT ( 'NONE',  ( -37.50900221036945226, -2.222235401316478232, -21.66089349574501455 ) ) ;
#60627 = ORIENTED_EDGE ( 'NONE', *, *, #19973, .F. ) ;
#60628 = DIRECTION ( 'NONE',  ( 1.000000000000000000, -0.000000000000000000, 0.000000000000000000 ) ) ;
#60629 = FACE_OUTER_BOUND ( 'NONE', #17757, .T. ) ;
#60630 = CARTESIAN_POINT ( 'NONE',  ( -37.00000000000000711, -12.21925492305359562, -3.640372113593682624 ) ) ;
#60631 = AXIS2_PLACEMENT_3D ( 'NONE', #63139, #12925, #12576 ) ;
#60632 = EDGE_CURVE ( 'NONE', #8461, #40758, #3981, .T. ) ;
#60633 = CARTESIAN_POINT ( 'NONE',  ( 0.000000000000000000, -3.859771122243078167, 5.613913289150019637 ) ) ;
#60634 = CARTESIAN_POINT ( 'NONE',  ( 0.000000000000000000, 0.000000000000000000, 0.000000000000000000 ) ) ;
#60635 = AXIS2_PLACEMENT_3D ( 'NONE', #63854, #43921, #34892 ) ;
#60636 = ORIENTED_EDGE ( 'NONE', *, *, #26282, .T. ) ;
#60637 = EDGE_CURVE ( 'NONE', #59860, #23486, #7592, .T. ) ;
#60638 = CARTESIAN_POINT ( 'NONE',  ( 2.263328370261531219, 0.1420109704215806457, 7.640407877530307701 ) ) ;
#60639 = CARTESIAN_POINT ( 'NONE',  ( 3.145174248154654517, 4.348535253017615787, -11.19168307967391129 ) ) ;
#60640 = CARTESIAN_POINT ( 'NONE',  ( 37.00000000000000711, 4.705694406421931860E-17, -3.469127814946512892E-15 ) ) ;
#60641 = ORIENTED_EDGE ( 'NONE', *, *, #59913, .T. ) ;
#60642 = FACE_OUTER_BOUND ( 'NONE', #64516, .T. ) ;
#60643 = CIRCLE ( 'NONE', #12843, 12.18650000000000411 ) ;
#60644 = PLANE ( 'NONE',  #22428 ) ;
#60645 = ADVANCED_FACE ( 'NONE', ( #14896 ), #44510, .T. ) ;
#60646 = ORIENTED_EDGE ( 'NONE', *, *, #44775, .T. ) ;
#60647 = VERTEX_POINT ( 'NONE', #50520 ) ;
#60648 = ORIENTED_EDGE ( 'NONE', *, *, #1517, .T. ) ;
#60649 = CIRCLE ( 'NONE', #8691, 4.999999999999999112 ) ;
#60650 = CIRCLE ( 'NONE', #37296, 5.000000000000000888 ) ;
#60651 = CIRCLE ( 'NONE', #55334, 12.18649999999999878 ) ;
#60652 = ORIENTED_EDGE ( 'NONE', *, *, #1745, .F. ) ;
#60653 = CARTESIAN_POINT ( 'NONE',  ( -37.00000000000000711, 0.000000000000000000, 0.000000000000000000 ) ) ;
#60654 = CARTESIAN_POINT ( 'NONE',  ( 1.719304012340733934, -11.67935079956419031, -5.066286238786891438 ) ) ;
#60655 = CARTESIAN_POINT ( 'NONE',  ( 0.2911222467163532279, -6.312159098066242535, 10.50411792397755661 ) ) ;
#60656 = CARTESIAN_POINT ( 'NONE',  ( 0.2651627682582903267, 4.105539787731869339, -11.53745347823611667 ) ) ;
#60657 = DIRECTION ( 'NONE',  ( -1.000000000000000000, 0.000000000000000000, 0.000000000000000000 ) ) ;
#60658 = EDGE_CURVE ( 'NONE', #14915, #40547, #24576, .T. ) ;
#60660 = B_SPLINE_CURVE_WITH_KNOTS ( 'NONE', 3,
 ( #31438, #36073, #1532, #16790, #57049, #16146, #27110, #26129, #11470, #51737, #21120, #26443, #16484, #12130, #32076, #36753, #57368, #31746 ),
 .UNSPECIFIED., .F., .F.,
 ( 4, 2, 2, 2, 2, 2, 2, 2, 4 ),
 ( 0.000000000000000000, 0.0007405344560050070241, 0.001481068912010014048, 0.002221603368015021181, 0.002962137824020028096, 0.003702672280025034578, 0.004443206736030042361, 0.005183741192035048843, 0.005924275648040054458 ),
 .UNSPECIFIED. ) ;
#60659 = CARTESIAN_POINT ( 'NONE',  ( -11.91618201078742523, -29.31229682091932176, 6.386286639733019577 ) ) ;
#60661 = LINE ( 'NONE', #800, #48356 ) ;
#60663 = ORIENTED_EDGE ( 'NONE', *, *, #64156, .F. ) ;
#60662 = DIRECTION ( 'NONE',  ( 0.000000000000000000, -0.7196168960969868689, -0.6943713148249562872 ) ) ;
#60664 = DIRECTION ( 'NONE',  ( 0.000000000000000000, 0.01356324068817998940, -0.9999080150203990547 ) ) ;
#60665 = ADVANCED_FACE ( 'NONE', ( #19269 ), #24246, .T. ) ;
#60666 = ORIENTED_EDGE ( 'NONE', *, *, #62170, .T. ) ;
#60667 = DIRECTION ( 'NONE',  ( -1.000000000000000000, 0.000000000000000000, 0.000000000000000000 ) ) ;
#60668 = ORIENTED_EDGE ( 'NONE', *, *, #22969, .F. ) ;
#60669 = EDGE_LOOP ( 'NONE', ( #60315, #26834, #42992, #34151 ) ) ;
#60670 = CARTESIAN_POINT ( 'NONE',  ( 0.3053067050349255740, 9.538004819224459752, -7.702091166065907935 ) ) ;
#60671 = EDGE_CURVE ( 'NONE', #52324, #53488, #52233, .T. ) ;
#60672 = VECTOR ( 'NONE', #54724, 1000.000000000000000 ) ;
#60673 = CARTESIAN_POINT ( 'NONE',  ( 11.15801620995519805, -32.62087690404786144, 12.20531625113500596 ) ) ;
#60674 = CARTESIAN_POINT ( 'NONE',  ( 3.152665057734040488, 0.000000000000000000, 0.000000000000000000 ) ) ;
#60675 = CIRCLE ( 'NONE', #51148, 12.18650000000000055 ) ;
#60676 = CARTESIAN_POINT ( 'NONE',  ( 2.705197763288549773, 7.714317563576064352, -1.076142490489789605 ) ) ;
#60677 = FACE_OUTER_BOUND ( 'NONE', #39467, .T. ) ;
#60678 = CYLINDRICAL_SURFACE ( 'NONE', #158, 12.75000000000000178 ) ;
#60681 = ORIENTED_EDGE ( 'NONE', *, *, #35720, .T. ) ;
#60680 = ADVANCED_FACE ( 'NONE', ( #65765 ), #44203, .T. ) ;
#60679 = CIRCLE ( 'NONE', #52242, 12.18650000000000411 ) ;
#60682 = EDGE_LOOP ( 'NONE', ( #39141, #38852, #20991, #23295 ) ) ;
#60683 = DIRECTION ( 'NONE',  ( -0.9606638835031802159, -0.2674900627617609605, -0.07465901992590913416 ) ) ;
#60684 = ORIENTED_EDGE ( 'NONE', *, *, #29698, .F. ) ;
#60685 = AXIS2_PLACEMENT_3D ( 'NONE', #25752, #45047, #40042 ) ;
#60686 = EDGE_CURVE ( 'NONE', #49701, #7386, #47947, .T. ) ;
#60687 = ORIENTED_EDGE ( 'NONE', *, *, #27301, .F. ) ;
#60688 = TOROIDAL_SURFACE ( 'NONE', #52212, 20.19615242270663558, 3.000000000000000000 ) ;
#60689 = DIRECTION ( 'NONE',  ( -1.000000000000000000, 0.000000000000000000, 0.000000000000000000 ) ) ;
#60690 = DIRECTION ( 'NONE',  ( 1.000000000000000000, 0.000000000000000000, 0.000000000000000000 ) ) ;
#60691 = DIRECTION ( 'NONE',  ( -1.000000000000000000, 0.000000000000000000, 0.000000000000000000 ) ) ;
#60692 = CARTESIAN_POINT ( 'NONE',  ( 17.87656210312829330, -6.543550415627087169, 10.06239431139154306 ) ) ;
#60693 = DIRECTION ( 'NONE',  ( -1.000000000000000000, 0.000000000000000000, 0.000000000000000000 ) ) ;
#60694 = CARTESIAN_POINT ( 'NONE',  ( 2.665405856346778624, -9.304623509366210854, -2.226920474533478078 ) ) ;
#60695 = CARTESIAN_POINT ( 'NONE',  ( -27.05874794189610455, 1.734723475976807094E-15, -8.673617379884035472E-15 ) ) ;
#60696 = AXIS2_PLACEMENT_3D ( 'NONE', #19560, #14528, #28222 ) ;
#60697 = EDGE_LOOP ( 'NONE', ( #31328, #29564, #43895, #38853 ) ) ;
#60698 = ORIENTED_EDGE ( 'NONE', *, *, #19755, .F. ) ;
#60699 = CIRCLE ( 'NONE', #26707, 4.000000000000000000 ) ;
#60700 = CIRCLE ( 'NONE', #49043, 12.18650000000000411 ) ;
#60701 = CARTESIAN_POINT ( 'NONE',  ( 10.48620311856346454, 8.250315036047107142, -10.68561190601526789 ) ) ;
#60702 = CARTESIAN_POINT ( 'NONE',  ( 0.000000000000000000, 3.859771122243123465, -5.613913289150012531 ) ) ;
#60703 = LINE ( 'NONE', #47621, #58560 ) ;
#60704 = ADVANCED_FACE ( 'NONE', ( #29880 ), #50192, .T. ) ;
#60705 = AXIS2_PLACEMENT_3D ( 'NONE', #27303, #12339, #32604 ) ;
#60706 = CARTESIAN_POINT ( 'NONE',  ( 35.00000000000000000, 7.474872387601131152, 9.060822531525964507 ) ) ;
#60707 = AXIS2_PLACEMENT_3D ( 'NONE', #40018, #54989, #59665 ) ;
#60708 = CARTESIAN_POINT ( 'NONE',  ( 2.941278708680199916, 5.383216837018982126, -2.952340773940052898 ) ) ;
#60709 = FACE_OUTER_BOUND ( 'NONE', #38248, .T. ) ;
#60710 = CYLINDRICAL_SURFACE ( 'NONE', #42830, 13.50000000000000178 ) ;
#60711 = CARTESIAN_POINT ( 'NONE',  ( -27.08416813689867908, -2.150738950797701499, -0.7899859999124564380 ) ) ;
#60712 = ORIENTED_EDGE ( 'NONE', *, *, #14998, .F. ) ;
#60713 = DIRECTION ( 'NONE',  ( 1.000000000000000000, 0.000000000000000000, 0.000000000000000000 ) ) ;
#60714 = B_SPLINE_CURVE_WITH_KNOTS ( 'NONE', 3,
 ( #15552, #30835, #54829, #613, #5610, #35813, #56115, #41143, #10555, #34833, #65114, #50502, #34530 ),
 .UNSPECIFIED., .F., .F.,
 ( 4, 3, 3, 3, 4 ),
 ( 3.035766082959412415E-18, 6.607593386745472762E-05, 0.0001321518677373527319, 0.0001982171734706220795, 0.0002642860854759487171 ),
 .UNSPECIFIED. ) ;
#60715 = EDGE_CURVE ( 'NONE', #12171, #52971, #19270, .T. ) ;
#60716 = CARTESIAN_POINT ( 'NONE',  ( 0.000000000000000000, -0.3246585432986597852, 6.805031400696099020 ) ) ;
#60717 = EDGE_CURVE ( 'NONE', #45739, #33077, #58597, .T. ) ;
#60718 = AXIS2_PLACEMENT_3D ( 'NONE', #4464, #40329, #54681 ) ;
#60719 = DIRECTION ( 'NONE',  ( 1.000000000000000000, -0.000000000000000000, 0.000000000000000000 ) ) ;
#60720 = CARTESIAN_POINT ( 'NONE',  ( 0.3675815128205894289, 10.50067073900660652, -6.367184624550055183 ) ) ;
#60721 = ORIENTED_EDGE ( 'NONE', *, *, #30960, .F. ) ;
#60722 = CARTESIAN_POINT ( 'NONE',  ( 2.241352910868908310, 7.633946224498473931, 0.08337961031706864201 ) ) ;
#60723 = FACE_OUTER_BOUND ( 'NONE', #7464, .T. ) ;
#60724 = CARTESIAN_POINT ( 'NONE',  ( 17.91771366450749525, -28.72671386922736758, -8.232269603669239544 ) ) ;
#60725 = ORIENTED_EDGE ( 'NONE', *, *, #5435, .F. ) ;
#60726 = DIRECTION ( 'NONE',  ( -1.000000000000000000, 0.000000000000000000, -0.000000000000000000 ) ) ;
#60727 = CARTESIAN_POINT ( 'NONE',  ( 35.00000000000000000, 12.02534193257720574, -4.237174932027271801 ) ) ;
#60728 = CARTESIAN_POINT ( 'NONE',  ( -22.28694879868232803, -1.011812214896728346, -3.570244315741557983 ) ) ;
#60729 = EDGE_CURVE ( 'NONE', #23899, #11586, #31524, .T. ) ;
#60730 = CIRCLE ( 'NONE', #32049, 12.18650000000000055 ) ;
#60732 = ORIENTED_EDGE ( 'NONE', *, *, #43881, .T. ) ;
#60731 = CYLINDRICAL_SURFACE ( 'NONE', #27533, 5.000000000000000888 ) ;
#60733 = CARTESIAN_POINT ( 'NONE',  ( -27.09229696323320979, 2.247106967994373594, 0.5586335684093640674 ) ) ;
#60734 = CARTESIAN_POINT ( 'NONE',  ( 0.2646305136544072623, 9.465888453933068547, -7.770320294339081890 ) ) ;
#60735 = VERTEX_POINT ( 'NONE', #15249 ) ;
#60736 = CIRCLE ( 'NONE', #40565, 4.999999999999999112 ) ;
#60737 = CARTESIAN_POINT ( 'NONE',  ( -9.327891528110853869, 11.85922960855886821, -6.460470496795954531 ) ) ;
#60738 = DIRECTION ( 'NONE',  ( 1.000000000000000000, 0.000000000000000000, 0.000000000000000000 ) ) ;
#60739 = DIRECTION ( 'NONE',  ( 0.000000000000000000, -0.3554799084909036067, -0.9346839223284515441 ) ) ;
#60740 = CARTESIAN_POINT ( 'NONE',  ( 0.3002738374340830907, -11.43949898053768166, -4.403689978763186019 ) ) ;
#60741 = CARTESIAN_POINT ( 'NONE',  ( 2.241451721903216843, 2.668222118333546611, -7.153019588493043202 ) ) ;
#60742 = FACE_OUTER_BOUND ( 'NONE', #34959, .T. ) ;
#60743 = ORIENTED_EDGE ( 'NONE', *, *, #5380, .F. ) ;
#60744 = CARTESIAN_POINT ( 'NONE',  ( 35.00000000000000000, -11.66953048682396954, 3.511814412392239682 ) ) ;
#60745 = ORIENTED_EDGE ( 'NONE', *, *, #53079, .T. ) ;
#60746 = CIRCLE ( 'NONE', #10855, 12.74999999999999822 ) ;
#60747 =( LENGTH_UNIT ( ) NAMED_UNIT ( * ) SI_UNIT ( .MILLI., .METRE. ) );
#60748 = EDGE_CURVE ( 'NONE', #31515, #64802, #44988, .T. ) ;
#60750 = CARTESIAN_POINT ( 'NONE',  ( 0.3053067050349130840, 11.43920902168906828, 4.409108891833689370 ) ) ;
#60749 = AXIS2_PLACEMENT_3D ( 'NONE', #53040, #27122, #63651 ) ;
#60751 = CIRCLE ( 'NONE', #52129, 12.75000000000000178 ) ;
#60752 = CIRCLE ( 'NONE', #20401, 5.000000000000001776 ) ;
#60753 = ADVANCED_FACE ( 'NONE', ( #25899 ), #52154, .T. ) ;
#60754 = CARTESIAN_POINT ( 'NONE',  ( 41.00000000000000711, -1.694065894508600678E-18, 0.000000000000000000 ) ) ;
#60755 = ORIENTED_EDGE ( 'NONE', *, *, #12459, .F. ) ;
#60756 = CARTESIAN_POINT ( 'NONE',  ( 2.000000000000001776, 0.000000000000000000, 0.000000000000000000 ) ) ;
#60757 = DIRECTION ( 'NONE',  ( 0.000000000000000000, 0.4698238015817365332, 0.8827602140260315533 ) ) ;
#60758 = CARTESIAN_POINT ( 'NONE',  ( -22.27720412283625961, -1.161733799004162293, 3.493592264983210516 ) ) ;
#60759 = EDGE_LOOP ( 'NONE', ( #16657, #42257, #47119, #36385 ) ) ;
#60760 = VERTEX_POINT ( 'NONE', #45847 ) ;
#60761 = ADVANCED_FACE ( 'NONE', ( #15568 ), #1289, .T. ) ;
#60762 = CARTESIAN_POINT ( 'NONE',  ( 2.373367633546870969, 0.1808255748566540144, -7.676289145832772221 ) ) ;
#60763 = VERTEX_POINT ( 'NONE', #16576 ) ;
#60764 = CARTESIAN_POINT ( 'NONE',  ( 5.515188684475870851, 0.002983184900674853111, -0.004442604682416488940 ) ) ;
#60765 = CARTESIAN_POINT ( 'NONE',  ( -27.08639648637141661, 0.5801562253478033115, -2.223359598374795354 ) ) ;
#60766 = AXIS2_PLACEMENT_3D ( 'NONE', #40798, #878, #34788 ) ;
#60767 = DIRECTION ( 'NONE',  ( 1.000000000000000000, 0.000000000000000000, 0.000000000000000000 ) ) ;
#60768 = LINE ( 'NONE', #55112, #13542 ) ;
#60769 = AXIS2_PLACEMENT_3D ( 'NONE', #54917, #35921, #40264 ) ;
#60770 = CARTESIAN_POINT ( 'NONE',  ( 35.00000000000000000, 12.08216339958902630, 1.591260454995109930 ) ) ;
#60771 = CARTESIAN_POINT ( 'NONE',  ( -35.00000000000000000, -7.561043153947899498, -9.557269938331636183 ) ) ;
#60772 = CARTESIAN_POINT ( 'NONE',  ( -22.59969328935897792, -1.672297795814008392, -4.339503524536198142 ) ) ;
#60773 = ORIENTED_EDGE ( 'NONE', *, *, #21816, .F. ) ;
#60774 = CARTESIAN_POINT ( 'NONE',  ( 2.255723233588951437, -1.456523090672661613, 7.499053486174015681 ) ) ;
#60775 = CIRCLE ( 'NONE', #8766, 7.938172270156617749 ) ;
#60776 = CARTESIAN_POINT ( 'NONE',  ( 21.94281256157706750, 11.68886982501328475, -2.741018260906308068 ) ) ;
#60777 = CARTESIAN_POINT ( 'NONE',  ( 9.772170780982303739, 13.45371974242435442, -1.117788476161230227 ) ) ;
#60778 = PLANE ( 'NONE',  #46706 ) ;
#60779 = CARTESIAN_POINT ( 'NONE',  ( 37.00000000000000711, 8.017674001891784030, -9.913596905230145140 ) ) ;
#60780 = DIRECTION ( 'NONE',  ( 0.000000000000000000, 0.2960891610144441022, 0.9551603052523501836 ) ) ;
#60781 = FACE_OUTER_BOUND ( 'NONE', #28125, .T. ) ;
#60782 = EDGE_CURVE ( 'NONE', #21703, #54954, #5470, .T. ) ;
#60783 = VERTEX_POINT ( 'NONE', #30857 ) ;
#60784 = CARTESIAN_POINT ( 'NONE',  ( 35.00000000000000000, 11.80185301892980299, -4.824807283154166626 ) ) ;
#60785 = AXIS2_PLACEMENT_3D ( 'NONE', #27819, #47459, #53089 ) ;
#60786 = EDGE_CURVE ( 'NONE', #6776, #40631, #56429, .T. ) ;
#60787 =( BOUNDED_SURFACE ( )  B_SPLINE_SURFACE ( 3, 1, ( 
 ( #21725, #27029 ),
 ( #1768, #17038 ),
 ( #42281, #16402 ),
 ( #57955, #61597 ) ),
 .UNSPECIFIED., .F., .F., .F. ) 
 B_SPLINE_SURFACE_WITH_KNOTS ( ( 4, 4 ),
 ( 2, 2 ),
 ( 0.000000000000000000, 1.000000000000000000 ),
 ( 0.000000000000000000, 1.000000000000000000 ),
 .UNSPECIFIED. ) 
 GEOMETRIC_REPRESENTATION_ITEM ( )  RATIONAL_B_SPLINE_SURFACE ( (
 ( 1.000000000000000000, 1.000000000000000000),
 ( 0.9856612449720755231, 0.9999558406602322425),
 ( 0.9856612449720755231, 0.9999558406602322425),
 ( 1.000000000000000000, 1.000000000000000000) ) ) 
 REPRESENTATION_ITEM ( '' )  SURFACE ( )  );
#60788 = VERTEX_POINT ( 'NONE', #36843 ) ;
#60789 = FACE_OUTER_BOUND ( 'NONE', #53727, .T. ) ;
#60790 = DIRECTION ( 'NONE',  ( 1.000000000000000000, -0.000000000000000000, -0.000000000000000000 ) ) ;
#60791 = CARTESIAN_POINT ( 'NONE',  ( -17.29753452029093097, 7.115740787999835781, -11.47405852577958107 ) ) ;
#60792 = CARTESIAN_POINT ( 'NONE',  ( 3.152665057735899001, -7.886634106564667235, -0.9030954876721221103 ) ) ;
#60793 = CARTESIAN_POINT ( 'NONE',  ( -37.00000000000000711, -10.43555801961479190, 5.391785509270926369 ) ) ;
#60794 = ORIENTED_EDGE ( 'NONE', *, *, #55031, .T. ) ;
#60795 = DIRECTION ( 'NONE',  ( 1.000000000000000000, 0.000000000000000000, 0.000000000000000000 ) ) ;
#60796 = DIRECTION ( 'NONE',  ( -1.000000000000000000, 0.000000000000000000, 0.000000000000000000 ) ) ;
#60797 = ADVANCED_FACE ( 'NONE', ( #21893 ), #40859, .T. ) ;
#60798 = AXIS2_PLACEMENT_3D ( 'NONE', #12314, #31934, #8016 ) ;
#60799 = DIRECTION ( 'NONE',  ( 0.000000000000000000, 0.01356324068817992175, -0.9999080150203990547 ) ) ;
#60800 = CARTESIAN_POINT ( 'NONE',  ( 0.3675815128205894289, -7.689697408877338880, 9.574637318041938627 ) ) ;
#60801 = AXIS2_PLACEMENT_3D ( 'NONE', #28902, #43523, #29234 ) ;
#60802 = CARTESIAN_POINT ( 'NONE',  ( 9.773978258136098773, 6.946402228990928407, -11.57921718125522581 ) ) ;
#60803 = CARTESIAN_POINT ( 'NONE',  ( -27.20102706715913143, 1.765193291701727896, -1.966718264078090250 ) ) ;
#60804 = ORIENTED_EDGE ( 'NONE', *, *, #57073, .T. ) ;
#60805 = CARTESIAN_POINT ( 'NONE',  ( 5.536195898058073439, 0.004468797463753785421, 0.007230647766619707588 ) ) ;
#60806 = VERTEX_POINT ( 'NONE', #10576 ) ;
#60807 = FACE_OUTER_BOUND ( 'NONE', #16601, .T. ) ;
#60808 = DIRECTION ( 'NONE',  ( -1.000000000000000000, 0.000000000000000000, 0.000000000000000000 ) ) ;
#60809 = EDGE_CURVE ( 'NONE', #8001, #1325, #26730, .T. ) ;
#60810 = CARTESIAN_POINT ( 'NONE',  ( 29.12753374973488363, -5.698473394425191074, 10.60092621982456862 ) ) ;
#60811 = EDGE_CURVE ( 'NONE', #9981, #8357, #3255, .T. ) ;
#60812 = DIRECTION ( 'NONE',  ( -1.000000000000000000, 0.000000000000000000, 0.000000000000000000 ) ) ;
#60813 = CIRCLE ( 'NONE', #54468, 5.000000000000001776 ) ;
#60814 = VERTEX_POINT ( 'NONE', #37500 ) ;
#60815 = EDGE_LOOP ( 'NONE', ( #62271, #40286, #30015, #637 ) ) ;
#60816 = CARTESIAN_POINT ( 'NONE',  ( 22.57855258442564761, -4.427776684447072952, 25.00000000000000000 ) ) ;
#60817 = EDGE_LOOP ( 'NONE', ( #54864, #10882, #57336, #3605 ) ) ;
#60818 = CARTESIAN_POINT ( 'NONE',  ( 2.262775599886255762, -6.546038779272016050, -3.942403752832075892 ) ) ;
#60820 = VECTOR ( 'NONE', #60571, 1000.000000000000000 ) ;
#60819 = CARTESIAN_POINT ( 'NONE',  ( 0.2646305136544065406, -0.1321451301297000003, -12.24595685781654630 ) ) ;
#60821 = CYLINDRICAL_SURFACE ( 'NONE', #46894, 4.999999999999999112 ) ;
#60822 = DIRECTION ( 'NONE',  ( 1.000000000000000000, 0.000000000000000000, 0.000000000000000000 ) ) ;
#60823 = AXIS2_PLACEMENT_3D ( 'NONE', #48105, #2563, #8179 ) ;
#60824 = CARTESIAN_POINT ( 'NONE',  ( 0.9296196016852261712, 10.99907063288950049, -5.870433615766662783 ) ) ;
#60825 = DIRECTION ( 'NONE',  ( -1.000000000000000000, 0.000000000000000000, 0.000000000000000000 ) ) ;
#60826 = ORIENTED_EDGE ( 'NONE', *, *, #37307, .T. ) ;
#60827 = CARTESIAN_POINT ( 'NONE',  ( 0.000000000000000000, 0.000000000000000000, 0.000000000000000000 ) ) ;
#60828 = ORIENTED_EDGE ( 'NONE', *, *, #1831, .F. ) ;
#60829 = CARTESIAN_POINT ( 'NONE',  ( 37.00000000000000711, 10.25474254703961918, 6.584150480049438592 ) ) ;
#60830 = ADVANCED_FACE ( 'NONE', ( #57470 ), #16889, .T. ) ;
#60831 = FACE_OUTER_BOUND ( 'NONE', #29201, .T. ) ;
#60832 = ORIENTED_EDGE ( 'NONE', *, *, #20847, .T. ) ;
#60833 = ADVANCED_FACE ( 'NONE', ( #27511 ), #8632, .T. ) ;
#60834 = FACE_BOUND ( 'NONE', #12808, .T. ) ;
#60835 = EDGE_LOOP ( 'NONE', ( #8108, #4251, #52883, #16211 ) ) ;
#60836 = CARTESIAN_POINT ( 'NONE',  ( -37.00000000000000711, 9.506317355798371338, 8.496612874013196759 ) ) ;
#60837 = DIRECTION ( 'NONE',  ( 1.000000000000000000, 0.000000000000000000, 0.000000000000000000 ) ) ;
#60838 = LINE ( 'NONE', #26247, #28646 ) ;
#60839 = LINE ( 'NONE', #55853, #53701 ) ;
#60840 = ORIENTED_EDGE ( 'NONE', *, *, #58103, .F. ) ;
#60841 = ORIENTED_EDGE ( 'NONE', *, *, #62318, .T. ) ;
#60842 = CARTESIAN_POINT ( 'NONE',  ( 2.406456491625819094, 2.970787154401585806, -10.00134798414976345 ) ) ;
#60843 = ORIENTED_EDGE ( 'NONE', *, *, #56534, .F. ) ;
#60844 = CARTESIAN_POINT ( 'NONE',  ( 2.000000000000001776, -6.253963800348261159, 4.139799123620986343 ) ) ;
#60845 = ORIENTED_EDGE ( 'NONE', *, *, #60871, .T. ) ;
#60846 = CIRCLE ( 'NONE', #47086, 12.18650000000000055 ) ;
#60847 = B_SPLINE_CURVE_WITH_KNOTS ( 'NONE', 3,
 ( #5777, #46325, #31348, #40667, #6409, #46978, #46640, #55965, #60964, #41646, #25710, #21026, #20722, #15398, #41309, #61589, #16036, #35668, #36330 ),
 .UNSPECIFIED., .F., .F.,
 ( 4, 3, 3, 3, 3, 3, 4 ),
 ( 0.000000000000000000, 2.836829843012736788E-05, 4.224792512551080192E-05, 5.612066614913364178E-05, 6.998859278355053920E-05, 9.832141288087331251E-05, 0.0001178161482478538510 ),
 .UNSPECIFIED. ) ;
#60848 = AXIS2_PLACEMENT_3D ( 'NONE', #4583, #39810, #51457 ) ;
#60849 = ORIENTED_EDGE ( 'NONE', *, *, #40224, .T. ) ;
#60850 = VERTEX_POINT ( 'NONE', #37831 ) ;
#60851 = CARTESIAN_POINT ( 'NONE',  ( 2.844750968615358033, -5.783165144077080377, 5.286885609674477848 ) ) ;
#60852 = CARTESIAN_POINT ( 'NONE',  ( -14.88966238093840921, -27.95127710492162265, 11.23339344092909897 ) ) ;
#60853 = AXIS2_PLACEMENT_3D ( 'NONE', #62741, #52476, #36153 ) ;
#60854 = CIRCLE ( 'NONE', #1438, 5.000000000000000000 ) ;
#60855 = DIRECTION ( 'NONE',  ( 1.000000000000000000, 0.000000000000000000, 0.000000000000000000 ) ) ;
#60856 = CARTESIAN_POINT ( 'NONE',  ( -37.00000000000000711, 0.000000000000000000, 0.000000000000000000 ) ) ;
#60857 = CARTESIAN_POINT ( 'NONE',  ( -22.31328051695926007, -2.748895659348118858, -2.608921479762132734 ) ) ;
#60858 = ORIENTED_EDGE ( 'NONE', *, *, #2552, .T. ) ;
#60859 = DIRECTION ( 'NONE',  ( 1.000000000000000000, 0.000000000000000000, 0.000000000000000000 ) ) ;
#60860 = ORIENTED_EDGE ( 'NONE', *, *, #28150, .T. ) ;
#60861 = DIRECTION ( 'NONE',  ( 1.000000000000000000, -0.000000000000000000, -0.000000000000000000 ) ) ;
#60863 = CARTESIAN_POINT ( 'NONE',  ( -27.08588607604432852, 0.6046196991083065964, 2.215240480751981877 ) ) ;
#60862 = CIRCLE ( 'NONE', #13106, 5.000000000000001776 ) ;
#60864 = VERTEX_POINT ( 'NONE', #37158 ) ;
#60865 = CARTESIAN_POINT ( 'NONE',  ( -27.23368049396187374, 11.01758315594069870, -7.819524286938179358 ) ) ;
#60866 = VECTOR ( 'NONE', #36246, 1000.000000000000000 ) ;
#60867 = CARTESIAN_POINT ( 'NONE',  ( 29.16097531476821203, 8.613045793590645260, 8.368184035611974991 ) ) ;
#60868 = DIRECTION ( 'NONE',  ( 0.6442147435043042991, 0.000000000000000000, 0.7648446667472313942 ) ) ;
#60869 = VERTEX_POINT ( 'NONE', #63733 ) ;
#60870 = CARTESIAN_POINT ( 'NONE',  ( -35.00000000000000000, 7.971186206369601734, -9.217970097227642157 ) ) ;
#60871 = EDGE_CURVE ( 'NONE', #56061, #60283, #5042, .T. ) ;
#60872 = ORIENTED_EDGE ( 'NONE', *, *, #16302, .F. ) ;
#60873 = CARTESIAN_POINT ( 'NONE',  ( 0.2834382757447994061, 10.71064820518743055, 5.949714385480675993 ) ) ;
#60874 = CARTESIAN_POINT ( 'NONE',  ( -18.78786164167387085, -13.48564496196971874, -0.7125357888566099529 ) ) ;
#60875 = AXIS2_PLACEMENT_3D ( 'NONE', #2395, #63216, #12016 ) ;
#60876 = CARTESIAN_POINT ( 'NONE',  ( -7.961359079021516294, -27.27258404549932536, 15.08967732372090964 ) ) ;
#60877 = CARTESIAN_POINT ( 'NONE',  ( 2.298277635560095344, -3.682855706290095732, -6.709004959608344976 ) ) ;
#60878 = CARTESIAN_POINT ( 'NONE',  ( -35.04709527796842394, -0.007095259204982495849, 0.01012471662512753889 ) ) ;
#60879 = ORIENTED_EDGE ( 'NONE', *, *, #19694, .F. ) ;
#60880 = CYLINDRICAL_SURFACE ( 'NONE', #53651, 4.999999999999999112 ) ;
#60881 = DIRECTION ( 'NONE',  ( -1.000000000000000000, 0.000000000000000000, 0.000000000000000000 ) ) ;
#60882 = CARTESIAN_POINT ( 'NONE',  ( 1.948354844648095607, -2.783443994770122387, -11.63671644762040458 ) ) ;
#60883 = DIRECTION ( 'NONE',  ( -1.000000000000000000, 0.000000000000000000, -0.000000000000000000 ) ) ;
#60884 = ADVANCED_FACE ( 'NONE', ( #28498 ), #12538, .T. ) ;
#60885 = AXIS2_PLACEMENT_3D ( 'NONE', #39429, #29769, #14475 ) ;
#60886 = B_SPLINE_CURVE_WITH_KNOTS ( 'NONE', 3,
 ( #51418, #201, #61045, #41390, #15477, #35740 ),
 .UNSPECIFIED., .F., .F.,
 ( 4, 2, 4 ),
 ( 0.0001654224980408524042, 0.0006219428995476594538, 0.001078463301054466503 ),
 .UNSPECIFIED. ) ;
#60887 = CARTESIAN_POINT ( 'NONE',  ( 0.3057689695767448201, 12.25749431726083394, -0.2309407641933178545 ) ) ;
#60888 = CARTESIAN_POINT ( 'NONE',  ( -22.30625920655495165, 0.2529928606556913206, 3.783486345733959588 ) ) ;
#60890 = EDGE_CURVE ( 'NONE', #2445, #35323, #60649, .T. ) ;
#60889 = CARTESIAN_POINT ( 'NONE',  ( 2.288423627607476973, -5.962686897379168904, -4.792733268640440691 ) ) ;
#60891 = DIRECTION ( 'NONE',  ( 1.000000000000000000, 0.000000000000000000, 0.000000000000000000 ) ) ;
#60892 = CARTESIAN_POINT ( 'NONE',  ( -37.00000000000000711, 9.621072037177118119, -8.366449238204259231 ) ) ;
#60893 = CIRCLE ( 'NONE', #1483, 7.499999999999988454 ) ;
#60894 = VECTOR ( 'NONE', #3794, 1000.000000000000000 ) ;
#60895 = EDGE_CURVE ( 'NONE', #53953, #60970, #50126, .T. ) ;
#60896 = VECTOR ( 'NONE', #36339, 1000.000000000000000 ) ;
#60897 = ORIENTED_EDGE ( 'NONE', *, *, #27487, .F. ) ;
#60898 = ORIENTED_EDGE ( 'NONE', *, *, #47465, .F. ) ;
#60899 = CARTESIAN_POINT ( 'NONE',  ( -41.00000000000000711, 5.493969937218003549E-16, -4.500000000000000888 ) ) ;
#60900 = FACE_OUTER_BOUND ( 'NONE', #17869, .T. ) ;
#60901 = LINE ( 'NONE', #15975, #15128 ) ;
#60902 = AXIS2_PLACEMENT_3D ( 'NONE', #17622, #21945, #16947 ) ;
#60903 = DIRECTION ( 'NONE',  ( -1.000000000000000000, 0.000000000000000000, 0.000000000000000000 ) ) ;
#60904 = EDGE_LOOP ( 'NONE', ( #15729, #12220, #51158, #19915 ) ) ;
#60905 = CIRCLE ( 'NONE', #32228, 12.75000000000000178 ) ;
#60906 = VERTEX_POINT ( 'NONE', #18214 ) ;
#60907 = ORIENTED_EDGE ( 'NONE', *, *, #63059, .F. ) ;
#60908 = CARTESIAN_POINT ( 'NONE',  ( 0.2638984909335716500, 8.023974293733301622, -9.252728947330998821 ) ) ;
#60909 = EDGE_CURVE ( 'NONE', #32398, #9122, #13990, .T. ) ;
#60910 = VECTOR ( 'NONE', #5137, 1000.000000000000000 ) ;
#60911 = CARTESIAN_POINT ( 'NONE',  ( -22.27706485742869091, 0.9221835209182547288, 3.563814065926663499 ) ) ;
#60912 = EDGE_LOOP ( 'NONE', ( #36845, #7754, #65073, #26417 ) ) ;
#60913 = DIRECTION ( 'NONE',  ( -1.000000000000000000, 0.000000000000000000, 0.000000000000000000 ) ) ;
#60914 = CARTESIAN_POINT ( 'NONE',  ( 35.00000000000000000, 4.705694406421931860E-17, -3.469127814946512892E-15 ) ) ;
#60915 = CARTESIAN_POINT ( 'NONE',  ( 2.350038591458109227, -10.55267716396077482, 1.210550722320991701 ) ) ;
#60916 = ORIENTED_EDGE ( 'NONE', *, *, #29237, .F. ) ;
#60917 = CIRCLE ( 'NONE', #408, 7.499999999999988454 ) ;
#60918 = CARTESIAN_POINT ( 'NONE',  ( -27.08426571771018487, -0.2528330215897320321, -2.277536580310470793 ) ) ;
#60919 = CIRCLE ( 'NONE', #20526, 4.999999999999999112 ) ;
#60920 = CARTESIAN_POINT ( 'NONE',  ( 4.972137933589803716, -28.45452681573965137, -13.21946257706011174 ) ) ;
#60921 = DIRECTION ( 'NONE',  ( 1.000000000000000000, 0.000000000000000000, 0.000000000000000000 ) ) ;
#60922 = ORIENTED_EDGE ( 'NONE', *, *, #43203, .T. ) ;
#60923 = CARTESIAN_POINT ( 'NONE',  ( -37.00000000000000711, 0.000000000000000000, 0.000000000000000000 ) ) ;
#60924 = ORIENTED_EDGE ( 'NONE', *, *, #64368, .T. ) ;
#60925 = DIRECTION ( 'NONE',  ( -0.3939253465568944290, 0.7910971609033267127, -0.4679616473074760807 ) ) ;
#60926 = ORIENTED_EDGE ( 'NONE', *, *, #45220, .T. ) ;
#60927 = DIRECTION ( 'NONE',  ( 0.000000000000000000, -0.01356324068817998940, 0.9999080150203990547 ) ) ;
#60928 = CARTESIAN_POINT ( 'NONE',  ( 5.514624014163232779, 0.003498325728817963057, 0.002216125254993220762 ) ) ;
#60929 = FACE_OUTER_BOUND ( 'NONE', #40903, .T. ) ;
#60930 = EDGE_CURVE ( 'NONE', #23499, #51119, #63111, .T. ) ;
#60931 = DIRECTION ( 'NONE',  ( -1.000000000000000000, 0.000000000000000000, 0.000000000000000000 ) ) ;
#60932 = CARTESIAN_POINT ( 'NONE',  ( 2.000000000000001776, -2.469490258309472441, 6.482025155313308140 ) ) ;
#60933 = CARTESIAN_POINT ( 'NONE',  ( 11.12599276166011464, 0.3473812333126252150, 11.99566059042195754 ) ) ;
#60934 = DIRECTION ( 'NONE',  ( 1.000000000000000000, 0.000000000000000000, 0.000000000000000000 ) ) ;
#60935 = CARTESIAN_POINT ( 'NONE',  ( 0.3278977287071186963, -3.961557589215535913, -11.60975784853196657 ) ) ;
#60937 = ORIENTED_EDGE ( 'NONE', *, *, #6714, .F. ) ;
#60936 = CARTESIAN_POINT ( 'NONE',  ( 47.00000000000000711, 4.705694406421931860E-17, -3.469127814946512892E-15 ) ) ;
#60938 = DIRECTION ( 'NONE',  ( 0.000000000000000000, -0.2006870767258961963, 0.9796553971857727694 ) ) ;
#60939 = VERTEX_POINT ( 'NONE', #54452 ) ;
#60940 = DIRECTION ( 'NONE',  ( 0.000000000000000000, 0.3807014730195219521, -0.9246979985058723095 ) ) ;
#60941 = VERTEX_POINT ( 'NONE', #19840 ) ;
#60942 = CARTESIAN_POINT ( 'NONE',  ( 37.00000000000000711, 4.309077947445811851, 10.92721691015450780 ) ) ;
#60943 = CIRCLE ( 'NONE', #15266, 2.899999999999994582 ) ;
#60944 = ORIENTED_EDGE ( 'NONE', *, *, #57455, .T. ) ;
#60946 = AXIS2_PLACEMENT_3D ( 'NONE', #5625, #50188, #65130 ) ;
#60945 = CARTESIAN_POINT ( 'NONE',  ( 1.104777566491143892, -12.51694124543052311, 0.4777483965053294646 ) ) ;
#60947 = CARTESIAN_POINT ( 'NONE',  ( 5.514970785353741078, -0.002093325033904051488, -0.004233694591582509194 ) ) ;
#60948 = CYLINDRICAL_SURFACE ( 'NONE', #6826, 12.75000000000000178 ) ;
#60949 = DIRECTION ( 'NONE',  ( -1.000000000000000000, 0.000000000000000000, 0.000000000000000000 ) ) ;
#60950 = AXIS2_PLACEMENT_3D ( 'NONE', #44275, #30946, #1368 ) ;
#60951 = CARTESIAN_POINT ( 'NONE',  ( 3.152665057734040488, 0.000000000000000000, 0.000000000000000000 ) ) ;
#60952 = EDGE_LOOP ( 'NONE', ( #14833, #14441, #26262, #30610 ) ) ;
#60953 = DIRECTION ( 'NONE',  ( -0.9015184547431841500, -0.4327406564646559262, 0.000000000000000000 ) ) ;
#60954 = EDGE_CURVE ( 'NONE', #48650, #60581, #49050, .T. ) ;
#60955 = CIRCLE ( 'NONE', #15277, 12.75000000000000178 ) ;
#60956 = VERTEX_POINT ( 'NONE', #40100 ) ;
#60957 = CARTESIAN_POINT ( 'NONE',  ( 3.152665057735546839, 0.4801242025606423658, 7.923639299008859105 ) ) ;
#60958 = AXIS2_PLACEMENT_3D ( 'NONE', #47468, #2587, #17850 ) ;
#60959 = DIRECTION ( 'NONE',  ( -1.000000000000000000, 0.000000000000000000, 0.000000000000000000 ) ) ;
#60960 = EDGE_CURVE ( 'NONE', #21860, #27364, #9757, .T. ) ;
#60961 = CARTESIAN_POINT ( 'NONE',  ( -29.92777678363736626, -3.750539801530011985, -12.96855624952674724 ) ) ;
#60962 = EDGE_LOOP ( 'NONE', ( #28557, #10109, #28126, #53156 ) ) ;
#60963 = CIRCLE ( 'NONE', #6810, 5.000000000000000888 ) ;
#60964 = CARTESIAN_POINT ( 'NONE',  ( -27.09252613521593389, -1.005681546875654364, 2.086468883257830420 ) ) ;
#60965 = CIRCLE ( 'NONE', #53570, 12.18650000000000055 ) ;
#60966 = EDGE_CURVE ( 'NONE', #25175, #24785, #25675, .T. ) ;
#60967 = CARTESIAN_POINT ( 'NONE',  ( 41.49302228377221979, -1.586477970524126313, 18.85982933713411569 ) ) ;
#60968 = CARTESIAN_POINT ( 'NONE',  ( -4.975205859172449507, -1.416020129149132778, 13.42553116244733680 ) ) ;
#60969 = CARTESIAN_POINT ( 'NONE',  ( 0.2676618633000466541, -5.983781707237532110, -10.68562420805848490 ) ) ;
#60970 = VERTEX_POINT ( 'NONE', #44766 ) ;
#60971 = CARTESIAN_POINT ( 'NONE',  ( 1.000000000000000888, -6.997684042076912192, 2.698595569414189210 ) ) ;
#60972 = DIRECTION ( 'NONE',  ( 0.000000000000000000, -0.9289767198167950824, 0.3701381553399052948 ) ) ;
#60973 = CARTESIAN_POINT ( 'NONE',  ( 2.241352910868908754, -3.889181972941404553, -6.569501556381482921 ) ) ;
#60974 = AXIS2_PLACEMENT_3D ( 'NONE', #12024, #1742, #2056 ) ;
#60975 = EDGE_CURVE ( 'NONE', #10208, #25087, #24238, .T. ) ;
#60976 = LINE ( 'NONE', #5455, #38443 ) ;
#60977 = CARTESIAN_POINT ( 'NONE',  ( 0.2638984909335720941, -10.70468911391660072, -5.950360275955167921 ) ) ;
#60978 =( BOUNDED_CURVE ( )  B_SPLINE_CURVE ( 3, ( #45648, #20385, #40663, #10725 ),
 .UNSPECIFIED., .F., .F. ) 
 B_SPLINE_CURVE_WITH_KNOTS ( ( 4, 4 ),
 ( 5.851531777320561289, 5.909121302884260629 ),
 .UNSPECIFIED. ) 
 CURVE ( )  GEOMETRIC_REPRESENTATION_ITEM ( )  RATIONAL_B_SPLINE_CURVE ( ( 1.000000000000000000, 0.9997236396413186066, 0.9997236396413186066, 1.000000000000000000 ) ) 
 REPRESENTATION_ITEM ( '' )  );
#60979 = ORIENTED_EDGE ( 'NONE', *, *, #64613, .F. ) ;
#60980 = CARTESIAN_POINT ( 'NONE',  ( 2.266490820343227242, 0.1453321357832749183, 7.641399530653802508 ) ) ;
#60981 = CARTESIAN_POINT ( 'NONE',  ( 1.585986311398264403, 1.432643833071485906, -11.91909886592589451 ) ) ;
#60982 = CARTESIAN_POINT ( 'NONE',  ( 5.530133899448235191, -0.01324661008606523721, -0.008946569461392297334 ) ) ;
#60983 = ORIENTED_EDGE ( 'NONE', *, *, #11270, .T. ) ;
#60984 = CARTESIAN_POINT ( 'NONE',  ( -18.45334481119305892, 4.188336017657096733, 11.24834648941091864 ) ) ;
#60985 = CARTESIAN_POINT ( 'NONE',  ( 2.241537034860907163, 6.609284473755334233, 3.821322318518396433 ) ) ;
#60986 = ORIENTED_EDGE ( 'NONE', *, *, #43540, .F. ) ;
#60987 = AXIS2_PLACEMENT_3D ( 'NONE', #2857, #64325, #44361 ) ;
#60988 = AXIS2_PLACEMENT_3D ( 'NONE', #61439, #32488, #42136 ) ;
#60989 = ORIENTED_EDGE ( 'NONE', *, *, #34278, .T. ) ;
#60990 = ORIENTED_EDGE ( 'NONE', *, *, #22345, .F. ) ;
#60991 = ORIENTED_EDGE ( 'NONE', *, *, #48537, .T. ) ;
#60992 = DIRECTION ( 'NONE',  ( 0.000000000000000000, 0.01356324068817998940, -0.9999080150203990547 ) ) ;
#60993 = CARTESIAN_POINT ( 'NONE',  ( -35.05175862995318425, 0.003331684148536948054, 0.01212835938693181126 ) ) ;
#60994 = DIRECTION ( 'NONE',  ( -1.000000000000000000, 0.000000000000000000, 0.000000000000000000 ) ) ;
#60995 = DIRECTION ( 'NONE',  ( -1.000000000000000000, 0.000000000000000000, 0.000000000000000000 ) ) ;
#60996 = PLANE ( 'NONE',  #4552 ) ;
#60997 = CARTESIAN_POINT ( 'NONE',  ( -6.641947195041168150, -28.39580239767160919, 11.12859478088952336 ) ) ;
#60998 = CARTESIAN_POINT ( 'NONE',  ( 22.88594695219327235, -4.822122601967141264, -12.60940655271284427 ) ) ;
#61000 = EDGE_LOOP ( 'NONE', ( #30421, #24031, #57040, #47504 ) ) ;
#60999 = FACE_OUTER_BOUND ( 'NONE', #14025, .T. ) ;
#61001 = CARTESIAN_POINT ( 'NONE',  ( 2.241526690369557429, -2.594870554108887895, 7.179945570618750494 ) ) ;
#61002 = VERTEX_POINT ( 'NONE', #33806 ) ;
#61003 = DIRECTION ( 'NONE',  ( 1.000000000000000000, 0.000000000000000000, 0.000000000000000000 ) ) ;
#61004 = EDGE_LOOP ( 'NONE', ( #22116, #37428, #21390, #26255 ) ) ;
#61005 = ORIENTED_EDGE ( 'NONE', *, *, #17201, .T. ) ;
#61006 = CARTESIAN_POINT ( 'NONE',  ( 3.152665057736177445, 3.161213418915486795, 7.281573230473766145 ) ) ;
#61007 = CARTESIAN_POINT ( 'NONE',  ( 19.27363075669222425, -29.98494805059729984, 5.891112176854364613 ) ) ;
#61008 = AXIS2_PLACEMENT_3D ( 'NONE', #873, #1215, #20508 ) ;
#61009 = DIRECTION ( 'NONE',  ( 1.000000000000000000, 1.685093406416449860E-16, -1.011030131491573426E-17 ) ) ;
#61010 = ADVANCED_FACE ( 'NONE', ( #54774 ), #38817, .T. ) ;
#61011 = CARTESIAN_POINT ( 'NONE',  ( 37.00000000000000711, -6.307491713048959170, 9.908974237959705889 ) ) ;
#61012 = CARTESIAN_POINT ( 'NONE',  ( 0.4626703367443949499, -2.416235258139843634, 12.07256244737114059 ) ) ;
#61013 = CARTESIAN_POINT ( 'NONE',  ( 5.514970785353741078, 0.002796696073589738894, -0.003805873180274792905 ) ) ;
#61014 = ORIENTED_EDGE ( 'NONE', *, *, #25830, .T. ) ;
#61015 = ORIENTED_EDGE ( 'NONE', *, *, #894, .F. ) ;
#61016 = DIRECTION ( 'NONE',  ( 0.000000000000000000, -0.01356324068817998940, 0.9999080150203990547 ) ) ;
#61017 = ORIENTED_EDGE ( 'NONE', *, *, #30587, .T. ) ;
#61018 = CIRCLE ( 'NONE', #32323, 12.18650000000000055 ) ;
#61019 = ORIENTED_EDGE ( 'NONE', *, *, #51752, .T. ) ;
#61020 = DIRECTION ( 'NONE',  ( 0.000000000000000000, -1.000000000000000000, 0.000000000000000000 ) ) ;
#61021 = CARTESIAN_POINT ( 'NONE',  ( -27.08429572838383947, -2.279961732801590646, 0.2296550094122822017 ) ) ;
#61022 = DIRECTION ( 'NONE',  ( 0.3865475372811021937, 0.4442537292684328731, 0.8082200352954663769 ) ) ;
#61023 = CARTESIAN_POINT ( 'NONE',  ( 2.000000000000001776, 4.444115772890187444, -5.163689623839299081 ) ) ;
#61024 = DIRECTION ( 'NONE',  ( 0.000000000000000000, 0.000000000000000000, 1.000000000000000000 ) ) ;
#61025 = CARTESIAN_POINT ( 'NONE',  ( 0.000000000000000000, -6.767909380267593811, 0.7805499053120233954 ) ) ;
#61026 = VECTOR ( 'NONE', #33219, 1000.000000000000000 ) ;
#61027 = EDGE_CURVE ( 'NONE', #62196, #26384, #7977, .T. ) ;
#61028 = VERTEX_POINT ( 'NONE', #14817 ) ;
#61029 = EDGE_CURVE ( 'NONE', #22470, #13538, #17179, .T. ) ;
#61030 = ORIENTED_EDGE ( 'NONE', *, *, #63977, .F. ) ;
#61031 = EDGE_CURVE ( 'NONE', #27642, #28605, #44850, .T. ) ;
#61032 = CARTESIAN_POINT ( 'NONE',  ( -35.00000000000000000, 0.000000000000000000, 0.000000000000000000 ) ) ;
#61033 = CIRCLE ( 'NONE', #10094, 5.000000000000000000 ) ;
#61034 = CARTESIAN_POINT ( 'NONE',  ( 10.48620311856346454, 8.250315036047107142, 25.00000000000000000 ) ) ;
#61035 = DIRECTION ( 'NONE',  ( 0.000000000000000000, -0.01356324068817991828, 0.9999080150203990547 ) ) ;
#61036 = CARTESIAN_POINT ( 'NONE',  ( -27.28563798457902223, -2.896153581097044238, -0.04047623855284221417 ) ) ;
#61037 = CARTESIAN_POINT ( 'NONE',  ( 3.388896915696421708, -10.79019736087639281, 5.264843862020491372 ) ) ;
#61038 = ADVANCED_FACE ( 'NONE', ( #14183 ), #4888, .T. ) ;
#61039 = AXIS2_PLACEMENT_3D ( 'NONE', #36414, #65664, #14791 ) ;
#61040 = LINE ( 'NONE', #25792, #5472 ) ;
#61041 = EDGE_CURVE ( 'NONE', #32207, #3171, #41667, .T. ) ;
#61042 = CARTESIAN_POINT ( 'NONE',  ( 0.2851083653049504285, -0.4107471485392698018, -11.99296822225284131 ) ) ;
#61043 = CARTESIAN_POINT ( 'NONE',  ( -27.08417473062937475, -2.166271322019585277, -0.7460375461499409999 ) ) ;
#61044 = VERTEX_POINT ( 'NONE', #11485 ) ;
#61045 = CARTESIAN_POINT ( 'NONE',  ( -27.28563798457902223, 2.487904455214894117, 1.483130241384891468 ) ) ;
#61046 = CARTESIAN_POINT ( 'NONE',  ( 2.000000000000001776, 6.338823199656720142, -2.816798305433633853 ) ) ;
#61047 = CARTESIAN_POINT ( 'NONE',  ( 2.000000000000001776, -6.767909380267597363, -0.7805499053121327524 ) ) ;
#61048 = CIRCLE ( 'NONE', #30295, 4.999999999999999112 ) ;
#61049 = ADVANCED_FACE ( 'NONE', ( #5208 ), #46740, .T. ) ;
#61050 = CARTESIAN_POINT ( 'NONE',  ( 0.2646305136544072623, -12.08286001766534312, -1.996350543473119021 ) ) ;
#61051 = CARTESIAN_POINT ( 'NONE',  ( 2.969415267404796221, -7.260393470501854019, 3.055358878717769677 ) ) ;
#61052 = VERTEX_POINT ( 'NONE', #36441 ) ;
#61053 = CARTESIAN_POINT ( 'NONE',  ( -17.37319572219799113, -6.065883689981585114, -12.06447225982703486 ) ) ;
#61054 = DIRECTION ( 'NONE',  ( 0.000000000000000000, -0.4698238015817426949, -0.8827602140260283337 ) ) ;
#61056 = EDGE_CURVE ( 'NONE', #33077, #2794, #19327, .T. ) ;
#61055 = CARTESIAN_POINT ( 'NONE',  ( 2.241311220309555097, 1.234192392743173050, 7.533971938435846560 ) ) ;
#61057 = ORIENTED_EDGE ( 'NONE', *, *, #54093, .T. ) ;
#61058 = CYLINDRICAL_SURFACE ( 'NONE', #7934, 4.999999999999999112 ) ;
#61059 = CARTESIAN_POINT ( 'NONE',  ( -17.15720051295231485, 7.250774436309729509, -9.563211349854379151 ) ) ;
#61060 = DIRECTION ( 'NONE',  ( -1.000000000000000000, 0.000000000000000000, 0.000000000000000000 ) ) ;
#61062 = ORIENTED_EDGE ( 'NONE', *, *, #43077, .F. ) ;
#61061 = CARTESIAN_POINT ( 'NONE',  ( -32.00000000000000711, 12.00000000000000000, 1.469576158976823553E-15 ) ) ;
#61063 = DIRECTION ( 'NONE',  ( -1.000000000000000000, 0.000000000000000000, 0.000000000000000000 ) ) ;
#61064 = VECTOR ( 'NONE', #25870, 1000.000000000000000 ) ;
#61065 = CARTESIAN_POINT ( 'NONE',  ( 2.653899356900045081, -7.388433688587411119, -2.411250235128119090 ) ) ;
#61066 = ORIENTED_EDGE ( 'NONE', *, *, #17641, .F. ) ;
#61067 = CARTESIAN_POINT ( 'NONE',  ( 0.2648321136542688414, 7.762514728658100438, 9.471460387169299722 ) ) ;
#61068 = CARTESIAN_POINT ( 'NONE',  ( -35.00000000000000000, -8.699265615722922007, -8.534258022646191932 ) ) ;
#61069 = CARTESIAN_POINT ( 'NONE',  ( 24.08299418260464719, 1.037082133578634213, -11.95962290153675056 ) ) ;
#61070 = CARTESIAN_POINT ( 'NONE',  ( 8.437200413559441614, 4.669230153606584111, -12.66846808887212106 ) ) ;
#61071 = CARTESIAN_POINT ( 'NONE',  ( 0.1900979142430823110, -0.2738684153833558232, -13.49791647769710679 ) ) ;
#61072 = CARTESIAN_POINT ( 'NONE',  ( -18.58686583997219088, 4.910876720226735159, 12.57779378420807781 ) ) ;
#61073 = CARTESIAN_POINT ( 'NONE',  ( 0.3109076770649040200, 11.43910935267338580, -4.414555973477709117 ) ) ;
#61074 = ORIENTED_EDGE ( 'NONE', *, *, #12809, .F. ) ;
#61075 = DIRECTION ( 'NONE',  ( -0.000000000000000000, -0.000000000000000000, -1.000000000000000000 ) ) ;
#61076 = ORIENTED_EDGE ( 'NONE', *, *, #34731, .F. ) ;
#61077 = LINE ( 'NONE', #15508, #43265 ) ;
#61078 = CARTESIAN_POINT ( 'NONE',  ( 0.3002738374340798710, 11.43949898053770653, 4.403689978763103419 ) ) ;
#61079 = ADVANCED_FACE ( 'NONE', ( #35452 ), #21482, .T. ) ;
#61080 = EDGE_CURVE ( 'NONE', #27549, #2404, #1290, .T. ) ;
#61081 = EDGE_LOOP ( 'NONE', ( #8549, #14372, #43537, #34303 ) ) ;
#61082 = CARTESIAN_POINT ( 'NONE',  ( 2.000000000000001776, -6.586971819220355684, 3.586335490831369821 ) ) ;
#61083 = DIRECTION ( 'NONE',  ( 1.000000000000000000, 0.000000000000000000, 0.000000000000000000 ) ) ;
#61084 = CARTESIAN_POINT ( 'NONE',  ( 35.00000000000000000, -9.321877890560486435, -7.146664589317880178 ) ) ;
#61085 = ORIENTED_EDGE ( 'NONE', *, *, #48962, .F. ) ;
#61086 = ORIENTED_EDGE ( 'NONE', *, *, #59393, .F. ) ;
#61087 = CARTESIAN_POINT ( 'NONE',  ( 2.276905613633648073, -7.236369456722863802, -2.469846004795382743 ) ) ;
#61088 = EDGE_CURVE ( 'NONE', #43036, #12741, #53306, .T. ) ;
#61089 = VERTEX_POINT ( 'NONE', #41087 ) ;
#61090 = DIRECTION ( 'NONE',  ( 0.000000000000000000, -0.9718671068226434340, 0.2355298848897617037 ) ) ;
#61091 = CARTESIAN_POINT ( 'NONE',  ( 0.2648978790185593790, 9.295532325666449935, 7.972372351883061370 ) ) ;
#61092 = FACE_OUTER_BOUND ( 'NONE', #40237, .T. ) ;
#61093 = VECTOR ( 'NONE', #29742, 1000.000000000000000 ) ;
#61094 = CARTESIAN_POINT ( 'NONE',  ( 35.00000000000000000, 10.32377448871667625, -6.475373545682339582 ) ) ;
#61095 = CARTESIAN_POINT ( 'NONE',  ( 36.00000000000000711, 12.42372387097886488, 2.865935305911484043 ) ) ;
#61096 = FACE_OUTER_BOUND ( 'NONE', #20434, .T. ) ;
#61097 = ADVANCED_FACE ( 'NONE', ( #20497 ), #51093, .T. ) ;
#61098 = DIRECTION ( 'NONE',  ( -1.000000000000000000, -0.000000000000000000, -0.000000000000000000 ) ) ;
#61099 = ORIENTED_EDGE ( 'NONE', *, *, #62016, .T. ) ;
#61100 = CARTESIAN_POINT ( 'NONE',  ( 37.00000000000000711, 11.32068061209303522, 5.865551165830957814 ) ) ;
#61101 = CARTESIAN_POINT ( 'NONE',  ( 23.20721382908649488, 9.991207635573182699, -6.653344022984436279 ) ) ;
#61102 = EDGE_CURVE ( 'NONE', #40994, #14607, #11848, .T. ) ;
#61103 = CARTESIAN_POINT ( 'NONE',  ( 5.536195898058073439, 0.001224473329857981652, -0.008411485181669245415 ) ) ;
#61104 = CARTESIAN_POINT ( 'NONE',  ( -18.92121795399529915, 13.50133162273161069, 0.2605718306269828033 ) ) ;
#61105 = CARTESIAN_POINT ( 'NONE',  ( -2.952869152607111136, 7.581333670610111319, 11.17020052527586138 ) ) ;
#61106 = CARTESIAN_POINT ( 'NONE',  ( 2.354167843600960097, -6.278647867796540716, 25.00000000000000000 ) ) ;
#61107 = CARTESIAN_POINT ( 'NONE',  ( 2.827825597296800719, 8.278234963587719264, 3.592949031604448340 ) ) ;
#61108 = DIRECTION ( 'NONE',  ( 1.000000000000000000, 0.000000000000000000, 0.000000000000000000 ) ) ;
#61109 = VECTOR ( 'NONE', #39927, 1000.000000000000114 ) ;
#61110 = ORIENTED_EDGE ( 'NONE', *, *, #31910, .T. ) ;
#61111 = CARTESIAN_POINT ( 'NONE',  ( -7.489022030332961322, -5.127957880411574187, -10.84914964302385521 ) ) ;
#61112 = ORIENTED_EDGE ( 'NONE', *, *, #45409, .F. ) ;
#61113 = CARTESIAN_POINT ( 'NONE',  ( -3.322308238815765868, -10.53368969201583916, 5.762262606413962374 ) ) ;
#61114 = CARTESIAN_POINT ( 'NONE',  ( 0.2652384529303108418, 0.06607367983853688898, 12.24598125395192838 ) ) ;
#61115 = ADVANCED_FACE ( 'NONE', ( #40782 ), #15492, .T. ) ;
#61116 = DIRECTION ( 'NONE',  ( 0.000000000000000000, -0.01356324068817998940, 0.9999080150203990547 ) ) ;
#61117 = DIRECTION ( 'NONE',  ( 0.000000000000000000, 0.000000000000000000, -1.000000000000000000 ) ) ;
#61118 = DIRECTION ( 'NONE',  ( -1.000000000000000000, 0.000000000000000000, 0.000000000000000000 ) ) ;
#61119 = EDGE_CURVE ( 'NONE', #24026, #18208, #41408, .T. ) ;
#61120 = ORIENTED_EDGE ( 'NONE', *, *, #11852, .T. ) ;
#61121 = PRODUCT_DEFINITION_FORMATION_WITH_SPECIFIED_SOURCE ( 'ANY', '', #33322, .NOT_KNOWN. ) ;
#61122 = CARTESIAN_POINT ( 'NONE',  ( 5.515539859299206427, 0.0001942659352247811874, -0.006049968793488399305 ) ) ;
#61123 = CARTESIAN_POINT ( 'NONE',  ( 2.000000000000001776, 1.865193240757095916, 6.552473556515182374 ) ) ;
#61124 = CARTESIAN_POINT ( 'NONE',  ( 0.8320506296491587683, -1.781423711749659189, 12.30686996250300069 ) ) ;
#61125 = CARTESIAN_POINT ( 'NONE',  ( -22.31328051695926007, 3.401210163132566411, 1.671726071983929307 ) ) ;
#61126 = B_SPLINE_CURVE_WITH_KNOTS ( 'NONE', 3,
 ( #16679, #61565, #51627, #36302, #11047, #6073, #26330, #1069, #46951, #21338, #41944, #1731, #21997 ),
 .UNSPECIFIED., .F., .F.,
 ( 4, 3, 3, 3, 4 ),
 ( 2.602085213965210642E-18, 6.607593386745585248E-05, 0.0001321518677373532740, 0.0001982171734706192877, 0.0002642860854759484460 ),
 .UNSPECIFIED. ) ;
#61127 = EDGE_CURVE ( 'NONE', #47727, #37018, #56056, .T. ) ;
#61128 = ADVANCED_FACE ( 'NONE', ( #30773 ), #61365, .T. ) ;
#61129 = CARTESIAN_POINT ( 'NONE',  ( 1.452237505248552996, 12.64182585313126062, 0.5922625322517451885 ) ) ;
#61130 = DIRECTION ( 'NONE',  ( -1.000000000000000000, 0.000000000000000000, 0.000000000000000000 ) ) ;
#61131 = AXIS2_PLACEMENT_3D ( 'NONE', #45486, #60795, #12207 ) ;
#61132 = ORIENTED_EDGE ( 'NONE', *, *, #34210, .F. ) ;
#61134 = EDGE_CURVE ( 'NONE', #55855, #53922, #11176, .T. ) ;
#61133 = DIRECTION ( 'NONE',  ( -1.000000000000000000, 0.000000000000000000, -0.000000000000000000 ) ) ;
#61135 = VERTEX_POINT ( 'NONE', #47418 ) ;
#61136 = CARTESIAN_POINT ( 'NONE',  ( 0.2652384529303146166, 12.24598125395190884, -0.06607367983857954929 ) ) ;
#61137 = CARTESIAN_POINT ( 'NONE',  ( 2.241528039335006994, 7.168649579907130587, 2.625917297988412002 ) ) ;
#61138 = CARTESIAN_POINT ( 'NONE',  ( 29.03457606387295087, -4.854210015632035358, 10.97436308512422265 ) ) ;
#61139 = CARTESIAN_POINT ( 'NONE',  ( -5.804292984923859144, -1.481750644001851525, 11.90855073620921267 ) ) ;
#61140 = CIRCLE ( 'NONE', #32453, 4.999999999999997335 ) ;
#61141 = ORIENTED_EDGE ( 'NONE', *, *, #56789, .T. ) ;
#61142 = ORIENTED_EDGE ( 'NONE', *, *, #48382, .T. ) ;
#61143 = CARTESIAN_POINT ( 'NONE',  ( 0.3040950598368144520, -1.881452845810294594, -12.11647736519423191 ) ) ;
#61144 = ORIENTED_EDGE ( 'NONE', *, *, #39277, .T. ) ;
#61145 = DIRECTION ( 'NONE',  ( -1.000000000000000000, 0.000000000000000000, 0.000000000000000000 ) ) ;
#61146 = CARTESIAN_POINT ( 'NONE',  ( 35.00000000000000000, -9.063649021438894948, 8.146229107149494553 ) ) ;
#61147 = CARTESIAN_POINT ( 'NONE',  ( 47.00000000000000711, 4.705694406421931860E-17, -3.469127814946512892E-15 ) ) ;
#61148 = CARTESIAN_POINT ( 'NONE',  ( 1.375507693217069560, 9.273955665125992454, 8.553661013311447903 ) ) ;
#61149 = CARTESIAN_POINT ( 'NONE',  ( 1.372161826076961910, 9.274145586376256745, -8.551811013234910774 ) ) ;
#61150 = FACE_OUTER_BOUND ( 'NONE', #25392, .T. ) ;
#61151 = CARTESIAN_POINT ( 'NONE',  ( -11.24844400926880716, -6.045701199311597662, 10.37522813442839009 ) ) ;
#61152 = ORIENTED_EDGE ( 'NONE', *, *, #64674, .T. ) ;
#61153 = DIRECTION ( 'NONE',  ( 0.000000000000000000, 0.3554799084908970563, 0.9346839223284539866 ) ) ;
#61154 = ORIENTED_EDGE ( 'NONE', *, *, #9794, .F. ) ;
#61155 = CARTESIAN_POINT ( 'NONE',  ( 0.3675815128205894289, -2.391755495700522705, -12.04510820461661780 ) ) ;
#61156 = CARTESIAN_POINT ( 'NONE',  ( 0.3006302518452019235, -9.243299516615085309, 8.051021221755751966 ) ) ;
#61157 = CARTESIAN_POINT ( 'NONE',  ( -35.00000000000000000, -11.91791701451264629, -2.544412758415973030 ) ) ;
#61158 = EDGE_CURVE ( 'NONE', #42345, #33595, #13136, .T. ) ;
#61159 = ORIENTED_EDGE ( 'NONE', *, *, #14959, .T. ) ;
#61160 = B_SPLINE_CURVE_WITH_KNOTS ( 'NONE', 3,
 ( #33862, #59469, #22932, #63459, #33218, #2981, #8596, #58506, #17931, #48854, #63786, #18273, #38534, #26671, #28885, #58856 ),
 .UNSPECIFIED., .F., .F.,
 ( 4, 3, 3, 3, 3, 4 ),
 ( 0.000000000000000000, 6.991367980366391542E-05, 0.0001398269368981360167, 0.0002097400188389093628, 0.0002811534801551364318, 0.0003526297678872490409 ),
 .UNSPECIFIED. ) ;
#61161 = DIRECTION ( 'NONE',  ( -1.836970198721029688E-16, 1.000000000000000000, 0.000000000000000000 ) ) ;
#61162 = EDGE_CURVE ( 'NONE', #45235, #24100, #22496, .T. ) ;
#61163 = ORIENTED_EDGE ( 'NONE', *, *, #25231, .F. ) ;
#61164 = DIRECTION ( 'NONE',  ( 1.000000000000000000, 0.000000000000000000, 0.000000000000000000 ) ) ;
#61165 = CARTESIAN_POINT ( 'NONE',  ( 6.361445718264521432, -4.355102044641763648, -12.77822703589027320 ) ) ;
#61166 = DIRECTION ( 'NONE',  ( 0.000000000000000000, 0.000000000000000000, 1.000000000000000000 ) ) ;
#61167 = CARTESIAN_POINT ( 'NONE',  ( -27.09342121492585065, -2.251107617621292967, -0.5565043948850181277 ) ) ;
#61168 = ORIENTED_EDGE ( 'NONE', *, *, #40381, .F. ) ;
#61169 = ORIENTED_EDGE ( 'NONE', *, *, #58315, .T. ) ;
#61170 = CARTESIAN_POINT ( 'NONE',  ( 3.152665057736245391, 2.258875078500370837, -7.609997527622033076 ) ) ;
#61171 = ORIENTED_EDGE ( 'NONE', *, *, #57402, .T. ) ;
#61172 = CARTESIAN_POINT ( 'NONE',  ( 37.00000000000000711, -12.71517666308947092, 0.9416912585475696318 ) ) ;
#61173 = ORIENTED_EDGE ( 'NONE', *, *, #52853, .T. ) ;
#61174 = EDGE_CURVE ( 'NONE', #15952, #51800, #62350, .T. ) ;
#61175 = VERTEX_POINT ( 'NONE', #11806 ) ;
#61176 = EDGE_LOOP ( 'NONE', ( #43764, #14512, #18927, #9057 ) ) ;
#61177 = DIRECTION ( 'NONE',  ( -1.000000000000000000, 0.000000000000000000, 0.000000000000000000 ) ) ;
#61178 = DIRECTION ( 'NONE',  ( -1.000000000000000000, 0.000000000000000000, 0.000000000000000000 ) ) ;
#61179 = CARTESIAN_POINT ( 'NONE',  ( 35.00000000000000000, -9.348667969174460524, -7.817492529713823579 ) ) ;
#61180 = CARTESIAN_POINT ( 'NONE',  ( -24.42101984568203576, 3.884389025764524384, -1.824625598916865155 ) ) ;
#61181 = DIRECTION ( 'NONE',  ( 0.000000000000000000, 0.000000000000000000, 1.000000000000000000 ) ) ;
#61182 = ORIENTED_EDGE ( 'NONE', *, *, #10420, .F. ) ;
#61183 = VECTOR ( 'NONE', #37703, 1000.000000000000000 ) ;
#61184 = CARTESIAN_POINT ( 'NONE',  ( -28.41827485489077532, 3.509237424706437292, 11.47541949982830722 ) ) ;
#61185 = VECTOR ( 'NONE', #10405, 1000.000000000000000 ) ;
#61186 = ORIENTED_EDGE ( 'NONE', *, *, #60242, .T. ) ;
#61187 =( BOUNDED_SURFACE ( )  B_SPLINE_SURFACE ( 3, 1, ( 
 ( #17536, #53097 ),
 ( #1599, #58096 ),
 ( #62731, #17197 ),
 ( #57781, #12851 ) ),
 .UNSPECIFIED., .F., .F., .F. ) 
 B_SPLINE_SURFACE_WITH_KNOTS ( ( 4, 4 ),
 ( 2, 2 ),
 ( 0.000000000000000000, 1.000000000000000000 ),
 ( 0.000000000000000000, 1.000000000000000000 ),
 .UNSPECIFIED. ) 
 GEOMETRIC_REPRESENTATION_ITEM ( )  RATIONAL_B_SPLINE_SURFACE ( (
 ( 1.000000000000000000, 1.000000000000000000),
 ( 0.9856612449720755231, 0.9999558406602322425),
 ( 0.9856612449720755231, 0.9999558406602322425),
 ( 1.000000000000000000, 1.000000000000000000) ) ) 
 REPRESENTATION_ITEM ( '' )  SURFACE ( )  );
#61188 = CARTESIAN_POINT ( 'NONE',  ( 2.305787727787085295, 5.970480882365287734, -4.792270232040832134 ) ) ;
#61189 = DIRECTION ( 'NONE',  ( 1.000000000000000000, -0.000000000000000000, 0.000000000000000000 ) ) ;
#61190 = CARTESIAN_POINT ( 'NONE',  ( 5.515188684475870851, -0.0003622115669623649468, 0.005339000964281801972 ) ) ;
#61191 = EDGE_CURVE ( 'NONE', #47785, #9350, #27767, .T. ) ;
#61192 = CARTESIAN_POINT ( 'NONE',  ( 1.634816307077888498, 10.17753964889907436, -7.601181930720465552 ) ) ;
#61193 = DIRECTION ( 'NONE',  ( 0.9606638835031803270, 0.2249116044183872010, -0.1629100154396133371 ) ) ;
#61194 = CARTESIAN_POINT ( 'NONE',  ( 2.573738926104374158, -7.741646296020614493, -0.2352053552898267230 ) ) ;
#61195 = EDGE_CURVE ( 'NONE', #43792, #9473, #22122, .T. ) ;
#61196 = ORIENTED_EDGE ( 'NONE', *, *, #39529, .T. ) ;
#61197 = LINE ( 'NONE', #60870, #8835 ) ;
#61198 = ORIENTED_EDGE ( 'NONE', *, *, #19701, .F. ) ;
#61199 = CARTESIAN_POINT ( 'NONE',  ( 0.2671309869109465551, 10.68612389951478114, 5.982543484153262980 ) ) ;
#61200 = CARTESIAN_POINT ( 'NONE',  ( -35.00000000000000000, -11.42599468261432527, 4.237620530777758354 ) ) ;
#61201 = CARTESIAN_POINT ( 'NONE',  ( 36.00000000000000711, 8.366449238204499039, 9.621072037176899627 ) ) ;
#61202 = DIRECTION ( 'NONE',  ( 1.000000000000000000, -0.000000000000000000, -0.000000000000000000 ) ) ;
#61203 = ORIENTED_EDGE ( 'NONE', *, *, #31834, .F. ) ;
#61204 = CARTESIAN_POINT ( 'NONE',  ( 37.00000000000000711, 1.171570255487609291, 11.68758509253246380 ) ) ;
#61205 = DIRECTION ( 'NONE',  ( 0.000000000000000000, -0.5767582926624852391, -0.8169148498130358593 ) ) ;
#61206 = CARTESIAN_POINT ( 'NONE',  ( -37.00000000000000711, 0.000000000000000000, 0.000000000000000000 ) ) ;
#61207 = DIRECTION ( 'NONE',  ( 0.000000000000000000, 0.000000000000000000, 1.000000000000000000 ) ) ;
#61208 = EDGE_CURVE ( 'NONE', #22936, #27434, #56476, .T. ) ;
#61209 = EDGE_CURVE ( 'NONE', #50989, #7512, #48070, .T. ) ;
#61210 = CARTESIAN_POINT ( 'NONE',  ( 5.530133899448235191, -0.008946569461392342437, -0.01324661008606586518 ) ) ;
#61211 = B_SPLINE_CURVE_WITH_KNOTS ( 'NONE', 3,
 ( #5574, #25845, #31477, #26818, #35476, #15833, #1230, #21511, #60758, #251, #5913, #46134, #36111, #40807, #41434, #35783, #56419, #30484, #57087, #55774, #10867, #5231 ),
 .UNSPECIFIED., .F., .F.,
 ( 4, 3, 3, 3, 3, 3, 3, 4 ),
 ( 4.735866574735071843E-18, 6.990956068646401111E-05, 0.0001398191187764049009, 0.0002097286751720215444, 0.0002796382307041361554, 0.0003495477861619815082, 0.0004194573423310287374, 0.0005586102576333139540 ),
 .UNSPECIFIED. ) ;
#61213 = EDGE_CURVE ( 'NONE', #37677, #34871, #52277, .T. ) ;
#61212 = CARTESIAN_POINT ( 'NONE',  ( 5.530133899448235191, -0.01536822665454898318, 0.004396748047611176956 ) ) ;
#61214 = CARTESIAN_POINT ( 'NONE',  ( 2.242418902651938772, -5.912154560271186021, -4.830735119000208577 ) ) ;
#61215 = LINE ( 'NONE', #65523, #15546 ) ;
#61216 = CARTESIAN_POINT ( 'NONE',  ( 2.253265082352431392, 0.1282654837135756010, -7.637296367516834827 ) ) ;
#61217 = EDGE_CURVE ( 'NONE', #48103, #44068, #44785, .T. ) ;
#61218 = ORIENTED_EDGE ( 'NONE', *, *, #50744, .F. ) ;
#61219 = CIRCLE ( 'NONE', #30417, 12.18650000000000055 ) ;
#61220 = ORIENTED_EDGE ( 'NONE', *, *, #32685, .F. ) ;
#61221 = CARTESIAN_POINT ( 'NONE',  ( 0.000000000000000000, 0.3246585432987117992, -6.805031400696120336 ) ) ;
#61222 = CARTESIAN_POINT ( 'NONE',  ( 28.14317553103694181, -3.466682545733132503, -23.84441711261399988 ) ) ;
#61223 = DIRECTION ( 'NONE',  ( -1.000000000000000000, 0.000000000000000000, 0.000000000000000000 ) ) ;
#61224 = CARTESIAN_POINT ( 'NONE',  ( 2.253265082353311577, -1.199885753715151715, -7.543541742287505514 ) ) ;
#61225 = ORIENTED_EDGE ( 'NONE', *, *, #5858, .T. ) ;
#61226 = VERTEX_POINT ( 'NONE', #47731 ) ;
#61227 = ORIENTED_EDGE ( 'NONE', *, *, #41048, .F. ) ;
#61228 = CARTESIAN_POINT ( 'NONE',  ( 29.26291958553499484, -9.868730160957575492, 6.831222511614969406 ) ) ;
#61229 = CARTESIAN_POINT ( 'NONE',  ( -21.04906020170784586, -11.41231286973902215, -3.710994071045400133 ) ) ;
#61230 = EDGE_LOOP ( 'NONE', ( #28030, #50645, #62013, #57505 ) ) ;
#61231 = DIRECTION ( 'NONE',  ( 0.000000000000000000, 0.01356324068817998940, -0.9999080150203989437 ) ) ;
#61232 = DIRECTION ( 'NONE',  ( 0.000000000000000000, -0.01356324068817992175, 0.9999080150203990547 ) ) ;
#61233 = ADVANCED_FACE ( 'NONE', ( #2175 ), #52408, .T. ) ;
#61234 = ORIENTED_EDGE ( 'NONE', *, *, #1831, .T. ) ;
#61235 = CARTESIAN_POINT ( 'NONE',  ( 2.259025283528617756, 4.805599953367311272, -5.939720477913882135 ) ) ;
#61236 = CARTESIAN_POINT ( 'NONE',  ( 15.07617326819549142, -33.99933334076585112, -8.515830899730527648 ) ) ;
#61237 = CARTESIAN_POINT ( 'NONE',  ( -35.00000000000000000, 0.000000000000000000, 0.000000000000000000 ) ) ;
#61238 = EDGE_LOOP ( 'NONE', ( #27973, #29669, #56822, #23955 ) ) ;
#61239 = CYLINDRICAL_SURFACE ( 'NONE', #36325, 4.999999999999999112 ) ;
#61240 = ORIENTED_EDGE ( 'NONE', *, *, #7041, .T. ) ;
#61241 = CARTESIAN_POINT ( 'NONE',  ( 0.3006302518452045880, -6.323626002161014448, -10.50091819089221978 ) ) ;
#61242 = VERTEX_POINT ( 'NONE', #22452 ) ;
#61243 = CARTESIAN_POINT ( 'NONE',  ( -22.30625920655495165, 3.403091720605023962, 1.672644928563048472 ) ) ;
#61244 = DIRECTION ( 'NONE',  ( 0.000000000000000000, 0.8827602140260332186, -0.4698238015817334245 ) ) ;
#61245 = CARTESIAN_POINT ( 'NONE',  ( 12.93723047338301058, 4.476360154859203355, 25.00000000000000000 ) ) ;
#61246 = LINE ( 'NONE', #51940, #6038 ) ;
#61247 = CARTESIAN_POINT ( 'NONE',  ( 0.3164563675027638467, -12.26087493884171487, 0.2404665832030958295 ) ) ;
#61248 = CARTESIAN_POINT ( 'NONE',  ( 5.514970785353741078, 0.003805873180274780762, 0.002796696073589751037 ) ) ;
#61249 = CARTESIAN_POINT ( 'NONE',  ( -32.00000000000000000, 15.00000000000000000, 1.836970198721029589E-15 ) ) ;
#61250 = CARTESIAN_POINT ( 'NONE',  ( 2.000000000000001776, 6.906413915731192787, 0.6453518998147528274 ) ) ;
#61252 = VERTEX_POINT ( 'NONE', #52727 ) ;
#61251 = CARTESIAN_POINT ( 'NONE',  ( 36.00000000000000711, -5.865551165831000446, 11.32068061209301035 ) ) ;
#61253 = CARTESIAN_POINT ( 'NONE',  ( -35.04834644901396956, 0.002604658385682454436, -0.01358669851862852156 ) ) ;
#61254 = ORIENTED_EDGE ( 'NONE', *, *, #43979, .F. ) ;
#61255 = CARTESIAN_POINT ( 'NONE',  ( 0.3053067050349138056, -4.409108891833727562, 11.43920902168905407 ) ) ;
#61256 = ORIENTED_EDGE ( 'NONE', *, *, #45473, .F. ) ;
#61257 = CARTESIAN_POINT ( 'NONE',  ( 2.000000000000001776, 6.160607635185464837, -4.277489166005534749 ) ) ;
#61258 = ADVANCED_FACE ( 'NONE', ( #42718 ), #7476, .T. ) ;
#61259 = APPLICATION_CONTEXT ( 'automotive_design' ) ;
#61260 = ORIENTED_EDGE ( 'NONE', *, *, #43354, .F. ) ;
#61261 = CARTESIAN_POINT ( 'NONE',  ( -35.00000000000000000, -4.946702696913093611, -11.13736569743279681 ) ) ;
#61262 = LINE ( 'NONE', #56951, #14868 ) ;
#61263 = DIRECTION ( 'NONE',  ( 1.000000000000000000, 0.000000000000000000, -0.000000000000000000 ) ) ;
#61264 = CIRCLE ( 'NONE', #45317, 2.899999999999994582 ) ;
#61265 = DIRECTION ( 'NONE',  ( -1.000000000000000000, 0.000000000000000000, -0.000000000000000000 ) ) ;
#61266 = ADVANCED_FACE ( 'NONE', ( #58717 ), #33419, .T. ) ;
#61267 = CARTESIAN_POINT ( 'NONE',  ( 0.000000000000000000, 3.979254915827366901, 5.681598592373755530 ) ) ;
#61268 = ORIENTED_EDGE ( 'NONE', *, *, #7345, .F. ) ;
#61269 = CIRCLE ( 'NONE', #62300, 12.74999999999999822 ) ;
#61270 = CARTESIAN_POINT ( 'NONE',  ( 5.516018279890452902, 0.006707902355168863032, 0.0009545156522404598482 ) ) ;
#61271 = ORIENTED_EDGE ( 'NONE', *, *, #32624, .F. ) ;
#61272 = DIRECTION ( 'NONE',  ( -1.000000000000000000, -1.836970198721029688E-16, 0.000000000000000000 ) ) ;
#61273 = DIRECTION ( 'NONE',  ( 1.000000000000000000, 0.000000000000000000, 0.000000000000000000 ) ) ;
#61274 = CARTESIAN_POINT ( 'NONE',  ( 0.2648978790185619880, -7.972372351882965447, -9.295532325666529871 ) ) ;
#61275 = ORIENTED_EDGE ( 'NONE', *, *, #57958, .F. ) ;
#61276 = DIRECTION ( 'NONE',  ( 1.000000000000000000, -0.000000000000000000, -0.000000000000000000 ) ) ;
#61277 = ADVANCED_FACE ( 'NONE', ( #7832 ), #37750, .T. ) ;
#61278 = FACE_OUTER_BOUND ( 'NONE', #19444, .T. ) ;
#61279 = DIRECTION ( 'NONE',  ( -1.000000000000000000, -0.000000000000000000, 0.000000000000000000 ) ) ;
#61280 = DIRECTION ( 'NONE',  ( -0.000000000000000000, -1.000000000000000000, -0.000000000000000000 ) ) ;
#61281 = LINE ( 'NONE', #1099, #24314 ) ;
#61282 = ORIENTED_EDGE ( 'NONE', *, *, #8392, .F. ) ;
#61283 = DIRECTION ( 'NONE',  ( 0.000000000000000000, -0.01356324068817998940, 0.9999080150203990547 ) ) ;
#61284 = CARTESIAN_POINT ( 'NONE',  ( 1.719304012338199517, 0.000000000000000000, 0.000000000000000000 ) ) ;
#61285 = CARTESIAN_POINT ( 'NONE',  ( -35.00000000000000000, -12.70128625845193682, 1.113475361586445889 ) ) ;
#61286 = EDGE_CURVE ( 'NONE', #42768, #32729, #43758, .T. ) ;
#61287 = CARTESIAN_POINT ( 'NONE',  ( 0.2655924914740778187, 9.352877839710604491, 7.905499957109269893 ) ) ;
#61288 = CARTESIAN_POINT ( 'NONE',  ( 2.941278708680199916, 4.788765081995630446, 3.842273877444578822 ) ) ;
#61289 = EDGE_LOOP ( 'NONE', ( #42356, #30320, #12969, #14698 ) ) ;
#61290 = CIRCLE ( 'NONE', #22001, 2.899999999999994582 ) ;
#61291 = CARTESIAN_POINT ( 'NONE',  ( 1.109979610368954095, 10.60154531817190993, 6.674783385103837396 ) ) ;
#61292 = DIRECTION ( 'NONE',  ( 1.000000000000000000, -0.000000000000000000, 0.000000000000000000 ) ) ;
#61293 = CARTESIAN_POINT ( 'NONE',  ( -22.28073302975501235, 3.560599703067816701, -0.9769664947681093725 ) ) ;
#61294 = EDGE_LOOP ( 'NONE', ( #19147, #56107, #5668, #2365 ) ) ;
#61295 = DIRECTION ( 'NONE',  ( 0.000000000000000000, 0.3193015301359806157, -0.9476531711828021232 ) ) ;
#61296 = ORIENTED_EDGE ( 'NONE', *, *, #59439, .F. ) ;
#61297 = ORIENTED_EDGE ( 'NONE', *, *, #14014, .T. ) ;
#61298 = AXIS2_PLACEMENT_3D ( 'NONE', #54483, #64120, #3637 ) ;
#61299 = ORIENTED_EDGE ( 'NONE', *, *, #6848, .F. ) ;
#61300 = LINE ( 'NONE', #61967, #62416 ) ;
#61301 = ORIENTED_EDGE ( 'NONE', *, *, #818, .T. ) ;
#61302 = CARTESIAN_POINT ( 'NONE',  ( 3.152665057735509979, 7.102135024646700323, 3.546019893115181620 ) ) ;
#61303 = FACE_OUTER_BOUND ( 'NONE', #62283, .T. ) ;
#61304 = CARTESIAN_POINT ( 'NONE',  ( -35.00000000000000000, -6.753013023069787124, 10.14433819232432477 ) ) ;
#61305 = CARTESIAN_POINT ( 'NONE',  ( 0.2650492594609225039, 4.291723947796471705, -11.46945808033129310 ) ) ;
#61306 = ADVANCED_FACE ( 'NONE', ( #16804 ), #43054, .T. ) ;
#61307 = CARTESIAN_POINT ( 'NONE',  ( 2.903928887688177696, 7.316175791236187997, -4.835706109686608301 ) ) ;
#61308 = CARTESIAN_POINT ( 'NONE',  ( -6.778443870680312067, -26.22850392868687663, 14.88193859458597856 ) ) ;
#61309 = CARTESIAN_POINT ( 'NONE',  ( -27.10719052120871098, 1.044362304621487825, -2.116547233941206585 ) ) ;
#61311 = VERTEX_POINT ( 'NONE', #58367 ) ;
#61310 = DIRECTION ( 'NONE',  ( 0.000000000000000000, -0.4935949184179321825, 0.8696919319575150409 ) ) ;
#61312 = EDGE_CURVE ( 'NONE', #31078, #2293, #32012, .T. ) ;
#61313 = FACE_OUTER_BOUND ( 'NONE', #9558, .T. ) ;
#61314 = ORIENTED_EDGE ( 'NONE', *, *, #60782, .F. ) ;
#61315 = CARTESIAN_POINT ( 'NONE',  ( -47.00000000000000711, 0.000000000000000000, 0.000000000000000000 ) ) ;
#61316 = ORIENTED_EDGE ( 'NONE', *, *, #1361, .F. ) ;
#61317 = VERTEX_POINT ( 'NONE', #24412 ) ;
#61318 = CARTESIAN_POINT ( 'NONE',  ( -22.27719381268171261, -0.9730858478813817491, 3.550654232855428027 ) ) ;
#61319 = CARTESIAN_POINT ( 'NONE',  ( 11.58535936493820273, -28.03978107659456498, 13.63905399333220281 ) ) ;
#61320 = CARTESIAN_POINT ( 'NONE',  ( -35.04660725145885891, 0.008590646501148855446, 0.008800808525098732099 ) ) ;
#61321 = ADVANCED_FACE ( 'NONE', ( #28420 ), #8470, .T. ) ;
#61322 = CARTESIAN_POINT ( 'NONE',  ( 2.931247277082682512, 7.800615791174669411, -0.9994150891045507912 ) ) ;
#61323 = CARTESIAN_POINT ( 'NONE',  ( 1.109979610369596470, -2.646302643132046217, 12.24510427445470384 ) ) ;
#61324 = LINE ( 'NONE', #16449, #37310 ) ;
#61325 = ORIENTED_EDGE ( 'NONE', *, *, #5245, .T. ) ;
#61326 = ORIENTED_EDGE ( 'NONE', *, *, #51967, .F. ) ;
#61327 = DIRECTION ( 'NONE',  ( -0.000000000000000000, -0.000000000000000000, -1.000000000000000000 ) ) ;
#61328 = VERTEX_POINT ( 'NONE', #60007 ) ;
#61329 = EDGE_CURVE ( 'NONE', #21190, #21166, #40616, .T. ) ;
#61330 = VERTEX_POINT ( 'NONE', #53715 ) ;
#61331 = CARTESIAN_POINT ( 'NONE',  ( -37.00000000000000711, 10.62137734850268345, 5.015831474386344802 ) ) ;
#61332 = LINE ( 'NONE', #26752, #11588 ) ;
#61333 = CARTESIAN_POINT ( 'NONE',  ( -22.28856623400852399, 0.9049353338066689068, -3.603818606161816707 ) ) ;
#61334 = DIRECTION ( 'NONE',  ( 1.000000000000000000, 0.000000000000000000, 0.000000000000000000 ) ) ;
#61335 = CARTESIAN_POINT ( 'NONE',  ( -22.27721701579900682, 1.205877546543726364, -3.478642907697082620 ) ) ;
#61336 = DIRECTION ( 'NONE',  ( 0.000000000000000000, -0.01356324068817991828, 0.9999080150203990547 ) ) ;
#61337 = AXIS2_PLACEMENT_3D ( 'NONE', #3645, #64436, #32862 ) ;
#61338 = VERTEX_POINT ( 'NONE', #59037 ) ;
#61339 = DIRECTION ( 'NONE',  ( -1.000000000000000000, 0.000000000000000000, -0.000000000000000000 ) ) ;
#61340 = CARTESIAN_POINT ( 'NONE',  ( 5.376045869553820467, -9.552872917373893102, 7.269855246128603454 ) ) ;
#61341 = DIRECTION ( 'NONE',  ( -1.000000000000000000, -0.000000000000000000, 0.000000000000000000 ) ) ;
#61342 = AXIS2_PLACEMENT_3D ( 'NONE', #34494, #49798, #15194 ) ;
#61343 =( BOUNDED_SURFACE ( )  B_SPLINE_SURFACE ( 3, 1, ( 
 ( #21960, #6681 ),
 ( #17639, #16965 ),
 ( #37235, #11971 ),
 ( #52570, #6999 ) ),
 .UNSPECIFIED., .F., .F., .F. ) 
 B_SPLINE_SURFACE_WITH_KNOTS ( ( 4, 4 ),
 ( 2, 2 ),
 ( 0.000000000000000000, 1.000000000000000000 ),
 ( 0.000000000000000000, 1.000000000000000000 ),
 .UNSPECIFIED. ) 
 GEOMETRIC_REPRESENTATION_ITEM ( )  RATIONAL_B_SPLINE_SURFACE ( (
 ( 1.000000000000000000, 1.000000000000000000),
 ( 0.9856612449720755231, 0.9999558406602322425),
 ( 0.9856612449720755231, 0.9999558406602322425),
 ( 1.000000000000000000, 1.000000000000000000) ) ) 
 REPRESENTATION_ITEM ( '' )  SURFACE ( )  );
#61344 = FACE_OUTER_BOUND ( 'NONE', #36285, .T. ) ;
#61345 = LINE ( 'NONE', #21110, #4604 ) ;
#61346 = CARTESIAN_POINT ( 'NONE',  ( 2.000000000000001776, 0.000000000000000000, 0.000000000000000000 ) ) ;
#61347 = ORIENTED_EDGE ( 'NONE', *, *, #26688, .T. ) ;
#61348 = EDGE_CURVE ( 'NONE', #63981, #8085, #53355, .T. ) ;
#61349 = CARTESIAN_POINT ( 'NONE',  ( 0.2652384529303122851, 10.63836770010965793, 6.065769141714241641 ) ) ;
#61350 = CARTESIAN_POINT ( 'NONE',  ( 2.907497136251165681, 1.009055026157950952, -7.791429554169957861 ) ) ;
#61351 = CARTESIAN_POINT ( 'NONE',  ( 36.00000000000000711, 3.473736367725426266, 12.26766708251987836 ) ) ;
#61352 = ADVANCED_FACE ( 'NONE', ( #48720 ), #2126, .F. ) ;
#61353 = CARTESIAN_POINT ( 'NONE',  ( 2.639814597422738718, -6.594772041715911470, -4.103563379978084846 ) ) ;
#61354 = CARTESIAN_POINT ( 'NONE',  ( 5.530133899448235191, -0.001661287012794241151, 0.01589823604557754830 ) ) ;
#61355 = ORIENTED_EDGE ( 'NONE', *, *, #13236, .T. ) ;
#61356 = CARTESIAN_POINT ( 'NONE',  ( 2.241451721903217731, -3.764430789729930726, -6.641849090084989804 ) ) ;
#61357 = CYLINDRICAL_SURFACE ( 'NONE', #37543, 12.18649999999999878 ) ;
#61358 = CARTESIAN_POINT ( 'NONE',  ( 16.10228578084485562, -34.99999999976227372, -4.568518662555822729 ) ) ;
#61359 = ORIENTED_EDGE ( 'NONE', *, *, #40669, .T. ) ;
#61360 = CYLINDRICAL_SURFACE ( 'NONE', #22785, 13.50000000000000178 ) ;
#61361 = CARTESIAN_POINT ( 'NONE',  ( -10.00000000000000178, 0.000000000000000000, 0.000000000000000000 ) ) ;
#61362 = CARTESIAN_POINT ( 'NONE',  ( 36.00000000000000711, 2.696588552979229725, 12.46157735505186004 ) ) ;
#61364 = ORIENTED_EDGE ( 'NONE', *, *, #35711, .T. ) ;
#61363 = FACE_OUTER_BOUND ( 'NONE', #34628, .T. ) ;
#61365 = CYLINDRICAL_SURFACE ( 'NONE', #5520, 6.936499999999988120 ) ;
#61366 = AXIS2_PLACEMENT_3D ( 'NONE', #20273, #10289, #34575 ) ;
#61367 = EDGE_CURVE ( 'NONE', #311, #44305, #1343, .T. ) ;
#61368 = CARTESIAN_POINT ( 'NONE',  ( 2.430348790457330210, -7.297553103283477505, -2.448665558939176368 ) ) ;
#61369 = ORIENTED_EDGE ( 'NONE', *, *, #39102, .T. ) ;
#61370 = DIRECTION ( 'NONE',  ( 0.000000000000000000, -0.9246979985058680906, -0.3807014730195321661 ) ) ;
#61371 = CARTESIAN_POINT ( 'NONE',  ( -27.08506889328327816, 1.324351020479957564, 1.872884652026852725 ) ) ;
#61372 = FACE_OUTER_BOUND ( 'NONE', #58706, .T. ) ;
#61373 = CARTESIAN_POINT ( 'NONE',  ( 8.676227275390266058, 5.971235288444897371, -12.11418353888797661 ) ) ;
#61374 = EDGE_CURVE ( 'NONE', #63634, #14535, #8808, .T. ) ;
#61375 = DIRECTION ( 'NONE',  ( -1.000000000000000000, 0.000000000000000000, 0.000000000000000000 ) ) ;
#61376 = ADVANCED_FACE ( 'NONE', ( #29096 ), #49401, .T. ) ;
#61377 = CARTESIAN_POINT ( 'NONE',  ( -18.56098820112710968, 4.668070274350404780, 12.66988895734626297 ) ) ;
#61378 = CYLINDRICAL_SURFACE ( 'NONE', #10, 5.000000000000000888 ) ;
#61379 = CIRCLE ( 'NONE', #7223, 2.899999999999995026 ) ;
#61380 = EDGE_CURVE ( 'NONE', #64240, #19313, #59677, .T. ) ;
#61381 = ORIENTED_EDGE ( 'NONE', *, *, #62320, .T. ) ;
#61382 = CARTESIAN_POINT ( 'NONE',  ( 2.000000000000001776, -3.979254915827311390, -5.681598592373819478 ) ) ;
#61383 = EDGE_LOOP ( 'NONE', ( #55586, #27616, #60009, #27009 ) ) ;
#61384 = CARTESIAN_POINT ( 'NONE',  ( 0.000000000000000000, 0.000000000000000000, 0.000000000000000000 ) ) ;
#61385 = CYLINDRICAL_SURFACE ( 'NONE', #13498, 5.000000000000000888 ) ;
#61386 = DIRECTION ( 'NONE',  ( 0.000000000000000000, -0.8835120444460178302, -0.4684084406997996997 ) ) ;
#61387 = ADVANCED_FACE ( 'NONE', ( #54029 ), #9123, .T. ) ;
#61388 = CARTESIAN_POINT ( 'NONE',  ( 35.00000000000000000, 0.01609748574445066943, -11.74614673114903773 ) ) ;
#61389 = ORIENTED_EDGE ( 'NONE', *, *, #30011, .F. ) ;
#61390 = CARTESIAN_POINT ( 'NONE',  ( -22.30625920655495165, -0.8854385781085337692, 3.687109008463850479 ) ) ;
#61391 = DIRECTION ( 'NONE',  ( 0.000000000000000000, -0.04924826701375277505, -0.9987865678893275145 ) ) ;
#61393 = EDGE_CURVE ( 'NONE', #35473, #45350, #18340, .T. ) ;
#61392 = LINE ( 'NONE', #31155, #40400 ) ;
#61394 = ORIENTED_EDGE ( 'NONE', *, *, #62630, .T. ) ;
#61395 = ORIENTED_EDGE ( 'NONE', *, *, #31265, .T. ) ;
#61396 = CARTESIAN_POINT ( 'NONE',  ( 35.00000000000000000, 10.12742074351896271, -7.745827850123049529 ) ) ;
#61397 = B_SPLINE_CURVE_WITH_KNOTS ( 'NONE', 3,
 ( #59397, #44105, #3575, #17855, #38119, #58775, #12858, #53447, #29151, #2908, #23168, #54086, #8208, #28474, #18842, #34107, #3230, #43780, #64056 ),
 .UNSPECIFIED., .F., .F.,
 ( 4, 3, 3, 3, 3, 3, 4 ),
 ( 6.829613154537258970E-18, 2.825908398831227493E-05, 4.208813692483927239E-05, 5.591713746943774302E-05, 6.279584083231731729E-05, 9.105792820296498889E-05, 0.0001153131102488858250 ),
 .UNSPECIFIED. ) ;
#61398 = EDGE_LOOP ( 'NONE', ( #46755, #25945, #39251, #3191 ) ) ;
#61399 = CARTESIAN_POINT ( 'NONE',  ( 22.64436338924570080, -10.50028284738791839, -5.818370998278716399 ) ) ;
#61400 = LINE ( 'NONE', #50141, #55434 ) ;
#61401 = CARTESIAN_POINT ( 'NONE',  ( -27.08506889328343803, 2.284141197253897193, -0.2104793012480347114 ) ) ;
#61402 = CARTESIAN_POINT ( 'NONE',  ( 37.00000000000000711, 11.72195762423409704, 0.7536123767498881243 ) ) ;
#61403 = DIRECTION ( 'NONE',  ( 0.000000000000000000, -1.000000000000000000, 0.000000000000000000 ) ) ;
#61404 = CARTESIAN_POINT ( 'NONE',  ( -36.00000000000000711, 5.710938531231713355, 11.39945968423473666 ) ) ;
#61405 = ADVANCED_FACE ( 'NONE', ( #18482 ), #29404, .T. ) ;
#61406 = CARTESIAN_POINT ( 'NONE',  ( 35.00000000000000000, 7.110831038798420600, 9.896810808925309288 ) ) ;
#61407 = VERTEX_POINT ( 'NONE', #13449 ) ;
#61408 = DIRECTION ( 'NONE',  ( -1.000000000000000000, 0.000000000000000000, 0.000000000000000000 ) ) ;
#61409 = CIRCLE ( 'NONE', #1957, 12.18650000000000233 ) ;
#61410 = CARTESIAN_POINT ( 'NONE',  ( 22.22111349864275809, 11.93717068860222774, -1.276428617110490382 ) ) ;
#61411 = CARTESIAN_POINT ( 'NONE',  ( -37.00000000000000711, 11.91791701451266405, 2.544412758415886877 ) ) ;
#61412 = CARTESIAN_POINT ( 'NONE',  ( 5.516018279890452902, 0.005042957932159071975, 0.004525000489649949435 ) ) ;
#61413 = CARTESIAN_POINT ( 'NONE',  ( -25.00000000000000355, -9.999999999999998224, 5.000000000000002665 ) ) ;
#61414 = DIRECTION ( 'NONE',  ( 0.000000000000000000, 0.01356324068817998073, -0.9999080150203990547 ) ) ;
#61415 = LINE ( 'NONE', #22093, #17501 ) ;
#61416 = CARTESIAN_POINT ( 'NONE',  ( 0.3675815128205894289, 9.574637318041965273, 7.689697408877307794 ) ) ;
#61417 = AXIS2_PLACEMENT_3D ( 'NONE', #23907, #53516, #54487 ) ;
#61418 = VERTEX_POINT ( 'NONE', #33732 ) ;
#61419 = ORIENTED_EDGE ( 'NONE', *, *, #40574, .F. ) ;
#61420 = DIRECTION ( 'NONE',  ( -1.000000000000000000, 0.000000000000000000, 0.000000000000000000 ) ) ;
#61421 = AXIS2_PLACEMENT_3D ( 'NONE', #25539, #10562, #56122 ) ;
#61422 = VECTOR ( 'NONE', #46682, 1000.000000000000000 ) ;
#61423 = VERTEX_POINT ( 'NONE', #27651 ) ;
#61424 = DIRECTION ( 'NONE',  ( -1.000000000000000000, -0.000000000000000000, -0.000000000000000000 ) ) ;
#61425 = CARTESIAN_POINT ( 'NONE',  ( 2.298277635560284526, 4.791911337974176455, 5.967558917212159031 ) ) ;
#61426 = CARTESIAN_POINT ( 'NONE',  ( 2.244591118396414675, 2.510215291309781271, -7.211060161907408173 ) ) ;
#61427 = VERTEX_POINT ( 'NONE', #58607 ) ;
#61428 = CARTESIAN_POINT ( 'NONE',  ( -35.04582288351658548, -0.01092946910274502324, 0.006479247284604020517 ) ) ;
#61429 = CYLINDRICAL_SURFACE ( 'NONE', #58738, 12.18649999999999878 ) ;
#61430 = CARTESIAN_POINT ( 'NONE',  ( 35.00000000000000000, -6.946017217730008575, -10.01317267707884184 ) ) ;
#61431 = CIRCLE ( 'NONE', #24282, 7.499999999999988454 ) ;
#61432 = FACE_OUTER_BOUND ( 'NONE', #155, .T. ) ;
#61433 = ADVANCED_FACE ( 'NONE', ( #32961 ), #57944, .T. ) ;
#61434 = DIRECTION ( 'NONE',  ( -1.000000000000000000, 0.000000000000000000, 0.000000000000000000 ) ) ;
#61435 = CARTESIAN_POINT ( 'NONE',  ( 2.260457164927186291, 2.742969430850518808, 7.131443009846811343 ) ) ;
#61436 = VERTEX_POINT ( 'NONE', #8056 ) ;
#61437 = DIRECTION ( 'NONE',  ( -1.000000000000000000, 0.000000000000000000, 0.000000000000000000 ) ) ;
#61438 = ORIENTED_EDGE ( 'NONE', *, *, #55567, .F. ) ;
#61439 = CARTESIAN_POINT ( 'NONE',  ( 35.00000000000000000, 4.705694406421931860E-17, -3.469127814946512892E-15 ) ) ;
#61440 = CARTESIAN_POINT ( 'NONE',  ( -35.00000000000000000, 0.000000000000000000, 0.000000000000000000 ) ) ;
#61441 = CARTESIAN_POINT ( 'NONE',  ( 27.76533532700122464, -10.82083892906157629, 5.202369787004509583 ) ) ;
#61442 = DIRECTION ( 'NONE',  ( 0.000000000000000000, -0.9868265225415276953, 0.1617819965527552140 ) ) ;
#61443 = AXIS2_PLACEMENT_3D ( 'NONE', #18363, #59244, #38625 ) ;
#61444 = ADVANCED_FACE ( 'NONE', ( #27327 ), #47622, .T. ) ;
#61445 = ORIENTED_EDGE ( 'NONE', *, *, #56803, .T. ) ;
#61446 = ORIENTED_EDGE ( 'NONE', *, *, #2199, .F. ) ;
#61447 = CARTESIAN_POINT ( 'NONE',  ( 2.000000000000001776, -6.662861565602071323, 1.421313227905616650 ) ) ;
#61448 = ORIENTED_EDGE ( 'NONE', *, *, #13063, .T. ) ;
#61449 = CARTESIAN_POINT ( 'NONE',  ( -35.00000000000000000, 0.000000000000000000, 0.000000000000000000 ) ) ;
#61450 = CARTESIAN_POINT ( 'NONE',  ( 0.000000000000000000, -1.734723475976807094E-15, -13.50000000000000178 ) ) ;
#61451 = CARTESIAN_POINT ( 'NONE',  ( 1.719304012338199517, 0.000000000000000000, 0.000000000000000000 ) ) ;
#61452 = CARTESIAN_POINT ( 'NONE',  ( -27.10719052120871098, 1.962717903527675611, -1.310802520592017295 ) ) ;
#61454 = CARTESIAN_POINT ( 'NONE',  ( 0.000000000000000000, 3.673940397442060361E-16, 3.000000000000000444 ) ) ;
#61453 = CIRCLE ( 'NONE', #6329, 12.18650000000000055 ) ;
#61455 = EDGE_CURVE ( 'NONE', #8359, #36589, #43600, .T. ) ;
#61456 = CARTESIAN_POINT ( 'NONE',  ( 0.7446945582530694052, 10.91757157182845717, -5.891988114923994324 ) ) ;
#61457 = CARTESIAN_POINT ( 'NONE',  ( 1.020182472826105746, 12.37761526492893083, -1.729367949133470361 ) ) ;
#61458 = ORIENTED_EDGE ( 'NONE', *, *, #12852, .T. ) ;
#61459 = ADVANCED_FACE ( 'NONE', ( #52935 ), #37962, .T. ) ;
#61460 = CARTESIAN_POINT ( 'NONE',  ( 2.963017218115631568, -2.328652339224295709, -7.522800244854603413 ) ) ;
#61461 = ORIENTED_EDGE ( 'NONE', *, *, #9083, .T. ) ;
#61462 = DIRECTION ( 'NONE',  ( 0.000000000000000000, -0.4198891015602715382, 0.9075754196709537869 ) ) ;
#61463 = CARTESIAN_POINT ( 'NONE',  ( 0.3164563675027640133, -9.237806174449815444, 8.065346584422218967 ) ) ;
#61464 = AXIS2_PLACEMENT_3D ( 'NONE', #52330, #62273, #11408 ) ;
#61465 = CARTESIAN_POINT ( 'NONE',  ( 17.86670421114028073, 9.033888303652016560, 10.06012754632461004 ) ) ;
#61466 = ORIENTED_EDGE ( 'NONE', *, *, #16552, .F. ) ;
#61467 = CARTESIAN_POINT ( 'NONE',  ( -22.27706485742869091, 3.662257305743817692, -0.3729136217355926153 ) ) ;
#61469 = EDGE_LOOP ( 'NONE', ( #994, #43836, #9591, #65609 ) ) ;
#61468 = VECTOR ( 'NONE', #59256, 1000.000000000000000 ) ;
#61470 = DIRECTION ( 'NONE',  ( -0.000000000000000000, -1.000000000000000000, -0.000000000000000000 ) ) ;
#61471 = FACE_OUTER_BOUND ( 'NONE', #30924, .T. ) ;
#61473 = EDGE_CURVE ( 'NONE', #32620, #45080, #4525, .T. ) ;
#61472 = DIRECTION ( 'NONE',  ( 0.000000000000000000, 0.000000000000000000, -1.000000000000000000 ) ) ;
#61474 = CARTESIAN_POINT ( 'NONE',  ( -48.84424248505261090, -0.2332870993691606720, 3.158587530951954658 ) ) ;
#61475 = ORIENTED_EDGE ( 'NONE', *, *, #5418, .F. ) ;
#61476 = ORIENTED_EDGE ( 'NONE', *, *, #55787, .T. ) ;
#61477 = AXIS2_PLACEMENT_3D ( 'NONE', #997, #15935, #37206 ) ;
#61478 = DIRECTION ( 'NONE',  ( 0.000000000000000000, 0.01356324068817998940, -0.9999080150203990547 ) ) ;
#61480 = VERTEX_POINT ( 'NONE', #28323 ) ;
#61479 = ADVANCED_FACE ( 'NONE', ( #48620 ), #22691, .T. ) ;
#61481 = CARTESIAN_POINT ( 'NONE',  ( 0.3675815128205894289, -11.62724744438063063, -3.951233083390586209 ) ) ;
#61482 = ORIENTED_EDGE ( 'NONE', *, *, #37051, .F. ) ;
#61483 = EDGE_LOOP ( 'NONE', ( #61198, #16243, #47068, #51854 ) ) ;
#61484 = CIRCLE ( 'NONE', #32801, 12.73084802173761787 ) ;
#61486 = EDGE_CURVE ( 'NONE', #3067, #44205, #13031, .T. ) ;
#61485 = ORIENTED_EDGE ( 'NONE', *, *, #6213, .T. ) ;
#61487 = CARTESIAN_POINT ( 'NONE',  ( 37.00000000000000711, 4.705694406421931860E-17, -3.469127814946512892E-15 ) ) ;
#61488 = CARTESIAN_POINT ( 'NONE',  ( 18.79103332550323913, -28.91360719445345140, 6.866334764117086209 ) ) ;
#61489 = FACE_OUTER_BOUND ( 'NONE', #34073, .T. ) ;
#61490 = CARTESIAN_POINT ( 'NONE',  ( -27.10719052120871098, 1.044362304621487825, -2.116547233941206585 ) ) ;
#61491 = CARTESIAN_POINT ( 'NONE',  ( 2.305787727787084407, -6.545285700970554288, 3.971363876083942035 ) ) ;
#61492 = ORIENTED_EDGE ( 'NONE', *, *, #53517, .F. ) ;
#61493 = EDGE_CURVE ( 'NONE', #55501, #34288, #59044, .T. ) ;
#61494 = CARTESIAN_POINT ( 'NONE',  ( 2.284126774967169649, -2.466502196989121654, -7.240052432235436264 ) ) ;
#61495 = ORIENTED_EDGE ( 'NONE', *, *, #30239, .F. ) ;
#61496 = DIRECTION ( 'NONE',  ( 1.000000000000000000, 0.000000000000000000, 0.000000000000000000 ) ) ;
#61497 = CARTESIAN_POINT ( 'NONE',  ( -27.08702828306176258, 0.6138566972905430408, 2.216258174335470787 ) ) ;
#61498 = EDGE_CURVE ( 'NONE', #27716, #18175, #58417, .T. ) ;
#61499 = CARTESIAN_POINT ( 'NONE',  ( 2.000000000000001776, 0.000000000000000000, 0.000000000000000000 ) ) ;
#61500 = CARTESIAN_POINT ( 'NONE',  ( 0.2833330754217371905, -2.326361469893312606, 12.02930703389099598 ) ) ;
#61501 = CARTESIAN_POINT ( 'NONE',  ( 29.21915657715117121, 6.866533784549974762, 9.851962652288564826 ) ) ;
#61502 = LINE ( 'NONE', #52546, #24902 ) ;
#61503 = AXIS2_PLACEMENT_3D ( 'NONE', #15318, #56891, #51577 ) ;
#61504 = VERTEX_POINT ( 'NONE', #43272 ) ;
#61505 = DIRECTION ( 'NONE',  ( -1.000000000000000000, 0.000000000000000000, 0.000000000000000000 ) ) ;
#61506 = VECTOR ( 'NONE', #27992, 1000.000000000000000 ) ;
#61507 = ORIENTED_EDGE ( 'NONE', *, *, #16922, .F. ) ;
#61508 = CARTESIAN_POINT ( 'NONE',  ( -10.95212338237647920, -9.902220863987562183, -6.778349501228825069 ) ) ;
#61509 = CARTESIAN_POINT ( 'NONE',  ( -35.00000000000000000, -3.640372113593638215, 12.21925492305360983 ) ) ;
#61510 = CARTESIAN_POINT ( 'NONE',  ( 19.42209513767211249, -29.99999999999998934, 5.494601501491730211 ) ) ;
#61511 = DIRECTION ( 'NONE',  ( 0.000000000000000000, -0.01356324068817998940, 0.9999080150203990547 ) ) ;
#61512 = DIRECTION ( 'NONE',  ( 1.000000000000000000, -0.000000000000000000, 0.000000000000000000 ) ) ;
#61513 = ORIENTED_EDGE ( 'NONE', *, *, #48405, .T. ) ;
#61514 = CARTESIAN_POINT ( 'NONE',  ( 35.00000000000000000, 6.280308599560279426, 9.926225166346956286 ) ) ;
#61515 = CARTESIAN_POINT ( 'NONE',  ( -35.00000000000000000, 4.018060380616562455, -11.50504120060938718 ) ) ;
#61516 = CARTESIAN_POINT ( 'NONE',  ( 35.00000000000000000, 4.946702696913328090, 11.13736569743268845 ) ) ;
#61517 = CARTESIAN_POINT ( 'NONE',  ( 24.44374455839395921, -11.03111509265887591, -7.786461916442146247 ) ) ;
#61518 = CIRCLE ( 'NONE', #967, 4.999999999999999112 ) ;
#61519 = EDGE_CURVE ( 'NONE', #62927, #55740, #19368, .T. ) ;
#61520 = CIRCLE ( 'NONE', #9482, 12.74999999999999822 ) ;
#61521 = LINE ( 'NONE', #30942, #62632 ) ;
#61522 = DIRECTION ( 'NONE',  ( 0.000000000000000000, -0.9937233664769772323, 0.1118654143051511785 ) ) ;
#61523 = CARTESIAN_POINT ( 'NONE',  ( 5.536195898058073439, -0.0002547682446687435961, 0.008496323383586254843 ) ) ;
#61524 = CARTESIAN_POINT ( 'NONE',  ( -27.08419642509982950, 1.697757994346406951, -1.538761233743668910 ) ) ;
#61525 = DIRECTION ( 'NONE',  ( 0.000000000000000000, -0.1740410799127471153, -0.9847383929261642743 ) ) ;
#61526 = EDGE_CURVE ( 'NONE', #6547, #25804, #38629, .T. ) ;
#61527 = AXIS2_PLACEMENT_3D ( 'NONE', #5310, #56162, #45215 ) ;
#61528 = ORIENTED_EDGE ( 'NONE', *, *, #31797, .F. ) ;
#61529 =( BOUNDED_CURVE ( )  B_SPLINE_CURVE ( 3, ( #15577, #11264, #50530, #55838 ),
 .UNSPECIFIED., .F., .F. ) 
 B_SPLINE_CURVE_WITH_KNOTS ( ( 4, 4 ),
 ( 5.368938899291405775, 5.390737220995221790 ),
 .UNSPECIFIED. ) 
 CURVE ( )  GEOMETRIC_REPRESENTATION_ITEM ( )  RATIONAL_B_SPLINE_CURVE ( ( 1.000000000000000000, 0.9999604031562251416, 0.9999604031562251416, 1.000000000000000000 ) ) 
 REPRESENTATION_ITEM ( '' )  );
#61530 = ORIENTED_EDGE ( 'NONE', *, *, #31834, .T. ) ;
#61531 = CARTESIAN_POINT ( 'NONE',  ( 37.00000000000000711, 4.705694406421931860E-17, -3.469127814946512892E-15 ) ) ;
#61532 = CARTESIAN_POINT ( 'NONE',  ( 48.84659035979348829, -0.2326159177123071076, 2.738175293146158928 ) ) ;
#61533 = CARTESIAN_POINT ( 'NONE',  ( 35.00000000000000000, 10.07641281632177588, -6.036400161834603928 ) ) ;
#61534 = DIRECTION ( 'NONE',  ( -1.000000000000000000, 0.000000000000000000, 0.000000000000000000 ) ) ;
#61535 = ORIENTED_EDGE ( 'NONE', *, *, #10217, .T. ) ;
#61536 = EDGE_CURVE ( 'NONE', #63186, #28450, #23648, .T. ) ;
#61537 = ORIENTED_EDGE ( 'NONE', *, *, #31598, .F. ) ;
#61538 = ORIENTED_EDGE ( 'NONE', *, *, #65363, .F. ) ;
#61539 = DIRECTION ( 'NONE',  ( 1.000000000000000000, 0.000000000000000000, 0.000000000000000000 ) ) ;
#61541 = CARTESIAN_POINT ( 'NONE',  ( 37.00000000000000711, 9.752226076388984310, 6.547236723513913503 ) ) ;
#61540 = AXIS2_PLACEMENT_3D ( 'NONE', #40497, #16219, #25208 ) ;
#61542 = VECTOR ( 'NONE', #65735, 1000.000000000000000 ) ;
#61543 = ORIENTED_EDGE ( 'NONE', *, *, #34295, .F. ) ;
#61544 = CARTESIAN_POINT ( 'NONE',  ( 6.511276587883018330, -4.283181266385642338, 12.80273922584868629 ) ) ;
#61545 = CARTESIAN_POINT ( 'NONE',  ( -35.00000000000000000, 11.07407352312212723, 3.916263239775389149 ) ) ;
#61546 = EDGE_LOOP ( 'NONE', ( #48778, #14280, #48018, #3023 ) ) ;
#61547 = DIRECTION ( 'NONE',  ( -1.000000000000000000, -0.000000000000000000, 0.000000000000000000 ) ) ;
#61548 = CONICAL_SURFACE ( 'NONE', #49901, 2.214855479030549468, 1.249045772030607848 ) ;
#61549 = CARTESIAN_POINT ( 'NONE',  ( 12.39041149895467875, -29.91764912108168417, -8.475516454291387447 ) ) ;
#61550 = CARTESIAN_POINT ( 'NONE',  ( 2.258463476537673653, 7.131741622455168184, 2.740340677912665335 ) ) ;
#61551 = ORIENTED_EDGE ( 'NONE', *, *, #13358, .T. ) ;
#61552 = LINE ( 'NONE', #35941, #25646 ) ;
#61553 = VERTEX_POINT ( 'NONE', #49530 ) ;
#61554 = FACE_OUTER_BOUND ( 'NONE', #3430, .T. ) ;
#61555 = ORIENTED_EDGE ( 'NONE', *, *, #39665, .T. ) ;
#61556 = DIRECTION ( 'NONE',  ( 0.000000000000000000, -0.01356324068817998940, 0.9999080150203990547 ) ) ;
#61557 = EDGE_CURVE ( 'NONE', #22685, #44279, #22546, .T. ) ;
#61558 = DIRECTION ( 'NONE',  ( 0.000000000000000000, 0.2618041379715635442, -0.9651210252299794456 ) ) ;
#61559 = CARTESIAN_POINT ( 'NONE',  ( 1.719304012338820131, 1.452142814150020556, 12.64775761152757561 ) ) ;
#61560 = CARTESIAN_POINT ( 'NONE',  ( -22.59969328935886423, -3.618004136135291038, -2.921971394153373591 ) ) ;
#61561 = B_SPLINE_CURVE_WITH_KNOTS ( 'NONE', 3,
 ( #51588, #12527, #31595, #26294, #46908, #63725, #48795, #56563 ),
 .UNSPECIFIED., .F., .F.,
 ( 4, 2, 2, 4 ),
 ( 0.004035003267135223344, 0.006329346555864282138, 0.007476518200228814137, 0.008623689844593347004 ),
 .UNSPECIFIED. ) ;
#61562 = CARTESIAN_POINT ( 'NONE',  ( -7.489022030332961322, 5.127957880411581293, -10.84914964302385521 ) ) ;
#61563 = CARTESIAN_POINT ( 'NONE',  ( 3.152665057734127529, -7.281573230474269742, -3.161213418913537687 ) ) ;
#61564 = CARTESIAN_POINT ( 'NONE',  ( -27.08426571771018487, 2.277536580310463243, -0.2528330215897251487 ) ) ;
#61565 = CARTESIAN_POINT ( 'NONE',  ( 0.2650492594609232810, 4.084774262246084753, 11.54478160586238644 ) ) ;
#61567 = VERTEX_POINT ( 'NONE', #12952 ) ;
#61566 = CARTESIAN_POINT ( 'NONE',  ( -17.68536118190054651, 2.866363609320780270, -13.19378535958787069 ) ) ;
#61568 = EDGE_CURVE ( 'NONE', #40799, #40241, #3968, .T. ) ;
#61569 = CIRCLE ( 'NONE', #62599, 5.000000000000000000 ) ;
#61570 = DIRECTION ( 'NONE',  ( 1.000000000000000000, 0.000000000000000000, 0.000000000000000000 ) ) ;
#61571 = VERTEX_POINT ( 'NONE', #53195 ) ;
#61572 = CARTESIAN_POINT ( 'NONE',  ( 2.241352910868908754, 3.744764251556992996, 6.652881166698525028 ) ) ;
#61573 = CARTESIAN_POINT ( 'NONE',  ( 37.00000000000000711, -11.29812557209478996, -3.213188559034203529 ) ) ;
#61574 = ADVANCED_FACE ( 'NONE', ( #64152 ), #24654, .F. ) ;
#61575 = ORIENTED_EDGE ( 'NONE', *, *, #28327, .T. ) ;
#61576 = CARTESIAN_POINT ( 'NONE',  ( 37.00000000000000711, 4.705694406421931860E-17, -3.469127814946512892E-15 ) ) ;
#61577 = DIRECTION ( 'NONE',  ( 0.000000000000000000, 0.01356324068817998940, -0.9999080150203990547 ) ) ;
#61578 = AXIS2_PLACEMENT_3D ( 'NONE', #13247, #22906, #43159 ) ;
#61579 = CARTESIAN_POINT ( 'NONE',  ( 0.2653519991613836893, -9.366979519113291630, -7.888569541500616289 ) ) ;
#61580 = DIRECTION ( 'NONE',  ( 0.000000000000000000, 0.000000000000000000, 1.000000000000000000 ) ) ;
#61581 = CARTESIAN_POINT ( 'NONE',  ( -35.00000000000000000, -7.718225330433740261, -9.430788938294131896 ) ) ;
#61582 = ORIENTED_EDGE ( 'NONE', *, *, #34216, .F. ) ;
#61583 = LINE ( 'NONE', #62246, #55549 ) ;
#61584 = ORIENTED_EDGE ( 'NONE', *, *, #29951, .T. ) ;
#61585 = CARTESIAN_POINT ( 'NONE',  ( -37.00000000000000711, 0.000000000000000000, 0.000000000000000000 ) ) ;
#61586 = DIRECTION ( 'NONE',  ( 1.000000000000000000, 0.000000000000000000, 0.000000000000000000 ) ) ;
#61587 = CARTESIAN_POINT ( 'NONE',  ( -35.00000000000000000, 0.000000000000000000, 0.000000000000000000 ) ) ;
#61588 = VERTEX_POINT ( 'NONE', #43200 ) ;
#61589 = CARTESIAN_POINT ( 'NONE',  ( -27.08506889328327816, -0.9597901767732647249, 2.083363953276908376 ) ) ;
#61590 = EDGE_CURVE ( 'NONE', #3506, #48302, #59714, .T. ) ;
#61591 = AXIS2_PLACEMENT_3D ( 'NONE', #35151, #21185, #25194 ) ;
#61592 = ADVANCED_FACE ( 'NONE', ( #44192 ), #63475, .T. ) ;
#61593 = CARTESIAN_POINT ( 'NONE',  ( -35.04834644901396956, 0.01306875526353248884, -0.004537648929138059922 ) ) ;
#61594 = CARTESIAN_POINT ( 'NONE',  ( 0.000000000000000000, 6.812627895098307462, 2.855765430652722259 ) ) ;
#61595 = CARTESIAN_POINT ( 'NONE',  ( 37.00000000000000711, 4.705694406421931860E-17, -3.469127814946512892E-15 ) ) ;
#61596 = CARTESIAN_POINT ( 'NONE',  ( 0.3675815128205894289, -5.910255304480370953, -10.76447900494946452 ) ) ;
#61597 = CARTESIAN_POINT ( 'NONE',  ( 0.2646305136544072623, 4.064188116014551433, 11.55263159009959928 ) ) ;
#61598 = CARTESIAN_POINT ( 'NONE',  ( 4.308196110052892319E-12, -30.53649492335491189, 15.30974548841782656 ) ) ;
#61599 = DIRECTION ( 'NONE',  ( 0.000000000000000000, -0.01356324068817999114, 0.9999080150203989437 ) ) ;
#61600 = EDGE_CURVE ( 'NONE', #58586, #16833, #6660, .T. ) ;
#61601 = ORIENTED_EDGE ( 'NONE', *, *, #34332, .T. ) ;
#61602 = CARTESIAN_POINT ( 'NONE',  ( -16.15337078595565501, 7.823288771779902007, 11.00216753322003704 ) ) ;
#61603 = DIRECTION ( 'NONE',  ( 0.000000000000000000, 1.000000000000000000, 0.000000000000000000 ) ) ;
#61604 = CIRCLE ( 'NONE', #22311, 5.000000000000000000 ) ;
#61605 = ORIENTED_EDGE ( 'NONE', *, *, #1987, .F. ) ;
#61606 = LINE ( 'NONE', #46998, #7732 ) ;
#61607 = CARTESIAN_POINT ( 'NONE',  ( 3.485421372826590591, 6.960100877362279448, -9.812747699357830200 ) ) ;
#61608 = CARTESIAN_POINT ( 'NONE',  ( -22.30861784526116054, 3.620936716852761084, -1.070462554923803378 ) ) ;
#61609 = EDGE_LOOP ( 'NONE', ( #46378, #55674, #54928, #63102 ) ) ;
#61610 = CARTESIAN_POINT ( 'NONE',  ( 5.514970785353741078, -0.004713149585127533042, 0.0003039746380528807537 ) ) ;
#61611 = DIRECTION ( 'NONE',  ( -0.000000000000000000, -0.000000000000000000, -1.000000000000000000 ) ) ;
#61612 = VERTEX_POINT ( 'NONE', #7642 ) ;
#61613 = EDGE_CURVE ( 'NONE', #3310, #19106, #15697, .T. ) ;
#61614 = EDGE_CURVE ( 'NONE', #64143, #13395, #10858, .T. ) ;
#61615 = CIRCLE ( 'NONE', #4300, 5.000000000000000888 ) ;
#61616 = CARTESIAN_POINT ( 'NONE',  ( 35.00000000000000000, 11.35427606708806003, -4.426194442447284771 ) ) ;
#61617 = ORIENTED_EDGE ( 'NONE', *, *, #7520, .T. ) ;
#61618 = VERTEX_POINT ( 'NONE', #48869 ) ;
#61619 = EDGE_CURVE ( 'NONE', #65138, #53550, #48037, .T. ) ;
#61620 = CARTESIAN_POINT ( 'NONE',  ( 2.305787727787083519, 1.493241775258524084, -7.508843116234142911 ) ) ;
#61621 = VERTEX_POINT ( 'NONE', #28252 ) ;
#61622 = DIRECTION ( 'NONE',  ( 0.000000000000000000, 1.000000000000000000, 0.000000000000000000 ) ) ;
#61623 = CARTESIAN_POINT ( 'NONE',  ( 5.514970785353741078, 0.004532877335078317783, -0.001326349372336594603 ) ) ;
#61624 = CARTESIAN_POINT ( 'NONE',  ( 36.00000000000000711, -4.983891302653661981, -11.73555825188274682 ) ) ;
#61625 = AXIS2_PLACEMENT_3D ( 'NONE', #46439, #63602, #13083 ) ;
#61626 = CARTESIAN_POINT ( 'NONE',  ( 10.47337281987918267, 7.645786758740480415, 9.252117967043277602 ) ) ;
#61627 = ORIENTED_EDGE ( 'NONE', *, *, #17547, .F. ) ;
#61628 = CARTESIAN_POINT ( 'NONE',  ( 5.515539859299206427, -0.005751553894235456911, -0.001886660928063758945 ) ) ;
#61629 = CARTESIAN_POINT ( 'NONE',  ( 4.699914177767785084, -28.11199977926868598, 11.88398404624164506 ) ) ;
#61630 = CARTESIAN_POINT ( 'NONE',  ( 3.031336079629839197, -7.886784934834946803, 0.4165536638494340416 ) ) ;
#61632 = ORIENTED_EDGE ( 'NONE', *, *, #13397, .T. ) ;
#61631 = CARTESIAN_POINT ( 'NONE',  ( 0.2653141334712562083, -12.06772877558522516, -2.083134085643168820 ) ) ;
#61634 = AXIS2_PLACEMENT_3D ( 'NONE', #59685, #33738, #27775 ) ;
#61633 = DIRECTION ( 'NONE',  ( 0.000000000000000000, -0.01356324068817998940, 0.9999080150203990547 ) ) ;
#61635 = ORIENTED_EDGE ( 'NONE', *, *, #41975, .T. ) ;
#61636 = CARTESIAN_POINT ( 'NONE',  ( 37.00000000000000711, -5.672855678558609505, 10.28547182238013669 ) ) ;
#61637 = ORIENTED_EDGE ( 'NONE', *, *, #47403, .F. ) ;
#61638 = ORIENTED_EDGE ( 'NONE', *, *, #62730, .T. ) ;
#61639 = DIRECTION ( 'NONE',  ( 0.000000000000000000, 1.000000000000000000, 0.000000000000000000 ) ) ;
#61640 = DIRECTION ( 'NONE',  ( -1.000000000000000000, 0.000000000000000000, 0.000000000000000000 ) ) ;
#61641 = EDGE_CURVE ( 'NONE', #51910, #55560, #29981, .T. ) ;
#61642 = DIRECTION ( 'NONE',  ( 1.000000000000000000, 0.000000000000000000, 0.000000000000000000 ) ) ;
#61643 = VECTOR ( 'NONE', #43444, 1000.000000000000000 ) ;
#61644 = EDGE_LOOP ( 'NONE', ( #5853, #22797, #39441, #61144 ) ) ;
#61645 = CIRCLE ( 'NONE', #38235, 12.18649999999999878 ) ;
#61647 = AXIS2_PLACEMENT_3D ( 'NONE', #49861, #34227, #38904 ) ;
#61646 = CARTESIAN_POINT ( 'NONE',  ( 2.440552418640498988, 7.615619946579186283, -1.142369876085246316 ) ) ;
#61648 = CARTESIAN_POINT ( 'NONE',  ( 10.48620311856346454, 8.250315036047107142, 8.713914264323181058 ) ) ;
#61649 = CARTESIAN_POINT ( 'NONE',  ( -17.97077823246242900, -9.629623312810577929, -9.462431742398621282 ) ) ;
#61650 = VERTEX_POINT ( 'NONE', #44498 ) ;
#61651 = EDGE_CURVE ( 'NONE', #18427, #29827, #13286, .T. ) ;
#61652 = EDGE_LOOP ( 'NONE', ( #47417, #49384, #52523, #55558 ) ) ;
#61653 = CARTESIAN_POINT ( 'NONE',  ( -26.43258404273188589, -2.854888342447764238, -1.987083010659173699 ) ) ;
#61654 = VERTEX_POINT ( 'NONE', #53544 ) ;
#61655 = ORIENTED_EDGE ( 'NONE', *, *, #10751, .T. ) ;
#61656 = DIRECTION ( 'NONE',  ( 0.000000000000000000, 0.9903235168508544017, 0.1387779952735853917 ) ) ;
#61657 = CARTESIAN_POINT ( 'NONE',  ( 1.719304012339844867, -10.62216384465586216, 7.017415949612814785 ) ) ;
#61658 = CARTESIAN_POINT ( 'NONE',  ( 2.827825597296803828, -7.528560921609593670, -4.975864478227487453 ) ) ;
#61659 = CARTESIAN_POINT ( 'NONE',  ( -21.17861794710831091, -13.00977982294134883, -3.604945070120774808 ) ) ;
#61661 = AXIS2_PLACEMENT_3D ( 'NONE', #49639, #4079, #14369 ) ;
#61660 = CARTESIAN_POINT ( 'NONE',  ( 2.000000000000001776, -6.441884263200848615, 2.217201541069723891 ) ) ;
#61662 = VECTOR ( 'NONE', #59021, 1000.000000000000114 ) ;
#61663 = CARTESIAN_POINT ( 'NONE',  ( 0.000000000000000000, 1.754183803416655474, -6.711026108862266248 ) ) ;
#61664 = CARTESIAN_POINT ( 'NONE',  ( -22.27715239060371744, -0.8317362037004212283, -3.586346956688103660 ) ) ;
#61665 = AXIS2_PLACEMENT_3D ( 'NONE', #35071, #49442, #13812 ) ;
#61666 = VERTEX_POINT ( 'NONE', #39191 ) ;
#61667 = CARTESIAN_POINT ( 'NONE',  ( -22.28236030719477512, -3.035028179399219983, 2.111163412226035430 ) ) ;
#61668 = CIRCLE ( 'NONE', #18165, 4.999999999999999112 ) ;
#61669 = FACE_OUTER_BOUND ( 'NONE', #38985, .T. ) ;
#61670 = LINE ( 'NONE', #55386, #17293 ) ;
#61671 = CIRCLE ( 'NONE', #29820, 12.74999999999999822 ) ;
#61672 = EDGE_CURVE ( 'NONE', #36560, #20729, #28262, .T. ) ;
#61673 = CARTESIAN_POINT ( 'NONE',  ( 24.39765525450732753, -1.078022420954182437, -13.46171517445628041 ) ) ;
#61674 = DIRECTION ( 'NONE',  ( -1.000000000000000000, 0.000000000000000000, 0.000000000000000000 ) ) ;
#61675 = CARTESIAN_POINT ( 'NONE',  ( -22.27384469013076185, 2.154627400808035276, 2.985904959940879344 ) ) ;
#61676 = AXIS2_PLACEMENT_3D ( 'NONE', #11172, #62666, #46417 ) ;
#61677 = EDGE_LOOP ( 'NONE', ( #905, #50966, #51819, #4918 ) ) ;
#61678 = DIRECTION ( 'NONE',  ( 0.000000000000000000, -0.01356324068817998940, 0.9999080150203990547 ) ) ;
#61679 = CARTESIAN_POINT ( 'NONE',  ( 0.000000000000000000, 3.073484823194434057, -6.841322316745026555 ) ) ;
#61680 = CARTESIAN_POINT ( 'NONE',  ( 35.00000000000000000, 5.927257550915316919, -10.64792938439757641 ) ) ;
#61681 = VECTOR ( 'NONE', #3831, 1000.000000000000000 ) ;
#61682 = AXIS2_PLACEMENT_3D ( 'NONE', #23166, #43108, #58428 ) ;
#61683 = EDGE_CURVE ( 'NONE', #29429, #47259, #65437, .T. ) ;
#61684 = VECTOR ( 'NONE', #12233, 1000.000000000000000 ) ;
#61685 = CARTESIAN_POINT ( 'NONE',  ( 1.000000000000000888, -7.484036900328550956, 0.4890722589968952150 ) ) ;
#61686 = CARTESIAN_POINT ( 'NONE',  ( 2.556980015514025872, -7.190718924764563980, 2.862731173724000655 ) ) ;
#61687 = ORIENTED_EDGE ( 'NONE', *, *, #34777, .T. ) ;
#61688 = LINE ( 'NONE', #36429, #31236 ) ;
#61689 = DIRECTION ( 'NONE',  ( 0.000000000000000000, -0.1387779952735886391, 0.9903235168508540687 ) ) ;
#61690 = CARTESIAN_POINT ( 'NONE',  ( 2.241352910868908754, 1.243507963608094347, 7.532448145350512547 ) ) ;
#61691 = EDGE_LOOP ( 'NONE', ( #57641, #44287, #47636, #49411 ) ) ;
#61692 = CARTESIAN_POINT ( 'NONE',  ( -28.85619398320021745, 3.750539801530000439, -12.96855624952673836 ) ) ;
#61693 = DIRECTION ( 'NONE',  ( -1.000000000000000000, 0.000000000000000000, -0.000000000000000000 ) ) ;
#61694 = FACE_OUTER_BOUND ( 'NONE', #14428, .T. ) ;
#61695 = EDGE_CURVE ( 'NONE', #58669, #38796, #40575, .T. ) ;
#61697 = ORIENTED_EDGE ( 'NONE', *, *, #29798, .T. ) ;
#61696 = FACE_OUTER_BOUND ( 'NONE', #1320, .T. ) ;
#61698 = DIRECTION ( 'NONE',  ( 1.000000000000000000, -0.000000000000000000, -0.000000000000000000 ) ) ;
#61699 = AXIS2_PLACEMENT_3D ( 'NONE', #39146, #19547, #39477 ) ;
#61700 = CIRCLE ( 'NONE', #53277, 12.75000000000000178 ) ;
#61701 = CARTESIAN_POINT ( 'NONE',  ( 5.514624014163232779, -0.002529391395135029055, 0.003278974416024975358 ) ) ;
#61702 = ORIENTED_EDGE ( 'NONE', *, *, #22467, .T. ) ;
#61703 = AXIS2_PLACEMENT_3D ( 'NONE', #62825, #52556, #57535 ) ;
#61704 = DIRECTION ( 'NONE',  ( 0.000000000000000000, -0.3218879778916040602, 0.9467777615094549182 ) ) ;
#61705 = CARTESIAN_POINT ( 'NONE',  ( -37.00000000000000711, 0.000000000000000000, 0.000000000000000000 ) ) ;
#61706 = CARTESIAN_POINT ( 'NONE',  ( 24.18338352651159084, -2.157158703131657695, -11.80984941100301810 ) ) ;
#61707 = CARTESIAN_POINT ( 'NONE',  ( 2.000000000000001776, 0.000000000000000000, 0.000000000000000000 ) ) ;
#61708 = CARTESIAN_POINT ( 'NONE',  ( -9.632141019976685925, 11.15750179195580394, -4.437120446396224160 ) ) ;
#61709 = CIRCLE ( 'NONE', #18265, 6.936499999999991672 ) ;
#61710 = DIRECTION ( 'NONE',  ( -1.000000000000000000, 0.000000000000000000, 0.000000000000000000 ) ) ;
#61712 = ORIENTED_EDGE ( 'NONE', *, *, #22042, .F. ) ;
#61711 = CARTESIAN_POINT ( 'NONE',  ( -37.00000000000000711, -7.110831038798204773, -9.896810808925470937 ) ) ;
#61713 = ORIENTED_EDGE ( 'NONE', *, *, #58816, .T. ) ;
#61714 = CARTESIAN_POINT ( 'NONE',  ( 37.00000000000000711, 11.30684963584395675, 4.545979934229284147 ) ) ;
#61715 = VECTOR ( 'NONE', #44808, 1000.000000000000000 ) ;
#61716 = EDGE_LOOP ( 'NONE', ( #22578, #41193, #20747, #15599 ) ) ;
#61717 = SURFACE_STYLE_FILL_AREA ( #35466 ) ;
#61718 = CARTESIAN_POINT ( 'NONE',  ( -35.00000000000000000, 12.09831040184926287, -1.463443770872647542 ) ) ;
#61719 = EDGE_CURVE ( 'NONE', #59375, #41165, #45907, .T. ) ;
#61720 = CARTESIAN_POINT ( 'NONE',  ( -18.06493064879303034, 4.742646137938961282, 11.02526057695991923 ) ) ;
#61721 = LINE ( 'NONE', #57403, #28816 ) ;
#61722 = ORIENTED_EDGE ( 'NONE', *, *, #44579, .T. ) ;
#61723 = CIRCLE ( 'NONE', #30964, 6.936499999999989008 ) ;
#61724 = CARTESIAN_POINT ( 'NONE',  ( -10.00000000000000178, 0.000000000000000000, 0.000000000000000000 ) ) ;
#61725 = DIRECTION ( 'NONE',  ( -0.000000000000000000, -1.000000000000000000, -0.000000000000000000 ) ) ;
#61726 = VERTEX_POINT ( 'NONE', #34837 ) ;
#61727 = VERTEX_POINT ( 'NONE', #14559 ) ;
#61728 = CARTESIAN_POINT ( 'NONE',  ( 29.14505760361227260, -8.530938414384094060, 10.47125003768023888 ) ) ;
#61729 = AXIS2_PLACEMENT_3D ( 'NONE', #21579, #36850, #51835 ) ;
#61730 = VERTEX_POINT ( 'NONE', #10560 ) ;
#61731 = CARTESIAN_POINT ( 'NONE',  ( 22.48820342141346984, -10.66318017514404914, -5.515879813209774163 ) ) ;
#61732 = DIRECTION ( 'NONE',  ( -1.000000000000000000, 0.000000000000000000, 0.000000000000000000 ) ) ;
#61733 = DIRECTION ( 'NONE',  ( -1.000000000000000000, 0.000000000000000000, 0.000000000000000000 ) ) ;
#61734 = CARTESIAN_POINT ( 'NONE',  ( 0.000000000000000000, 4.976357229393855164, 4.652926418895560801 ) ) ;
#61735 = EDGE_CURVE ( 'NONE', #18185, #16970, #19508, .T. ) ;
#61736 = AXIS2_PLACEMENT_3D ( 'NONE', #32168, #11892, #1931 ) ;
#61737 = AXIS2_PLACEMENT_3D ( 'NONE', #30751, #20472, #65666 ) ;
#61738 = DIRECTION ( 'NONE',  ( 0.000000000000000000, -0.6876994588534139918, -0.7259954919231395021 ) ) ;
#61739 = CARTESIAN_POINT ( 'NONE',  ( 35.00000000000000000, 8.017674001891782254, -9.913596905230143363 ) ) ;
#61740 = CIRCLE ( 'NONE', #43660, 2.899999999999995026 ) ;
#61741 = CARTESIAN_POINT ( 'NONE',  ( 0.000000000000000000, -3.795144977083577675, -6.468916029978841742 ) ) ;
#61742 = ORIENTED_EDGE ( 'NONE', *, *, #29003, .F. ) ;
#61743 =( BOUNDED_SURFACE ( )  B_SPLINE_SURFACE ( 3, 1, ( 
 ( #17220, #21887 ),
 ( #58116, #62751 ),
 ( #53464, #7909 ),
 ( #2922, #42134 ) ),
 .UNSPECIFIED., .F., .F., .F. ) 
 B_SPLINE_SURFACE_WITH_KNOTS ( ( 4, 4 ),
 ( 2, 2 ),
 ( 0.000000000000000000, 1.000000000000000000 ),
 ( 0.000000000000000000, 1.000000000000000000 ),
 .UNSPECIFIED. ) 
 GEOMETRIC_REPRESENTATION_ITEM ( )  RATIONAL_B_SPLINE_SURFACE ( (
 ( 1.000000000000000000, 1.000000000000000000),
 ( 0.9942764183789327692, 0.8450855930916580938),
 ( 0.9942764183789327692, 0.8450855930916580938),
 ( 1.000000000000000000, 1.000000000000000000) ) ) 
 REPRESENTATION_ITEM ( '' )  SURFACE ( )  );
#61744 = CARTESIAN_POINT ( 'NONE',  ( 0.5547464869798262033, 12.33891836761635830, -0.3049355384529440771 ) ) ;
#61745 = CARTESIAN_POINT ( 'NONE',  ( 2.507146904658100972, 4.047319006787570395, -6.577532285019726643 ) ) ;
#61746 = CARTESIAN_POINT ( 'NONE',  ( -27.22214261968804294, 12.41558776886551740, 5.304269109247361058 ) ) ;
#61747 = DIRECTION ( 'NONE',  ( 0.000000000000000000, 0.000000000000000000, 1.000000000000000000 ) ) ;
#61748 = DIRECTION ( 'NONE',  ( 1.000000000000000000, 0.000000000000000000, 0.000000000000000000 ) ) ;
#61749 = CARTESIAN_POINT ( 'NONE',  ( 35.00000000000000000, -11.54110654723647400, 2.185196060784003524 ) ) ;
#61750 = DIRECTION ( 'NONE',  ( -1.000000000000000000, 0.000000000000000000, 0.000000000000000000 ) ) ;
#61751 = CIRCLE ( 'NONE', #33079, 2.899999999999995026 ) ;
#61752 = ORIENTED_EDGE ( 'NONE', *, *, #27654, .F. ) ;
#61753 = EDGE_LOOP ( 'NONE', ( #64058, #51799, #36900, #4547 ) ) ;
#61754 = CARTESIAN_POINT ( 'NONE',  ( 0.000000000000000000, -3.859771122242995123, -5.613913289150092467 ) ) ;
#61755 = CIRCLE ( 'NONE', #18259, 7.938172270156617749 ) ;
#61756 = EDGE_CURVE ( 'NONE', #10568, #55595, #14254, .T. ) ;
#61757 = ORIENTED_EDGE ( 'NONE', *, *, #50336, .F. ) ;
#61758 = EDGE_CURVE ( 'NONE', #31935, #38476, #20566, .T. ) ;
#61759 = CARTESIAN_POINT ( 'NONE',  ( -28.66013792860432119, -1.776574787184029169, 0.4631296695479288905 ) ) ;
#61760 = CARTESIAN_POINT ( 'NONE',  ( 3.152665057734040488, 0.000000000000000000, 0.000000000000000000 ) ) ;
#61761 = AXIS2_PLACEMENT_3D ( 'NONE', #62607, #12079, #42647 ) ;
#61762 = CARTESIAN_POINT ( 'NONE',  ( 1.459561108993782996, -10.08002506399567899, -7.633517148169387312 ) ) ;
#61763 = EDGE_CURVE ( 'NONE', #58057, #38611, #32213, .T. ) ;
#61764 = CARTESIAN_POINT ( 'NONE',  ( 5.516018279890452902, 0.006771744149385740437, 0.0002248006052446895335 ) ) ;
#61765 = VERTEX_POINT ( 'NONE', #54833 ) ;
#61766 = CARTESIAN_POINT ( 'NONE',  ( 5.515188684475870851, -0.0005703990286343194960, -0.005320786921497270075 ) ) ;
#61768 = VECTOR ( 'NONE', #44725, 1000.000000000000000 ) ;
#61767 = CARTESIAN_POINT ( 'NONE',  ( 12.47628546223243617, 0.000000000000000000, 11.99999999999999645 ) ) ;
#61769 = FACE_OUTER_BOUND ( 'NONE', #33536, .T. ) ;
#61770 = CARTESIAN_POINT ( 'NONE',  ( -22.27756824490284515, 2.599719761044746669, 2.608445836294031928 ) ) ;
#61771 = EDGE_CURVE ( 'NONE', #63912, #33199, #5270, .T. ) ;
#61772 = CARTESIAN_POINT ( 'NONE',  ( 12.10998784662220729, -8.443435280036764468, -8.526922110106905706 ) ) ;
#61773 = AXIS2_PLACEMENT_3D ( 'NONE', #49984, #46237, #9088 ) ;
#61774 = CYLINDRICAL_SURFACE ( 'NONE', #20209, 12.18650000000000055 ) ;
#61775 = EDGE_LOOP ( 'NONE', ( #20703, #47484, #57662, #40347 ) ) ;
#61776 = DIRECTION ( 'NONE',  ( 1.000000000000000000, -0.000000000000000000, 0.000000000000000000 ) ) ;
#61777 = ORIENTED_EDGE ( 'NONE', *, *, #45712, .F. ) ;
#61778 = DIRECTION ( 'NONE',  ( 1.000000000000000000, 0.000000000000000000, 0.000000000000000000 ) ) ;
#61779 = DIRECTION ( 'NONE',  ( 0.000000000000000000, -0.01356324068817998940, 0.9999080150203990547 ) ) ;
#61780 = CARTESIAN_POINT ( 'NONE',  ( -47.00000000000000711, 0.000000000000000000, 0.000000000000000000 ) ) ;
#61781 = DIRECTION ( 'NONE',  ( 0.000000000000000000, -0.01356324068817999114, 0.9999080150203989437 ) ) ;
#61782 = B_SPLINE_CURVE_WITH_KNOTS ( 'NONE', 3,
 ( #7938, #28207, #6495, #22781, #52388, #31739, #11787, #32068 ),
 .UNSPECIFIED., .F., .F.,
 ( 4, 2, 2, 4 ),
 ( 0.01146705142166408453, 0.01597709677061665001, 0.01823211944509292928, 0.02048714211956921202 ),
 .UNSPECIFIED. ) ;
#61783 = CARTESIAN_POINT ( 'NONE',  ( -10.66894337560421135, -5.799424265809170365, 10.51297739570658685 ) ) ;
#61784 = AXIS2_PLACEMENT_3D ( 'NONE', #64082, #34135, #34471 ) ;
#61785 = AXIS2_PLACEMENT_3D ( 'NONE', #14729, #55661, #14416 ) ;
#61786 = ORIENTED_EDGE ( 'NONE', *, *, #26763, .T. ) ;
#61787 = ORIENTED_EDGE ( 'NONE', *, *, #6592, .T. ) ;
#61789 = EDGE_CURVE ( 'NONE', #32257, #13767, #65010, .T. ) ;
#61788 = CARTESIAN_POINT ( 'NONE',  ( 5.514970785353741078, -0.0005190732562555385940, 0.004694330894494707501 ) ) ;
#61790 = EDGE_LOOP ( 'NONE', ( #42695, #58912, #22656, #17363 ) ) ;
#61791 = CARTESIAN_POINT ( 'NONE',  ( -27.08418322526031119, -2.265123059255407689, 0.3452258100746847247 ) ) ;
#61792 = DIRECTION ( 'NONE',  ( 1.000000000000000000, -0.000000000000000000, -0.000000000000000000 ) ) ;
#61793 = CYLINDRICAL_SURFACE ( 'NONE', #59657, 6.842778212674966554 ) ;
#61794 = CARTESIAN_POINT ( 'NONE',  ( 2.406456491626151273, -9.571062220821335842, 4.152987573055939130 ) ) ;
#61795 = CARTESIAN_POINT ( 'NONE',  ( -37.00000000000000711, 11.67026961469348123, 4.564151185897115326 ) ) ;
#61796 = CARTESIAN_POINT ( 'NONE',  ( 10.57504247840391010, 8.113525156875745381, -8.843426623829302002 ) ) ;
#61797 = DIRECTION ( 'NONE',  ( -1.000000000000000000, -0.000000000000000000, 0.000000000000000000 ) ) ;
#61798 = EDGE_LOOP ( 'NONE', ( #5313, #15004, #16269, #61446 ) ) ;
#61799 = CARTESIAN_POINT ( 'NONE',  ( 0.6511581176963334716, -10.87850887236078989, 5.898618881004756176 ) ) ;
#61800 = VERTEX_POINT ( 'NONE', #19256 ) ;
#61801 = AXIS2_PLACEMENT_3D ( 'NONE', #62618, #27710, #52682 ) ;
#61802 = CARTESIAN_POINT ( 'NONE',  ( 2.000000000000001776, 6.777474576704068276, 0.6925993764990892032 ) ) ;
#61803 = DIRECTION ( 'NONE',  ( 0.000000000000000000, -0.01356324068817991481, 0.9999080150203990547 ) ) ;
#61804 = ORIENTED_EDGE ( 'NONE', *, *, #13420, .T. ) ;
#61805 = AXIS2_PLACEMENT_3D ( 'NONE', #41976, #36335, #25713 ) ;
#61806 = CARTESIAN_POINT ( 'NONE',  ( -27.09030469827931853, 1.657623467486019075, 1.608164674722569965 ) ) ;
#61807 = CARTESIAN_POINT ( 'NONE',  ( -22.27706485742869091, 3.563814065926677710, -0.9221835209182235316 ) ) ;
#61808 = VERTEX_POINT ( 'NONE', #29534 ) ;
#61809 = CARTESIAN_POINT ( 'NONE',  ( 37.00000000000000711, 4.705694406421931860E-17, -3.469127814946512892E-15 ) ) ;
#61810 = CARTESIAN_POINT ( 'NONE',  ( -12.82483530079958989, -29.99871789793482435, -7.856364084349718446 ) ) ;
#61811 = DIRECTION ( 'NONE',  ( 0.000000000000000000, -0.04924826701375277505, -0.9987865678893272925 ) ) ;
#61812 = EDGE_CURVE ( 'NONE', #26639, #21973, #49838, .T. ) ;
#61813 = ORIENTED_EDGE ( 'NONE', *, *, #1142, .F. ) ;
#61814 = CIRCLE ( 'NONE', #25704, 5.000000000000000000 ) ;
#61815 = ORIENTED_EDGE ( 'NONE', *, *, #11066, .F. ) ;
#61816 = DIRECTION ( 'NONE',  ( -1.000000000000000000, 0.000000000000000000, 0.000000000000000000 ) ) ;
#61817 = B_SPLINE_CURVE_WITH_KNOTS ( 'NONE', 3,
 ( #34514, #13267, #49818, #39831, #33548, #60117, #14538 ),
 .UNSPECIFIED., .F., .F.,
 ( 4, 3, 4 ),
 ( 0.000000000000000000, 0.001700533616330535819, 0.005002426799371335539 ),
 .UNSPECIFIED. ) ;
#61818 = ORIENTED_EDGE ( 'NONE', *, *, #13278, .F. ) ;
#61819 = CARTESIAN_POINT ( 'NONE',  ( 0.2648321136542730048, 11.55519783395232558, -4.054947570138777380 ) ) ;
#61820 = ORIENTED_EDGE ( 'NONE', *, *, #5335, .T. ) ;
#61821 = ORIENTED_EDGE ( 'NONE', *, *, #816, .F. ) ;
#61822 = ORIENTED_EDGE ( 'NONE', *, *, #12034, .F. ) ;
#61823 = CARTESIAN_POINT ( 'NONE',  ( 2.000000000000001776, 2.473437528934240515, -7.080403010454960011 ) ) ;
#61824 = CARTESIAN_POINT ( 'NONE',  ( -16.73721172569806015, -28.43318523521388741, 9.619723400408263458 ) ) ;
#61825 = EDGE_CURVE ( 'NONE', #5002, #56493, #16177, .T. ) ;
#61826 = DIRECTION ( 'NONE',  ( 0.000000000000000000, 0.7790879021242528291, -0.6269146997507959451 ) ) ;
#61827 = CARTESIAN_POINT ( 'NONE',  ( 2.251139882113959434, 2.728563091335249435, -7.133642337268828015 ) ) ;
#61828 = CARTESIAN_POINT ( 'NONE',  ( 37.00000000000000711, 12.02534193257720574, -4.237174932027271801 ) ) ;
#61829 = ORIENTED_EDGE ( 'NONE', *, *, #12366, .T. ) ;
#61830 = CARTESIAN_POINT ( 'NONE',  ( 25.00000000000000355, -9.999999999999998224, 25.00000000000000000 ) ) ;
#61831 = VECTOR ( 'NONE', #57522, 1000.000000000000000 ) ;
#61832 = VERTEX_POINT ( 'NONE', #7212 ) ;
#61833 = DIRECTION ( 'NONE',  ( 0.000000000000000000, 0.01356324068818000848, -0.9999080150203990547 ) ) ;
#61834 = CARTESIAN_POINT ( 'NONE',  ( -3.515176343547850468, 10.77627674567199634, 8.139927681337322696 ) ) ;
#61835 = CYLINDRICAL_SURFACE ( 'NONE', #40604, 19.00000000000000000 ) ;
#61836 = CARTESIAN_POINT ( 'NONE',  ( 0.3160775863651080764, -2.365582350580143878, 12.03278055228170196 ) ) ;
#61837 = CARTESIAN_POINT ( 'NONE',  ( 0.3665391374699467075, -9.237363111276712502, -8.095513416941326312 ) ) ;
#61838 = CARTESIAN_POINT ( 'NONE',  ( 35.00000000000000000, 4.705694406421931860E-17, -3.469127814946512892E-15 ) ) ;
#61839 = AXIS2_PLACEMENT_3D ( 'NONE', #43464, #34145, #49152 ) ;
#61840 = CIRCLE ( 'NONE', #33164, 5.000000000000001776 ) ;
#61841 = EDGE_CURVE ( 'NONE', #51096, #50020, #61884, .T. ) ;
#61842 = EDGE_LOOP ( 'NONE', ( #4249, #5977, #49575, #42550 ) ) ;
#61843 = CARTESIAN_POINT ( 'NONE',  ( -18.08686583997218733, 5.151216734910788908, -10.83812558286602012 ) ) ;
#61844 = ORIENTED_EDGE ( 'NONE', *, *, #34060, .T. ) ;
#61845 = EDGE_CURVE ( 'NONE', #31785, #13407, #10911, .T. ) ;
#61846 = CARTESIAN_POINT ( 'NONE',  ( 0.3632410797595246876, 10.76277061791640399, 5.910360611678860288 ) ) ;
#61847 = PRESENTATION_STYLE_ASSIGNMENT (( #40243 ) ) ;
#61848 = DIRECTION ( 'NONE',  ( -0.3865475372811021382, -0.3335716741247135575, -0.8598319252293152859 ) ) ;
#61849 = CARTESIAN_POINT ( 'NONE',  ( -27.10512513516276911, -0.6711200423626885181, -2.256292013315177591 ) ) ;
#61850 = EDGE_CURVE ( 'NONE', #63179, #53475, #47476, .T. ) ;
#61851 = CARTESIAN_POINT ( 'NONE',  ( -22.70624764888619751, -2.547047087672834387, -4.591418580540065797 ) ) ;
#61852 = ORIENTED_EDGE ( 'NONE', *, *, #17758, .T. ) ;
#61853 = CARTESIAN_POINT ( 'NONE',  ( 2.406456491625782679, 4.662370073864249953, -9.333533259765646406 ) ) ;
#61854 = CARTESIAN_POINT ( 'NONE',  ( 0.2648978790185584908, 2.256510822326303956, -12.03635331166809941 ) ) ;
#61855 = CARTESIAN_POINT ( 'NONE',  ( 2.000000000000001776, 0.000000000000000000, 0.000000000000000000 ) ) ;
#61856 = DIRECTION ( 'NONE',  ( 0.000000000000000000, -0.01356324068817998940, 0.9999080150203990547 ) ) ;
#61857 = CIRCLE ( 'NONE', #39537, 12.18649999999999878 ) ;
#61858 = AXIS2_PLACEMENT_3D ( 'NONE', #18858, #13836, #64708 ) ;
#61859 = EDGE_CURVE ( 'NONE', #2298, #42095, #44111, .T. ) ;
#61860 = CARTESIAN_POINT ( 'NONE',  ( 0.3164563675027630696, 12.26087493884171664, -0.2404665832031822048 ) ) ;
#61861 = CIRCLE ( 'NONE', #49118, 5.000000000000000000 ) ;
#61862 = ADVANCED_FACE ( 'NONE', ( #41470 ), #36507, .T. ) ;
#61863 = CARTESIAN_POINT ( 'NONE',  ( 0.9232058338315058954, -4.617996777200498393, -11.58467545991558367 ) ) ;
#61864 = CARTESIAN_POINT ( 'NONE',  ( 0.9232058338315058954, -11.58467545991557301, 4.617996777200534808 ) ) ;
#61865 = FACE_OUTER_BOUND ( 'NONE', #56424, .T. ) ;
#61866 = CARTESIAN_POINT ( 'NONE',  ( 1.452237505248555660, 7.672309600508830485, -10.06489946308194483 ) ) ;
#61867 = EDGE_CURVE ( 'NONE', #26214, #32335, #33222, .T. ) ;
#61868 = B_SPLINE_CURVE_WITH_KNOTS ( 'NONE', 3,
 ( #63927, #44291, #23713, #3773, #43981, #14031, #64255, #29333, #49328, #23368, #43637, #34322, #18402, #19036, #38981, #24032, #49630, #59277, #54298, #39299, #28039, #48339 ),
 .UNSPECIFIED., .F., .F.,
 ( 4, 3, 3, 3, 3, 3, 3, 4 ),
 ( 0.000000000000000000, 6.990956068646460742E-05, 0.0001398191187764047383, 0.0002097286751720217070, 0.0002796382307041362638, 0.0003495477861619818334, 0.0004194573423310300926, 0.0005586102576332987752 ),
 .UNSPECIFIED. ) ;
#61869 = ORIENTED_EDGE ( 'NONE', *, *, #61619, .F. ) ;
#61870 = EDGE_CURVE ( 'NONE', #58250, #21512, #32156, .T. ) ;
#61871 = CIRCLE ( 'NONE', #7723, 12.75000000000000178 ) ;
#61872 = ORIENTED_EDGE ( 'NONE', *, *, #63421, .T. ) ;
#61873 = CARTESIAN_POINT ( 'NONE',  ( 2.907497136250956515, -6.617189382231103423, 4.235253383576313091 ) ) ;
#61874 = CARTESIAN_POINT ( 'NONE',  ( 26.58564210842044773, -3.638521970294203101, -24.00000000000000711 ) ) ;
#61875 = LINE ( 'NONE', #50927, #38540 ) ;
#61876 = EDGE_CURVE ( 'NONE', #18185, #20267, #39580, .T. ) ;
#61877 = LINE ( 'NONE', #6358, #43473 ) ;
#61878 = ORIENTED_EDGE ( 'NONE', *, *, #59595, .F. ) ;
#61879 = AXIS2_PLACEMENT_3D ( 'NONE', #44670, #64961, #25389 ) ;
#61880 = AXIS2_PLACEMENT_3D ( 'NONE', #53226, #17324, #7673 ) ;
#61881 = ORIENTED_EDGE ( 'NONE', *, *, #16548, .F. ) ;
#61882 = ORIENTED_EDGE ( 'NONE', *, *, #33383, .F. ) ;
#61883 = DIRECTION ( 'NONE',  ( -1.000000000000000000, 0.000000000000000000, 0.000000000000000000 ) ) ;
#61884 = CIRCLE ( 'NONE', #23693, 7.499999999999988454 ) ;
#61886 = VECTOR ( 'NONE', #4399, 1000.000000000000000 ) ;
#61885 = CARTESIAN_POINT ( 'NONE',  ( -22.27721056931765631, 0.7178530073137668888, 3.610969226755180728 ) ) ;
#61887 = ORIENTED_EDGE ( 'NONE', *, *, #51322, .F. ) ;
#61888 = CARTESIAN_POINT ( 'NONE',  ( 37.25000000000000711, -27.56175630915211627, -1.528111002209141978 ) ) ;
#61889 = CARTESIAN_POINT ( 'NONE',  ( 36.00000000000000711, 6.265926637539650734, 11.10408318471052347 ) ) ;
#61890 = ORIENTED_EDGE ( 'NONE', *, *, #2408, .T. ) ;
#61891 = CARTESIAN_POINT ( 'NONE',  ( -19.47984447937493613, -3.750539801530005768, 25.00000000000000000 ) ) ;
#61892 = CARTESIAN_POINT ( 'NONE',  ( 8.372133460183917464, -31.76502814486181592, -13.66429824708577812 ) ) ;
#61893 = CARTESIAN_POINT ( 'NONE',  ( 24.85820284700998428, 0.06691071362158636238, 12.00631040446440778 ) ) ;
#61894 = VERTEX_POINT ( 'NONE', #61767 ) ;
#61895 = CARTESIAN_POINT ( 'NONE',  ( 0.3537226245948401626, 12.13174752084888830, -1.874138792912886764 ) ) ;
#61896 = ORIENTED_EDGE ( 'NONE', *, *, #37899, .T. ) ;
#61897 = CARTESIAN_POINT ( 'NONE',  ( 1.194176325881334932, 7.670099510969203394, -9.940715479868371673 ) ) ;
#61898 = VECTOR ( 'NONE', #50734, 1000.000000000000000 ) ;
#61899 = CARTESIAN_POINT ( 'NONE',  ( 2.241528039335009659, 4.895273998034002538, 5.858435878248524631 ) ) ;
#61900 = CARTESIAN_POINT ( 'NONE',  ( -10.63305928497607411, -33.14245637257592847, 11.52579945308272968 ) ) ;
#61901 = AXIS2_PLACEMENT_3D ( 'NONE', #42217, #21967, #7311 ) ;
#61902 = CARTESIAN_POINT ( 'NONE',  ( 37.00000000000000711, -6.475373545682373333, -10.32377448871666026 ) ) ;
#61903 = ADVANCED_FACE ( 'NONE', ( #16225 ), #16872, .T. ) ;
#61904 = ADVANCED_FACE ( 'NONE', ( #62109 ), #61429, .T. ) ;
#61905 = CARTESIAN_POINT ( 'NONE',  ( 35.00000000000000000, -1.903127969211267700, -11.59095880812007628 ) ) ;
#61906 = CARTESIAN_POINT ( 'NONE',  ( 2.350038591458045723, -9.744161863086636899, -4.227970903880900799 ) ) ;
#61907 = LINE ( 'NONE', #32938, #17530 ) ;
#61908 = CARTESIAN_POINT ( 'NONE',  ( 0.3665391374699464300, 1.872534962004799297, 12.13918562134719181 ) ) ;
#61909 = VERTEX_POINT ( 'NONE', #27182 ) ;
#61910 = DIRECTION ( 'NONE',  ( -1.000000000000000000, -0.000000000000000000, 0.000000000000000000 ) ) ;
#61911 = EDGE_LOOP ( 'NONE', ( #16268, #57055, #59130, #10816 ) ) ;
#61912 = CARTESIAN_POINT ( 'NONE',  ( 41.00000000000000711, 5.493969937218003549E-16, -4.500000000000000888 ) ) ;
#61913 = AXIS2_PLACEMENT_3D ( 'NONE', #54062, #38433, #8496 ) ;
#61914 = DIRECTION ( 'NONE',  ( 0.000000000000000000, -0.01356324068817999114, 0.9999080150203989437 ) ) ;
#61915 = ORIENTED_EDGE ( 'NONE', *, *, #64676, .F. ) ;
#61916 = EDGE_CURVE ( 'NONE', #45822, #60806, #43856, .T. ) ;
#61917 = DIRECTION ( 'NONE',  ( -1.000000000000000000, 0.000000000000000000, 0.000000000000000000 ) ) ;
#61918 = CARTESIAN_POINT ( 'NONE',  ( 2.000000000000001776, -5.217815162096805182, -5.387430271863635767 ) ) ;
#61919 = CARTESIAN_POINT ( 'NONE',  ( 35.00000000000000000, -10.91072401419414462, -5.428340790341669830 ) ) ;
#61920 = CARTESIAN_POINT ( 'NONE',  ( -37.00000000000000711, 0.000000000000000000, 0.000000000000000000 ) ) ;
#61921 = CARTESIAN_POINT ( 'NONE',  ( 5.514970785353741078, -0.004713149585127258956, -0.0003039746380524797073 ) ) ;
#61922 = CIRCLE ( 'NONE', #57709, 12.74999999999999822 ) ;
#61923 = EDGE_CURVE ( 'NONE', #21512, #16453, #36829, .T. ) ;
#61924 = ORIENTED_EDGE ( 'NONE', *, *, #43667, .F. ) ;
#61925 = CARTESIAN_POINT ( 'NONE',  ( -18.87381964659587297, -4.101229939362269761, -11.27785301288100506 ) ) ;
#61926 = ORIENTED_EDGE ( 'NONE', *, *, #14702, .T. ) ;
#61927 = CARTESIAN_POINT ( 'NONE',  ( 35.00000000000000000, 11.59605747147793586, 5.300372733891518529 ) ) ;
#61928 = DIRECTION ( 'NONE',  ( 0.000000000000000000, 0.7196168960969767658, 0.6943713148249667233 ) ) ;
#61929 = DIRECTION ( 'NONE',  ( 0.000000000000000000, 0.000000000000000000, -1.000000000000000000 ) ) ;
#61930 = EDGE_CURVE ( 'NONE', #15285, #45739, #12208, .T. ) ;
#61931 = ORIENTED_EDGE ( 'NONE', *, *, #61771, .F. ) ;
#61932 = VECTOR ( 'NONE', #19278, 1000.000000000000114 ) ;
#61933 = VECTOR ( 'NONE', #42828, 1000.000000000000000 ) ;
#61934 = CARTESIAN_POINT ( 'NONE',  ( 3.152665057734129750, -7.102135024645910732, 3.546019893116286958 ) ) ;
#61935 = AXIS2_PLACEMENT_3D ( 'NONE', #11468, #12440, #18110 ) ;
#61936 = CIRCLE ( 'NONE', #55585, 5.000000000000000888 ) ;
#61937 =( BOUNDED_SURFACE ( )  B_SPLINE_SURFACE ( 3, 1, ( 
 ( #28049, #59612 ),
 ( #64572, #49641 ),
 ( #38679, #54309 ),
 ( #48350, #38330 ) ),
 .UNSPECIFIED., .F., .F., .F. ) 
 B_SPLINE_SURFACE_WITH_KNOTS ( ( 4, 4 ),
 ( 2, 2 ),
 ( 0.000000000000000000, 1.000000000000000000 ),
 ( 0.000000000000000000, 1.000000000000000000 ),
 .UNSPECIFIED. ) 
 GEOMETRIC_REPRESENTATION_ITEM ( )  RATIONAL_B_SPLINE_SURFACE ( (
 ( 1.000000000000000000, 1.000000000000000000),
 ( 0.9942764183789327692, 0.8450855930916585379),
 ( 0.9942764183789327692, 0.8450855930916585379),
 ( 1.000000000000000000, 1.000000000000000000) ) ) 
 REPRESENTATION_ITEM ( '' )  SURFACE ( )  );
#61938 = DIRECTION ( 'NONE',  ( 0.000000000000000000, 0.01356324068817991828, -0.9999080150203990547 ) ) ;
#61940 = EDGE_CURVE ( 'NONE', #56624, #37857, #32478, .T. ) ;
#61939 = B_SPLINE_CURVE_WITH_KNOTS ( 'NONE', 3,
 ( #59764, #54784, #59125, #54115, #48174, #2627, #63420, #28199, #13535, #33816 ),
 .UNSPECIFIED., .F., .F.,
 ( 4, 3, 3, 4 ),
 ( 1.226634733346699349E-18, 6.607638129004547159E-05, 9.911389841680564271E-05, 0.0001667630577588624196 ),
 .UNSPECIFIED. ) ;
#61941 = AXIS2_PLACEMENT_3D ( 'NONE', #5344, #40579, #36232 ) ;
#61942 = DIRECTION ( 'NONE',  ( -1.000000000000000000, 0.000000000000000000, 0.000000000000000000 ) ) ;
#61943 = DIRECTION ( 'NONE',  ( -1.000000000000000000, 0.000000000000000000, 0.000000000000000000 ) ) ;
#61944 = ADVANCED_FACE ( 'NONE', ( #47159 ), #1608, .T. ) ;
#61945 = CARTESIAN_POINT ( 'NONE',  ( 35.00000000000000000, 2.936739658819871313, -11.37311665002364869 ) ) ;
#61946 = CARTESIAN_POINT ( 'NONE',  ( -37.00000000000000711, 0.000000000000000000, 0.000000000000000000 ) ) ;
#61947 = CARTESIAN_POINT ( 'NONE',  ( 1.000000000000000888, -5.097042323172487954, 5.501832381651415638 ) ) ;
#61948 = AXIS2_PLACEMENT_3D ( 'NONE', #10561, #30841, #11555 ) ;
#61949 = EDGE_CURVE ( 'NONE', #34626, #33925, #42127, .T. ) ;
#61950 = CIRCLE ( 'NONE', #53474, 12.74999999999999822 ) ;
#61951 = ORIENTED_EDGE ( 'NONE', *, *, #33284, .T. ) ;
#61952 = EDGE_CURVE ( 'NONE', #5936, #17594, #7612, .T. ) ;
#61953 = CARTESIAN_POINT ( 'NONE',  ( -15.92735611090874848, 7.887070990759704969, 10.95653452613623102 ) ) ;
#61954 = DIRECTION ( 'NONE',  ( 1.000000000000000000, -0.000000000000000000, 0.000000000000000000 ) ) ;
#61955 = ORIENTED_EDGE ( 'NONE', *, *, #63965, .T. ) ;
#61956 = CARTESIAN_POINT ( 'NONE',  ( 5.520433897694421610, 0.01432141647227063407, -0.004666464468078087950 ) ) ;
#61957 = CARTESIAN_POINT ( 'NONE',  ( 3.382263751109486627, 5.483660712610938681, -10.67588914012733348 ) ) ;
#61958 = VECTOR ( 'NONE', #59153, 1000.000000000000000 ) ;
#61959 = CARTESIAN_POINT ( 'NONE',  ( 37.00000000000000711, 11.61175578952788356, 1.771820996347031940 ) ) ;
#61960 = EDGE_LOOP ( 'NONE', ( #22323, #15281, #47231, #34889 ) ) ;
#61961 = EDGE_CURVE ( 'NONE', #12164, #49077, #62922, .T. ) ;
#61962 = CARTESIAN_POINT ( 'NONE',  ( -35.05012975565874456, -0.01323209221896530161, -0.004360246756763594411 ) ) ;
#61963 = ORIENTED_EDGE ( 'NONE', *, *, #1884, .F. ) ;
#61964 = CARTESIAN_POINT ( 'NONE',  ( -35.00000000000000000, -9.076753354954062658, 8.954052073409570767 ) ) ;
#61965 = ORIENTED_EDGE ( 'NONE', *, *, #44726, .F. ) ;
#61966 = ORIENTED_EDGE ( 'NONE', *, *, #15464, .F. ) ;
#61967 = CARTESIAN_POINT ( 'NONE',  ( 12.52750123246316072, 0.4973700281276248192, 25.00000000000000000 ) ) ;
#61968 = VECTOR ( 'NONE', #61470, 1000.000000000000000 ) ;
#61969 = ORIENTED_EDGE ( 'NONE', *, *, #16454, .T. ) ;
#61970 = CARTESIAN_POINT ( 'NONE',  ( -25.56972390839818843, -10.04380371306811881, 6.568580827850054149 ) ) ;
#61971 = CARTESIAN_POINT ( 'NONE',  ( -22.29770266787582145, -3.593535545924356533, 1.047554374660444321 ) ) ;
#61972 = DIRECTION ( 'NONE',  ( 0.3939253465568944290, 0.9068155327749443106, -0.1500280335741446258 ) ) ;
#61973 = DIRECTION ( 'NONE',  ( 1.000000000000000000, 0.000000000000000000, 0.000000000000000000 ) ) ;
#61974 = ORIENTED_EDGE ( 'NONE', *, *, #58044, .T. ) ;
#61975 = CARTESIAN_POINT ( 'NONE',  ( 2.177405672430977379, 9.343720763426027531, -6.173731551724596756 ) ) ;
#61976 = CARTESIAN_POINT ( 'NONE',  ( 2.990024434114437302, -31.21813892570122206, 14.24440799104838717 ) ) ;
#61977 = DIRECTION ( 'NONE',  ( 0.000000000000000000, 0.000000000000000000, 1.000000000000000000 ) ) ;
#61979 = ORIENTED_EDGE ( 'NONE', *, *, #31470, .F. ) ;
#61978 = DIRECTION ( 'NONE',  ( 0.000000000000000000, -0.4698238015817237101, -0.8827602140260384367 ) ) ;
#61980 = CARTESIAN_POINT ( 'NONE',  ( -28.07033260158857857, 9.867324763291481560, -6.836013876802826239 ) ) ;
#61981 = VERTEX_POINT ( 'NONE', #54435 ) ;
#61982 = AXIS2_PLACEMENT_3D ( 'NONE', #22098, #53358, #27096 ) ;
#61983 = DIRECTION ( 'NONE',  ( 0.000000000000000000, -0.9970832820307047317, -0.07632122047555414679 ) ) ;
#61984 = AXIS2_PLACEMENT_3D ( 'NONE', #7419, #3126, #64579 ) ;
#61985 = ORIENTED_EDGE ( 'NONE', *, *, #3729, .F. ) ;
#61986 = CARTESIAN_POINT ( 'NONE',  ( -27.08429572838383947, 2.089332284968718145, 0.9410937941433747955 ) ) ;
#61987 = CARTESIAN_POINT ( 'NONE',  ( -35.00000000000000000, 0.000000000000000000, 0.000000000000000000 ) ) ;
#61989 = DIRECTION ( 'NONE',  ( -1.000000000000000000, 0.000000000000000000, 0.000000000000000000 ) ) ;
#61988 = AXIS2_PLACEMENT_3D ( 'NONE', #40935, #62193, #25636 ) ;
#61991 = EDGE_CURVE ( 'NONE', #2019, #18023, #22602, .T. ) ;
#61990 = VERTEX_POINT ( 'NONE', #28814 ) ;
#61992 = CARTESIAN_POINT ( 'NONE',  ( 1.633930747250582849, 8.702439996574263148, 9.253127167384969098 ) ) ;
#61993 = CARTESIAN_POINT ( 'NONE',  ( -35.00000000000000000, -11.70009620280410978, -1.039216533673027243 ) ) ;
#61994 = CARTESIAN_POINT ( 'NONE',  ( 0.2834382757448007384, -12.02923522794683642, 2.326926314863269951 ) ) ;
#61995 = ORIENTED_EDGE ( 'NONE', *, *, #3771, .T. ) ;
#61996 = EDGE_CURVE ( 'NONE', #30317, #35454, #28478, .T. ) ;
#61997 = ORIENTED_EDGE ( 'NONE', *, *, #46824, .F. ) ;
#61998 = DIRECTION ( 'NONE',  ( -1.000000000000000000, 0.000000000000000000, 0.000000000000000000 ) ) ;
#61999 = ORIENTED_EDGE ( 'NONE', *, *, #56532, .F. ) ;
#62000 = VECTOR ( 'NONE', #35505, 1000.000000000000000 ) ;
#62001 = ORIENTED_EDGE ( 'NONE', *, *, #49275, .T. ) ;
#62002 = CIRCLE ( 'NONE', #38644, 4.999999999999999112 ) ;
#62003 = EDGE_CURVE ( 'NONE', #26234, #33347, #29058, .T. ) ;
#62004 = CARTESIAN_POINT ( 'NONE',  ( 2.241352910868908310, 1.407733736974867034, 7.503490710578237355 ) ) ;
#62005 = CYLINDRICAL_SURFACE ( 'NONE', #30699, 2.899999999999994582 ) ;
#62006 = CARTESIAN_POINT ( 'NONE',  ( 2.241352910868908310, -7.145045428366559648, -2.689314586382423045 ) ) ;
#62007 = CARTESIAN_POINT ( 'NONE',  ( 5.536195898058073439, 0.008411485181668783978, -0.001224473329857621697 ) ) ;
#62008 = CARTESIAN_POINT ( 'NONE',  ( 35.00000000000000000, 4.705694406421931860E-17, -3.469127814946512892E-15 ) ) ;
#62009 = CIRCLE ( 'NONE', #54619, 5.000000000000000000 ) ;
#62010 = B_SPLINE_CURVE_WITH_KNOTS ( 'NONE', 3,
 ( #956, #25237, #641, #20899, #61148, #40869, #5973, #25564, #1300, #30544, #50847, #45509, #45859, #35540, #10264, #21225 ),
 .UNSPECIFIED., .F., .F.,
 ( 4, 3, 3, 3, 3, 4 ),
 ( 0.000000000000000000, 0.0002999043160757210776, 0.0005998071753050730282, 0.0008997092107374146620, 0.001204458948194614670, 0.001510329163474479104 ),
 .UNSPECIFIED. ) ;
#62011 = DIRECTION ( 'NONE',  ( -1.000000000000000000, -0.000000000000000000, 0.000000000000000000 ) ) ;
#62012 = DIRECTION ( 'NONE',  ( 0.000000000000000000, 0.01356324068817998940, -0.9999080150203990547 ) ) ;
#62013 = ORIENTED_EDGE ( 'NONE', *, *, #45255, .T. ) ;
#62014 = CIRCLE ( 'NONE', #15303, 2.899999999999994582 ) ;
#62015 = DIRECTION ( 'NONE',  ( 1.000000000000000000, 0.000000000000000000, 0.000000000000000000 ) ) ;
#62016 = EDGE_CURVE ( 'NONE', #53424, #33400, #40668, .T. ) ;
#62017 = EDGE_CURVE ( 'NONE', #28911, #24086, #42789, .T. ) ;
#62018 = CARTESIAN_POINT ( 'NONE',  ( 12.47628546223243617, 0.000000000000000000, -11.99999999999998224 ) ) ;
#62019 = CIRCLE ( 'NONE', #35471, 12.18650000000000055 ) ;
#62020 = CARTESIAN_POINT ( 'NONE',  ( 2.000000000000001776, 0.000000000000000000, 0.000000000000000000 ) ) ;
#62021 = DIRECTION ( 'NONE',  ( 0.000000000000000000, -0.01356324068817991828, 0.9999080150203990547 ) ) ;
#62022 = CARTESIAN_POINT ( 'NONE',  ( 2.750171585628739646, 2.206612499183723486, -11.80217412294446788 ) ) ;
#62023 = CARTESIAN_POINT ( 'NONE',  ( -22.27834755396594346, 2.447855249718994930, 2.756126180273619219 ) ) ;
#62024 = EDGE_LOOP ( 'NONE', ( #6233, #21548, #44232, #10027 ) ) ;
#62025 = CARTESIAN_POINT ( 'NONE',  ( 2.000000000000001776, 4.962980376314141573, -4.846014654777754060 ) ) ;
#62026 = CIRCLE ( 'NONE', #21695, 4.000000000000000000 ) ;
#62027 = DIRECTION ( 'NONE',  ( -1.000000000000000000, 0.000000000000000000, 0.000000000000000000 ) ) ;
#62028 = LINE ( 'NONE', #42359, #49198 ) ;
#62029 = CIRCLE ( 'NONE', #56736, 12.18649999999999878 ) ;
#62030 = LINE ( 'NONE', #61680, #54566 ) ;
#62031 = EDGE_CURVE ( 'NONE', #42381, #53925, #30034, .T. ) ;
#62032 = EDGE_CURVE ( 'NONE', #8001, #65794, #58107, .T. ) ;
#62033 = DIRECTION ( 'NONE',  ( 0.000000000000000000, 0.000000000000000000, 1.000000000000000000 ) ) ;
#62034 = CARTESIAN_POINT ( 'NONE',  ( -25.37693896798699456, -11.65917517926966873, 6.807023274763674081 ) ) ;
#62035 = ORIENTED_EDGE ( 'NONE', *, *, #31704, .F. ) ;
#62036 = DIRECTION ( 'NONE',  ( 0.000000000000000000, -0.01356324068817998940, 0.9999080150203990547 ) ) ;
#62037 = CARTESIAN_POINT ( 'NONE',  ( -27.41041641377506011, -11.32519648962278680, -7.368711486028817426 ) ) ;
#62038 = CARTESIAN_POINT ( 'NONE',  ( 1.014383007554949589, -12.37541872618880667, -1.731118468094042351 ) ) ;
#62039 = ORIENTED_EDGE ( 'NONE', *, *, #13856, .F. ) ;
#62040 = EDGE_CURVE ( 'NONE', #42133, #32028, #13138, .T. ) ;
#62041 = CARTESIAN_POINT ( 'NONE',  ( 2.653899356900181417, 6.857477569908602355, 3.657605971842781134 ) ) ;
#62042 = CARTESIAN_POINT ( 'NONE',  ( -17.31450763390795800, 7.097772087455203938, -9.677943051329000568 ) ) ;
#62043 = FACE_OUTER_BOUND ( 'NONE', #30562, .T. ) ;
#62044 = CIRCLE ( 'NONE', #18543, 4.999999999999999112 ) ;
#62046 = VERTEX_POINT ( 'NONE', #202 ) ;
#62045 = CARTESIAN_POINT ( 'NONE',  ( -37.00000000000000711, 0.000000000000000000, 0.000000000000000000 ) ) ;
#62047 = CARTESIAN_POINT ( 'NONE',  ( -27.10113028276028757, 2.276991616286352382, 0.5479825692853625974 ) ) ;
#62049 = AXIS2_PLACEMENT_3D ( 'NONE', #53528, #48529, #31891 ) ;
#62048 = CIRCLE ( 'NONE', #33381, 12.74999999999999822 ) ;
#62050 = LINE ( 'NONE', #20163, #20180 ) ;
#62051 = VERTEX_POINT ( 'NONE', #15148 ) ;
#62052 = CARTESIAN_POINT ( 'NONE',  ( 0.000000000000000000, -4.962980376314093611, 4.846014654777763830 ) ) ;
#62053 = DIRECTION ( 'NONE',  ( -1.000000000000000000, 0.000000000000000000, -0.000000000000000000 ) ) ;
#62054 = CYLINDRICAL_SURFACE ( 'NONE', #57696, 2.899999999999994582 ) ;
#62055 = DIRECTION ( 'NONE',  ( 0.000000000000000000, -0.01356324068817992001, 0.9999080150203990547 ) ) ;
#62056 = CARTESIAN_POINT ( 'NONE',  ( 37.00000000000000711, 4.705694406421931860E-17, -3.469127814946512892E-15 ) ) ;
#62057 = AXIS2_PLACEMENT_3D ( 'NONE', #48983, #34315, #38663 ) ;
#62058 = LINE ( 'NONE', #36777, #6854 ) ;
#62060 = ORIENTED_EDGE ( 'NONE', *, *, #64602, .F. ) ;
#62059 = CARTESIAN_POINT ( 'NONE',  ( 0.2915757698887314064, 11.44067056871814714, -4.392559307431786131 ) ) ;
#62061 = VERTEX_POINT ( 'NONE', #59736 ) ;
#62062 = CARTESIAN_POINT ( 'NONE',  ( 23.19458397200137867, -4.581538694898370068, -11.09407635438899931 ) ) ;
#62063 = EDGE_LOOP ( 'NONE', ( #6150, #300, #19486, #4765 ) ) ;
#62064 = CARTESIAN_POINT ( 'NONE',  ( -35.04999999999999716, -19.99999999999998934, 3.143706735044647313E-15 ) ) ;
#62065 = CARTESIAN_POINT ( 'NONE',  ( 2.000000000000001776, 5.396716205731433291, 4.158041573745082431 ) ) ;
#62066 = CARTESIAN_POINT ( 'NONE',  ( 1.937114397841932290, -10.38782037574621597, 7.538912286488311132 ) ) ;
#62067 = AXIS2_PLACEMENT_3D ( 'NONE', #27911, #2671, #47864 ) ;
#62068 = DIRECTION ( 'NONE',  ( 1.000000000000000000, 0.000000000000000000, 0.000000000000000000 ) ) ;
#62069 = ORIENTED_EDGE ( 'NONE', *, *, #63306, .T. ) ;
#62070 = DIRECTION ( 'NONE',  ( 0.000000000000000000, -0.01356324068817998940, 0.9999080150203990547 ) ) ;
#62071 = ADVANCED_FACE ( 'NONE', ( #65360 ), #49755, .T. ) ;
#62072 = CARTESIAN_POINT ( 'NONE',  ( 0.2655924914740778742, 11.49267051747974122, -4.229867354073444830 ) ) ;
#62073 = FACE_OUTER_BOUND ( 'NONE', #14319, .T. ) ;
#62074 = ORIENTED_EDGE ( 'NONE', *, *, #8811, .F. ) ;
#62076 = ORIENTED_EDGE ( 'NONE', *, *, #50688, .F. ) ;
#62075 = B_SPLINE_CURVE_WITH_KNOTS ( 'NONE', 3,
 ( #2778, #32985, #22359, #7389, #6765, #27038, #1776 ),
 .UNSPECIFIED., .F., .F.,
 ( 4, 3, 4 ),
 ( 1.013772664892015885E-14, 0.002398160485434997630, 0.005002426799387000092 ),
 .UNSPECIFIED. ) ;
#62077 = CARTESIAN_POINT ( 'NONE',  ( 2.717984159219562379, 7.620583877640641823, -1.631703089060060119 ) ) ;
#62078 = AXIS2_PLACEMENT_3D ( 'NONE', #27360, #63263, #6124 ) ;
#62079 = ORIENTED_EDGE ( 'NONE', *, *, #21995, .F. ) ;
#62080 = DIRECTION ( 'NONE',  ( -1.000000000000000000, 0.000000000000000000, -0.000000000000000000 ) ) ;
#62081 = CARTESIAN_POINT ( 'NONE',  ( 9.105023507364348845, 3.304801514924585959, 13.09129911384226652 ) ) ;
#62082 = DIRECTION ( 'NONE',  ( -1.000000000000000000, -0.000000000000000000, 0.000000000000000000 ) ) ;
#62083 = CARTESIAN_POINT ( 'NONE',  ( 9.687175622948609899, 13.48729812737144940, -0.5854820436212360146 ) ) ;
#62084 = CARTESIAN_POINT ( 'NONE',  ( 2.639814597422739606, -7.689608172406200204, 1.095525832903460506 ) ) ;
#62085 = CARTESIAN_POINT ( 'NONE',  ( 2.268878695253354394, 7.500319319173578414, 1.472930498387300613 ) ) ;
#62086 = VERTEX_POINT ( 'NONE', #14799 ) ;
#62087 = CIRCLE ( 'NONE', #26021, 2.899999999999995914 ) ;
#62088 = CARTESIAN_POINT ( 'NONE',  ( -35.00000000000000000, 4.237174932027226504, 12.02534193257722350 ) ) ;
#62089 = ORIENTED_EDGE ( 'NONE', *, *, #56688, .T. ) ;
#62090 = DIRECTION ( 'NONE',  ( 0.000000000000000000, 0.01356324068817992001, -0.9999080150203990547 ) ) ;
#62091 = EDGE_CURVE ( 'NONE', #49961, #23637, #65049, .T. ) ;
#62092 = DIRECTION ( 'NONE',  ( 1.000000000000000000, -0.000000000000000000, 0.000000000000000000 ) ) ;
#62093 = LINE ( 'NONE', #601, #4089 ) ;
#62094 = CARTESIAN_POINT ( 'NONE',  ( 2.653899356899724893, -2.902068786425232805, -7.209790345489500929 ) ) ;
#62095 = CARTESIAN_POINT ( 'NONE',  ( -36.00000000000000711, 11.73555825188283741, -4.983891302653458588 ) ) ;
#62096 = CARTESIAN_POINT ( 'NONE',  ( 36.00000000000000711, -12.38385022362083987, -3.033604067594536602 ) ) ;
#62097 = EDGE_CURVE ( 'NONE', #14797, #63500, #16105, .T. ) ;
#62098 = AXIS2_PLACEMENT_3D ( 'NONE', #57070, #26801, #17808 ) ;
#62099 = ORIENTED_EDGE ( 'NONE', *, *, #40756, .T. ) ;
#62100 = ORIENTED_EDGE ( 'NONE', *, *, #37821, .F. ) ;
#62101 = CARTESIAN_POINT ( 'NONE',  ( 2.241352910868908310, 1.407733736974966288, -7.503490710578218703 ) ) ;
#62102 = ORIENTED_EDGE ( 'NONE', *, *, #61174, .F. ) ;
#62103 = FACE_OUTER_BOUND ( 'NONE', #41049, .T. ) ;
#62104 = DIRECTION ( 'NONE',  ( 0.000000000000000000, 0.9999080150203989437, 0.01356324068818338426 ) ) ;
#62105 = CARTESIAN_POINT ( 'NONE',  ( 2.247206125382836817, 4.819320926502623337, 5.923516414428621424 ) ) ;
#62106 = CARTESIAN_POINT ( 'NONE',  ( 0.2653519890538383330, -0.02202471025202958066, -12.24619734961521544 ) ) ;
#62107 = ORIENTED_EDGE ( 'NONE', *, *, #45736, .F. ) ;
#62108 = CARTESIAN_POINT ( 'NONE',  ( 0.3665391374699472626, 9.576575648339021640, 7.691255657244324695 ) ) ;
#62109 = FACE_OUTER_BOUND ( 'NONE', #31478, .T. ) ;
#62110 = CARTESIAN_POINT ( 'NONE',  ( -37.00000000000000711, 0.000000000000000000, 0.000000000000000000 ) ) ;
#62111 = LINE ( 'NONE', #16563, #4109 ) ;
#62112 = EDGE_CURVE ( 'NONE', #8415, #27274, #17281, .T. ) ;
#62113 = DIRECTION ( 'NONE',  ( 1.000000000000000000, -0.000000000000000000, 0.000000000000000000 ) ) ;
#62114 = CARTESIAN_POINT ( 'NONE',  ( -27.15525204139121840, 1.707635684994321945, -1.831989866434744485 ) ) ;
#62115 = VERTEX_POINT ( 'NONE', #10164 ) ;
#62116 = DIRECTION ( 'NONE',  ( 1.000000000000000000, -0.000000000000000000, 0.000000000000000000 ) ) ;
#62117 = ORIENTED_EDGE ( 'NONE', *, *, #38799, .F. ) ;
#62118 = CARTESIAN_POINT ( 'NONE',  ( -22.30625920655495165, 3.635849356906417640, -1.076742202099146839 ) ) ;
#62119 = DIRECTION ( 'NONE',  ( 0.000000000000000000, 1.000000000000000000, 0.000000000000000000 ) ) ;
#62120 = CARTESIAN_POINT ( 'NONE',  ( 3.152665057735335452, -7.719888720907720270, 1.848755561853250295 ) ) ;
#62121 = CARTESIAN_POINT ( 'NONE',  ( 28.46403053133689198, -10.24654051476648497, 6.260428664560219403 ) ) ;
#62122 = CARTESIAN_POINT ( 'NONE',  ( -8.606002450955907435, -2.738469685186787128, 11.68403320950772795 ) ) ;
#62123 = ADVANCED_FACE ( 'NONE', ( #55060 ), #54763, .F. ) ;
#62124 = ORIENTED_EDGE ( 'NONE', *, *, #20439, .T. ) ;
#62125 = ORIENTED_EDGE ( 'NONE', *, *, #59614, .F. ) ;
#62126 = DIRECTION ( 'NONE',  ( 0.000000000000000000, -0.9467777615094604693, -0.3218879778915875178 ) ) ;
#62127 = ORIENTED_EDGE ( 'NONE', *, *, #41972, .T. ) ;
#62128 = CARTESIAN_POINT ( 'NONE',  ( 3.425926600331120397, 5.853248163474676247, 10.47781994178590104 ) ) ;
#62130 = AXIS2_PLACEMENT_3D ( 'NONE', #44191, #9923, #48868 ) ;
#62129 = DIRECTION ( 'NONE',  ( -1.000000000000000000, 0.000000000000000000, 0.000000000000000000 ) ) ;
#62131 = LINE ( 'NONE', #27205, #37330 ) ;
#62132 = CARTESIAN_POINT ( 'NONE',  ( 2.177405672431695027, -10.27382588316267231, 4.457418613956002140 ) ) ;
#62133 = CARTESIAN_POINT ( 'NONE',  ( 1.020182472823639053, -7.686484208904866833, -9.854645283130558653 ) ) ;
#62134 = CARTESIAN_POINT ( 'NONE',  ( -35.00000000000000000, -0.7008968033237865658, -12.16632754454237819 ) ) ;
#62135 = CARTESIAN_POINT ( 'NONE',  ( 0.7446945582541437680, 12.27434006248903664, -1.802628359587088891 ) ) ;
#62136 = ORIENTED_EDGE ( 'NONE', *, *, #32286, .T. ) ;
#62137 = FACE_OUTER_BOUND ( 'NONE', #37762, .T. ) ;
#62138 = ORIENTED_EDGE ( 'NONE', *, *, #60284, .T. ) ;
#62139 = DIRECTION ( 'NONE',  ( 0.000000000000000000, -0.7196168960969868689, -0.6943713148249562872 ) ) ;
#62140 = DIRECTION ( 'NONE',  ( 1.000000000000000000, 0.000000000000000000, 0.000000000000000000 ) ) ;
#62141 = CARTESIAN_POINT ( 'NONE',  ( 0.8375941296819096049, 8.285008510335908127, -9.275620596396473516 ) ) ;
#62142 = DIRECTION ( 'NONE',  ( 0.000000000000000000, 0.2960891610144441022, 0.9551603052523501836 ) ) ;
#62143 = ORIENTED_EDGE ( 'NONE', *, *, #16605, .T. ) ;
#62144 = CARTESIAN_POINT ( 'NONE',  ( -35.00000000000000000, -10.80478261802186246, 5.636262487437281976 ) ) ;
#62145 = EDGE_CURVE ( 'NONE', #9803, #30859, #24152, .T. ) ;
#62146 =( BOUNDED_SURFACE ( )  B_SPLINE_SURFACE ( 3, 1, ( 
 ( #30240, #25242 ),
 ( #21908, #38156 ),
 ( #2634, #58467 ),
 ( #6289, #52171 ) ),
 .UNSPECIFIED., .F., .F., .F. ) 
 B_SPLINE_SURFACE_WITH_KNOTS ( ( 4, 4 ),
 ( 2, 2 ),
 ( 0.000000000000000000, 1.000000000000000000 ),
 ( 0.000000000000000000, 1.000000000000000000 ),
 .UNSPECIFIED. ) 
 GEOMETRIC_REPRESENTATION_ITEM ( )  RATIONAL_B_SPLINE_SURFACE ( (
 ( 1.000000000000000000, 1.000000000000000000),
 ( 0.9856612449720755231, 0.9999558406602322425),
 ( 0.9856612449720755231, 0.9999558406602322425),
 ( 1.000000000000000000, 1.000000000000000000) ) ) 
 REPRESENTATION_ITEM ( '' )  SURFACE ( )  );
#62147 = LINE ( 'NONE', #16600, #62610 ) ;
#62148 = VERTEX_POINT ( 'NONE', #4203 ) ;
#62149 = ORIENTED_EDGE ( 'NONE', *, *, #33094, .T. ) ;
#62150 = CARTESIAN_POINT ( 'NONE',  ( 0.6705955404150230059, 0.5055564190250056988, 13.49364205544756423 ) ) ;
#62151 = ADVANCED_FACE ( 'NONE', ( #45741 ), #45097, .T. ) ;
#62152 = ORIENTED_EDGE ( 'NONE', *, *, #41549, .F. ) ;
#62153 = DIRECTION ( 'NONE',  ( 0.000000000000000000, 0.01356324068817998940, -0.9999080150203990547 ) ) ;
#62154 = ORIENTED_EDGE ( 'NONE', *, *, #40016, .T. ) ;
#62155 = VERTEX_POINT ( 'NONE', #9832 ) ;
#62156 = ORIENTED_EDGE ( 'NONE', *, *, #36258, .T. ) ;
#62157 = CARTESIAN_POINT ( 'NONE',  ( -22.27715526084302056, -2.930376837866825124, 2.228953214080627632 ) ) ;
#62158 = CARTESIAN_POINT ( 'NONE',  ( 2.290907136832905255, 5.041121061899806577, -5.755317856506234619 ) ) ;
#62159 = VECTOR ( 'NONE', #18697, 1000.000000000000000 ) ;
#62160 = CARTESIAN_POINT ( 'NONE',  ( -20.74858375370908803, -11.60713604139673905, -3.059550090777561682 ) ) ;
#62162 = ADVANCED_FACE ( 'NONE', ( #55393 ), #51849, .F. ) ;
#62161 = CARTESIAN_POINT ( 'NONE',  ( -35.00000000000000000, 9.430788938294162094, -7.718225330433707398 ) ) ;
#62163 = CYLINDRICAL_SURFACE ( 'NONE', #26355, 5.000000000000000888 ) ;
#62164 = ORIENTED_EDGE ( 'NONE', *, *, #13736, .F. ) ;
#62165 = CARTESIAN_POINT ( 'NONE',  ( 37.00000000000000711, 11.71932350927024657, -3.511386971104992760 ) ) ;
#62166 = VERTEX_POINT ( 'NONE', #9490 ) ;
#62167 = CARTESIAN_POINT ( 'NONE',  ( -10.64311535907470230, -9.781890035361625380, -9.304428041637391900 ) ) ;
#62168 = CARTESIAN_POINT ( 'NONE',  ( -2.798074428798408952, 8.529348309608609568, 10.48748355420409339 ) ) ;
#62169 = CARTESIAN_POINT ( 'NONE',  ( -25.00000000000000355, -9.999999999999998224, -5.000000000000000888 ) ) ;
#62170 = EDGE_CURVE ( 'NONE', #9280, #27036, #29774, .T. ) ;
#62171 = COLOUR_RGB ( '', 0.09019608, 0.27058824, 0.51372549) ;
#62172 = DIRECTION ( 'NONE',  ( 0.000000000000000000, 0.000000000000000000, -1.000000000000000000 ) ) ;
#62173 = CARTESIAN_POINT ( 'NONE',  ( -27.45775109278351067, 25.00000000000000000, -1.989333891161980894 ) ) ;
#62174 = CARTESIAN_POINT ( 'NONE',  ( 2.440552418640495436, -7.698292014589408261, -0.1974238147510066488 ) ) ;
#62175 = ORIENTED_EDGE ( 'NONE', *, *, #23920, .F. ) ;
#62176 = DIRECTION ( 'NONE',  ( -1.000000000000000000, -0.000000000000000000, 0.000000000000000000 ) ) ;
#62177 = AXIS2_PLACEMENT_3D ( 'NONE', #65359, #39433, #13821 ) ;
#62178 = ORIENTED_EDGE ( 'NONE', *, *, #1759, .T. ) ;
#62179 = CARTESIAN_POINT ( 'NONE',  ( 0.3675815128205894289, 10.76447900494940235, 5.910255304480483751 ) ) ;
#62180 = CARTESIAN_POINT ( 'NONE',  ( 12.41715713833625401, -27.32744910944862937, -12.80873342738428988 ) ) ;
#62181 = CARTESIAN_POINT ( 'NONE',  ( 19.56743653832047514, -30.00000000000000000, 5.000000000000000888 ) ) ;
#62182 = DIRECTION ( 'NONE',  ( -1.000000000000000000, 0.000000000000000000, 0.000000000000000000 ) ) ;
#62183 = CARTESIAN_POINT ( 'NONE',  ( 3.152665057735747567, 7.886634106564638813, 0.9030954876722160352 ) ) ;
#62184 = ORIENTED_EDGE ( 'NONE', *, *, #63224, .F. ) ;
#62185 = CARTESIAN_POINT ( 'NONE',  ( 37.00000000000000711, 4.705694406421931860E-17, -3.469127814946512892E-15 ) ) ;
#62186 = CARTESIAN_POINT ( 'NONE',  ( 0.3401186441510221092, 2.382124782498519000, -12.03768714635922166 ) ) ;
#62187 = CARTESIAN_POINT ( 'NONE',  ( 35.00000000000000000, -11.50504120060945645, -4.018060380616356397 ) ) ;
#62188 = CARTESIAN_POINT ( 'NONE',  ( 8.434373009623573836, -31.78234095107705670, -13.63772037845195939 ) ) ;
#62189 = CIRCLE ( 'NONE', #4861, 12.18649999999999878 ) ;
#62190 = CYLINDRICAL_SURFACE ( 'NONE', #20160, 12.74999999999999822 ) ;
#62191 = CARTESIAN_POINT ( 'NONE',  ( 2.241537034860906275, 2.606707005150542766, 7.175668896091105253 ) ) ;
#62192 = CARTESIAN_POINT ( 'NONE',  ( 1.634816307077033404, -5.718391684265862196, -11.34285134320889377 ) ) ;
#62193 = DIRECTION ( 'NONE',  ( 1.000000000000000000, 0.000000000000000000, 0.000000000000000000 ) ) ;
#62194 = EDGE_CURVE ( 'NONE', #40279, #36481, #6697, .T. ) ;
#62195 = ORIENTED_EDGE ( 'NONE', *, *, #41562, .F. ) ;
#62196 = VERTEX_POINT ( 'NONE', #40411 ) ;
#62197 = CARTESIAN_POINT ( 'NONE',  ( -37.00000000000000711, 1.113475361586490298, 12.70128625845193326 ) ) ;
#62198 = CARTESIAN_POINT ( 'NONE',  ( 48.84424248505259669, -0.2332870993691684991, -3.158587530951941780 ) ) ;
#62199 = CYLINDRICAL_SURFACE ( 'NONE', #53457, 4.500030059823568074 ) ;
#62200 = DIRECTION ( 'NONE',  ( 1.000000000000000000, 0.000000000000000000, 0.000000000000000000 ) ) ;
#62201 = ORIENTED_EDGE ( 'NONE', *, *, #13856, .T. ) ;
#62202 = ORIENTED_EDGE ( 'NONE', *, *, #2832, .F. ) ;
#62203 = EDGE_LOOP ( 'NONE', ( #31759, #19822, #24948, #9620 ) ) ;
#62204 = CARTESIAN_POINT ( 'NONE',  ( 37.00000000000000711, 10.49591321039688019, 5.273331777780226659 ) ) ;
#62205 = FACE_OUTER_BOUND ( 'NONE', #2674, .T. ) ;
#62206 = EDGE_CURVE ( 'NONE', #44869, #11584, #8922, .T. ) ;
#62207 = ORIENTED_EDGE ( 'NONE', *, *, #7002, .T. ) ;
#62208 = AXIS2_PLACEMENT_3D ( 'NONE', #32601, #52909, #36298 ) ;
#62209 = CARTESIAN_POINT ( 'NONE',  ( 35.00000000000000000, 4.705694406421931860E-17, -3.469127814946512892E-15 ) ) ;
#62210 = FACE_OUTER_BOUND ( 'NONE', #47681, .T. ) ;
#62211 = EDGE_LOOP ( 'NONE', ( #40658, #61271, #65787, #49668 ) ) ;
#62212 = CIRCLE ( 'NONE', #9147, 6.936499999999989008 ) ;
#62213 = CARTESIAN_POINT ( 'NONE',  ( 0.2653519890518175051, 11.50765826381083201, -4.188454465438567809 ) ) ;
#62214 = EDGE_CURVE ( 'NONE', #29569, #39344, #34262, .T. ) ;
#62215 = CARTESIAN_POINT ( 'NONE',  ( 17.05023968204111284, -34.49999999999999289, -4.356789313881303194 ) ) ;
#62216 = CYLINDRICAL_SURFACE ( 'NONE', #1692, 4.999999999999999112 ) ;
#62217 = ORIENTED_EDGE ( 'NONE', *, *, #49756, .F. ) ;
#62218 = DIRECTION ( 'NONE',  ( 1.000000000000000000, -0.000000000000000000, 0.000000000000000000 ) ) ;
#62219 = EDGE_CURVE ( 'NONE', #35774, #56983, #46466, .T. ) ;
#62220 = EDGE_LOOP ( 'NONE', ( #64408, #54565, #48969, #22488 ) ) ;
#62221 = CARTESIAN_POINT ( 'NONE',  ( 0.8320506296491566589, 7.696193170530746031, -9.767350172724349022 ) ) ;
#62222 = ORIENTED_EDGE ( 'NONE', *, *, #55887, .F. ) ;
#62223 = DIRECTION ( 'NONE',  ( -1.000000000000000000, 0.000000000000000000, -0.000000000000000000 ) ) ;
#62224 = VECTOR ( 'NONE', #56698, 1000.000000000000000 ) ;
#62225 = CARTESIAN_POINT ( 'NONE',  ( -16.21117406328131949, -35.00000000000000000, 4.142385751841757724 ) ) ;
#62226 = LINE ( 'NONE', #38254, #59145 ) ;
#62227 = CARTESIAN_POINT ( 'NONE',  ( 2.241537034860906275, -6.614004440763070924, 3.813147095850959900 ) ) ;
#62229 = EDGE_CURVE ( 'NONE', #21159, #29920, #37436, .T. ) ;
#62228 = CARTESIAN_POINT ( 'NONE',  ( -35.00000000000000000, 0.000000000000000000, 0.000000000000000000 ) ) ;
#62230 = FACE_OUTER_BOUND ( 'NONE', #26541, .T. ) ;
#62231 = DIRECTION ( 'NONE',  ( 1.000000000000000000, -0.000000000000000000, 0.000000000000000000 ) ) ;
#62232 = ORIENTED_EDGE ( 'NONE', *, *, #57795, .T. ) ;
#62233 = CARTESIAN_POINT ( 'NONE',  ( -37.00000000000000711, 0.6593684648222315481, -12.73293890771482850 ) ) ;
#62234 = ORIENTED_EDGE ( 'NONE', *, *, #64047, .F. ) ;
#62235 = DIRECTION ( 'NONE',  ( -1.000000000000000000, 0.000000000000000000, 0.000000000000000000 ) ) ;
#62236 = ADVANCED_FACE ( 'NONE', ( #36069 ), #27174, .F. ) ;
#62237 = CARTESIAN_POINT ( 'NONE',  ( 35.00000000000000000, 8.624332853796058629, -9.390600770288020982 ) ) ;
#62238 = ORIENTED_EDGE ( 'NONE', *, *, #37897, .T. ) ;
#62239 = B_SPLINE_CURVE_WITH_KNOTS ( 'NONE', 3,
 ( #56367, #37056, #1522, #6175, #57039, #52386, #41068, #17118, #12121, #46398, #32397, #31430, #36066, #42355, #51729, #1835, #26769, #56730 ),
 .UNSPECIFIED., .F., .F.,
 ( 4, 2, 2, 2, 2, 2, 2, 2, 4 ),
 ( 0.005052247689395389027, 0.005881123449897000116, 0.006709999210398609470, 0.007538874970900218825, 0.008367750731401828179, 0.009196626491903437534, 0.01002550225240504515, 0.01085437801290665451, 0.01168325377340826386 ),
 .UNSPECIFIED. ) ;
#62240 = CARTESIAN_POINT ( 'NONE',  ( 0.2648978790185593790, 4.312320170909392125, -11.46165506714223703 ) ) ;
#62241 = DIRECTION ( 'NONE',  ( 1.000000000000000000, -0.000000000000000000, 0.000000000000000000 ) ) ;
#62242 = DIRECTION ( 'NONE',  ( -1.000000000000000000, 0.000000000000000000, -0.000000000000000000 ) ) ;
#62243 = FACE_OUTER_BOUND ( 'NONE', #63666, .T. ) ;
#62244 = ORIENTED_EDGE ( 'NONE', *, *, #35527, .F. ) ;
#62245 = ORIENTED_EDGE ( 'NONE', *, *, #18199, .T. ) ;
#62246 = CARTESIAN_POINT ( 'NONE',  ( 36.00000000000000711, -9.733281772932102172, 8.235637554476744171 ) ) ;
#62247 = EDGE_CURVE ( 'NONE', #29901, #41167, #42740, .T. ) ;
#62248 = ORIENTED_EDGE ( 'NONE', *, *, #15879, .F. ) ;
#62249 = DIRECTION ( 'NONE',  ( 0.000000000000000000, 0.000000000000000000, 1.000000000000000000 ) ) ;
#62250 = EDGE_CURVE ( 'NONE', #43149, #39558, #53408, .T. ) ;
#62251 = CARTESIAN_POINT ( 'NONE',  ( -37.00000000000000711, 11.72195762423408816, 0.7536123767500589876 ) ) ;
#62252 = DIRECTION ( 'NONE',  ( 0.3509218304786018705, 0.9364047569793457759, 0.000000000000000000 ) ) ;
#62253 = ORIENTED_EDGE ( 'NONE', *, *, #38267, .T. ) ;
#62254 = CARTESIAN_POINT ( 'NONE',  ( 0.2872850955227765346, -4.386654201695071364, -11.44140577127596892 ) ) ;
#62255 = CARTESIAN_POINT ( 'NONE',  ( -35.00000000000000000, -12.15823808070322087, -0.8294751490780611913 ) ) ;
#62256 = CYLINDRICAL_SURFACE ( 'NONE', #11792, 5.000000000000000888 ) ;
#62257 = CARTESIAN_POINT ( 'NONE',  ( 11.74548640120467979, 10.73597826697114677, -8.184666801472349817 ) ) ;
#62258 = DIRECTION ( 'NONE',  ( -1.000000000000000000, 0.000000000000000000, 0.000000000000000000 ) ) ;
#62259 = CYLINDRICAL_SURFACE ( 'NONE', #18200, 4.999999999999999112 ) ;
#62260 = CARTESIAN_POINT ( 'NONE',  ( 2.251152103363644574, -5.769488058190768598, 5.004701566805206170 ) ) ;
#62261 = CARTESIAN_POINT ( 'NONE',  ( -25.42680463514452072, -2.219378695194082152, 3.188632951113938852 ) ) ;
#62262 = EDGE_CURVE ( 'NONE', #54132, #21703, #18380, .T. ) ;
#62263 = ORIENTED_EDGE ( 'NONE', *, *, #31725, .T. ) ;
#62264 = CYLINDRICAL_SURFACE ( 'NONE', #29942, 2.899999999999994582 ) ;
#62265 = DIRECTION ( 'NONE',  ( 0.000000000000000000, 0.01356324068817998940, -0.9999080150203990547 ) ) ;
#62266 = ORIENTED_EDGE ( 'NONE', *, *, #4130, .F. ) ;
#62267 = CARTESIAN_POINT ( 'NONE',  ( 1.452237505248555660, 2.778494755359055546, 12.34692280296792788 ) ) ;
#62268 = CARTESIAN_POINT ( 'NONE',  ( 1.198791140420721657, -9.279671759317723811, -8.460175745279153503 ) ) ;
#62269 = VERTEX_POINT ( 'NONE', #61679 ) ;
#62270 = CARTESIAN_POINT ( 'NONE',  ( 2.241311220309654129, 6.564680916077612949, 3.897297589552382480 ) ) ;
#62271 = ORIENTED_EDGE ( 'NONE', *, *, #33875, .F. ) ;
#62272 = EDGE_CURVE ( 'NONE', #32962, #39957, #62028, .T. ) ;
#62273 = DIRECTION ( 'NONE',  ( -1.000000000000000000, 0.000000000000000000, 0.000000000000000000 ) ) ;
#62274 = ORIENTED_EDGE ( 'NONE', *, *, #5565, .T. ) ;
#62275 = EDGE_LOOP ( 'NONE', ( #45027, #42936, #5827, #31140 ) ) ;
#62276 = CARTESIAN_POINT ( 'NONE',  ( 2.288423627607477862, -7.131972212895026253, 2.767471693622772566 ) ) ;
#62277 = ADVANCED_FACE ( 'NONE', ( #37061 ), #26440, .T. ) ;
#62278 = EDGE_LOOP ( 'NONE', ( #51981, #64885, #51087, #60804 ) ) ;
#62279 = DIRECTION ( 'NONE',  ( 0.000000000000000000, 0.000000000000000000, 1.000000000000000000 ) ) ;
#62280 = CARTESIAN_POINT ( 'NONE',  ( 0.7446945582524583385, -11.53120448859782599, -4.576048078259130847 ) ) ;
#62281 = DIRECTION ( 'NONE',  ( 0.000000000000000000, -0.01356324068817998940, 0.9999080150203990547 ) ) ;
#62282 = CARTESIAN_POINT ( 'NONE',  ( 0.8320506296491575471, -0.3827056590415959247, -12.42924193558400603 ) ) ;
#62283 = EDGE_LOOP ( 'NONE', ( #26629, #40114, #12358, #57981 ) ) ;
#62284 = LINE ( 'NONE', #22056, #1234 ) ;
#62285 = CARTESIAN_POINT ( 'NONE',  ( -2.647174210752905488, -25.80125502049867947, 15.55106108913133767 ) ) ;
#62286 = LINE ( 'NONE', #37688, #6899 ) ;
#62288 = EDGE_LOOP ( 'NONE', ( #1824, #55030, #3425, #17703 ) ) ;
#62287 = CARTESIAN_POINT ( 'NONE',  ( 0.2650492433740065934, -12.07870441534855210, -2.017984765249196677 ) ) ;
#62289 = CARTESIAN_POINT ( 'NONE',  ( 35.00000000000000000, 11.73463472867580393, 3.287724142101285274 ) ) ;
#62290 = EDGE_CURVE ( 'NONE', #17119, #61052, #57633, .T. ) ;
#62291 = VERTEX_POINT ( 'NONE', #6179 ) ;
#62292 = DIRECTION ( 'NONE',  ( -1.000000000000000000, -0.000000000000000000, 0.000000000000000000 ) ) ;
#62293 = ORIENTED_EDGE ( 'NONE', *, *, #22895, .T. ) ;
#62294 = AXIS2_PLACEMENT_3D ( 'NONE', #51623, #50954, #25674 ) ;
#62295 = CARTESIAN_POINT ( 'NONE',  ( 21.77067674801237374, -10.88489934719429719, -5.055603271500189955 ) ) ;
#62296 = DIRECTION ( 'NONE',  ( 1.000000000000000000, -0.000000000000000000, 0.000000000000000000 ) ) ;
#62297 = CARTESIAN_POINT ( 'NONE',  ( 1.634816307075114272, -5.013416918607946471, 11.67158647524045811 ) ) ;
#62298 = ORIENTED_EDGE ( 'NONE', *, *, #30526, .F. ) ;
#62299 = CARTESIAN_POINT ( 'NONE',  ( 1.547277799337564597, 8.651049845883598266, 9.261681528764491134 ) ) ;
#62300 = AXIS2_PLACEMENT_3D ( 'NONE', #60914, #8738, #26311 ) ;
#62301 = CARTESIAN_POINT ( 'NONE',  ( 0.3665391374699472626, 12.04754782681760794, -2.392238720110336558 ) ) ;
#62303 = CARTESIAN_POINT ( 'NONE',  ( 0.2638984909335716500, -11.57533005135181803, 4.001111175853703017 ) ) ;
#62302 = B_SPLINE_CURVE_WITH_KNOTS ( 'NONE', 3,
 ( #20330, #45945, #10672, #14663, #19700, #10036, #59934, #44598, #39959, #15002, #46, #14357, #55253, #25322, #30959, #49944 ),
 .UNSPECIFIED., .F., .F.,
 ( 4, 3, 3, 3, 3, 4 ),
 ( 0.000000000000000000, 0.0002176109881720252981, 0.0004352086762394631603, 0.0006528017811446922784, 0.0007615147961451762884, 0.0009453342004947409664 ),
 .UNSPECIFIED. ) ;
#62304 = ORIENTED_EDGE ( 'NONE', *, *, #13316, .F. ) ;
#62305 = ORIENTED_EDGE ( 'NONE', *, *, #28426, .F. ) ;
#62306 = CARTESIAN_POINT ( 'NONE',  ( 1.000000000000000888, 4.604744433234757572, -5.919993978425451608 ) ) ;
#62307 = ORIENTED_EDGE ( 'NONE', *, *, #57899, .F. ) ;
#62308 = EDGE_CURVE ( 'NONE', #6868, #34813, #62978, .T. ) ;
#62309 = ADVANCED_FACE ( 'NONE', ( #6835 ), #57043, .T. ) ;
#62310 = ORIENTED_EDGE ( 'NONE', *, *, #53934, .F. ) ;
#62311 = CARTESIAN_POINT ( 'NONE',  ( -35.00000000000000000, 4.545979934229578134, -11.30684963584384128 ) ) ;
#62312 = CARTESIAN_POINT ( 'NONE',  ( 1.283627346226612564, -10.61381050043334717, 6.763590725840863627 ) ) ;
#62313 = CARTESIAN_POINT ( 'NONE',  ( 35.00000000000000000, 11.44858830469736333, -2.627174906297124135 ) ) ;
#62314 = CARTESIAN_POINT ( 'NONE',  ( -22.29570301036918778, 1.042190670255910723, 3.588849529203719246 ) ) ;
#62315 = EDGE_CURVE ( 'NONE', #44838, #7784, #27378, .T. ) ;
#62316 = DIRECTION ( 'NONE',  ( 0.000000000000000000, 0.000000000000000000, 1.000000000000000000 ) ) ;
#62317 = CARTESIAN_POINT ( 'NONE',  ( -35.00000000000000000, -11.07407352312210058, -3.916263239775468197 ) ) ;
#62318 = EDGE_CURVE ( 'NONE', #56972, #45989, #48145, .T. ) ;
#62319 = CARTESIAN_POINT ( 'NONE',  ( 37.00000000000000711, 4.705694406421931860E-17, -3.469127814946512892E-15 ) ) ;
#62320 = EDGE_CURVE ( 'NONE', #43224, #40174, #22644, .T. ) ;
#62321 =( BOUNDED_SURFACE ( )  B_SPLINE_SURFACE ( 3, 1, ( 
 ( #4280, #24552 ),
 ( #39845, #9913 ),
 ( #48745, #34421 ),
 ( #4168, #34077 ) ),
 .UNSPECIFIED., .F., .F., .F. ) 
 B_SPLINE_SURFACE_WITH_KNOTS ( ( 4, 4 ),
 ( 2, 2 ),
 ( 0.000000000000000000, 1.000000000000000000 ),
 ( 0.000000000000000000, 1.000000000000000000 ),
 .UNSPECIFIED. ) 
 GEOMETRIC_REPRESENTATION_ITEM ( )  RATIONAL_B_SPLINE_SURFACE ( (
 ( 1.000000000000000000, 1.000000000000000000),
 ( 0.9856612449720755231, 0.9999558406602322425),
 ( 0.9856612449720755231, 0.9999558406602322425),
 ( 1.000000000000000000, 1.000000000000000000) ) ) 
 REPRESENTATION_ITEM ( '' )  SURFACE ( )  );
#62322 = ORIENTED_EDGE ( 'NONE', *, *, #34488, .F. ) ;
#62323 = EDGE_CURVE ( 'NONE', #55188, #53297, #65105, .T. ) ;
#62324 = FACE_OUTER_BOUND ( 'NONE', #32777, .T. ) ;
#62325 = CARTESIAN_POINT ( 'NONE',  ( -2.952869152607106251, -11.39722960915210592, 3.755417052241485365 ) ) ;
#62326 = FACE_OUTER_BOUND ( 'NONE', #7390, .T. ) ;
#62327 = CARTESIAN_POINT ( 'NONE',  ( 20.00005080000000035, 5.400000000000000355, 1.000000000000000000 ) ) ;
#62328 = CARTESIAN_POINT ( 'NONE',  ( -35.00000000000000000, 0.06441628369853458214, -12.18632975068353019 ) ) ;
#62329 = PLANE ( 'NONE',  #62846 ) ;
#62330 = EDGE_LOOP ( 'NONE', ( #6224, #55335, #42870, #40804 ) ) ;
#62331 = LINE ( 'NONE', #7454, #48267 ) ;
#62332 = DIRECTION ( 'NONE',  ( -0.000000000000000000, -0.000000000000000000, -1.000000000000000000 ) ) ;
#62333 = CARTESIAN_POINT ( 'NONE',  ( 0.2646305136544065406, -12.24595685781654630, 0.1321451301297427439 ) ) ;
#62334 = CYLINDRICAL_SURFACE ( 'NONE', #59876, 2.899999999999994582 ) ;
#62335 = CIRCLE ( 'NONE', #24141, 5.000000000000000000 ) ;
#62336 = EDGE_CURVE ( 'NONE', #44318, #2190, #7456, .T. ) ;
#62337 = AXIS2_PLACEMENT_3D ( 'NONE', #62065, #16825, #16516 ) ;
#62338 = CARTESIAN_POINT ( 'NONE',  ( -26.09336990274247015, 10.32957149698990662, 6.108314406108311445 ) ) ;
#62339 = CARTESIAN_POINT ( 'NONE',  ( 1.000000000000000888, -1.530946385938423582, 7.342084388195347699 ) ) ;
#62340 = ORIENTED_EDGE ( 'NONE', *, *, #58276, .F. ) ;
#62341 = CARTESIAN_POINT ( 'NONE',  ( -37.00000000000000711, 11.47561260193585042, -5.556331110570289056 ) ) ;
#62342 = CARTESIAN_POINT ( 'NONE',  ( -27.75607595719766252, -12.49444088651119245, -5.120525247301848992 ) ) ;
#62343 = CARTESIAN_POINT ( 'NONE',  ( 1.283627346226765997, -12.47820286973617598, -1.641214790177956351 ) ) ;
#62344 = ORIENTED_EDGE ( 'NONE', *, *, #59679, .T. ) ;
#62345 = CARTESIAN_POINT ( 'NONE',  ( 0.2648978790185619880, 2.256510822326142751, 12.03635331166812783 ) ) ;
#62346 = DIRECTION ( 'NONE',  ( 0.000000000000000000, -0.8827602140260264463, 0.4698238015817460256 ) ) ;
#62347 = ADVANCED_FACE ( 'NONE', ( #58028 ), #48051, .T. ) ;
#62349 = ORIENTED_EDGE ( 'NONE', *, *, #47230, .T. ) ;
#62348 = DIRECTION ( 'NONE',  ( 1.000000000000000000, 0.000000000000000000, 0.000000000000000000 ) ) ;
#62350 = LINE ( 'NONE', #57381, #59662 ) ;
#62351 = CARTESIAN_POINT ( 'NONE',  ( -35.00000000000000000, 10.49591321039680736, 5.273331777780375873 ) ) ;
#62352 = VERTEX_POINT ( 'NONE', #62999 ) ;
#62353 = LINE ( 'NONE', #58372, #6789 ) ;
#62354 = DIRECTION ( 'NONE',  ( -1.000000000000000000, 0.000000000000000000, 0.000000000000000000 ) ) ;
#62355 = DIRECTION ( 'NONE',  ( 0.000000000000000000, 0.000000000000000000, 1.000000000000000000 ) ) ;
#62356 = DIRECTION ( 'NONE',  ( 0.000000000000000000, 0.000000000000000000, 1.000000000000000000 ) ) ;
#62357 = DIRECTION ( 'NONE',  ( 0.000000000000000000, -0.9985334138511232638, -0.05413890858542831641 ) ) ;
#62358 = CARTESIAN_POINT ( 'NONE',  ( 0.3160775863651087980, 5.922381034681598599, 10.73821170199157748 ) ) ;
#62360 = VERTEX_POINT ( 'NONE', #33404 ) ;
#62359 = FACE_OUTER_BOUND ( 'NONE', #26698, .T. ) ;
#62361 = ADVANCED_FACE ( 'NONE', ( #49048 ), #53700, .T. ) ;
#62362 = ORIENTED_EDGE ( 'NONE', *, *, #15090, .T. ) ;
#62363 = CARTESIAN_POINT ( 'NONE',  ( 35.00000000000000000, 1.171570255487609291, 11.68758509253246380 ) ) ;
#62364 = VERTEX_POINT ( 'NONE', #17460 ) ;
#62365 = APPLICATION_PROTOCOL_DEFINITION ( 'draft international standard', 'automotive_design', 1998, #65029 ) ;
#62366 = DIRECTION ( 'NONE',  ( -1.000000000000000000, 0.000000000000000000, 0.000000000000000000 ) ) ;
#62367 = CIRCLE ( 'NONE', #18864, 2.899999999999995026 ) ;
#62368 = LINE ( 'NONE', #42399, #25814 ) ;
#62369 = DIRECTION ( 'NONE',  ( 0.000000000000000000, 0.01356324068817998940, -0.9999080150203989437 ) ) ;
#62370 = ORIENTED_EDGE ( 'NONE', *, *, #56521, .T. ) ;
#62371 = CARTESIAN_POINT ( 'NONE',  ( 35.00000000000000000, -11.78745411414841726, -3.093009498343884722 ) ) ;
#62372 = CARTESIAN_POINT ( 'NONE',  ( 1.633930747250948334, -3.662223193116080466, 12.16309769563573084 ) ) ;
#62373 = ORIENTED_EDGE ( 'NONE', *, *, #45352, .T. ) ;
#62374 = VERTEX_POINT ( 'NONE', #2840 ) ;
#62375 = CARTESIAN_POINT ( 'NONE',  ( 26.44133037087954108, -12.90712213389093144, 3.963402434803054319 ) ) ;
#62376 = ORIENTED_EDGE ( 'NONE', *, *, #30812, .T. ) ;
#62377 = CARTESIAN_POINT ( 'NONE',  ( 35.00000000000000000, 4.705694406421931860E-17, -3.469127814946512892E-15 ) ) ;
#62378 = FACE_OUTER_BOUND ( 'NONE', #6318, .T. ) ;
#62379 = ADVANCED_FACE ( 'NONE', ( #23423 ), #11439, .F. ) ;
#62380 = CARTESIAN_POINT ( 'NONE',  ( 0.000000000000000000, -6.767909380267597363, -0.7805499053121327524 ) ) ;
#62381 = EDGE_CURVE ( 'NONE', #20489, #48808, #49241, .T. ) ;
#62382 = CARTESIAN_POINT ( 'NONE',  ( 1.000000000000000888, -7.484036900328561615, -0.4890722589970097345 ) ) ;
#62383 = DIRECTION ( 'NONE',  ( 1.000000000000000000, -0.000000000000000000, 0.000000000000000000 ) ) ;
#62384 = CARTESIAN_POINT ( 'NONE',  ( -35.00000000000000000, 8.496612874013292682, -9.506317355798284296 ) ) ;
#62385 = VECTOR ( 'NONE', #43209, 1000.000000000000000 ) ;
#62386 = ADVANCED_FACE ( 'NONE', ( #48705 ), #36497, .F. ) ;
#62387 = CARTESIAN_POINT ( 'NONE',  ( 35.00000000000000000, -9.240395740215580744, 7.251710744571670197 ) ) ;
#62388 = ORIENTED_EDGE ( 'NONE', *, *, #20957, .T. ) ;
#62389 = DIRECTION ( 'NONE',  ( -1.000000000000000000, 0.000000000000000000, 0.000000000000000000 ) ) ;
#62390 = ORIENTED_EDGE ( 'NONE', *, *, #48074, .F. ) ;
#62391 = ADVANCED_FACE ( 'NONE', ( #7814 ), #28097, .T. ) ;
#62392 = CARTESIAN_POINT ( 'NONE',  ( 37.00000000000000711, 5.814360711498443912, 10.70999494708485678 ) ) ;
#62393 = DIRECTION ( 'NONE',  ( 1.000000000000000000, 0.000000000000000000, 0.000000000000000000 ) ) ;
#62394 = CARTESIAN_POINT ( 'NONE',  ( -35.00000000000000000, 0.000000000000000000, 0.000000000000000000 ) ) ;
#62395 = CARTESIAN_POINT ( 'NONE',  ( -35.00000000000000000, -9.926225166347071749, 6.280308599560108007 ) ) ;
#62396 = CARTESIAN_POINT ( 'NONE',  ( 5.536195898058073439, -0.004027525919832901369, 0.007485416011288145710 ) ) ;
#62397 = LINE ( 'NONE', #62096, #12818 ) ;
#62398 = ORIENTED_EDGE ( 'NONE', *, *, #62645, .F. ) ;
#62399 = EDGE_LOOP ( 'NONE', ( #25650, #7203, #45224, #51920 ) ) ;
#62400 = CARTESIAN_POINT ( 'NONE',  ( -27.08456565417852246, 0.2166646653334106387, 2.282055114149001529 ) ) ;
#62401 = VERTEX_POINT ( 'NONE', #39037 ) ;
#62402 = DIRECTION ( 'NONE',  ( 1.000000000000000000, 0.000000000000000000, 0.000000000000000000 ) ) ;
#62403 = CYLINDRICAL_SURFACE ( 'NONE', #4873, 5.000000000000000888 ) ;
#62404 = CARTESIAN_POINT ( 'NONE',  ( 2.241352910868908310, 4.843133558968128582, 5.901537464758471074 ) ) ;
#62405 = CARTESIAN_POINT ( 'NONE',  ( -35.04709527796842394, 0.007095259204987700019, -0.01012471662515009030 ) ) ;
#62406 = ORIENTED_EDGE ( 'NONE', *, *, #41952, .T. ) ;
#62407 = CARTESIAN_POINT ( 'NONE',  ( 2.899286259009674183, 2.348384892629369336, 7.494390643303780131 ) ) ;
#62408 = DIRECTION ( 'NONE',  ( 0.000000000000000000, -0.01356324068817991828, 0.9999080150203990547 ) ) ;
#62409 = CARTESIAN_POINT ( 'NONE',  ( -28.62233190725736520, 3.138911663004114949, -13.13561239495938793 ) ) ;
#62410 = DIRECTION ( 'NONE',  ( 0.000000000000000000, -1.000000000000000000, 0.000000000000000000 ) ) ;
#62411 = CIRCLE ( 'NONE', #44376, 12.75000000000000178 ) ;
#62412 = EDGE_CURVE ( 'NONE', #20824, #51886, #21016, .T. ) ;
#62413 = CARTESIAN_POINT ( 'NONE',  ( 0.2657645697724684286, 6.253766234004070945, -10.52916014490824814 ) ) ;
#62414 = ADVANCED_FACE ( 'NONE', ( #35004 ), #40333, .T. ) ;
#62415 = CARTESIAN_POINT ( 'NONE',  ( 9.575800908719084958, -11.95193887484098028, -1.072919909436247154 ) ) ;
#62416 = VECTOR ( 'NONE', #16729, 1000.000000000000000 ) ;
#62417 = ORIENTED_EDGE ( 'NONE', *, *, #28519, .T. ) ;
#62418 = DIRECTION ( 'NONE',  ( 1.000000000000000000, 0.000000000000000000, 0.000000000000000000 ) ) ;
#62419 = ORIENTED_EDGE ( 'NONE', *, *, #17360, .T. ) ;
#62420 = AXIS2_PLACEMENT_3D ( 'NONE', #8764, #53984, #43664 ) ;
#62421 = CARTESIAN_POINT ( 'NONE',  ( 10.66646312117316420, 7.972760762573109616, -10.89565866104123515 ) ) ;
#62422 = CARTESIAN_POINT ( 'NONE',  ( -35.00000000000000000, -4.309077947445573820, -10.92721691015460550 ) ) ;
#62423 = DIRECTION ( 'NONE',  ( 0.000000000000000000, 0.000000000000000000, 1.000000000000000000 ) ) ;
#62424 = B_SPLINE_CURVE_WITH_KNOTS ( 'NONE', 3,
 ( #47477, #32154, #22866, #27840, #63393, #1915, #17861, #12520, #62409, #12209 ),
 .UNSPECIFIED., .F., .F.,
 ( 4, 2, 2, 2, 4 ),
 ( 0.002277974501771297573, 0.003563696101339898156, 0.004849417700908497872, 0.006135139300477097588, 0.007420860900045698171 ),
 .UNSPECIFIED. ) ;
#62425 = EDGE_CURVE ( 'NONE', #22366, #57124, #24777, .T. ) ;
#62426 = VECTOR ( 'NONE', #39014, 1000.000000000000000 ) ;
#62427 = CARTESIAN_POINT ( 'NONE',  ( -28.85619398320021745, 3.750539801530000439, -12.96855624952673836 ) ) ;
#62428 = DIRECTION ( 'NONE',  ( 1.000000000000000000, -0.000000000000000000, 0.000000000000000000 ) ) ;
#62429 = ORIENTED_EDGE ( 'NONE', *, *, #53366, .T. ) ;
#62430 = ORIENTED_EDGE ( 'NONE', *, *, #64460, .F. ) ;
#62431 = DIRECTION ( 'NONE',  ( 0.000000000000000000, -0.4134677391718577510, -0.9105187689795923855 ) ) ;
#62432 = VERTEX_POINT ( 'NONE', #60630 ) ;
#62433 = CARTESIAN_POINT ( 'NONE',  ( 3.352489165639872315, 5.289728451004561904, 10.77323605601821122 ) ) ;
#62434 = CARTESIAN_POINT ( 'NONE',  ( 3.427805754086258982, 7.593281694980515972, -11.19290452534897540 ) ) ;
#62435 = CARTESIAN_POINT ( 'NONE',  ( -37.00000000000000711, 2.220215194441898632, 11.98254675519229195 ) ) ;
#62436 = FACE_OUTER_BOUND ( 'NONE', #59969, .T. ) ;
#62437 = DIRECTION ( 'NONE',  ( 1.000000000000000000, 0.000000000000000000, -0.000000000000000000 ) ) ;
#62438 = CARTESIAN_POINT ( 'NONE',  ( 2.241352910868909643, -1.243507963608144751, 7.532448145350502777 ) ) ;
#62439 = CARTESIAN_POINT ( 'NONE',  ( 3.152665057734040488, 0.000000000000000000, 0.000000000000000000 ) ) ;
#62440 = ORIENTED_EDGE ( 'NONE', *, *, #25720, .F. ) ;
#62441 = EDGE_CURVE ( 'NONE', #51508, #7867, #18441, .T. ) ;
#62442 = EDGE_CURVE ( 'NONE', #46362, #21537, #15219, .T. ) ;
#62443 = CARTESIAN_POINT ( 'NONE',  ( 2.665405856346791502, -6.580881457836760262, 6.944580094494306799 ) ) ;
#62444 = ORIENTED_EDGE ( 'NONE', *, *, #1091, .T. ) ;
#62445 =( NAMED_UNIT ( * ) SI_UNIT ( $, .STERADIAN. ) SOLID_ANGLE_UNIT ( ) );
#62446 = ADVANCED_FACE ( 'NONE', ( #13752 ), #54685, .T. ) ;
#62447 = CARTESIAN_POINT ( 'NONE',  ( 21.48131883620574101, -13.31057713625612671, -2.288337088862757440 ) ) ;
#62448 = CARTESIAN_POINT ( 'NONE',  ( 1.109979610372777925, 8.414317452283274434, -9.281420052101090334 ) ) ;
#62449 = FACE_OUTER_BOUND ( 'NONE', #12512, .T. ) ;
#62450 = ORIENTED_EDGE ( 'NONE', *, *, #49656, .F. ) ;
#62451 = DIRECTION ( 'NONE',  ( -1.000000000000000000, -0.000000000000000000, 0.000000000000000000 ) ) ;
#62452 = CARTESIAN_POINT ( 'NONE',  ( -17.05023968204110574, -34.50000000000000000, -4.356789313881320957 ) ) ;
#62453 = AXIS2_PLACEMENT_3D ( 'NONE', #30174, #20191, #61090 ) ;
#62454 = DIRECTION ( 'NONE',  ( -1.000000000000000000, 0.000000000000000000, 0.000000000000000000 ) ) ;
#62455 = EDGE_LOOP ( 'NONE', ( #5591, #5071, #46098, #44449 ) ) ;
#62456 = VERTEX_POINT ( 'NONE', #29078 ) ;
#62457 = FACE_OUTER_BOUND ( 'NONE', #22458, .T. ) ;
#62458 = ORIENTED_EDGE ( 'NONE', *, *, #48774, .T. ) ;
#62459 = ORIENTED_EDGE ( 'NONE', *, *, #14959, .F. ) ;
#62460 = EDGE_LOOP ( 'NONE', ( #11259, #26068, #33655, #5388 ) ) ;
#62461 = EDGE_LOOP ( 'NONE', ( #15683, #12825, #56500, #64843 ) ) ;
#62462 = CARTESIAN_POINT ( 'NONE',  ( -22.27713295444592845, -2.673940016109006113, 2.530364014314291143 ) ) ;
#62463 = EDGE_CURVE ( 'NONE', #12785, #17303, #44936, .T. ) ;
#62465 = AXIS2_PLACEMENT_3D ( 'NONE', #11935, #32217, #37200 ) ;
#62464 = DIRECTION ( 'NONE',  ( -1.000000000000000000, 0.000000000000000000, 0.000000000000000000 ) ) ;
#62466 = CARTESIAN_POINT ( 'NONE',  ( -15.27729454824424948, 5.151216734910788908, 25.00000000000000000 ) ) ;
#62467 = FACE_OUTER_BOUND ( 'NONE', #17815, .T. ) ;
#62468 = DIRECTION ( 'NONE',  ( 1.000000000000000000, 0.000000000000000000, 0.000000000000000000 ) ) ;
#62469 = VERTEX_POINT ( 'NONE', #5117 ) ;
#62470 = EDGE_CURVE ( 'NONE', #35654, #1814, #55584, .T. ) ;
#62471 = CARTESIAN_POINT ( 'NONE',  ( 0.000000000000000000, -6.664893814313753495, 3.439359016433473748 ) ) ;
#62472 = VECTOR ( 'NONE', #37813, 1000.000000000000000 ) ;
#62473 = AXIS2_PLACEMENT_3D ( 'NONE', #805, #47027, #32362 ) ;
#62474 = ORIENTED_EDGE ( 'NONE', *, *, #29566, .F. ) ;
#62475 = CARTESIAN_POINT ( 'NONE',  ( -35.00000000000000000, -11.05394794832833583, 5.130401251914692651 ) ) ;
#62476 = DIRECTION ( 'NONE',  ( -1.000000000000000000, 0.000000000000000000, 0.000000000000000000 ) ) ;
#62477 = CARTESIAN_POINT ( 'NONE',  ( -19.56743653832046803, -30.00000000000000000, -5.000000000000000888 ) ) ;
#62478 = CARTESIAN_POINT ( 'NONE',  ( 0.3057689695767498161, -8.055876362038281613, -9.241339546505164648 ) ) ;
#62479 = CARTESIAN_POINT ( 'NONE',  ( 2.000000000000001776, 6.606214214351074254, 2.114938770769925647 ) ) ;
#62480 = CARTESIAN_POINT ( 'NONE',  ( 3.100650473569751320, -7.907988569972081550, -0.4517506188708853010 ) ) ;
#62481 = CIRCLE ( 'NONE', #22142, 5.000000000000000888 ) ;
#62482 = ORIENTED_EDGE ( 'NONE', *, *, #52571, .F. ) ;
#62483 = CARTESIAN_POINT ( 'NONE',  ( -35.00000000000000000, -11.99999999999999289, 0.000000000000000000 ) ) ;
#62484 = EDGE_CURVE ( 'NONE', #28276, #36620, #3585, .T. ) ;
#62485 = ORIENTED_EDGE ( 'NONE', *, *, #38751, .F. ) ;
#62486 = FACE_OUTER_BOUND ( 'NONE', #41407, .T. ) ;
#62487 = DIRECTION ( 'NONE',  ( 0.000000000000000000, -0.8169148498130212044, 0.5767582926625058892 ) ) ;
#62488 = CARTESIAN_POINT ( 'NONE',  ( 1.719304012341537957, 12.20344780066137602, -3.626341562669237906 ) ) ;
#62489 = CARTESIAN_POINT ( 'NONE',  ( 2.655192694323502245, 5.716669423975853093, -7.714239566601391651 ) ) ;
#62490 = CARTESIAN_POINT ( 'NONE',  ( 2.258463476536644254, -6.683417898966903969, 3.701774005560837466 ) ) ;
#62491 = ORIENTED_EDGE ( 'NONE', *, *, #22989, .F. ) ;
#62492 = DIRECTION ( 'NONE',  ( -1.000000000000000000, 0.000000000000000000, 0.000000000000000000 ) ) ;
#62493 = CARTESIAN_POINT ( 'NONE',  ( -37.00000000000000711, -12.42372387097880626, -2.865935305911759379 ) ) ;
#62494 = DIRECTION ( 'NONE',  ( 0.000000000000000000, 0.3193015301359806712, -0.9476531711828022342 ) ) ;
#62495 = CARTESIAN_POINT ( 'NONE',  ( -3.351502423664876495, 12.75501326137288771, 4.438561732491696610 ) ) ;
#62496 = CIRCLE ( 'NONE', #4129, 5.000000000000001776 ) ;
#62497 = ADVANCED_FACE ( 'NONE', ( #39698 ), #49387, .T. ) ;
#62498 = CARTESIAN_POINT ( 'NONE',  ( -22.71097035706202405, -2.846599994298329328, 4.089776368546542251 ) ) ;
#62499 = ORIENTED_EDGE ( 'NONE', *, *, #23791, .F. ) ;
#62500 = VECTOR ( 'NONE', #32379, 1000.000000000000000 ) ;
#62501 = B_SPLINE_CURVE_WITH_KNOTS ( 'NONE', 3,
 ( #26165, #5568, #14836, #46127, #4908, #41102, #35777, #60750, #61078, #15190, #29817, #56413, #10859, #35122, #50462, #25839, #10199, #576, #9526 ),
 .UNSPECIFIED., .F., .F.,
 ( 4, 3, 3, 3, 3, 3, 4 ),
 ( 7.714043218345438553E-18, 4.457896483015216620E-05, 6.639290541542676644E-05, 8.820687556479619128E-05, 0.0001100173248779016537, 0.0001545671401658254380, 0.0001830328308068593899 ),
 .UNSPECIFIED. ) ;
#62502 = UNCERTAINTY_MEASURE_WITH_UNIT (LENGTH_MEASURE( 1.000000000000000082E-05 ), #50461, 'distance_accuracy_value', 'NONE');
#62503 = CARTESIAN_POINT ( 'NONE',  ( 2.941278708680199916, -5.248410529370202582, -3.185832147968502781 ) ) ;
#62504 = CARTESIAN_POINT ( 'NONE',  ( 1.198791140419927403, -5.826488554585672830, -11.12379938352737341 ) ) ;
#62505 = CIRCLE ( 'NONE', #52985, 5.000000000000000000 ) ;
#62506 = EDGE_CURVE ( 'NONE', #52387, #5064, #19091, .T. ) ;
#62507 = ORIENTED_EDGE ( 'NONE', *, *, #43508, .T. ) ;
#62508 = AXIS2_PLACEMENT_3D ( 'NONE', #43116, #42792, #17212 ) ;
#62509 = ORIENTED_EDGE ( 'NONE', *, *, #15216, .F. ) ;
#62511 =( BOUNDED_SURFACE ( )  B_SPLINE_SURFACE ( 3, 1, ( 
 ( #5714, #29630 ),
 ( #49937, #1701 ),
 ( #47899, #2013 ),
 ( #42545, #56568 ) ),
 .UNSPECIFIED., .F., .F., .F. ) 
 B_SPLINE_SURFACE_WITH_KNOTS ( ( 4, 4 ),
 ( 2, 2 ),
 ( 0.000000000000000000, 1.000000000000000000 ),
 ( 0.000000000000000000, 1.000000000000000000 ),
 .UNSPECIFIED. ) 
 GEOMETRIC_REPRESENTATION_ITEM ( )  RATIONAL_B_SPLINE_SURFACE ( (
 ( 1.000000000000000000, 1.000000000000000000),
 ( 0.9942764183789327692, 0.8450855930916580938),
 ( 0.9942764183789327692, 0.8450855930916580938),
 ( 1.000000000000000000, 1.000000000000000000) ) ) 
 REPRESENTATION_ITEM ( '' )  SURFACE ( )  );
#62510 = DIRECTION ( 'NONE',  ( 0.000000000000000000, -0.5155538571770286183, 0.8568571761675851661 ) ) ;
#62512 = DIRECTION ( 'NONE',  ( -1.000000000000000000, 0.000000000000000000, -0.000000000000000000 ) ) ;
#62513 = DIRECTION ( 'NONE',  ( 0.000000000000000000, -0.01356324068817999114, 0.9999080150203989437 ) ) ;
#62514 = CIRCLE ( 'NONE', #33855, 4.999999999999999112 ) ;
#62515 = CARTESIAN_POINT ( 'NONE',  ( 0.3164563675027642353, -1.892265234253194706, 12.11636128244743205 ) ) ;
#62516 = ORIENTED_EDGE ( 'NONE', *, *, #9737, .F. ) ;
#62517 = EDGE_CURVE ( 'NONE', #61730, #43263, #25818, .T. ) ;
#62518 = ORIENTED_EDGE ( 'NONE', *, *, #59029, .F. ) ;
#62519 = AXIS2_PLACEMENT_3D ( 'NONE', #41380, #41720, #11456 ) ;
#62520 = VERTEX_POINT ( 'NONE', #16711 ) ;
#62521 = CARTESIAN_POINT ( 'NONE',  ( 35.00000000000000000, 9.821084925794670184, 7.215058775251142364 ) ) ;
#62522 = LINE ( 'NONE', #6698, #65046 ) ;
#62523 = VERTEX_POINT ( 'NONE', #21379 ) ;
#62524 = CARTESIAN_POINT ( 'NONE',  ( -18.06530682554817702, 4.745038755617106752, -11.02423958223924139 ) ) ;
#62525 = DIRECTION ( 'NONE',  ( -1.000000000000000000, 0.000000000000000000, -0.000000000000000000 ) ) ;
#62526 = ORIENTED_EDGE ( 'NONE', *, *, #58816, .F. ) ;
#62527 = CARTESIAN_POINT ( 'NONE',  ( -27.08423923533013777, -0.2759775751761929241, -2.274768056034775388 ) ) ;
#62528 = CARTESIAN_POINT ( 'NONE',  ( 18.18435566811113446, -29.77699652454512957, -8.006764386360391228 ) ) ;
#62529 = CARTESIAN_POINT ( 'NONE',  ( 2.268878695254623601, 7.130600918714364411, 2.752970156155734038 ) ) ;
#62530 = VERTEX_POINT ( 'NONE', #60973 ) ;
#62531 = LINE ( 'NONE', #52600, #48022 ) ;
#62532 = ORIENTED_EDGE ( 'NONE', *, *, #29389, .F. ) ;
#62533 = CARTESIAN_POINT ( 'NONE',  ( -37.00000000000000711, -12.57916205664480103, -2.080187960898693511 ) ) ;
#62534 = CARTESIAN_POINT ( 'NONE',  ( -18.73860168220982914, -4.849834184236166301, 12.60028275727231772 ) ) ;
#62535 = FACE_OUTER_BOUND ( 'NONE', #8146, .T. ) ;
#62536 = DIRECTION ( 'NONE',  ( 1.000000000000000000, 0.000000000000000000, 0.000000000000000000 ) ) ;
#62538 = DIRECTION ( 'NONE',  ( -0.9688695217174484453, 0.000000000000000000, 0.2475719085175105139 ) ) ;
#62537 = CIRCLE ( 'NONE', #32817, 12.74999999999999822 ) ;
#62539 = CARTESIAN_POINT ( 'NONE',  ( 35.00000000000000000, 4.705694406421931860E-17, -3.469127814946512892E-15 ) ) ;
#62540 = CARTESIAN_POINT ( 'NONE',  ( 37.00000000000000711, 4.705694406421931860E-17, -3.469127814946512892E-15 ) ) ;
#62541 = FACE_OUTER_BOUND ( 'NONE', #19284, .T. ) ;
#62542 = VERTEX_POINT ( 'NONE', #16404 ) ;
#62543 = DIRECTION ( 'NONE',  ( 0.9582930651793754029, 0.1596922922278031787, 0.2370079598497637219 ) ) ;
#62544 = ORIENTED_EDGE ( 'NONE', *, *, #39437, .F. ) ;
#62545 = CONICAL_SURFACE ( 'NONE', #33886, 14.13397459621556251, 0.5235987755983000369 ) ;
#62546 = CARTESIAN_POINT ( 'NONE',  ( 1.452237505248555660, -1.611965288198815127, 12.55261342181974982 ) ) ;
#62547 = DIRECTION ( 'NONE',  ( 0.000000000000000000, -0.9346839223284579834, 0.3554799084908866202 ) ) ;
#62548 = VERTEX_POINT ( 'NONE', #21037 ) ;
#62549 = CARTESIAN_POINT ( 'NONE',  ( 35.00000000000000000, -1.039216533672818299, 11.70009620280412399 ) ) ;
#62550 = CARTESIAN_POINT ( 'NONE',  ( -35.00000000000000000, -11.32068061209291265, -5.865551165831199398 ) ) ;
#62551 = CARTESIAN_POINT ( 'NONE',  ( 0.2650492594609241137, -9.309909082761093302, -7.955687020697146394 ) ) ;
#62553 = EDGE_CURVE ( 'NONE', #43307, #60788, #46987, .T. ) ;
#62552 = ORIENTED_EDGE ( 'NONE', *, *, #34746, .T. ) ;
#62554 = ORIENTED_EDGE ( 'NONE', *, *, #39463, .T. ) ;
#62555 = CARTESIAN_POINT ( 'NONE',  ( 1.452237505248555660, -7.672309600508763872, 10.06489946308199634 ) ) ;
#62556 = CIRCLE ( 'NONE', #28584, 2.899999999999994582 ) ;
#62557 = VERTEX_POINT ( 'NONE', #11394 ) ;
#62558 = CARTESIAN_POINT ( 'NONE',  ( 2.177405672431943273, -10.73538068360496922, -3.189307221897523803 ) ) ;
#62559 = DIRECTION ( 'NONE',  ( -1.000000000000000000, 0.000000000000000000, 0.000000000000000000 ) ) ;
#62560 = FACE_OUTER_BOUND ( 'NONE', #54046, .T. ) ;
#62561 = CARTESIAN_POINT ( 'NONE',  ( 2.000000000000001776, 6.767909380267589370, 0.7805499053121639497 ) ) ;
#62562 = CARTESIAN_POINT ( 'NONE',  ( -7.181456785175555524, 5.890186129966279438, -10.45493698471458188 ) ) ;
#62563 = ORIENTED_EDGE ( 'NONE', *, *, #64329, .F. ) ;
#62564 = CIRCLE ( 'NONE', #2069, 12.75000000000000178 ) ;
#62565 = DIRECTION ( 'NONE',  ( -1.000000000000000000, -0.000000000000000000, 0.000000000000000000 ) ) ;
#62566 = EDGE_CURVE ( 'NONE', #61436, #7150, #45997, .T. ) ;
#62567 = EDGE_CURVE ( 'NONE', #29292, #45191, #17015, .T. ) ;
#62568 = CARTESIAN_POINT ( 'NONE',  ( 3.291290029914074378, 8.250315036047103590, 8.713914264323182834 ) ) ;
#62569 = CYLINDRICAL_SURFACE ( 'NONE', #57491, 12.18650000000000055 ) ;
#62570 = ADVANCED_FACE ( 'NONE', ( #57291 ), #31995, .T. ) ;
#62571 = CARTESIAN_POINT ( 'NONE',  ( 3.152665057735716037, -2.258875078500806044, 7.609997527621833235 ) ) ;
#62572 = DIRECTION ( 'NONE',  ( 1.000000000000000000, 0.000000000000000000, 0.000000000000000000 ) ) ;
#62573 = EDGE_CURVE ( 'NONE', #14653, #37445, #52316, .T. ) ;
#62574 = CARTESIAN_POINT ( 'NONE',  ( -9.351388602708162523, -11.42638970207761950, -3.665735721005252135 ) ) ;
#62575 = CARTESIAN_POINT ( 'NONE',  ( 1.372161826076013780, 4.864129100816595219, 11.63973780005242453 ) ) ;
#62576 = FACE_OUTER_BOUND ( 'NONE', #8427, .T. ) ;
#62577 = AXIS2_PLACEMENT_3D ( 'NONE', #39850, #13588, #39519 ) ;
#62578 = EDGE_CURVE ( 'NONE', #47123, #64495, #21727, .T. ) ;
#62579 = ORIENTED_EDGE ( 'NONE', *, *, #8526, .F. ) ;
#62580 = CARTESIAN_POINT ( 'NONE',  ( 5.514624014163232779, -0.003668383633201705799, -0.001921576324372078603 ) ) ;
#62581 = PLANE ( 'NONE',  #22435 ) ;
#62582 = EDGE_LOOP ( 'NONE', ( #23789, #59588, #36941, #22863, #18666, #47825 ) ) ;
#62583 = CIRCLE ( 'NONE', #33935, 12.18650000000000055 ) ;
#62584 = CARTESIAN_POINT ( 'NONE',  ( 0.9232058338315058954, 2.536181247095365077, 12.21058493388774302 ) ) ;
#62585 = EDGE_CURVE ( 'NONE', #39733, #14759, #32212, .T. ) ;
#62586 = CARTESIAN_POINT ( 'NONE',  ( 2.000000000000001776, 0.000000000000000000, 0.000000000000000000 ) ) ;
#62587 = VERTEX_POINT ( 'NONE', #61285 ) ;
#62588 = CARTESIAN_POINT ( 'NONE',  ( 2.242819959140783137, 6.560218843829382251, 3.905785747114707718 ) ) ;
#62589 = VERTEX_POINT ( 'NONE', #56648 ) ;
#62590 = DIRECTION ( 'NONE',  ( -1.000000000000000000, 0.000000000000000000, 0.000000000000000000 ) ) ;
#62591 = ORIENTED_EDGE ( 'NONE', *, *, #24082, .T. ) ;
#62592 = EDGE_LOOP ( 'NONE', ( #25708, #31464, #12342, #1771 ) ) ;
#62593 = VECTOR ( 'NONE', #11335, 1000.000000000000000 ) ;
#62594 = CYLINDRICAL_SURFACE ( 'NONE', #14617, 5.000000000000000888 ) ;
#62595 = ORIENTED_EDGE ( 'NONE', *, *, #30117, .T. ) ;
#62596 = EDGE_CURVE ( 'NONE', #7749, #44332, #14641, .T. ) ;
#62597 = CYLINDRICAL_SURFACE ( 'NONE', #22782, 7.499999999999988454 ) ;
#62598 = CARTESIAN_POINT ( 'NONE',  ( -22.27706485742869091, -3.563814065926672381, 0.9221835209182321913 ) ) ;
#62599 = AXIS2_PLACEMENT_3D ( 'NONE', #5797, #26064, #41326 ) ;
#62600 = LINE ( 'NONE', #41341, #29070 ) ;
#62601 = VERTEX_POINT ( 'NONE', #15715 ) ;
#62602 = CARTESIAN_POINT ( 'NONE',  ( 0.3057689695767464300, -7.702054583838531698, 9.538231270095076653 ) ) ;
#62603 = CARTESIAN_POINT ( 'NONE',  ( 10.20102756488484275, -26.83656875578374112, 13.80782716569073010 ) ) ;
#62604 = CARTESIAN_POINT ( 'NONE',  ( 2.430348790457650399, -7.694949746373904276, 0.1949172018040290222 ) ) ;
#62606 = ORIENTED_EDGE ( 'NONE', *, *, #42882, .T. ) ;
#62605 = CYLINDRICAL_SURFACE ( 'NONE', #3256, 7.499999999999988454 ) ;
#62607 = CARTESIAN_POINT ( 'NONE',  ( -35.00000000000000000, 2.936739658820028520, -11.37311665002360783 ) ) ;
#62608 = ORIENTED_EDGE ( 'NONE', *, *, #47808, .F. ) ;
#62609 = CARTESIAN_POINT ( 'NONE',  ( -35.00000000000000000, 11.73463472867576129, 3.287724142101457137 ) ) ;
#62610 = VECTOR ( 'NONE', #36871, 1000.000000000000114 ) ;
#62611 = ORIENTED_EDGE ( 'NONE', *, *, #30193, .T. ) ;
#62612 = CARTESIAN_POINT ( 'NONE',  ( 22.61346430089559334, -9.960673739116366221, -6.702005469580054609 ) ) ;
#62613 = FACE_OUTER_BOUND ( 'NONE', #12517, .T. ) ;
#62614 = DIRECTION ( 'NONE',  ( 1.000000000000000000, -0.000000000000000000, 0.000000000000000000 ) ) ;
#62615 = ORIENTED_EDGE ( 'NONE', *, *, #3771, .F. ) ;
#62616 = DIRECTION ( 'NONE',  ( 1.000000000000000000, -0.000000000000000000, 0.000000000000000000 ) ) ;
#62617 = CARTESIAN_POINT ( 'NONE',  ( -4.975205859172452172, -1.416020129149132778, -11.91616074890918675 ) ) ;
#62618 = CARTESIAN_POINT ( 'NONE',  ( -35.00000000000000000, 0.000000000000000000, 0.000000000000000000 ) ) ;
#62619 = EDGE_LOOP ( 'NONE', ( #25241, #39198, #54076, #12448 ) ) ;
#62620 = VERTEX_POINT ( 'NONE', #35992 ) ;
#62621 = CARTESIAN_POINT ( 'NONE',  ( 2.705197763288545332, 7.617149697727742641, 1.627208841526486038 ) ) ;
#62622 = ORIENTED_EDGE ( 'NONE', *, *, #28426, .T. ) ;
#62623 = B_SPLINE_CURVE_WITH_KNOTS ( 'NONE', 3,
 ( #65469, #19933, #36542, #56849, #14919, #29906, #55516 ),
 .UNSPECIFIED., .F., .F.,
 ( 4, 3, 4 ),
 ( 0.000000000000000000, 0.001700533616330574633, 0.005002426799371369366 ),
 .UNSPECIFIED. ) ;
#62624 = ORIENTED_EDGE ( 'NONE', *, *, #45132, .F. ) ;
#62625 = FACE_OUTER_BOUND ( 'NONE', #25821, .T. ) ;
#62626 = CARTESIAN_POINT ( 'NONE',  ( 1.194176325881343592, -10.60746084433560199, 6.717888447700793186 ) ) ;
#62627 = CARTESIAN_POINT ( 'NONE',  ( 3.152665057734125309, -6.622010822086626725, -4.377619405892440696 ) ) ;
#62628 = CARTESIAN_POINT ( 'NONE',  ( 36.00000000000000711, -2.696588552979145348, -12.46157735505188491 ) ) ;
#62629 = FACE_OUTER_BOUND ( 'NONE', #48819, .T. ) ;
#62630 = EDGE_CURVE ( 'NONE', #56943, #21481, #23389, .T. ) ;
#62631 = DIRECTION ( 'NONE',  ( -1.000000000000000000, 0.000000000000000000, 0.000000000000000000 ) ) ;
#62632 = VECTOR ( 'NONE', #35909, 1000.000000000000000 ) ;
#62633 = CIRCLE ( 'NONE', #61591, 4.999999999999999112 ) ;
#62634 = CARTESIAN_POINT ( 'NONE',  ( 22.68150004936238773, 3.158880575389232614, -11.57756885178368478 ) ) ;
#62635 = ORIENTED_EDGE ( 'NONE', *, *, #18181, .F. ) ;
#62636 = DIRECTION ( 'NONE',  ( 0.000000000000000000, 0.01356324068817998940, -0.9999080150203990547 ) ) ;
#62637 = DIRECTION ( 'NONE',  ( 0.000000000000000000, 0.000000000000000000, -1.000000000000000000 ) ) ;
#62638 = AXIS2_PLACEMENT_3D ( 'NONE', #2189, #13148, #63663 ) ;
#62639 = LINE ( 'NONE', #53013, #530 ) ;
#62640 = CARTESIAN_POINT ( 'NONE',  ( 2.000000000000001776, -5.097042323172487954, 5.501832381651415638 ) ) ;
#62641 = EDGE_CURVE ( 'NONE', #26234, #12277, #58247, .T. ) ;
#62642 = DIRECTION ( 'NONE',  ( -1.000000000000000000, 0.000000000000000000, -0.000000000000000000 ) ) ;
#62643 = VECTOR ( 'NONE', #23530, 1000.000000000000000 ) ;
#62644 = CARTESIAN_POINT ( 'NONE',  ( 22.57855258442564761, -4.427776684447072952, -12.75322679295976691 ) ) ;
#62645 = EDGE_CURVE ( 'NONE', #24342, #4186, #26555, .T. ) ;
#62646 = PLANE ( 'NONE',  #58612 ) ;
#62647 = EDGE_CURVE ( 'NONE', #50772, #8493, #42283, .T. ) ;
#62648 = EDGE_LOOP ( 'NONE', ( #29196, #44284, #32653, #15067 ) ) ;
#62649 = CARTESIAN_POINT ( 'NONE',  ( -27.08429572838383947, 0.5764601019426045525, 2.217805374070519253 ) ) ;
#62650 = CARTESIAN_POINT ( 'NONE',  ( 0.3537226245948370540, -1.874138792912929619, -12.13174752084888119 ) ) ;
#62651 = CARTESIAN_POINT ( 'NONE',  ( -37.00000000000000711, 4.603882218679707705, -10.80631716521661900 ) ) ;
#62652 = CARTESIAN_POINT ( 'NONE',  ( 4.037157412408303976E-12, -31.03649492335491544, 14.44372008463339085 ) ) ;
#62653 = AXIS2_PLACEMENT_3D ( 'NONE', #31784, #20843, #582 ) ;
#62654 = EDGE_CURVE ( 'NONE', #8110, #5463, #24913, .T. ) ;
#62655 = CYLINDRICAL_SURFACE ( 'NONE', #13929, 2.899999999999994582 ) ;
#62656 = CARTESIAN_POINT ( 'NONE',  ( -24.95436193843509187, -11.16571467309113075, 7.594604397006440522 ) ) ;
#62657 = AXIS2_PLACEMENT_3D ( 'NONE', #19378, #60248, #9699 ) ;
#62658 = ORIENTED_EDGE ( 'NONE', *, *, #12428, .T. ) ;
#62659 = CARTESIAN_POINT ( 'NONE',  ( 2.241352910868908310, -0.08337961031698915004, -7.633946224498474820 ) ) ;
#62660 = CARTESIAN_POINT ( 'NONE',  ( -27.73793999403614663, -12.15445282031313035, -5.902762415843590738 ) ) ;
#62661 = ADVANCED_FACE ( 'NONE', ( #62576 ), #32973, .T. ) ;
#62662 = DIRECTION ( 'NONE',  ( 1.000000000000000000, 0.000000000000000000, 0.000000000000000000 ) ) ;
#62663 = CARTESIAN_POINT ( 'NONE',  ( -35.04709527796842394, -0.007030359780627049027, 0.01016988845956717791 ) ) ;
#62664 = VERTEX_POINT ( 'NONE', #47971 ) ;
#62665 = CARTESIAN_POINT ( 'NONE',  ( 2.903928887688247418, -6.365315087929495519, 6.032681461746848939 ) ) ;
#62666 = DIRECTION ( 'NONE',  ( 1.000000000000000000, -0.000000000000000000, 0.000000000000000000 ) ) ;
#62667 = EDGE_CURVE ( 'NONE', #57486, #65758, #20550, .T. ) ;
#62669 = VERTEX_POINT ( 'NONE', #27662 ) ;
#62668 = CARTESIAN_POINT ( 'NONE',  ( -37.00000000000000711, -7.215058775251327994, 9.821084925794545839 ) ) ;
#62670 = DIRECTION ( 'NONE',  ( 0.000000000000000000, 0.000000000000000000, 1.000000000000000000 ) ) ;
#62671 = ADVANCED_FACE ( 'NONE', ( #33326 ), #28335, .T. ) ;
#62672 = CIRCLE ( 'NONE', #8527, 5.000000000000000000 ) ;
#62673 = AXIS2_PLACEMENT_3D ( 'NONE', #57604, #12347, #13017 ) ;
#62674 = VECTOR ( 'NONE', #33899, 1000.000000000000000 ) ;
#62675 = DIRECTION ( 'NONE',  ( 0.000000000000000000, -0.9551603052523447435, 0.2960891610144610886 ) ) ;
#62676 = ORIENTED_EDGE ( 'NONE', *, *, #13121, .F. ) ;
#62677 = EDGE_CURVE ( 'NONE', #10925, #43149, #3755, .T. ) ;
#62678 = CARTESIAN_POINT ( 'NONE',  ( -37.00000000000000711, 3.511814412392118445, 11.66953048682401040 ) ) ;
#62679 = LINE ( 'NONE', #41758, #30881 ) ;
#62680 = DIRECTION ( 'NONE',  ( -1.000000000000000000, 0.000000000000000000, 0.000000000000000000 ) ) ;
#62681 = CARTESIAN_POINT ( 'NONE',  ( 2.889800649504073782, 5.728825117897737407, -2.156828754871411125 ) ) ;
#62682 = DIRECTION ( 'NONE',  ( -1.000000000000000000, 0.000000000000000000, 0.000000000000000000 ) ) ;
#62683 = ADVANCED_FACE ( 'NONE', ( #64871 ), #64543, .T. ) ;
#62684 = CARTESIAN_POINT ( 'NONE',  ( 35.00000000000000000, 7.094637218249506994, 10.59380114696461739 ) ) ;
#62686 = ORIENTED_EDGE ( 'NONE', *, *, #50892, .F. ) ;
#62685 = CARTESIAN_POINT ( 'NONE',  ( 2.000000000000001776, 1.018311147294260977, -6.861346417234475581 ) ) ;
#62687 = CARTESIAN_POINT ( 'NONE',  ( 9.147009959156623182, 5.797999425567116560, 12.19668806932873295 ) ) ;
#62688 = EDGE_LOOP ( 'NONE', ( #34061, #45287, #30802, #28766 ) ) ;
#62689 = CARTESIAN_POINT ( 'NONE',  ( 37.00000000000000711, -5.130401251914806338, -11.05394794832827898 ) ) ;
#62690 = ORIENTED_EDGE ( 'NONE', *, *, #55883, .F. ) ;
#62691 = B_SPLINE_CURVE_WITH_KNOTS ( 'NONE', 3,
 ( #57445, #62106, #47473, #11550, #1604, #63389, #17205 ),
 .UNSPECIFIED., .F., .F.,
 ( 4, 3, 4 ),
 ( 0.0001321430428585257952, 0.0001982171734706201550, 0.0002642860854759486087 ),
 .UNSPECIFIED. ) ;
#62692 = DIRECTION ( 'NONE',  ( 1.000000000000000000, 0.000000000000000000, 0.000000000000000000 ) ) ;
#62693 = AXIS2_PLACEMENT_3D ( 'NONE', #9442, #31694, #61978 ) ;
#62694 = CARTESIAN_POINT ( 'NONE',  ( 37.00000000000000711, -7.110831038798346881, -9.896810808925367908 ) ) ;
#62695 = CARTESIAN_POINT ( 'NONE',  ( -47.45484198363494954, -0.5059748548177152028, 8.508429091481763962 ) ) ;
#62696 = CARTESIAN_POINT ( 'NONE',  ( 35.00000000000000000, 4.705694406421931860E-17, -3.469127814946512892E-15 ) ) ;
#62698 = ORIENTED_EDGE ( 'NONE', *, *, #45762, .F. ) ;
#62697 = VECTOR ( 'NONE', #61276, 1000.000000000000000 ) ;
#62699 = VECTOR ( 'NONE', #35945, 1000.000000000000227 ) ;
#62700 =( BOUNDED_SURFACE ( )  B_SPLINE_SURFACE ( 3, 1, ( 
 ( #26180, #57418 ),
 ( #262, #42101 ),
 ( #10533, #36122 ),
 ( #41444, #11850 ) ),
 .UNSPECIFIED., .F., .F., .F. ) 
 B_SPLINE_SURFACE_WITH_KNOTS ( ( 4, 4 ),
 ( 2, 2 ),
 ( 0.000000000000000000, 1.000000000000000000 ),
 ( 0.000000000000000000, 1.000000000000000000 ),
 .UNSPECIFIED. ) 
 GEOMETRIC_REPRESENTATION_ITEM ( )  RATIONAL_B_SPLINE_SURFACE ( (
 ( 1.000000000000000000, 1.000000000000000000),
 ( 0.8716676215708681896, 0.8964445200148164483),
 ( 0.8716676215708681896, 0.8964445200148164483),
 ( 1.000000000000000000, 1.000000000000000000) ) ) 
 REPRESENTATION_ITEM ( '' )  SURFACE ( )  );
#62701 = CYLINDRICAL_SURFACE ( 'NONE', #33999, 4.999999999999999112 ) ;
#62702 = ORIENTED_EDGE ( 'NONE', *, *, #16363, .F. ) ;
#62703 = ORIENTED_EDGE ( 'NONE', *, *, #8242, .F. ) ;
#62704 = CARTESIAN_POINT ( 'NONE',  ( 2.241352910868908754, -7.202080440908725123, -2.532612177304514933 ) ) ;
#62705 = ORIENTED_EDGE ( 'NONE', *, *, #37164, .T. ) ;
#62706 = AXIS2_PLACEMENT_3D ( 'NONE', #50236, #9001, #25600 ) ;
#62707 = DIRECTION ( 'NONE',  ( 0.000000000000000000, 0.01356324068817991828, -0.9999080150203990547 ) ) ;
#62708 = CARTESIAN_POINT ( 'NONE',  ( 5.515188684475870851, 0.004804816249378827432, -0.002355816063606946259 ) ) ;
#62709 = CARTESIAN_POINT ( 'NONE',  ( 12.47628546223243617, 0.000000000000000000, 11.99999999999999645 ) ) ;
#62710 = DIRECTION ( 'NONE',  ( -1.000000000000000000, 0.000000000000000000, -0.000000000000000000 ) ) ;
#62711 = EDGE_CURVE ( 'NONE', #56883, #27273, #44933, .T. ) ;
#62712 = LINE ( 'NONE', #7873, #35172 ) ;
#62713 = CARTESIAN_POINT ( 'NONE',  ( 3.100650473569745547, -7.866294126167263201, 0.9283202922944633340 ) ) ;
#62714 = DIRECTION ( 'NONE',  ( 1.000000000000000000, 0.000000000000000000, 0.000000000000000000 ) ) ;
#62715 = CIRCLE ( 'NONE', #43592, 5.000000000000000888 ) ;
#62716 = ORIENTED_EDGE ( 'NONE', *, *, #55778, .T. ) ;
#62717 = DIRECTION ( 'NONE',  ( 0.000000000000000000, 0.000000000000000000, 1.000000000000000000 ) ) ;
#62718 = ORIENTED_EDGE ( 'NONE', *, *, #23367, .F. ) ;
#62719 = AXIS2_PLACEMENT_3D ( 'NONE', #6523, #36449, #26798 ) ;
#62720 = CARTESIAN_POINT ( 'NONE',  ( -35.00000000000000000, 11.02904044024209185, -4.041347439435899247 ) ) ;
#62721 = CARTESIAN_POINT ( 'NONE',  ( -35.00000000000000000, -12.17626345777664021, 0.4993900848166987760 ) ) ;
#62722 = CARTESIAN_POINT ( 'NONE',  ( 2.491965175173876723, -2.837956678388268816, -7.177226758613644897 ) ) ;
#62723 = ADVANCED_FACE ( 'NONE', ( #55237 ), #29314, .T. ) ;
#62724 = B_SPLINE_CURVE_WITH_KNOTS ( 'NONE', 3,
 ( #57764, #26826, #7188, #21520, #16841, #37788, #51784, #56790, #17178, #6557, #1580, #52447, #47127, #6885, #1890, #47768 ),
 .UNSPECIFIED., .F., .F.,
 ( 4, 3, 3, 3, 3, 4 ),
 ( 0.000000000000000000, 0.0003017745587525228618, 0.0006035491769808714636, 0.0009053241094668154892, 0.001207275924539020053, 0.001510325902531028941 ),
 .UNSPECIFIED. ) ;
#62725 = CARTESIAN_POINT ( 'NONE',  ( -35.00000000000000000, 12.14284015767850100, 1.030638227056609679 ) ) ;
#62726 = EDGE_LOOP ( 'NONE', ( #29995, #31557, #43000, #32861 ) ) ;
#62727 = CIRCLE ( 'NONE', #49988, 4.999999999999999112 ) ;
#62728 = ORIENTED_EDGE ( 'NONE', *, *, #4375, .T. ) ;
#62729 = CIRCLE ( 'NONE', #22394, 5.000000000000000000 ) ;
#62730 = EDGE_CURVE ( 'NONE', #2869, #42754, #43962, .T. ) ;
#62731 = CARTESIAN_POINT ( 'NONE',  ( 5.514624014163232779, -0.004104370840204392586, -0.0005510299962881638107 ) ) ;
#62732 = VERTEX_POINT ( 'NONE', #19018 ) ;
#62733 = CIRCLE ( 'NONE', #29840, 12.74999999999999822 ) ;
#62734 = CARTESIAN_POINT ( 'NONE',  ( 0.2958664285830439056, 7.708042451272294926, -9.529149585189859550 ) ) ;
#62735 = CARTESIAN_POINT ( 'NONE',  ( 37.00000000000000711, 9.321877890560537949, 7.146664589317804683 ) ) ;
#62736 = CARTESIAN_POINT ( 'NONE',  ( 0.7400311444011723472, -9.726551103566755785, -7.698344902199187878 ) ) ;
#62737 = CARTESIAN_POINT ( 'NONE',  ( -22.30625920655495165, 1.076742202099183254, 3.635849356906398544 ) ) ;
#62738 = EDGE_CURVE ( 'NONE', #54185, #54568, #39619, .T. ) ;
#62739 = EDGE_LOOP ( 'NONE', ( #13780, #57175, #5150, #57743 ) ) ;
#62740 = CYLINDRICAL_SURFACE ( 'NONE', #40954, 4.999999999999998224 ) ;
#62741 = CARTESIAN_POINT ( 'NONE',  ( -35.00000000000000000, 0.000000000000000000, 0.000000000000000000 ) ) ;
#62742 = CARTESIAN_POINT ( 'NONE',  ( 2.781367136452695288, -1.052455537429601851, 7.743208838465638344 ) ) ;
#62743 = CARTESIAN_POINT ( 'NONE',  ( 145.1370849898475797, 3.309064568108273190E-14, 0.000000000000000000 ) ) ;
#62744 = AXIS2_PLACEMENT_3D ( 'NONE', #44790, #65072, #29190 ) ;
#62745 = AXIS2_PLACEMENT_3D ( 'NONE', #53698, #44662, #54354 ) ;
#62746 = AXIS2_PLACEMENT_3D ( 'NONE', #52225, #58182, #6025 ) ;
#62747 = CARTESIAN_POINT ( 'NONE',  ( -17.83419946441818027, -9.720786832536937538, 7.036071585506806336 ) ) ;
#62748 = DIRECTION ( 'NONE',  ( 0.000000000000000000, -0.01356324068817998940, 0.9999080150203990547 ) ) ;
#62749 = ORIENTED_EDGE ( 'NONE', *, *, #47986, .F. ) ;
#62750 = AXIS2_PLACEMENT_3D ( 'NONE', #5933, #1254, #36132 ) ;
#62751 = CARTESIAN_POINT ( 'NONE',  ( 0.2638984909335716500, 6.295352574289132974, -10.50550771760513591 ) ) ;
#62752 = ORIENTED_EDGE ( 'NONE', *, *, #39092, .F. ) ;
#62753 = CARTESIAN_POINT ( 'NONE',  ( -35.00000000000000000, -11.73463472867573643, -3.287724142101541958 ) ) ;
#62754 = DIRECTION ( 'NONE',  ( 1.000000000000000000, 0.000000000000000000, 0.000000000000000000 ) ) ;
#62755 = FACE_OUTER_BOUND ( 'NONE', #7232, .T. ) ;
#62756 = CIRCLE ( 'NONE', #47925, 2.899999999999996803 ) ;
#62757 = CARTESIAN_POINT ( 'NONE',  ( 1.375507693217066008, 12.60244951981694150, 0.5913006932453851450 ) ) ;
#62758 = CARTESIAN_POINT ( 'NONE',  ( 3.386626873725977038, -10.78029969106401253, 8.130803614474325869 ) ) ;
#62759 = ADVANCED_FACE ( 'NONE', ( #39616 ), #65524, .T. ) ;
#62760 = ORIENTED_EDGE ( 'NONE', *, *, #10650, .T. ) ;
#62761 = ORIENTED_EDGE ( 'NONE', *, *, #18013, .F. ) ;
#62762 = CARTESIAN_POINT ( 'NONE',  ( 0.2759803524722201917, 1.940323823244660906, 12.09509972435082403 ) ) ;
#62763 = EDGE_CURVE ( 'NONE', #31335, #36681, #44584, .T. ) ;
#62764 = ORIENTED_EDGE ( 'NONE', *, *, #16363, .T. ) ;
#62765 = CIRCLE ( 'NONE', #33001, 14.99999999999998757 ) ;
#62766 = CARTESIAN_POINT ( 'NONE',  ( -27.08426504710140392, -2.223709847896210512, 0.5533780324190709088 ) ) ;
#62767 = LINE ( 'NONE', #954, #359 ) ;
#62768 = DIRECTION ( 'NONE',  ( 1.000000000000000000, 0.000000000000000000, 0.000000000000000000 ) ) ;
#62769 = DIRECTION ( 'NONE',  ( -1.000000000000000000, 0.000000000000000000, 0.000000000000000000 ) ) ;
#62770 = CARTESIAN_POINT ( 'NONE',  ( 37.00000000000000711, 4.041347439436019151, 11.02904044024204211 ) ) ;
#62771 = EDGE_CURVE ( 'NONE', #10792, #16340, #24818, .T. ) ;
#62772 = CARTESIAN_POINT ( 'NONE',  ( 2.297017764050092392, 7.563558677601596614, 1.166330442180198768 ) ) ;
#62773 = CARTESIAN_POINT ( 'NONE',  ( 0.000000000000000000, 1.693411908627200146, 7.306323022404582979 ) ) ;
#62774 = ORIENTED_EDGE ( 'NONE', *, *, #5050, .F. ) ;
#62775 = AXIS2_PLACEMENT_3D ( 'NONE', #860, #16800, #37078 ) ;
#62776 = VERTEX_POINT ( 'NONE', #40259 ) ;
#62777 = CARTESIAN_POINT ( 'NONE',  ( -27.10719052120871098, 0.6736837626858914740, 2.261993590776020469 ) ) ;
#62778 = ORIENTED_EDGE ( 'NONE', *, *, #36805, .T. ) ;
#62779 = FILL_AREA_STYLE_COLOUR ( '', #41935 ) ;
#62780 = CARTESIAN_POINT ( 'NONE',  ( 24.48433763888825965, -10.56700585905174705, -8.404709212046528322 ) ) ;
#62781 = CYLINDRICAL_SURFACE ( 'NONE', #47046, 4.999999999999999112 ) ;
#62782 = CIRCLE ( 'NONE', #34103, 12.74999999999999822 ) ;
#62783 = CARTESIAN_POINT ( 'NONE',  ( -27.08776759928996825, 1.644157618165827728, 1.611072893085636615 ) ) ;
#62784 = VERTEX_POINT ( 'NONE', #60546 ) ;
#62785 = DIRECTION ( 'NONE',  ( 0.000000000000000000, 0.01356324068817998940, -0.9999080150203990547 ) ) ;
#62786 = CARTESIAN_POINT ( 'NONE',  ( -15.07969093506323865, -34.00054679314069972, -8.511206496388529885 ) ) ;
#62787 = CARTESIAN_POINT ( 'NONE',  ( 2.288423627607777622, -5.039850887180386430, -5.755330594805019295 ) ) ;
#62788 = ORIENTED_EDGE ( 'NONE', *, *, #57118, .T. ) ;
#62789 = ORIENTED_EDGE ( 'NONE', *, *, #20516, .F. ) ;
#62790 = CARTESIAN_POINT ( 'NONE',  ( 0.3040950598368152291, -2.376091969481135546, -12.02925914197707513 ) ) ;
#62791 = ORIENTED_EDGE ( 'NONE', *, *, #53079, .F. ) ;
#62792 = ORIENTED_EDGE ( 'NONE', *, *, #63400, .F. ) ;
#62793 = CARTESIAN_POINT ( 'NONE',  ( -36.00000000000000711, -3.473736367725172247, -12.26766708251995475 ) ) ;
#62794 = EDGE_LOOP ( 'NONE', ( #51464, #22794, #60239, #1327 ) ) ;
#62795 = ORIENTED_EDGE ( 'NONE', *, *, #49286, .T. ) ;
#62796 = AXIS2_PLACEMENT_3D ( 'NONE', #38346, #63606, #23392 ) ;
#62797 = CARTESIAN_POINT ( 'NONE',  ( 0.2958664285830405749, 4.398464391600323431, 11.43993536884558893 ) ) ;
#62798 = CARTESIAN_POINT ( 'NONE',  ( -37.00000000000000711, -12.26766708251994409, 3.473736367725208662 ) ) ;
#62799 = AXIS2_PLACEMENT_3D ( 'NONE', #53939, #38966, #63243 ) ;
#62800 = EDGE_CURVE ( 'NONE', #11272, #6611, #17375, .T. ) ;
#62801 = CARTESIAN_POINT ( 'NONE',  ( -35.00000000000000000, -11.68758509253249223, 1.171570255487406786 ) ) ;
#62802 = CARTESIAN_POINT ( 'NONE',  ( 0.2657645697724685396, 7.987126944299760112, -9.283243433322994065 ) ) ;
#62803 = CARTESIAN_POINT ( 'NONE',  ( 2.889800649504073782, -6.039722463373532690, -0.9965440656174344713 ) ) ;
#62804 = VECTOR ( 'NONE', #37140, 1000.000000000000000 ) ;
#62805 = CARTESIAN_POINT ( 'NONE',  ( 17.11293024090986492, 12.19363187244997881, 5.793609989425340778 ) ) ;
#62806 = ADVANCED_FACE ( 'NONE', ( #35274 ), #29966, .T. ) ;
#62807 = ORIENTED_EDGE ( 'NONE', *, *, #2863, .T. ) ;
#62808 = CARTESIAN_POINT ( 'NONE',  ( 35.00000000000000000, 4.705694406421931860E-17, -3.469127814946512892E-15 ) ) ;
#62809 = CARTESIAN_POINT ( 'NONE',  ( 2.835339799623868284, 4.778327228934593052, 6.206025468804318379 ) ) ;
#62810 = AXIS2_PLACEMENT_3D ( 'NONE', #36025, #35379, #30070 ) ;
#62811 = DIRECTION ( 'NONE',  ( -1.000000000000000000, -0.000000000000000000, -0.000000000000000000 ) ) ;
#62812 = CARTESIAN_POINT ( 'NONE',  ( 35.00000000000000000, 10.43555801961475282, -5.391785509271000087 ) ) ;
#62813 = DIRECTION ( 'NONE',  ( -1.000000000000000000, 0.000000000000000000, -0.000000000000000000 ) ) ;
#62814 = CIRCLE ( 'NONE', #34132, 5.000000000000002665 ) ;
#62815 = CARTESIAN_POINT ( 'NONE',  ( -28.71060117729525984, 3.670315194194624375, -12.99175741217617386 ) ) ;
#62816 = EDGE_CURVE ( 'NONE', #23443, #40945, #53513, .T. ) ;
#62817 = EDGE_LOOP ( 'NONE', ( #63521, #6641, #52611, #50872 ) ) ;
#62818 = CARTESIAN_POINT ( 'NONE',  ( 0.000000000000000000, 6.586971819220337032, 3.586335490831404460 ) ) ;
#62819 = VECTOR ( 'NONE', #4921, 1000.000000000000000 ) ;
#62820 = VERTEX_POINT ( 'NONE', #60227 ) ;
#62821 = CARTESIAN_POINT ( 'NONE',  ( 2.406456491626458583, 4.152987573055560766, 9.571062220820376609 ) ) ;
#62822 = CARTESIAN_POINT ( 'NONE',  ( 0.2833330754217383007, -0.2021515668286508749, 12.25052326018167648 ) ) ;
#62823 = CARTESIAN_POINT ( 'NONE',  ( 2.373367633546870969, 5.996611082972032492, -4.795703124519829608 ) ) ;
#62824 = AXIS2_PLACEMENT_3D ( 'NONE', #17410, #37686, #52972 ) ;
#62826 = CIRCLE ( 'NONE', #47940, 5.000000000000000000 ) ;
#62825 = CARTESIAN_POINT ( 'NONE',  ( -35.00000000000000000, 0.000000000000000000, 0.000000000000000000 ) ) ;
#62827 = CARTESIAN_POINT ( 'NONE',  ( 2.284126774967659923, -6.701756155761970923, 3.686252397487106425 ) ) ;
#62828 = EDGE_CURVE ( 'NONE', #2095, #13885, #441, .T. ) ;
#62829 = VERTEX_POINT ( 'NONE', #28655 ) ;
#62830 = CARTESIAN_POINT ( 'NONE',  ( 37.00000000000000711, -11.26103545359853264, 3.340853584269647847 ) ) ;
#62831 = DIRECTION ( 'NONE',  ( -1.000000000000000000, -0.000000000000000000, -0.000000000000000000 ) ) ;
#62832 = DIRECTION ( 'NONE',  ( 0.000000000000000000, 0.9868265225415265851, -0.1617819965527619031 ) ) ;
#62833 = CARTESIAN_POINT ( 'NONE',  ( -37.00000000000000711, 0.000000000000000000, 0.000000000000000000 ) ) ;
#62834 = EDGE_CURVE ( 'NONE', #25804, #34326, #44998, .T. ) ;
#62835 = AXIS2_PLACEMENT_3D ( 'NONE', #46420, #65691, #20159 ) ;
#62836 = CIRCLE ( 'NONE', #18235, 12.73084802173761787 ) ;
#62837 = CIRCLE ( 'NONE', #50131, 4.999999999999999112 ) ;
#62838 = DIRECTION ( 'NONE',  ( 1.000000000000000000, 0.000000000000000000, -0.000000000000000000 ) ) ;
#62839 = EDGE_LOOP ( 'NONE', ( #35560, #9311, #15198, #21053 ) ) ;
#62840 = DIRECTION ( 'NONE',  ( -0.3939253465568944290, -0.3052156353794380217, 0.8669868725995547587 ) ) ;
#62841 = CARTESIAN_POINT ( 'NONE',  ( 0.6511581176968139761, -5.898618881004688674, -10.87850887236101372 ) ) ;
#62842 = AXIS2_PLACEMENT_3D ( 'NONE', #13605, #55492, #65449 ) ;
#62843 = EDGE_CURVE ( 'NONE', #10126, #21470, #18710, .T. ) ;
#62844 = VECTOR ( 'NONE', #39204, 1000.000000000000000 ) ;
#62845 = VERTEX_POINT ( 'NONE', #8718 ) ;
#62846 = AXIS2_PLACEMENT_3D ( 'NONE', #16782, #44032, #58024 ) ;
#62847 = EDGE_CURVE ( 'NONE', #22815, #13989, #42849, .T. ) ;
#62848 = ORIENTED_EDGE ( 'NONE', *, *, #56944, .T. ) ;
#62849 = CARTESIAN_POINT ( 'NONE',  ( -18.15255838926453080, 3.492896982859142518, 11.48290758289192937 ) ) ;
#62850 = CARTESIAN_POINT ( 'NONE',  ( 0.000000000000000000, 1.225832621831950187, -6.827324998361564923 ) ) ;
#62851 = CYLINDRICAL_SURFACE ( 'NONE', #21601, 4.999999999999999112 ) ;
#62852 = CARTESIAN_POINT ( 'NONE',  ( 1.104777566491154550, -7.679758239385205520, 9.895624035730048007 ) ) ;
#62853 = AXIS2_PLACEMENT_3D ( 'NONE', #60500, #45533, #35225 ) ;
#62854 = CARTESIAN_POINT ( 'NONE',  ( -22.27384469013076185, -2.154627400808021509, -2.985904959940921088 ) ) ;
#62855 = VERTEX_POINT ( 'NONE', #49308 ) ;
#62856 = CIRCLE ( 'NONE', #21326, 5.000000000000001776 ) ;
#62857 = ORIENTED_EDGE ( 'NONE', *, *, #56338, .F. ) ;
#62858 = ORIENTED_EDGE ( 'NONE', *, *, #42215, .T. ) ;
#62859 = CARTESIAN_POINT ( 'NONE',  ( 2.770579946183334474, 7.804957730865694110, 0.3031629740256017724 ) ) ;
#62860 = DIRECTION ( 'NONE',  ( 1.000000000000000000, 0.000000000000000000, 0.000000000000000000 ) ) ;
#62861 = ORIENTED_EDGE ( 'NONE', *, *, #46369, .T. ) ;
#62862 = CYLINDRICAL_SURFACE ( 'NONE', #53833, 2.899999999999994582 ) ;
#62863 = AXIS2_PLACEMENT_3D ( 'NONE', #58406, #23479, #3555 ) ;
#62864 = CARTESIAN_POINT ( 'NONE',  ( 2.034671305879989678, -10.44529075078586722, 5.218565780488946260 ) ) ;
#62865 = ORIENTED_EDGE ( 'NONE', *, *, #58730, .F. ) ;
#62866 = CARTESIAN_POINT ( 'NONE',  ( 0.2652384770603677389, 11.53005438969049834, -4.126289928142288232 ) ) ;
#62867 = CYLINDRICAL_SURFACE ( 'NONE', #8433, 4.999999999999999112 ) ;
#62868 = CARTESIAN_POINT ( 'NONE',  ( 24.90125186782636035, -0.3305283664803125299, 12.00214278619375285 ) ) ;
#62869 = ORIENTED_EDGE ( 'NONE', *, *, #60065, .T. ) ;
#62870 = ORIENTED_EDGE ( 'NONE', *, *, #48168, .T. ) ;
#62871 = CARTESIAN_POINT ( 'NONE',  ( -35.00000000000000000, 0.6593684648222323252, -12.73293890771482495 ) ) ;
#62872 = ORIENTED_EDGE ( 'NONE', *, *, #63676, .F. ) ;
#62873 = DIRECTION ( 'NONE',  ( 0.000000000000000000, 0.000000000000000000, 1.000000000000000000 ) ) ;
#62874 = CIRCLE ( 'NONE', #3586, 5.000000000000000000 ) ;
#62875 = CARTESIAN_POINT ( 'NONE',  ( 35.00000000000000000, 5.130401251914885385, 11.05394794832823813 ) ) ;
#62876 = CARTESIAN_POINT ( 'NONE',  ( 13.23110845409921055, -34.10188054478342679, -9.409930202775637298 ) ) ;
#62877 = DIRECTION ( 'NONE',  ( 1.000000000000000000, 0.000000000000000000, 0.000000000000000000 ) ) ;
#62878 = AXIS2_PLACEMENT_3D ( 'NONE', #18022, #13354, #22020 ) ;
#62880 = AXIS2_PLACEMENT_3D ( 'NONE', #59584, #14344, #34933 ) ;
#62879 = DIRECTION ( 'NONE',  ( 0.000000000000000000, 0.4698238015817302049, 0.8827602140260349950 ) ) ;
#62881 = CARTESIAN_POINT ( 'NONE',  ( -30.18541646480309026, -1.416020129149132334, -13.42553116244734746 ) ) ;
#62882 = CARTESIAN_POINT ( 'NONE',  ( 6.361445718264521432, -4.355102044641763648, -11.18181944858513077 ) ) ;
#62883 = ORIENTED_EDGE ( 'NONE', *, *, #13962, .F. ) ;
#62884 = LINE ( 'NONE', #47294, #47066 ) ;
#62885 = EDGE_CURVE ( 'NONE', #64819, #49332, #6795, .T. ) ;
#62886 = ORIENTED_EDGE ( 'NONE', *, *, #6538, .F. ) ;
#62887 = CARTESIAN_POINT ( 'NONE',  ( 1.719304012340734378, -7.581471372739226666, -10.22720798541506682 ) ) ;
#62888 = CARTESIAN_POINT ( 'NONE',  ( 2.257661810674659097, 6.682681612746527833, 3.702552158177466968 ) ) ;
#62889 = VERTEX_POINT ( 'NONE', #46909 ) ;
#62890 = CARTESIAN_POINT ( 'NONE',  ( -18.55545074886880386, 5.671797102417516001, 10.57879050686813116 ) ) ;
#62891 = CARTESIAN_POINT ( 'NONE',  ( 0.3109076770649020771, 12.03190317807027476, -2.361108455562717978 ) ) ;
#62892 = CARTESIAN_POINT ( 'NONE',  ( 0.2647959493198558945, -2.271080632827979784, -12.03358727341676726 ) ) ;
#62893 = AXIS2_PLACEMENT_3D ( 'NONE', #62363, #16512, #22473 ) ;
#62894 = VERTEX_POINT ( 'NONE', #46574 ) ;
#62895 = CIRCLE ( 'NONE', #55450, 4.999999999999999112 ) ;
#62896 = EDGE_CURVE ( 'NONE', #27449, #3878, #51380, .T. ) ;
#62897 = ORIENTED_EDGE ( 'NONE', *, *, #30914, .T. ) ;
#62898 = CARTESIAN_POINT ( 'NONE',  ( -35.00000000000000000, 0.000000000000000000, 0.000000000000000000 ) ) ;
#62899 = AXIS2_PLACEMENT_3D ( 'NONE', #22066, #6457, #42653 ) ;
#62900 = VERTEX_POINT ( 'NONE', #60892 ) ;
#62901 = FACE_OUTER_BOUND ( 'NONE', #42080, .T. ) ;
#62902 = AXIS2_PLACEMENT_3D ( 'NONE', #45141, #40128, #50784 ) ;
#62903 = CARTESIAN_POINT ( 'NONE',  ( -10.00000000000000178, 0.000000000000000000, 0.000000000000000000 ) ) ;
#62904 = CARTESIAN_POINT ( 'NONE',  ( -3.439258850808092571, -11.96382994935912514, 6.264996690403261681 ) ) ;
#62905 = CARTESIAN_POINT ( 'NONE',  ( -19.16330044134494415, -4.498325028293125527, 11.12691725379990082 ) ) ;
#62906 = EDGE_CURVE ( 'NONE', #10959, #47299, #50337, .T. ) ;
#62907 = ORIENTED_EDGE ( 'NONE', *, *, #30011, .T. ) ;
#62908 = DIRECTION ( 'NONE',  ( -1.000000000000000000, 0.000000000000000000, 0.000000000000000000 ) ) ;
#62909 = EDGE_CURVE ( 'NONE', #33373, #53424, #20964, .T. ) ;
#62910 = AXIS2_PLACEMENT_3D ( 'NONE', #31174, #40478, #6236 ) ;
#62911 = CARTESIAN_POINT ( 'NONE',  ( 2.931247277082682956, -7.672001188570249930, -1.728824746592349193 ) ) ;
#62912 =( BOUNDED_CURVE ( )  B_SPLINE_CURVE ( 3, ( #6528, #2188, #22468, #32429 ),
 .UNSPECIFIED., .F., .F. ) 
 B_SPLINE_CURVE_WITH_KNOTS ( ( 4, 4 ),
 ( 0.7473423473803021411, 0.7669100185107887713 ),
 .UNSPECIFIED. ) 
 CURVE ( )  GEOMETRIC_REPRESENTATION_ITEM ( )  RATIONAL_B_SPLINE_CURVE ( ( 1.000000000000000000, 0.9999680924417370109, 0.9999680924417370109, 1.000000000000000000 ) ) 
 REPRESENTATION_ITEM ( '' )  );
#62913 = FACE_OUTER_BOUND ( 'NONE', #2881, .T. ) ;
#62914 = CARTESIAN_POINT ( 'NONE',  ( 22.98437084614390713, 11.91223824963345024, -6.360283269683757901 ) ) ;
#62915 = CARTESIAN_POINT ( 'NONE',  ( -27.08417473062937120, -0.7460375461499253458, 2.166271322019566181 ) ) ;
#62916 = DIRECTION ( 'NONE',  ( -1.000000000000000000, 0.000000000000000000, -0.000000000000000000 ) ) ;
#62917 = CARTESIAN_POINT ( 'NONE',  ( 0.000000000000000000, -34.50000000000000000, 0.000000000000000000 ) ) ;
#62918 = CARTESIAN_POINT ( 'NONE',  ( 2.573738926104379487, 5.156412073069364332, -5.779258037546964211 ) ) ;
#62919 = CIRCLE ( 'NONE', #27907, 12.75000000000000178 ) ;
#62920 = CIRCLE ( 'NONE', #39574, 12.18650000000000411 ) ;
#62921 = EDGE_CURVE ( 'NONE', #60300, #11928, #25303, .T. ) ;
#62922 = CIRCLE ( 'NONE', #52373, 4.999999999999999112 ) ;
#62923 = AXIS2_PLACEMENT_3D ( 'NONE', #6112, #46656, #16720 ) ;
#62924 = ORIENTED_EDGE ( 'NONE', *, *, #53768, .F. ) ;
#62925 = CARTESIAN_POINT ( 'NONE',  ( -26.43258404273187523, 1.478864324198235769, 3.148308537883169222 ) ) ;
#62926 = CARTESIAN_POINT ( 'NONE',  ( 5.043734429376389272, -9.821217208287897904, 9.263622243474671336 ) ) ;
#62927 = VERTEX_POINT ( 'NONE', #35914 ) ;
#62928 = LINE ( 'NONE', #2087, #56573 ) ;
#62929 = CYLINDRICAL_SURFACE ( 'NONE', #20461, 12.18650000000000055 ) ;
#62930 = VERTEX_POINT ( 'NONE', #15967 ) ;
#62931 = UNCERTAINTY_MEASURE_WITH_UNIT (LENGTH_MEASURE( 1.000000000000000082E-05 ), #53612, 'distance_accuracy_value', 'NONE');
#62932 = CARTESIAN_POINT ( 'NONE',  ( -22.00000000000000711, -20.00000000000000000, 1.500000000000002887 ) ) ;
#62933 = ORIENTED_EDGE ( 'NONE', *, *, #15582, .T. ) ;
#62934 = CIRCLE ( 'NONE', #5627, 5.000000000000000000 ) ;
#62935 = CARTESIAN_POINT ( 'NONE',  ( -36.00000000000000711, 3.307597835713245171, 12.31350058095524425 ) ) ;
#62936 = ORIENTED_EDGE ( 'NONE', *, *, #62320, .F. ) ;
#62937 = ORIENTED_EDGE ( 'NONE', *, *, #48722, .F. ) ;
#62938 = ADVANCED_FACE ( 'NONE', ( #11003, #15332 ), #51589, .F. ) ;
#62939 = AXIS2_PLACEMENT_3D ( 'NONE', #64797, #34856, #55836 ) ;
#62940 = CARTESIAN_POINT ( 'NONE',  ( -22.29290468048228036, -3.357740900108097559, -1.621390503294487750 ) ) ;
#62941 = ORIENTED_EDGE ( 'NONE', *, *, #45484, .F. ) ;
#62942 = DIRECTION ( 'NONE',  ( -1.000000000000000000, 0.000000000000000000, 0.000000000000000000 ) ) ;
#62943 = CARTESIAN_POINT ( 'NONE',  ( 3.152665057733834431, -3.161213418913157991, 7.281573230474281289 ) ) ;
#62944 = DIRECTION ( 'NONE',  ( -1.000000000000000000, -1.836970198721029688E-16, -0.000000000000000000 ) ) ;
#62945 = DIRECTION ( 'NONE',  ( -1.000000000000000000, 0.000000000000000000, 0.000000000000000000 ) ) ;
#62946 = ORIENTED_EDGE ( 'NONE', *, *, #35252, .F. ) ;
#62947 = DIRECTION ( 'NONE',  ( 0.000000000000000000, 0.01356324068817998940, -0.9999080150203989437 ) ) ;
#62948 = VECTOR ( 'NONE', #8836, 1000.000000000000000 ) ;
#62949 = CARTESIAN_POINT ( 'NONE',  ( 4.286683309450310730, -28.06227586351137759, 12.00609810331033067 ) ) ;
#62950 = DIRECTION ( 'NONE',  ( 0.000000000000000000, -0.1764146379942750642, -0.9843159429275485373 ) ) ;
#62952 = ORIENTED_EDGE ( 'NONE', *, *, #2579, .T. ) ;
#62951 = CARTESIAN_POINT ( 'NONE',  ( -24.33265139114022091, 8.847575708096826475, 8.109868413052772951 ) ) ;
#62953 = FACE_OUTER_BOUND ( 'NONE', #16714, .T. ) ;
#62954 = ORIENTED_EDGE ( 'NONE', *, *, #29442, .F. ) ;
#62955 = CARTESIAN_POINT ( 'NONE',  ( -35.00000000000000000, -1.286231064351400555, 12.68495603654571369 ) ) ;
#62956 = ORIENTED_EDGE ( 'NONE', *, *, #13236, .F. ) ;
#62957 = DIRECTION ( 'NONE',  ( -1.000000000000000000, 0.000000000000000000, 0.000000000000000000 ) ) ;
#62958 = CARTESIAN_POINT ( 'NONE',  ( 2.241449424704146320, -4.954182807723299220, -5.808712090826661623 ) ) ;
#62959 = LINE ( 'NONE', #52356, #42844 ) ;
#62960 = VERTEX_POINT ( 'NONE', #41909 ) ;
#62961 = CARTESIAN_POINT ( 'NONE',  ( 0.4613984246114876120, 8.128335150814509191, 9.246873830555923490 ) ) ;
#62962 = DIRECTION ( 'NONE',  ( 0.000000000000000000, -0.01356324068818000848, 0.9999080150203990547 ) ) ;
#62963 = CARTESIAN_POINT ( 'NONE',  ( -22.27706485742869091, -3.547445275915918295, -0.9832726768967802178 ) ) ;
#62964 = ORIENTED_EDGE ( 'NONE', *, *, #15911, .T. ) ;
#62965 = EDGE_CURVE ( 'NONE', #9350, #2029, #2530, .T. ) ;
#62966 = EDGE_LOOP ( 'NONE', ( #65393, #47203, #63572, #62376 ) ) ;
#62967 = DIRECTION ( 'NONE',  ( -1.000000000000000000, 0.000000000000000000, 0.000000000000000000 ) ) ;
#62968 = VERTEX_POINT ( 'NONE', #20661 ) ;
#62969 = ADVANCED_FACE ( 'NONE', ( #31288 ), #20315, .T. ) ;
#62970 = AXIS2_PLACEMENT_3D ( 'NONE', #27867, #62769, #48173 ) ;
#62971 = EDGE_LOOP ( 'NONE', ( #62807, #43905, #20349, #16882 ) ) ;
#62973 = CIRCLE ( 'NONE', #34300, 5.000000000000000888 ) ;
#62972 = DIRECTION ( 'NONE',  ( -0.000000000000000000, -1.000000000000000000, -0.000000000000000000 ) ) ;
#62974 = DIRECTION ( 'NONE',  ( 1.000000000000000000, 0.000000000000000000, 0.000000000000000000 ) ) ;
#62975 = DIRECTION ( 'NONE',  ( 0.000000000000000000, 0.4134677391718512007, 0.9105187689795953832 ) ) ;
#62976 = LINE ( 'NONE', #26754, #56466 ) ;
#62977 = DIRECTION ( 'NONE',  ( 0.3865475372811021382, -0.1410344188397403553, -0.9114221272958275000 ) ) ;
#62978 = CIRCLE ( 'NONE', #27956, 2.899999999999995470 ) ;
#62979 = CARTESIAN_POINT ( 'NONE',  ( -35.00000000000000000, -9.196955404009360180, 8.830544224262913744 ) ) ;
#62980 = AXIS2_PLACEMENT_3D ( 'NONE', #27947, #48259, #2706 ) ;
#62981 = EDGE_CURVE ( 'NONE', #36790, #11928, #10646, .T. ) ;
#62982 = DIRECTION ( 'NONE',  ( 1.000000000000000000, 0.000000000000000000, 0.000000000000000000 ) ) ;
#62983 = ORIENTED_EDGE ( 'NONE', *, *, #58702, .T. ) ;
#62984 = CARTESIAN_POINT ( 'NONE',  ( 2.941278708680199916, -4.615461433467283214, 4.048809123187920633 ) ) ;
#62985 = FACE_OUTER_BOUND ( 'NONE', #43406, .T. ) ;
#62986 = CIRCLE ( 'NONE', #9922, 250.0000000000000000 ) ;
#62987 = AXIS2_PLACEMENT_3D ( 'NONE', #34780, #55085, #40790 ) ;
#62988 = CARTESIAN_POINT ( 'NONE',  ( 2.305787727787084407, -4.792270232040933386, 5.970480882365206909 ) ) ;
#62989 = LINE ( 'NONE', #27738, #38631 ) ;
#62990 = FACE_OUTER_BOUND ( 'NONE', #8317, .T. ) ;
#62991 = ADVANCED_FACE ( 'NONE', ( #56564 ), #52244, .F. ) ;
#62992 = AXIS2_PLACEMENT_3D ( 'NONE', #47348, #61973, #31383 ) ;
#62993 = CARTESIAN_POINT ( 'NONE',  ( 17.11293024090985071, -12.19363187244996105, 5.793609989425343443 ) ) ;
#62994 = CIRCLE ( 'NONE', #25847, 7.499999999999988454 ) ;
#62995 = CARTESIAN_POINT ( 'NONE',  ( 12.03305870789770360, 0.5719181555549518459, -11.98657499750327915 ) ) ;
#62996 = VERTEX_POINT ( 'NONE', #39118 ) ;
#62997 = DIRECTION ( 'NONE',  ( 0.000000000000000000, -0.01356324068817991828, 0.9999080150203990547 ) ) ;
#62998 = CYLINDRICAL_SURFACE ( 'NONE', #25111, 12.18650000000000055 ) ;
#62999 = CARTESIAN_POINT ( 'NONE',  ( -35.00000000000000000, 11.80185301892987582, -4.824807283153994319 ) ) ;
#63000 = CARTESIAN_POINT ( 'NONE',  ( -18.04274061274178109, -13.45660803163010755, 1.263225231962421313 ) ) ;
#63001 = CARTESIAN_POINT ( 'NONE',  ( -27.27855387000350262, 10.59660315834921640, 5.631341004100471892 ) ) ;
#63002 = CARTESIAN_POINT ( 'NONE',  ( 35.00000000000000000, -6.280308599560208371, -9.926225166347007800 ) ) ;
#63003 = ORIENTED_EDGE ( 'NONE', *, *, #63593, .T. ) ;
#63004 = CARTESIAN_POINT ( 'NONE',  ( 18.43933328720107667, -6.457919038062313710, 10.12447623701847554 ) ) ;
#63005 = CARTESIAN_POINT ( 'NONE',  ( -35.00000000000000000, 0.000000000000000000, 0.000000000000000000 ) ) ;
#63006 = CARTESIAN_POINT ( 'NONE',  ( 0.2648321136542701182, 9.289286523730419631, 7.979621084888147919 ) ) ;
#63007 = CYLINDRICAL_SURFACE ( 'NONE', #20092, 6.936499999999988120 ) ;
#63008 = ORIENTED_EDGE ( 'NONE', *, *, #51401, .T. ) ;
#63009 = CARTESIAN_POINT ( 'NONE',  ( 24.48320719723312777, 10.56747877308070827, -8.404134578084967444 ) ) ;
#63010 = DIRECTION ( 'NONE',  ( 1.000000000000000000, 0.000000000000000000, 0.000000000000000000 ) ) ;
#63011 = ORIENTED_EDGE ( 'NONE', *, *, #18166, .F. ) ;
#63012 = VECTOR ( 'NONE', #57698, 1000.000000000000000 ) ;
#63013 = AXIS2_PLACEMENT_3D ( 'NONE', #9454, #14445, #40719 ) ;
#63014 = EDGE_LOOP ( 'NONE', ( #54330, #47886, #3099, #33276 ) ) ;
#63015 = DIRECTION ( 'NONE',  ( -1.000000000000000000, 0.000000000000000000, 0.000000000000000000 ) ) ;
#63016 = AXIS2_PLACEMENT_3D ( 'NONE', #41399, #1537, #61689 ) ;
#63017 = ADVANCED_FACE ( 'NONE', ( #58115 ), #22519, .F. ) ;
#63018 = CARTESIAN_POINT ( 'NONE',  ( 0.2671309869109527169, -4.340541005679448006, -11.45180222993658248 ) ) ;
#63019 = ORIENTED_EDGE ( 'NONE', *, *, #6524, .T. ) ;
#63020 = CARTESIAN_POINT ( 'NONE',  ( 0.2869720083484341155, -9.519277517057156857, 7.715523637151736835 ) ) ;
#63021 = FACE_OUTER_BOUND ( 'NONE', #7205, .T. ) ;
#63022 = DIRECTION ( 'NONE',  ( 0.000000000000000000, -0.01356324068817998940, 0.9999080150203990547 ) ) ;
#63023 = CARTESIAN_POINT ( 'NONE',  ( -7.489022030332961322, 25.00000000000000000, -10.84914964302385521 ) ) ;
#63024 = CARTESIAN_POINT ( 'NONE',  ( -35.00000000000000000, 2.220215194441899076, 11.98254675519229195 ) ) ;
#63025 = CIRCLE ( 'NONE', #41812, 2.899999999999995026 ) ;
#63026 = DIRECTION ( 'NONE',  ( 1.000000000000000000, 0.000000000000000000, 0.000000000000000000 ) ) ;
#63028 = ORIENTED_EDGE ( 'NONE', *, *, #41048, .T. ) ;
#63027 = DIRECTION ( 'NONE',  ( 0.000000000000000000, 0.000000000000000000, 1.000000000000000000 ) ) ;
#63029 = CARTESIAN_POINT ( 'NONE',  ( 0.6511581176971957818, 4.541862140119915736, -11.51117493088913157 ) ) ;
#63030 = ORIENTED_EDGE ( 'NONE', *, *, #8774, .T. ) ;
#63031 = CARTESIAN_POINT ( 'NONE',  ( 24.88399796223642468, -1.143778065019554813, -11.94702019429119844 ) ) ;
#63032 = CIRCLE ( 'NONE', #18501, 7.499999999999988454 ) ;
#63033 = EDGE_LOOP ( 'NONE', ( #4738, #59460, #64742, #20848 ) ) ;
#63034 = ORIENTED_EDGE ( 'NONE', *, *, #24965, .F. ) ;
#63035 = CARTESIAN_POINT ( 'NONE',  ( 0.9232167919969139769, -11.56588005394301177, 4.649596781010366442 ) ) ;
#63036 = CARTESIAN_POINT ( 'NONE',  ( -13.57005631242150834, -30.10739101144227803, 6.607437777793664146 ) ) ;
#63037 = CARTESIAN_POINT ( 'NONE',  ( 2.524535260912860402, 1.559291270914676231, 7.569872524929055047 ) ) ;
#63038 = ADVANCED_FACE ( 'NONE', ( #29166 ), #43277, .F. ) ;
#63039 = CARTESIAN_POINT ( 'NONE',  ( -25.00000000000000355, -3.797884998337192286, 23.99999999999999289 ) ) ;
#63040 = CARTESIAN_POINT ( 'NONE',  ( 36.00000000000000711, -1.113475361586579337, -12.70128625845192616 ) ) ;
#63041 = ORIENTED_EDGE ( 'NONE', *, *, #29862, .T. ) ;
#63042 = AXIS2_PLACEMENT_3D ( 'NONE', #24682, #40622, #29336 ) ;
#63043 = CARTESIAN_POINT ( 'NONE',  ( -22.27722019094931127, 0.6491642780571855731, 3.623977093944191541 ) ) ;
#63044 = ADVANCED_FACE ( 'NONE', ( #8536 ), #38636, .F. ) ;
#63045 = CARTESIAN_POINT ( 'NONE',  ( 1.283627346226433596, -3.783098238613557207, 12.00363697230081605 ) ) ;
#63046 = ORIENTED_EDGE ( 'NONE', *, *, #455, .F. ) ;
#63047 = AXIS2_PLACEMENT_3D ( 'NONE', #64362, #63060, #13182 ) ;
#63048 = VERTEX_POINT ( 'NONE', #59409 ) ;
#63049 = CARTESIAN_POINT ( 'NONE',  ( -37.00000000000000711, 12.38385022362082033, 3.033604067594621867 ) ) ;
#63050 = ADVANCED_FACE ( 'NONE', ( #24158 ), #28489, .F. ) ;
#63051 = ORIENTED_EDGE ( 'NONE', *, *, #47973, .F. ) ;
#63052 = DIRECTION ( 'NONE',  ( -1.000000000000000000, 0.000000000000000000, -0.000000000000000000 ) ) ;
#63053 = LINE ( 'NONE', #56787, #12854 ) ;
#63054 = LINE ( 'NONE', #17517, #17217 ) ;
#63055 = LINE ( 'NONE', #36802, #58189 ) ;
#63056 = CARTESIAN_POINT ( 'NONE',  ( 0.000000000000000000, -6.160607635185433750, 4.277489166005560506 ) ) ;
#63057 = DIRECTION ( 'NONE',  ( -1.000000000000000000, 0.000000000000000000, 0.000000000000000000 ) ) ;
#63058 = VECTOR ( 'NONE', #38165, 1000.000000000000000 ) ;
#63059 = EDGE_CURVE ( 'NONE', #63385, #27449, #55640, .T. ) ;
#63060 = DIRECTION ( 'NONE',  ( -1.000000000000000000, 0.000000000000000000, 0.000000000000000000 ) ) ;
#63061 = ORIENTED_EDGE ( 'NONE', *, *, #65210, .T. ) ;
#63062 = CARTESIAN_POINT ( 'NONE',  ( -47.00000000000000711, 0.000000000000000000, 0.000000000000000000 ) ) ;
#63063 = ADVANCED_FACE ( 'NONE', ( #8219 ), #33494, .T. ) ;
#63064 = EDGE_LOOP ( 'NONE', ( #65782, #25024, #24787, #25624 ) ) ;
#63065 = CARTESIAN_POINT ( 'NONE',  ( 0.2653519890518140634, -6.123091032184224680, 10.60552241699065590 ) ) ;
#63066 = CARTESIAN_POINT ( 'NONE',  ( -8.650525597369476571, -10.29405175124346172, -8.740411465918450418 ) ) ;
#63067 = DIRECTION ( 'NONE',  ( 1.000000000000000000, 0.000000000000000000, -0.000000000000000000 ) ) ;
#63068 = AXIS2_PLACEMENT_3D ( 'NONE', #19214, #14213, #38851 ) ;
#63069 = CARTESIAN_POINT ( 'NONE',  ( 11.74548640120467979, 8.775604215601129354, -8.184666801472349817 ) ) ;
#63070 = ORIENTED_EDGE ( 'NONE', *, *, #46436, .F. ) ;
#63071 = VERTEX_POINT ( 'NONE', #43794 ) ;
#63072 = DIRECTION ( 'NONE',  ( 1.000000000000000000, 0.000000000000000000, -0.000000000000000000 ) ) ;
#63073 = ADVANCED_FACE ( 'NONE', ( #12528 ), #54098, .T. ) ;
#63074 = AXIS2_PLACEMENT_3D ( 'NONE', #30770, #51090, #5546 ) ;
#63075 = ORIENTED_EDGE ( 'NONE', *, *, #32320, .T. ) ;
#63076 = CARTESIAN_POINT ( 'NONE',  ( 0.2717059086739015417, 7.737372654246708947, -9.494961435243615355 ) ) ;
#63077 = CARTESIAN_POINT ( 'NONE',  ( -35.00000000000000000, 10.25474254703952859, 6.584150480049587806 ) ) ;
#63078 = CIRCLE ( 'NONE', #23797, 4.999999999999999112 ) ;
#63079 = EDGE_CURVE ( 'NONE', #48921, #29332, #21745, .T. ) ;
#63080 = CARTESIAN_POINT ( 'NONE',  ( -27.09048036756592026, -2.083857239073395373, -0.9969423855807594270 ) ) ;
#63081 = DIRECTION ( 'NONE',  ( -1.000000000000000000, -0.000000000000000000, -0.000000000000000000 ) ) ;
#63082 = ORIENTED_EDGE ( 'NONE', *, *, #101, .T. ) ;
#63083 = AXIS2_PLACEMENT_3D ( 'NONE', #33704, #8775, #8439 ) ;
#63084 = CARTESIAN_POINT ( 'NONE',  ( 0.3675815128205894289, 12.13672785388550324, 1.872154644482125763 ) ) ;
#63085 = CARTESIAN_POINT ( 'NONE',  ( 18.50973545861780423, 8.752035742591949941, 10.30270490042575737 ) ) ;
#63086 = CARTESIAN_POINT ( 'NONE',  ( -25.42680463514452072, 0.3277218550990906309, -3.871126486605867889 ) ) ;
#63087 = CYLINDRICAL_SURFACE ( 'NONE', #63509, 2.899999999999994582 ) ;
#63088 = DIRECTION ( 'NONE',  ( -0.000000000000000000, -1.000000000000000000, -0.000000000000000000 ) ) ;
#63089 = CYLINDRICAL_SURFACE ( 'NONE', #15968, 6.936499999999988120 ) ;
#63090 = ORIENTED_EDGE ( 'NONE', *, *, #54741, .F. ) ;
#63091 = CARTESIAN_POINT ( 'NONE',  ( 0.9232058338315058954, 12.34162163148533686, 1.793035206307387330 ) ) ;
#63092 = CARTESIAN_POINT ( 'NONE',  ( -12.26308380404417164, -33.73908083898199806, -10.29207979367737380 ) ) ;
#63093 = ORIENTED_EDGE ( 'NONE', *, *, #7115, .T. ) ;
#63094 = CARTESIAN_POINT ( 'NONE',  ( 36.00000000000000711, 11.66664283989686979, 5.143145423404152261 ) ) ;
#63095 = DIRECTION ( 'NONE',  ( -1.000000000000000000, 0.000000000000000000, -0.000000000000000000 ) ) ;
#63096 = CARTESIAN_POINT ( 'NONE',  ( 0.2646305136544072623, 12.24595685781654630, -0.1321451301298267600 ) ) ;
#63097 = DIRECTION ( 'NONE',  ( 0.000000000000000000, 0.01356324068818000328, -0.9999080150203990547 ) ) ;
#63098 = CARTESIAN_POINT ( 'NONE',  ( 0.2801149460245134226, -11.44368419510489154, 4.374013318106511505 ) ) ;
#63099 = EDGE_CURVE ( 'NONE', #16693, #3390, #34765, .T. ) ;
#63100 = CIRCLE ( 'NONE', #42931, 7.499999999999988454 ) ;
#63101 = ORIENTED_EDGE ( 'NONE', *, *, #8650, .F. ) ;
#63102 = ORIENTED_EDGE ( 'NONE', *, *, #48457, .T. ) ;
#63103 = CARTESIAN_POINT ( 'NONE',  ( 1.452237505248555660, -12.64182585313126417, 0.5922625322516575919 ) ) ;
#63104 = ORIENTED_EDGE ( 'NONE', *, *, #16789, .F. ) ;
#63105 = CARTESIAN_POINT ( 'NONE',  ( 3.780834652287974773, 8.352030633203074927, 25.00000000000000000 ) ) ;
#63107 = CARTESIAN_POINT ( 'NONE',  ( 2.305787727787085295, 7.249469779319941409, -2.461236246750998724 ) ) ;
#63106 =( BOUNDED_SURFACE ( )  B_SPLINE_SURFACE ( 3, 1, ( 
 ( #17928, #38189 ),
 ( #53525, #20711 ),
 ( #7967, #11061 ),
 ( #28235, #11373 ) ),
 .UNSPECIFIED., .F., .F., .F. ) 
 B_SPLINE_SURFACE_WITH_KNOTS ( ( 4, 4 ),
 ( 2, 2 ),
 ( 0.000000000000000000, 1.000000000000000000 ),
 ( 0.000000000000000000, 1.000000000000000000 ),
 .UNSPECIFIED. ) 
 GEOMETRIC_REPRESENTATION_ITEM ( )  RATIONAL_B_SPLINE_SURFACE ( (
 ( 1.000000000000000000, 1.000000000000000000),
 ( 0.8716676215708681896, 0.8964445200148164483),
 ( 0.8716676215708681896, 0.8964445200148164483),
 ( 1.000000000000000000, 1.000000000000000000) ) ) 
 REPRESENTATION_ITEM ( '' )  SURFACE ( )  );
#63108 = CARTESIAN_POINT ( 'NONE',  ( 2.000000000000001776, 0.000000000000000000, 0.000000000000000000 ) ) ;
#63109 = CARTESIAN_POINT ( 'NONE',  ( 1.287602823387600459, -7.659913635101688989, -9.987902848014105217 ) ) ;
#63110 = CARTESIAN_POINT ( 'NONE',  ( 2.259025283528084849, 7.546748801935450501, 1.191911401085038458 ) ) ;
#63112 = DIRECTION ( 'NONE',  ( 1.000000000000000000, 0.000000000000000000, 0.000000000000000000 ) ) ;
#63111 = B_SPLINE_CURVE_WITH_KNOTS ( 'NONE', 3,
 ( #12227, #27857, #8226, #47810, #2268, #22544, #63098, #17882, #38141, #58451, #12882, #33163, #28191, #38482, #48479, #2928, #58801, #13219, #60078, #55080, #23867, #9192 ),
 .UNSPECIFIED., .F., .F.,
 ( 4, 3, 3, 3, 3, 3, 3, 4 ),
 ( 1.755771606739170543E-18, 4.449119708436685694E-05, 6.626296329540286008E-05, 8.803456484962358117E-05, 0.0001098060367612769232, 0.0001315774408628471958, 0.0001760698110411115195, 0.0001829697163287824263 ),
 .UNSPECIFIED. ) ;
#63113 = VERTEX_POINT ( 'NONE', #44758 ) ;
#63114 = VERTEX_POINT ( 'NONE', #25145 ) ;
#63115 = EDGE_CURVE ( 'NONE', #34249, #32729, #41805, .T. ) ;
#63116 = CIRCLE ( 'NONE', #51468, 12.75000000000000178 ) ;
#63117 = CARTESIAN_POINT ( 'NONE',  ( 0.5547464869798244269, -5.905377260991297561, 10.83828453080463561 ) ) ;
#63118 = ORIENTED_EDGE ( 'NONE', *, *, #3500, .F. ) ;
#63119 = CARTESIAN_POINT ( 'NONE',  ( 47.00000000000000711, 4.705694406421931860E-17, -3.469127814946512892E-15 ) ) ;
#63120 = CARTESIAN_POINT ( 'NONE',  ( 1.549075743847258435, 8.652116335902604760, -9.261503792573503091 ) ) ;
#63121 = ADVANCED_FACE ( 'NONE', ( #60723 ), #65788, .F. ) ;
#63122 = DIRECTION ( 'NONE',  ( 1.000000000000000000, -0.000000000000000000, 0.000000000000000000 ) ) ;
#63123 = ORIENTED_EDGE ( 'NONE', *, *, #55843, .T. ) ;
#63124 = CARTESIAN_POINT ( 'NONE',  ( 5.516018279890452902, -0.005752102158673865970, 0.003580555109620777322 ) ) ;
#63125 = CARTESIAN_POINT ( 'NONE',  ( -16.02805653289969356, -29.20913999211483514, -10.57890313540256777 ) ) ;
#63126 = ORIENTED_EDGE ( 'NONE', *, *, #24947, .F. ) ;
#63127 = VERTEX_POINT ( 'NONE', #5540 ) ;
#63128 = CARTESIAN_POINT ( 'NONE',  ( -22.31328051695926007, 3.148362328073167404, -2.109671368890616350 ) ) ;
#63129 = EDGE_CURVE ( 'NONE', #44861, #39718, #45414, .T. ) ;
#63130 = EDGE_LOOP ( 'NONE', ( #27293, #63915, #49591, #54371 ) ) ;
#63131 = EDGE_LOOP ( 'NONE', ( #42332, #31151, #12100, #22941 ) ) ;
#63132 = CYLINDRICAL_SURFACE ( 'NONE', #36538, 6.936499999999988120 ) ;
#63133 = ORIENTED_EDGE ( 'NONE', *, *, #30107, .F. ) ;
#63134 = VERTEX_POINT ( 'NONE', #30765 ) ;
#63135 = CYLINDRICAL_SURFACE ( 'NONE', #43689, 12.18649999999999878 ) ;
#63136 = AXIS2_PLACEMENT_3D ( 'NONE', #44137, #13229, #33516 ) ;
#63137 = DIRECTION ( 'NONE',  ( -1.000000000000000000, -0.000000000000000000, 0.000000000000000000 ) ) ;
#63138 = CARTESIAN_POINT ( 'NONE',  ( 37.00000000000000711, 4.705694406421931860E-17, -3.469127814946512892E-15 ) ) ;
#63139 = CARTESIAN_POINT ( 'NONE',  ( 3.152665057734040488, 0.000000000000000000, 0.000000000000000000 ) ) ;
#63140 = CARTESIAN_POINT ( 'NONE',  ( 36.00000000000000711, -12.46157735505187247, 2.696588552979187536 ) ) ;
#63141 = B_SPLINE_CURVE_WITH_KNOTS ( 'NONE', 3,
 ( #52538, #51561, #27559, #27238, #16287, #1334, #47219, #1665 ),
 .UNSPECIFIED., .F., .F.,
 ( 4, 2, 2, 4 ),
 ( 0.000000000000000000, 0.0003639104015149997461, 0.0007278208030299994922, 0.001455641606059999635 ),
 .UNSPECIFIED. ) ;
#63142 = CARTESIAN_POINT ( 'NONE',  ( 2.000000000000001776, 0.000000000000000000, 0.000000000000000000 ) ) ;
#63143 = ORIENTED_EDGE ( 'NONE', *, *, #8060, .F. ) ;
#63144 = DIRECTION ( 'NONE',  ( -0.9688695217174487784, 0.000000000000000000, -0.2475719085175095702 ) ) ;
#63145 = EDGE_CURVE ( 'NONE', #55082, #8885, #7459, .T. ) ;
#63146 = FACE_OUTER_BOUND ( 'NONE', #1411, .T. ) ;
#63147 = CARTESIAN_POINT ( 'NONE',  ( -35.00000000000000000, -2.220215194441821360, -11.98254675519230794 ) ) ;
#63148 = ADVANCED_FACE ( 'NONE', ( #50434 ), #20773, .F. ) ;
#63149 = CARTESIAN_POINT ( 'NONE',  ( 29.60113888844488272, 8.983404872736210578, 7.970891106847078689 ) ) ;
#63150 = CARTESIAN_POINT ( 'NONE',  ( 37.00000000000000711, 10.92721691015455754, -4.309077947445693724 ) ) ;
#63151 = CARTESIAN_POINT ( 'NONE',  ( 3.152665057736204535, -4.377619405894248139, -6.622010822085805160 ) ) ;
#63152 = CARTESIAN_POINT ( 'NONE',  ( -28.41827485489077532, 3.509237424706437292, -13.03592162821790801 ) ) ;
#63153 = EDGE_CURVE ( 'NONE', #16086, #27902, #12089, .T. ) ;
#63154 = VECTOR ( 'NONE', #3956, 1000.000000000000000 ) ;
#63155 = VERTEX_POINT ( 'NONE', #39443 ) ;
#63156 = FACE_OUTER_BOUND ( 'NONE', #25044, .T. ) ;
#63157 = EDGE_CURVE ( 'NONE', #52994, #12978, #26955, .T. ) ;
#63158 = ORIENTED_EDGE ( 'NONE', *, *, #50130, .T. ) ;
#63159 = CARTESIAN_POINT ( 'NONE',  ( -35.00000000000000000, 0.000000000000000000, 0.000000000000000000 ) ) ;
#63160 = CARTESIAN_POINT ( 'NONE',  ( -17.07517663476617287, -28.52001404462332346, -9.261390606240931689 ) ) ;
#63161 = DIRECTION ( 'NONE',  ( 0.000000000000000000, 0.01356324068817998940, -0.9999080150203990547 ) ) ;
#63162 = ADVANCED_FACE ( 'NONE', ( #9185 ), #29463, .T. ) ;
#63163 = CARTESIAN_POINT ( 'NONE',  ( -37.00000000000000711, -4.824807283154036952, -11.80185301892985805 ) ) ;
#63164 = CARTESIAN_POINT ( 'NONE',  ( 3.100650473569755317, -4.737096019059220176, -6.348250400753952860 ) ) ;
#63165 = ORIENTED_EDGE ( 'NONE', *, *, #53288, .T. ) ;
#63166 = AXIS2_PLACEMENT_3D ( 'NONE', #38668, #53959, #38320 ) ;
#63167 = CARTESIAN_POINT ( 'NONE',  ( 1.719304012341585475, 10.62216384465587993, -7.017415949613843296 ) ) ;
#63168 = CARTESIAN_POINT ( 'NONE',  ( 35.00000000000000000, 12.21925492305367200, 3.640372113593418391 ) ) ;
#63169 = CARTESIAN_POINT ( 'NONE',  ( -37.00000000000000711, 9.493370459201697642, 6.917234959366862057 ) ) ;
#63170 = DIRECTION ( 'NONE',  ( -1.000000000000000000, 0.000000000000000000, 0.000000000000000000 ) ) ;
#63171 = CARTESIAN_POINT ( 'NONE',  ( 2.000000000000001776, -4.915517050588423587, 4.717154614762070430 ) ) ;
#63172 = CIRCLE ( 'NONE', #24922, 5.000000000000001776 ) ;
#63173 = ORIENTED_EDGE ( 'NONE', *, *, #34120, .T. ) ;
#63174 = CARTESIAN_POINT ( 'NONE',  ( 2.556980015513285132, -0.2307166419793932888, -7.736177238086551000 ) ) ;
#63175 = CARTESIAN_POINT ( 'NONE',  ( 2.297017764050093280, -3.968300849026712651, -6.543724852214719334 ) ) ;
#63176 = AXIS2_PLACEMENT_3D ( 'NONE', #26995, #17346, #42249 ) ;
#63177 = VECTOR ( 'NONE', #34957, 1000.000000000000000 ) ;
#63178 = EDGE_CURVE ( 'NONE', #6530, #46064, #18483, .T. ) ;
#63179 = VERTEX_POINT ( 'NONE', #1846 ) ;
#63180 = CARTESIAN_POINT ( 'NONE',  ( -36.00000000000000711, 12.66641127287626034, 1.457575200925590453 ) ) ;
#63181 = VERTEX_POINT ( 'NONE', #20811 ) ;
#63182 = CARTESIAN_POINT ( 'NONE',  ( 2.280717697723838366, -6.543326285614656790, 3.958470850374288030 ) ) ;
#63183 = CARTESIAN_POINT ( 'NONE',  ( 3.047904605210340456, -3.577928268982041526, -7.047014837597050274 ) ) ;
#63184 = CARTESIAN_POINT ( 'NONE',  ( -27.10307689719060065, -1.703783570821478133, -1.615391801698475849 ) ) ;
#63185 = CARTESIAN_POINT ( 'NONE',  ( -35.00000000000000000, 0.000000000000000000, 0.000000000000000000 ) ) ;
#63186 = VERTEX_POINT ( 'NONE', #37072 ) ;
#63187 = EDGE_CURVE ( 'NONE', #45883, #39718, #28099, .T. ) ;
#63188 = EDGE_LOOP ( 'NONE', ( #17937, #52673, #9220, #5164 ) ) ;
#63189 = EDGE_LOOP ( 'NONE', ( #49679, #63051, #8690, #16554 ) ) ;
#63190 = CYLINDRICAL_SURFACE ( 'NONE', #63846, 1.500000000000000444 ) ;
#63191 = VECTOR ( 'NONE', #52302, 1000.000000000000000 ) ;
#63192 = CARTESIAN_POINT ( 'NONE',  ( 5.514624014163232779, 0.001574979445068891036, -0.003830004412313253118 ) ) ;
#63193 = ORIENTED_EDGE ( 'NONE', *, *, #3351, .T. ) ;
#63194 = DIRECTION ( 'NONE',  ( -1.000000000000000000, -1.836970198721029688E-16, 0.000000000000000000 ) ) ;
#63195 = CARTESIAN_POINT ( 'NONE',  ( 2.247206125382827935, -7.539576157880608420, 1.211896144126903163 ) ) ;
#63196 = ORIENTED_EDGE ( 'NONE', *, *, #38142, .F. ) ;
#63197 = LINE ( 'NONE', #22294, #64049 ) ;
#63198 = CARTESIAN_POINT ( 'NONE',  ( -36.00000000000000711, 8.235637554476644695, 9.733281772932192766 ) ) ;
#63199 = LINE ( 'NONE', #33916, #32403 ) ;
#63200 = ORIENTED_EDGE ( 'NONE', *, *, #56588, .T. ) ;
#63201 = ORIENTED_EDGE ( 'NONE', *, *, #7030, .T. ) ;
#63202 = CARTESIAN_POINT ( 'NONE',  ( 0.2648321136542692855, 12.08378267055568500, -1.986804758683992755 ) ) ;
#63203 = EDGE_CURVE ( 'NONE', #12979, #15531, #21813, .T. ) ;
#63204 = ORIENTED_EDGE ( 'NONE', *, *, #25445, .F. ) ;
#63205 = STYLED_ITEM ( 'NONE', ( #35775 ), #28612 ) ;
#63206 = ORIENTED_EDGE ( 'NONE', *, *, #51971, .T. ) ;
#63207 = LINE ( 'NONE', #43243, #48972 ) ;
#63208 = EDGE_CURVE ( 'NONE', #51465, #25715, #35435, .T. ) ;
#63209 = CARTESIAN_POINT ( 'NONE',  ( 8.006888830052231398, -32.29065697289608750, -12.88904745434341947 ) ) ;
#63210 = CYLINDRICAL_SURFACE ( 'NONE', #26288, 2.899999999999994582 ) ;
#63211 = CARTESIAN_POINT ( 'NONE',  ( 37.00000000000000711, 8.830544224263075392, 9.196955404009196755 ) ) ;
#63212 = CARTESIAN_POINT ( 'NONE',  ( 37.25000000000000711, -1.694065894508600678E-18, 0.000000000000000000 ) ) ;
#63213 = CARTESIAN_POINT ( 'NONE',  ( -27.15525204139121840, -1.831989866434736713, -1.707635684994332825 ) ) ;
#63214 = CARTESIAN_POINT ( 'NONE',  ( 6.787498709350838766, -5.788853919323486252, -10.51921472689792658 ) ) ;
#63215 = ORIENTED_EDGE ( 'NONE', *, *, #19492, .T. ) ;
#63216 = DIRECTION ( 'NONE',  ( -1.000000000000000000, -0.000000000000000000, -0.000000000000000000 ) ) ;
#63217 = EDGE_LOOP ( 'NONE', ( #4577, #941, #60666, #56328 ) ) ;
#63218 = CARTESIAN_POINT ( 'NONE',  ( 0.000000000000000000, 0.000000000000000000, 0.000000000000000000 ) ) ;
#63219 = DIRECTION ( 'NONE',  ( 0.000000000000000000, 0.9937233664769756780, -0.1118654143051654171 ) ) ;
#63220 = VERTEX_POINT ( 'NONE', #6186 ) ;
#63221 = CARTESIAN_POINT ( 'NONE',  ( 35.00000000000000000, 2.185196060784047045, 11.54110654723646157 ) ) ;
#63222 = FACE_OUTER_BOUND ( 'NONE', #1247, .T. ) ;
#63223 = CARTESIAN_POINT ( 'NONE',  ( 0.2801149460245133671, -2.320387321174087969, -12.02936836014265864 ) ) ;
#63224 = EDGE_CURVE ( 'NONE', #8907, #50922, #11475, .T. ) ;
#63225 = CIRCLE ( 'NONE', #25028, 5.000000000000000000 ) ;
#63226 = ORIENTED_EDGE ( 'NONE', *, *, #40597, .T. ) ;
#63227 = ORIENTED_EDGE ( 'NONE', *, *, #30522, .F. ) ;
#63228 = DIRECTION ( 'NONE',  ( -1.000000000000000000, 0.000000000000000000, 0.000000000000000000 ) ) ;
#63229 = ADVANCED_FACE ( 'NONE', ( #32410 ), #36757, .F. ) ;
#63230 = ORIENTED_EDGE ( 'NONE', *, *, #25721, .T. ) ;
#63231 = CARTESIAN_POINT ( 'NONE',  ( 1.948354844646893458, -11.46941405766446920, -3.407825014329160407 ) ) ;
#63232 = DIRECTION ( 'NONE',  ( -1.000000000000000000, 0.000000000000000000, -0.000000000000000000 ) ) ;
#63233 = EDGE_CURVE ( 'NONE', #18752, #32907, #40764, .T. ) ;
#63234 = CARTESIAN_POINT ( 'NONE',  ( 2.000000000000001776, 5.107597897712347290, 4.693343793638412365 ) ) ;
#63235 = CARTESIAN_POINT ( 'NONE',  ( -17.68548993317135398, -8.030202814678021994, 8.922382581021231829 ) ) ;
#63236 = ORIENTED_EDGE ( 'NONE', *, *, #22619, .F. ) ;
#63237 = DIRECTION ( 'NONE',  ( -1.000000000000000000, 0.000000000000000000, 0.000000000000000000 ) ) ;
#63238 = AXIS2_PLACEMENT_3D ( 'NONE', #48231, #17627, #33229 ) ;
#63239 = ADVANCED_FACE ( 'NONE', ( #47721 ), #61357, .T. ) ;
#63240 = CARTESIAN_POINT ( 'NONE',  ( 2.639814597422737830, -7.600559958731733623, -1.600543348184890080 ) ) ;
#63241 = DIRECTION ( 'NONE',  ( -1.000000000000000000, 0.000000000000000000, 0.000000000000000000 ) ) ;
#63242 = CARTESIAN_POINT ( 'NONE',  ( 37.00000000000000711, 2.021542716731571154, 12.01765980939839196 ) ) ;
#63243 = DIRECTION ( 'NONE',  ( 0.000000000000000000, 0.000000000000000000, 1.000000000000000000 ) ) ;
#63244 = CARTESIAN_POINT ( 'NONE',  ( 2.242418902651938772, -5.783980263416061085, 4.983487297755536005 ) ) ;
#63245 = CARTESIAN_POINT ( 'NONE',  ( 2.305787727787083519, 5.047606869483132641, -5.756228004061408221 ) ) ;
#63246 = EDGE_LOOP ( 'NONE', ( #53037, #59668, #61931, #13648 ) ) ;
#63247 = CARTESIAN_POINT ( 'NONE',  ( 2.262775599886255762, -0.1412024122916401558, 7.640237753423681610 ) ) ;
#63248 = EDGE_CURVE ( 'NONE', #16664, #35283, #16150, .T. ) ;
#63249 = ORIENTED_EDGE ( 'NONE', *, *, #30338, .F. ) ;
#63250 = DIRECTION ( 'NONE',  ( 1.000000000000000000, 0.000000000000000000, 0.000000000000000000 ) ) ;
#63251 = CARTESIAN_POINT ( 'NONE',  ( 2.941278708680199916, 6.021511413163979753, -1.198640839021246851 ) ) ;
#63252 = LINE ( 'NONE', #18388, #52375 ) ;
#63253 = EDGE_LOOP ( 'NONE', ( #9231, #20450, #60164, #41125 ) ) ;
#63254 = CARTESIAN_POINT ( 'NONE',  ( 2.241506898688419458, 4.877157973187056683, -5.873558213059427047 ) ) ;
#63255 = ORIENTED_EDGE ( 'NONE', *, *, #52424, .F. ) ;
#63256 = CYLINDRICAL_SURFACE ( 'NONE', #16856, 2.899999999999994582 ) ;
#63257 = ORIENTED_EDGE ( 'NONE', *, *, #37196, .T. ) ;
#63258 = EDGE_LOOP ( 'NONE', ( #6892, #15681, #64701, #38784 ) ) ;
#63259 = DIRECTION ( 'NONE',  ( -1.000000000000000000, -0.000000000000000000, 0.000000000000000000 ) ) ;
#63260 = CIRCLE ( 'NONE', #5965, 5.000000000000000888 ) ;
#63261 = CARTESIAN_POINT ( 'NONE',  ( -22.29479313954897890, -3.360948587163224310, -1.627767898183759332 ) ) ;
#63262 = VERTEX_POINT ( 'NONE', #52397 ) ;
#63263 = DIRECTION ( 'NONE',  ( -1.000000000000000000, 0.000000000000000000, -0.000000000000000000 ) ) ;
#63264 = DIRECTION ( 'NONE',  ( 1.000000000000000000, 0.000000000000000000, 0.000000000000000000 ) ) ;
#63265 = CARTESIAN_POINT ( 'NONE',  ( -19.56743653832047514, -33.00000000000000000, -5.000000000000001776 ) ) ;
#63266 = CARTESIAN_POINT ( 'NONE',  ( 19.08014163997884083, 3.539499929403262968, 11.50397527077400106 ) ) ;
#63267 = VERTEX_POINT ( 'NONE', #17132 ) ;
#63268 = DIRECTION ( 'NONE',  ( -1.000000000000000000, -0.000000000000000000, -0.000000000000000000 ) ) ;
#63269 = DIRECTION ( 'NONE',  ( 1.000000000000000000, -0.000000000000000000, 0.000000000000000000 ) ) ;
#63270 = CARTESIAN_POINT ( 'NONE',  ( 2.000000000000001776, 0.000000000000000000, 0.000000000000000000 ) ) ;
#63272 = ORIENTED_EDGE ( 'NONE', *, *, #62206, .F. ) ;
#63271 = DIRECTION ( 'NONE',  ( -1.000000000000000000, -0.000000000000000000, -0.000000000000000000 ) ) ;
#63273 = CARTESIAN_POINT ( 'NONE',  ( -28.25740157508035821, 10.82141011665706465, -5.195967623798041224 ) ) ;
#63274 = EDGE_CURVE ( 'NONE', #2632, #63113, #25872, .T. ) ;
#63275 = EDGE_CURVE ( 'NONE', #57020, #60276, #13041, .T. ) ;
#63276 = ORIENTED_EDGE ( 'NONE', *, *, #53772, .T. ) ;
#63277 = CARTESIAN_POINT ( 'NONE',  ( 2.000000000000001776, 6.777474576704075382, -0.6925993764990371337 ) ) ;
#63278 = ORIENTED_EDGE ( 'NONE', *, *, #55642, .T. ) ;
#63279 = CARTESIAN_POINT ( 'NONE',  ( 2.241536586108913376, 7.171901127201328663, -2.617055111126378453 ) ) ;
#63280 = CARTESIAN_POINT ( 'NONE',  ( 0.3223008802179242460, 3.964361764750334860, -11.60682919296347926 ) ) ;
#63281 = ADVANCED_FACE ( 'NONE', ( #47409 ), #36430, .F. ) ;
#63282 = CARTESIAN_POINT ( 'NONE',  ( 5.536195898058073439, 0.008071068258923569036, 0.002666509901870094731 ) ) ;
#63283 = LINE ( 'NONE', #17753, #56689 ) ;
#63284 = CARTESIAN_POINT ( 'NONE',  ( -17.83419946441818027, -9.720786832536937538, 25.00000000000000000 ) ) ;
#63285 = DIRECTION ( 'NONE',  ( -1.000000000000000000, 0.000000000000000000, 0.000000000000000000 ) ) ;
#63286 = CARTESIAN_POINT ( 'NONE',  ( 2.241528039335008327, -5.858435878248543283, 4.895273998033984775 ) ) ;
#63287 = VERTEX_POINT ( 'NONE', #51429 ) ;
#63288 = ORIENTED_EDGE ( 'NONE', *, *, #64868, .F. ) ;
#63289 = CARTESIAN_POINT ( 'NONE',  ( 0.2676618633000453218, 12.03196378632210539, 2.284744117040117040 ) ) ;
#63290 = EDGE_LOOP ( 'NONE', ( #59952, #39822, #56906, #59315 ) ) ;
#63291 = ORIENTED_EDGE ( 'NONE', *, *, #45645, .F. ) ;
#63292 = DIRECTION ( 'NONE',  ( 1.000000000000000000, -0.000000000000000000, -0.000000000000000000 ) ) ;
#63293 = CARTESIAN_POINT ( 'NONE',  ( -22.29115169517546136, 3.355084543108111994, 1.614783311161169577 ) ) ;
#63294 = CARTESIAN_POINT ( 'NONE',  ( -37.00000000000000711, 10.02106554660708859, 7.882940143791811849 ) ) ;
#63295 = CARTESIAN_POINT ( 'NONE',  ( 0.3665391374699472626, -8.095513416941169993, -9.237363111276847505 ) ) ;
#63296 = DIRECTION ( 'NONE',  ( 1.000000000000000000, -0.000000000000000000, 0.000000000000000000 ) ) ;
#63297 = ADVANCED_FACE ( 'NONE', ( #31442 ), #51741, .T. ) ;
#63298 = CARTESIAN_POINT ( 'NONE',  ( 2.241352910868909643, -7.532448145350499225, -1.243507963608171174 ) ) ;
#63299 = DIRECTION ( 'NONE',  ( 0.000000000000000000, -0.8515178078024924213, 0.5243256840888473880 ) ) ;
#63300 = AXIS2_PLACEMENT_3D ( 'NONE', #47970, #47324, #17713 ) ;
#63301 =( BOUNDED_SURFACE ( )  B_SPLINE_SURFACE ( 3, 1, ( 
 ( #28002, #12678 ),
 ( #17700, #38282 ),
 ( #33637, #49289 ),
 ( #3744, #13029 ) ),
 .UNSPECIFIED., .F., .F., .F. ) 
 B_SPLINE_SURFACE_WITH_KNOTS ( ( 4, 4 ),
 ( 2, 2 ),
 ( 0.000000000000000000, 1.000000000000000000 ),
 ( 0.000000000000000000, 1.000000000000000000 ),
 .UNSPECIFIED. ) 
 GEOMETRIC_REPRESENTATION_ITEM ( )  RATIONAL_B_SPLINE_SURFACE ( (
 ( 1.000000000000000000, 1.000000000000000000),
 ( 0.9856612449720755231, 0.9999558406602322425),
 ( 0.9856612449720755231, 0.9999558406602322425),
 ( 1.000000000000000000, 1.000000000000000000) ) ) 
 REPRESENTATION_ITEM ( '' )  SURFACE ( )  );
#63302 = ORIENTED_EDGE ( 'NONE', *, *, #27879, .T. ) ;
#63303 = CARTESIAN_POINT ( 'NONE',  ( 2.000000000000001776, -6.201547234537033937, 2.820401998297862978 ) ) ;
#63304 = DIRECTION ( 'NONE',  ( -1.000000000000000000, 0.000000000000000000, 0.000000000000000000 ) ) ;
#63305 = B_SPLINE_CURVE_WITH_KNOTS ( 'NONE', 3,
 ( #18473, #3510, #7825, #59337, #29395, #64963, #39704, #38731, #13442, #3167, #39368, #49394 ),
 .UNSPECIFIED., .F., .F.,
 ( 4, 2, 2, 2, 2, 4 ),
 ( 0.006954109192215124878, 0.007747514422417968276, 0.008144217037519390842, 0.008540919652620814276, 0.009334324882823661143, 0.01012773011302650801 ),
 .UNSPECIFIED. ) ;
#63306 = EDGE_CURVE ( 'NONE', #11115, #27117, #5766, .T. ) ;
#63307 = DIRECTION ( 'NONE',  ( -1.000000000000000000, 0.000000000000000000, 0.000000000000000000 ) ) ;
#63308 = FACE_OUTER_BOUND ( 'NONE', #33302, .T. ) ;
#63309 = CARTESIAN_POINT ( 'NONE',  ( 5.516018279890452902, 0.006440244342253029219, 0.002104829434640694864 ) ) ;
#63310 = CYLINDRICAL_SURFACE ( 'NONE', #58538, 2.899999999999994582 ) ;
#63311 = CARTESIAN_POINT ( 'NONE',  ( -29.92777678363736626, -3.750539801530011985, 25.00000000000000000 ) ) ;
#63312 = VERTEX_POINT ( 'NONE', #17468 ) ;
#63313 = LINE ( 'NONE', #37059, #42908 ) ;
#63314 = FACE_OUTER_BOUND ( 'NONE', #58201, .T. ) ;
#63315 = CARTESIAN_POINT ( 'NONE',  ( -35.04643116707788408, -0.003844232202718234070, 0.01156612771643049375 ) ) ;
#63316 = FACE_OUTER_BOUND ( 'NONE', #41672, .T. ) ;
#63317 = DIRECTION ( 'NONE',  ( 0.000000000000000000, 0.01356324068817998940, -0.9999080150203989437 ) ) ;
#63318 = LINE ( 'NONE', #62339, #55333 ) ;
#63319 = ADVANCED_FACE ( 'NONE', ( #48712 ), #50098, .F. ) ;
#63320 = EDGE_LOOP ( 'NONE', ( #45213, #11692, #60498, #31620 ) ) ;
#63321 = CARTESIAN_POINT ( 'NONE',  ( -37.00000000000000711, -11.72397916322012890, 0.7214809346828189307 ) ) ;
#63322 = FACE_OUTER_BOUND ( 'NONE', #7936, .T. ) ;
#63323 = CARTESIAN_POINT ( 'NONE',  ( 2.290907136832898150, -4.792500160339676185, -5.963935563308297994 ) ) ;
#63324 = CARTESIAN_POINT ( 'NONE',  ( -37.00000000000000711, 0.000000000000000000, 0.000000000000000000 ) ) ;
#63325 = ORIENTED_EDGE ( 'NONE', *, *, #26344, .F. ) ;
#63326 = ADVANCED_FACE ( 'NONE', ( #63322 ), #23777, .T. ) ;
#63327 = CARTESIAN_POINT ( 'NONE',  ( 0.3109076770649043531, 2.361108455562842767, 12.03190317807024989 ) ) ;
#63328 = CARTESIAN_POINT ( 'NONE',  ( 2.000000000000001776, 0.000000000000000000, 0.000000000000000000 ) ) ;
#63329 = ORIENTED_EDGE ( 'NONE', *, *, #34238, .T. ) ;
#63330 = ORIENTED_EDGE ( 'NONE', *, *, #32847, .F. ) ;
#63331 = AXIS2_PLACEMENT_3D ( 'NONE', #39814, #46133, #60101 ) ;
#63332 = CARTESIAN_POINT ( 'NONE',  ( 35.00000000000000000, 2.905556151562782574, 11.38112321385047210 ) ) ;
#63333 = EDGE_CURVE ( 'NONE', #1853, #34412, #58732, .T. ) ;
#63334 = CIRCLE ( 'NONE', #48519, 5.000000000000000888 ) ;
#63335 = FACE_OUTER_BOUND ( 'NONE', #48254, .T. ) ;
#63336 = EDGE_LOOP ( 'NONE', ( #57963, #2985, #26518, #26903 ) ) ;
#63337 = CARTESIAN_POINT ( 'NONE',  ( -47.00000000000000711, 0.000000000000000000, 0.000000000000000000 ) ) ;
#63338 = DIRECTION ( 'NONE',  ( -0.000000000000000000, 0.000000000000000000, -1.000000000000000000 ) ) ;
#63339 = CARTESIAN_POINT ( 'NONE',  ( 35.00000000000000000, 12.73293890771483738, 0.6593684648219080291 ) ) ;
#63340 = CARTESIAN_POINT ( 'NONE',  ( 2.280717697723837478, -7.556934756535378384, -1.173604464351679866 ) ) ;
#63341 = CARTESIAN_POINT ( 'NONE',  ( -27.63833054859100002, 10.11270778234927548, -6.466741440011825937 ) ) ;
#63342 = CARTESIAN_POINT ( 'NONE',  ( 0.4613984246114881116, 11.66278164635734882, 3.943860067443686557 ) ) ;
#63344 = ORIENTED_EDGE ( 'NONE', *, *, #46394, .T. ) ;
#63343 = LINE ( 'NONE', #7487, #40390 ) ;
#63345 = CARTESIAN_POINT ( 'NONE',  ( -37.00000000000000711, -8.146229107149334681, -9.063649021439044162 ) ) ;
#63346 = EDGE_CURVE ( 'NONE', #31517, #53149, #8783, .T. ) ;
#63347 = ADVANCED_FACE ( 'NONE', ( #48061 ), #56907, .F. ) ;
#63348 = VERTEX_POINT ( 'NONE', #17791 ) ;
#63349 = CARTESIAN_POINT ( 'NONE',  ( 26.34661844826604593, 13.08594712317291986, 3.317828791472332117 ) ) ;
#63350 = ORIENTED_EDGE ( 'NONE', *, *, #64460, .T. ) ;
#63351 = ORIENTED_EDGE ( 'NONE', *, *, #35309, .T. ) ;
#63352 = CARTESIAN_POINT ( 'NONE',  ( -14.11589373245165469, 8.250315036047107142, 10.68561190601526611 ) ) ;
#63353 = CARTESIAN_POINT ( 'NONE',  ( -22.27722015946439171, 3.628085906632232849, -0.6262261846986482139 ) ) ;
#63354 = CARTESIAN_POINT ( 'NONE',  ( -3.385148144206586274, 5.981256269455808905, 10.44061326340053775 ) ) ;
#63355 = CARTESIAN_POINT ( 'NONE',  ( -48.06591103469482817, -0.3868811097602570803, 6.642178517338849453 ) ) ;
#63356 = CARTESIAN_POINT ( 'NONE',  ( 22.57855258442565116, 3.026812727784649493, 13.15630665159948975 ) ) ;
#63357 = ORIENTED_EDGE ( 'NONE', *, *, #65487, .T. ) ;
#63358 = CARTESIAN_POINT ( 'NONE',  ( -22.27715526084302056, -0.4651416883073714592, -3.652257391294517319 ) ) ;
#63359 = CARTESIAN_POINT ( 'NONE',  ( 37.00000000000000711, 1.738225594540171670, 12.63095688309027054 ) ) ;
#63361 = ORIENTED_EDGE ( 'NONE', *, *, #5034, .T. ) ;
#63360 = CARTESIAN_POINT ( 'NONE',  ( 35.00000000000000000, 7.110831038798420600, 9.896810808925309288 ) ) ;
#63362 = VERTEX_POINT ( 'NONE', #32721 ) ;
#63363 = DIRECTION ( 'NONE',  ( 0.3865475372811021382, -0.9220659470476461061, -0.01937500237528736249 ) ) ;
#63364 = VERTEX_POINT ( 'NONE', #27758 ) ;
#63365 = CYLINDRICAL_SURFACE ( 'NONE', #42265, 5.000000000000000888 ) ;
#63366 = CARTESIAN_POINT ( 'NONE',  ( 0.3053067050349136391, -10.49978800868456652, -6.328522421120378993 ) ) ;
#63367 = CARTESIAN_POINT ( 'NONE',  ( 11.32888944540964360, 0.8054644877949781456, 13.47643349399415058 ) ) ;
#63368 = CARTESIAN_POINT ( 'NONE',  ( -22.31099767395441091, 3.142100240805189681, -2.106713667647935662 ) ) ;
#63369 = CARTESIAN_POINT ( 'NONE',  ( -37.25000000000000711, -27.56270118634207833, 0.7455576661145032480 ) ) ;
#63370 = CARTESIAN_POINT ( 'NONE',  ( -29.54343203963513886, 0.2941795591554937084, 13.49847162130717493 ) ) ;
#63371 = CARTESIAN_POINT ( 'NONE',  ( -35.00000000000000000, -9.557269938331609538, 7.561043153947932360 ) ) ;
#63372 = VERTEX_POINT ( 'NONE', #63643 ) ;
#63373 = CARTESIAN_POINT ( 'NONE',  ( 17.27839441901508977, 12.20388373500084711, 5.771933972472493402 ) ) ;
#63374 = VECTOR ( 'NONE', #60278, 1000.000000000000227 ) ;
#63375 = ORIENTED_EDGE ( 'NONE', *, *, #32937, .F. ) ;
#63376 = CARTESIAN_POINT ( 'NONE',  ( -9.328146843779920871, -11.86223754448519507, -6.454750433817429744 ) ) ;
#63377 = EDGE_CURVE ( 'NONE', #41285, #52499, #62919, .T. ) ;
#63378 = CYLINDRICAL_SURFACE ( 'NONE', #1047, 2.977897737712716708 ) ;
#63379 = CARTESIAN_POINT ( 'NONE',  ( 0.2653519789438738563, -11.51519617080779234, -4.167744179924032011 ) ) ;
#63380 = ORIENTED_EDGE ( 'NONE', *, *, #22821, .T. ) ;
#63381 = EDGE_CURVE ( 'NONE', #40353, #45412, #22922, .T. ) ;
#63382 = ORIENTED_EDGE ( 'NONE', *, *, #37745, .T. ) ;
#63383 = CARTESIAN_POINT ( 'NONE',  ( -27.08871896697731785, 0.1856437051692989004, 2.297279805116099638 ) ) ;
#63384 = AXIS2_PLACEMENT_3D ( 'NONE', #9695, #64893, #34634 ) ;
#63385 = VERTEX_POINT ( 'NONE', #7822 ) ;
#63386 = CARTESIAN_POINT ( 'NONE',  ( 0.3610902822527232159, 7.689482111308977963, -9.572034936626812041 ) ) ;
#63387 = FACE_OUTER_BOUND ( 'NONE', #33943, .T. ) ;
#63388 = CARTESIAN_POINT ( 'NONE',  ( -27.08430418657510685, -2.086666645150138333, -0.9470735946419284179 ) ) ;
#63389 = CARTESIAN_POINT ( 'NONE',  ( 0.2650492433740075371, -0.1101179680248120796, -12.24562113162318866 ) ) ;
#63390 = ORIENTED_EDGE ( 'NONE', *, *, #2080, .T. ) ;
#63391 = CARTESIAN_POINT ( 'NONE',  ( 0.2739690278137236756, 12.09341522051409790, 1.946552041162949997 ) ) ;
#63392 = CARTESIAN_POINT ( 'NONE',  ( -22.30861784526116054, -2.600591904828400747, 2.737516124790397853 ) ) ;
#63393 = CARTESIAN_POINT ( 'NONE',  ( -29.46823373269320712, 0.7215570029219251502, -13.48712589208137125 ) ) ;
#63394 = CARTESIAN_POINT ( 'NONE',  ( -35.00000000000000000, 2.220215194441899076, 11.98254675519229195 ) ) ;
#63395 = ADVANCED_FACE ( 'NONE', ( #8799 ), #2845, .F. ) ;
#63396 = CARTESIAN_POINT ( 'NONE',  ( 2.241352910868908310, -0.08337961031698915004, -7.633946224498474820 ) ) ;
#63397 = CARTESIAN_POINT ( 'NONE',  ( 0.000000000000000000, -3.341639490130703827, -6.078525953551491057 ) ) ;
#63398 = EDGE_CURVE ( 'NONE', #28034, #44608, #35121, .T. ) ;
#63399 = VERTEX_POINT ( 'NONE', #34386 ) ;
#63400 = EDGE_CURVE ( 'NONE', #46189, #25502, #30032, .T. ) ;
#63401 = CARTESIAN_POINT ( 'NONE',  ( 2.000000000000001776, 4.962980376314068742, 4.846014654777798469 ) ) ;
#63402 = CARTESIAN_POINT ( 'NONE',  ( 5.516018279890452902, -0.0002248006052448983238, -0.006771744149385263388 ) ) ;
#63403 = CARTESIAN_POINT ( 'NONE',  ( -14.91771861688918399, -27.95837112815216230, -11.21176701200369763 ) ) ;
#63404 = VERTEX_POINT ( 'NONE', #14733 ) ;
#63405 = EDGE_CURVE ( 'NONE', #56864, #42378, #5613, .T. ) ;
#63406 = CARTESIAN_POINT ( 'NONE',  ( -7.954836218480799026, -1.696952596288976434, -13.39419882916700644 ) ) ;
#63407 = CARTESIAN_POINT ( 'NONE',  ( 0.3675815128205894289, -8.093875121226139058, 9.235491948679980467 ) ) ;
#63408 = DIRECTION ( 'NONE',  ( -0.000000000000000000, -1.000000000000000000, -0.000000000000000000 ) ) ;
#63409 = CARTESIAN_POINT ( 'NONE',  ( 5.536195898058073439, 0.006672323185952914494, 0.005266167600748188592 ) ) ;
#63410 = CARTESIAN_POINT ( 'NONE',  ( 35.00000000000000000, 4.725891942574903304, 10.75351884295722193 ) ) ;
#63411 = ORIENTED_EDGE ( 'NONE', *, *, #25445, .T. ) ;
#63413 = EDGE_LOOP ( 'NONE', ( #42297, #8413, #46537, #47742 ) ) ;
#63412 = EDGE_CURVE ( 'NONE', #3821, #14132, #10102, .T. ) ;
#63414 = CARTESIAN_POINT ( 'NONE',  ( 0.2648978790185593790, 1.996248716311628479, 12.08224454301449313 ) ) ;
#63415 = ORIENTED_EDGE ( 'NONE', *, *, #13789, .T. ) ;
#63416 = FACE_OUTER_BOUND ( 'NONE', #40419, .T. ) ;
#63417 = CARTESIAN_POINT ( 'NONE',  ( 0.2739690278137253965, -9.499928778897061221, -7.732471127692689628 ) ) ;
#63418 = FACE_OUTER_BOUND ( 'NONE', #32977, .T. ) ;
#63419 = FACE_OUTER_BOUND ( 'NONE', #20321, .T. ) ;
#63420 = CARTESIAN_POINT ( 'NONE',  ( 2.241528039335009215, -3.830846649711559859, 6.603755931420473679 ) ) ;
#63421 = EDGE_CURVE ( 'NONE', #30828, #10832, #36396, .T. ) ;
#63422 = CARTESIAN_POINT ( 'NONE',  ( 2.255723233589912446, 5.766109278027927054, 5.010912740809442489 ) ) ;
#63423 = CARTESIAN_POINT ( 'NONE',  ( -32.00000000000000711, 5.510910596163084625E-16, 0.000000000000000000 ) ) ;
#63424 = ORIENTED_EDGE ( 'NONE', *, *, #28534, .F. ) ;
#63425 = ORIENTED_EDGE ( 'NONE', *, *, #38256, .F. ) ;
#63426 = DIRECTION ( 'NONE',  ( 0.000000000000000000, 0.8369827122275363962, 0.5472293298355243030 ) ) ;
#63427 = ORIENTED_EDGE ( 'NONE', *, *, #29003, .T. ) ;
#63428 = VECTOR ( 'NONE', #51127, 1000.000000000000000 ) ;
#63429 = CARTESIAN_POINT ( 'NONE',  ( -22.30398854582848145, 2.594196582747005930, -2.724439933030905259 ) ) ;
#63430 = CARTESIAN_POINT ( 'NONE',  ( 1.375507693220862970, 8.553661013313627492, -9.273955665125701131 ) ) ;
#63431 = VECTOR ( 'NONE', #41355, 1000.000000000000000 ) ;
#63432 = EDGE_CURVE ( 'NONE', #32449, #433, #2428, .T. ) ;
#63433 = DIRECTION ( 'NONE',  ( 0.000000000000000000, 0.000000000000000000, -1.000000000000000000 ) ) ;
#63434 = ORIENTED_EDGE ( 'NONE', *, *, #63977, .T. ) ;
#63435 = CARTESIAN_POINT ( 'NONE',  ( 0.2958664285830411300, 5.936220506376383987, -10.72286791615082358 ) ) ;
#63436 = CARTESIAN_POINT ( 'NONE',  ( 2.256373768223410625, 6.548448293197187908, -3.934258165099992155 ) ) ;
#63437 = CARTESIAN_POINT ( 'NONE',  ( -22.27384469013075829, -3.663183248998797659, 0.3730095848193237251 ) ) ;
#63438 = VERTEX_POINT ( 'NONE', #49690 ) ;
#63439 = ORIENTED_EDGE ( 'NONE', *, *, #44522, .F. ) ;
#63440 = CARTESIAN_POINT ( 'NONE',  ( 1.000000000000000888, -6.160607635185433750, 4.277489166005560506 ) ) ;
#63441 = ORIENTED_EDGE ( 'NONE', *, *, #30462, .T. ) ;
#63442 = DIRECTION ( 'NONE',  ( -1.000000000000000000, 0.000000000000000000, 0.000000000000000000 ) ) ;
#63443 = VERTEX_POINT ( 'NONE', #50677 ) ;
#63444 = B_SPLINE_CURVE_WITH_KNOTS ( 'NONE', 3,
 ( #7168, #62062, #6867, #12163, #16171, #22814, #27138, #16821, #1869, #63031, #51766, #27784, #43071, #57075, #36456, #21835, #21498, #53055, #42082, #12473 ),
 .UNSPECIFIED., .F., .F.,
 ( 4, 2, 2, 2, 2, 2, 2, 2, 2, 4 ),
 ( 0.000000000000000000, 0.001199198029652149286, 0.002398396059304298573, 0.003597594088956448076, 0.004197193103782522611, 0.004796792118608597146, 0.005995990148260746215, 0.007195188177912896152, 0.008394386207565045221, 0.009593584237217194291 ),
 .UNSPECIFIED. ) ;
#63445 = VERTEX_POINT ( 'NONE', #9763 ) ;
#63446 = CARTESIAN_POINT ( 'NONE',  ( 0.3474126878361774584, 4.439989671676218386, 11.44231427242451460 ) ) ;
#63447 = CARTESIAN_POINT ( 'NONE',  ( 2.241311220309522234, 4.978033760028339749, -5.788190037953302891 ) ) ;
#63448 = DIRECTION ( 'NONE',  ( -1.000000000000000000, 0.000000000000000000, 0.000000000000000000 ) ) ;
#63449 = CARTESIAN_POINT ( 'NONE',  ( 0.2706063244538048362, 8.006269958070731718, -9.268878137104316295 ) ) ;
#63450 = FACE_OUTER_BOUND ( 'NONE', #51709, .T. ) ;
#63451 = CARTESIAN_POINT ( 'NONE',  ( 0.3109076770649005228, 11.60048803586498778, 3.971171685427437037 ) ) ;
#63452 = VERTEX_POINT ( 'NONE', #30382 ) ;
#63453 = CARTESIAN_POINT ( 'NONE',  ( 2.000000000000001776, -1.018311147294196806, 6.861346417234461370 ) ) ;
#63454 = CARTESIAN_POINT ( 'NONE',  ( 2.305787727787083519, 4.792270232040894307, 5.970480882365237996 ) ) ;
#63455 = CARTESIAN_POINT ( 'NONE',  ( 2.260457164927710316, 3.699855525212757179, -6.685239696063914216 ) ) ;
#63456 = DIRECTION ( 'NONE',  ( 0.000000000000000000, -0.01356324068817998940, 0.9999080150203990547 ) ) ;
#63457 = DIRECTION ( 'NONE',  ( -1.000000000000000000, 0.000000000000000000, 0.000000000000000000 ) ) ;
#63458 = CARTESIAN_POINT ( 'NONE',  ( 1.549075743846619391, 0.6747257554056480533, -12.65619669351077548 ) ) ;
#63459 = CARTESIAN_POINT ( 'NONE',  ( -27.08421860617808008, 1.394838596205212555, 1.817782142550182112 ) ) ;
#63460 = CARTESIAN_POINT ( 'NONE',  ( 0.2801149460245140332, -11.57793225195134745, -4.005169813315220040 ) ) ;
#63461 = CARTESIAN_POINT ( 'NONE',  ( 2.903928887688508098, -8.753847148605458983, 0.5297564406061141540 ) ) ;
#63462 = CIRCLE ( 'NONE', #64544, 4.999999999999999112 ) ;
#63463 = EDGE_CURVE ( 'NONE', #52684, #23475, #55664, .T. ) ;
#63464 = ORIENTED_EDGE ( 'NONE', *, *, #13348, .T. ) ;
#63465 = DIRECTION ( 'NONE',  ( 1.000000000000000000, 0.000000000000000000, 0.000000000000000000 ) ) ;
#63466 = AXIS2_PLACEMENT_3D ( 'NONE', #2762, #47959, #63550 ) ;
#63467 = VERTEX_POINT ( 'NONE', #30048 ) ;
#63468 = CARTESIAN_POINT ( 'NONE',  ( 25.00000000000000355, -9.999999999999998224, 5.000000000000002665 ) ) ;
#63469 = CARTESIAN_POINT ( 'NONE',  ( 2.259830038564997423, 5.940579220577243191, -4.804964945109127861 ) ) ;
#63470 = CARTESIAN_POINT ( 'NONE',  ( 35.00000000000000000, 4.705694406421931860E-17, -3.469127814946512892E-15 ) ) ;
#63471 = CARTESIAN_POINT ( 'NONE',  ( -25.75517367794919465, -7.863739964200362031, 10.97545609339455019 ) ) ;
#63472 = CARTESIAN_POINT ( 'NONE',  ( 2.907497136249922676, 7.791429554169492455, 1.009055026158340862 ) ) ;
#63473 = ORIENTED_EDGE ( 'NONE', *, *, #21039, .F. ) ;
#63474 = CYLINDRICAL_SURFACE ( 'NONE', #8040, 5.000000000000000888 ) ;
#63475 = CYLINDRICAL_SURFACE ( 'NONE', #43803, 13.50000000000000178 ) ;
#63476 = CARTESIAN_POINT ( 'NONE',  ( 2.000000000000001776, -1.693411908627144635, -7.306323022404617618 ) ) ;
#63477 = AXIS2_PLACEMENT_3D ( 'NONE', #39751, #55370, #9157 ) ;
#63478 = CARTESIAN_POINT ( 'NONE',  ( -3.167941684595230623, 12.87051617182347130, 4.089067520392708488 ) ) ;
#63479 = EDGE_CURVE ( 'NONE', #50867, #45916, #25771, .T. ) ;
#63480 = DIRECTION ( 'NONE',  ( 0.000000000000000000, 0.3193015301359742319, 0.9476531711828044546 ) ) ;
#63481 =( BOUNDED_CURVE ( )  B_SPLINE_CURVE ( 3, ( #48126, #28159, #53093, #39095 ),
 .UNSPECIFIED., .F., .F. ) 
 B_SPLINE_CURVE_WITH_KNOTS ( ( 4, 4 ),
 ( 3.532417926517623652, 3.558043830773766736 ),
 .UNSPECIFIED. ) 
 CURVE ( )  GEOMETRIC_REPRESENTATION_ITEM ( )  RATIONAL_B_SPLINE_CURVE ( ( 1.000000000000000000, 0.9999452768345937770, 0.9999452768345937770, 1.000000000000000000 ) ) 
 REPRESENTATION_ITEM ( '' )  );
#63482 = ORIENTED_EDGE ( 'NONE', *, *, #46641, .T. ) ;
#63483 = EDGE_CURVE ( 'NONE', #63404, #42570, #29393, .T. ) ;
#63484 = CYLINDRICAL_SURFACE ( 'NONE', #64684, 12.18650000000000055 ) ;
#63485 = EDGE_CURVE ( 'NONE', #61726, #52172, #34318, .T. ) ;
#63486 = DIRECTION ( 'NONE',  ( 0.000000000000000000, -0.01356324068817998940, 0.9999080150203990547 ) ) ;
#63487 = CARTESIAN_POINT ( 'NONE',  ( -3.683412895334400528, -30.77133338175680777, 15.02788192793085109 ) ) ;
#63488 = EDGE_LOOP ( 'NONE', ( #52726, #57582, #60177, #46086 ) ) ;
#63489 = CARTESIAN_POINT ( 'NONE',  ( 8.937200413559443390, 4.476360154859203355, -11.13383131558893346 ) ) ;
#63490 = ORIENTED_EDGE ( 'NONE', *, *, #41123, .T. ) ;
#63491 = CARTESIAN_POINT ( 'NONE',  ( 37.00000000000000711, 2.143131898507868297E-16, 1.750000000000000000 ) ) ;
#63492 = DIRECTION ( 'NONE',  ( 0.000000000000000000, 0.000000000000000000, 1.000000000000000000 ) ) ;
#63493 = LINE ( 'NONE', #22965, #22639 ) ;
#63494 = CYLINDRICAL_SURFACE ( 'NONE', #27958, 12.74999999999999822 ) ;
#63495 = ADVANCED_FACE ( 'NONE', ( #55978 ), #27560, .F. ) ;
#63496 = CARTESIAN_POINT ( 'NONE',  ( 1.937114397841935398, -10.38782037574611472, -7.538912286488452352 ) ) ;
#63497 = ORIENTED_EDGE ( 'NONE', *, *, #10015, .F. ) ;
#63498 = EDGE_CURVE ( 'NONE', #34267, #44216, #1380, .T. ) ;
#63499 = ORIENTED_EDGE ( 'NONE', *, *, #58352, .T. ) ;
#63500 = VERTEX_POINT ( 'NONE', #10413 ) ;
#63501 = CARTESIAN_POINT ( 'NONE',  ( 35.00000000000000000, -4.561791185930327508, 11.90598845858537835 ) ) ;
#63502 = EDGE_CURVE ( 'NONE', #48073, #63287, #26061, .T. ) ;
#63503 = CIRCLE ( 'NONE', #35916, 5.000000000000001776 ) ;
#63504 = DIRECTION ( 'NONE',  ( 0.000000000000000000, 0.3218879778915972878, -0.9467777615094571386 ) ) ;
#63505 = ORIENTED_EDGE ( 'NONE', *, *, #7197, .T. ) ;
#63506 = DIRECTION ( 'NONE',  ( 1.000000000000000000, -0.000000000000000000, 0.000000000000000000 ) ) ;
#63507 = EDGE_CURVE ( 'NONE', #30401, #6868, #41009, .T. ) ;
#63508 = DIRECTION ( 'NONE',  ( -1.000000000000000000, -0.000000000000000000, 0.000000000000000000 ) ) ;
#63510 = ORIENTED_EDGE ( 'NONE', *, *, #63735, .F. ) ;
#63509 = AXIS2_PLACEMENT_3D ( 'NONE', #17862, #48144, #1275 ) ;
#63511 = LINE ( 'NONE', #27613, #54532 ) ;
#63512 = DIRECTION ( 'NONE',  ( 1.000000000000000000, 0.000000000000000000, 0.000000000000000000 ) ) ;
#63513 = LINE ( 'NONE', #58566, #35601 ) ;
#63514 = ORIENTED_EDGE ( 'NONE', *, *, #34823, .F. ) ;
#63516 = EDGE_CURVE ( 'NONE', #39606, #60329, #61606, .T. ) ;
#63515 = ORIENTED_EDGE ( 'NONE', *, *, #789, .F. ) ;
#63517 = AXIS2_PLACEMENT_3D ( 'NONE', #4438, #55945, #56262 ) ;
#63518 = CARTESIAN_POINT ( 'NONE',  ( 37.00000000000000711, 4.705694406421931860E-17, -3.469127814946512892E-15 ) ) ;
#63519 = ORIENTED_EDGE ( 'NONE', *, *, #16220, .T. ) ;
#63520 = CARTESIAN_POINT ( 'NONE',  ( 35.00000000000000000, -9.896810808925339487, 7.110831038798382409 ) ) ;
#63521 = ORIENTED_EDGE ( 'NONE', *, *, #3503, .F. ) ;
#63522 = VECTOR ( 'NONE', #25048, 1000.000000000000000 ) ;
#63523 = DIRECTION ( 'NONE',  ( -1.000000000000000000, 0.000000000000000000, 0.000000000000000000 ) ) ;
#63524 = DIRECTION ( 'NONE',  ( -1.000000000000000000, -0.000000000000000000, 0.000000000000000000 ) ) ;
#63525 = CARTESIAN_POINT ( 'NONE',  ( 2.241352910868908310, 2.532612177304540246, -7.202080440908716241 ) ) ;
#63526 = DIRECTION ( 'NONE',  ( -1.000000000000000000, 0.000000000000000000, -0.000000000000000000 ) ) ;
#63527 = CYLINDRICAL_SURFACE ( 'NONE', #51062, 7.499999999999988454 ) ;
#63528 = CARTESIAN_POINT ( 'NONE',  ( 145.1370849898475797, 3.309064568108273190E-14, 0.000000000000000000 ) ) ;
#63529 = CYLINDRICAL_SURFACE ( 'NONE', #20400, 2.899999999999994582 ) ;
#63530 = ORIENTED_EDGE ( 'NONE', *, *, #54895, .F. ) ;
#63531 = DIRECTION ( 'NONE',  ( -1.000000000000000000, 0.000000000000000000, -0.000000000000000000 ) ) ;
#63532 = VERTEX_POINT ( 'NONE', #51669 ) ;
#63533 = CARTESIAN_POINT ( 'NONE',  ( -36.00000000000000711, -5.556331110570328136, -11.47561260193582733 ) ) ;
#63534 = ORIENTED_EDGE ( 'NONE', *, *, #33652, .T. ) ;
#63535 = CYLINDRICAL_SURFACE ( 'NONE', #3240, 6.615568257478080305 ) ;
#63536 = CARTESIAN_POINT ( 'NONE',  ( -35.04709527796842394, 0.001082316405385738700, -0.01231589140599127774 ) ) ;
#63537 = VERTEX_POINT ( 'NONE', #46017 ) ;
#63538 = EDGE_CURVE ( 'NONE', #18920, #56695, #56298, .T. ) ;
#63539 = AXIS2_PLACEMENT_3D ( 'NONE', #49204, #43515, #58863 ) ;
#63540 = ORIENTED_EDGE ( 'NONE', *, *, #57829, .F. ) ;
#63541 = PLANE ( 'NONE',  #36451 ) ;
#63542 = CIRCLE ( 'NONE', #18950, 12.74999999999999822 ) ;
#63543 = VERTEX_POINT ( 'NONE', #37327 ) ;
#63544 = DIRECTION ( 'NONE',  ( 1.000000000000000000, 0.000000000000000000, -0.000000000000000000 ) ) ;
#63545 = SURFACE_STYLE_USAGE ( .BOTH. , #16468 ) ;
#63546 = CARTESIAN_POINT ( 'NONE',  ( 2.241449424704146320, -1.386092121067156180, -7.507583637787362818 ) ) ;
#63547 = CARTESIAN_POINT ( 'NONE',  ( 0.3218525148189836926, -9.236582760335920739, -8.069481661595439448 ) ) ;
#63548 = ORIENTED_EDGE ( 'NONE', *, *, #4123, .F. ) ;
#63549 = EDGE_CURVE ( 'NONE', #62664, #33142, #12183, .T. ) ;
#63550 = DIRECTION ( 'NONE',  ( 0.000000000000000000, -0.01356324068817998940, 0.9999080150203990547 ) ) ;
#63551 = CIRCLE ( 'NONE', #61464, 5.000000000000001776 ) ;
#63552 = EDGE_CURVE ( 'NONE', #60603, #1207, #15367, .T. ) ;
#63553 = CIRCLE ( 'NONE', #19011, 5.000000000000000000 ) ;
#63554 = VECTOR ( 'NONE', #53728, 1000.000000000000000 ) ;
#63555 = CARTESIAN_POINT ( 'NONE',  ( 3.527934398658575610, -26.69696348912971473, -16.00979375678724637 ) ) ;
#63556 = DIRECTION ( 'NONE',  ( 0.000000000000000000, -0.2149704402110318713, 0.9766205557100849921 ) ) ;
#63558 = VECTOR ( 'NONE', #25352, 1000.000000000000000 ) ;
#63557 = DIRECTION ( 'NONE',  ( 1.000000000000000000, -0.000000000000000000, -0.000000000000000000 ) ) ;
#63559 = ADVANCED_FACE ( 'NONE', ( #21044 ), #47564, .F. ) ;
#63560 = CARTESIAN_POINT ( 'NONE',  ( 0.2648978790185584908, 7.769924372105204036, 9.465406350830633642 ) ) ;
#63561 = CARTESIAN_POINT ( 'NONE',  ( 2.000000000000001776, 0.000000000000000000, 0.000000000000000000 ) ) ;
#63562 = CARTESIAN_POINT ( 'NONE',  ( -22.39032720737627002, -0.9101257950220824622, 3.916738514147011685 ) ) ;
#63563 = VECTOR ( 'NONE', #41452, 1000.000000000000000 ) ;
#63564 = ORIENTED_EDGE ( 'NONE', *, *, #23214, .T. ) ;
#63565 = DIRECTION ( 'NONE',  ( 0.000000000000000000, 0.000000000000000000, -1.000000000000000000 ) ) ;
#63566 = ORIENTED_EDGE ( 'NONE', *, *, #5431, .T. ) ;
#63567 = CARTESIAN_POINT ( 'NONE',  ( -35.00000000000000000, -2.497432891016921008, 11.47758908105693720 ) ) ;
#63568 = DIRECTION ( 'NONE',  ( -1.000000000000000000, 0.000000000000000000, 0.000000000000000000 ) ) ;
#63569 = CARTESIAN_POINT ( 'NONE',  ( 0.7446945582529739260, -9.270687147117394389, -8.243982823409684357 ) ) ;
#63570 = ORIENTED_EDGE ( 'NONE', *, *, #58159, .F. ) ;
#63571 = DIRECTION ( 'NONE',  ( 0.000000000000000000, 0.000000000000000000, -1.000000000000000000 ) ) ;
#63572 = ORIENTED_EDGE ( 'NONE', *, *, #58501, .F. ) ;
#63573 = CARTESIAN_POINT ( 'NONE',  ( -35.00000000000000000, -0.3137578094508303161, -12.74613886779085448 ) ) ;
#63574 = EDGE_LOOP ( 'NONE', ( #48609, #13410, #54433, #34572 ) ) ;
#63575 = ORIENTED_EDGE ( 'NONE', *, *, #63949, .T. ) ;
#63576 = B_SPLINE_CURVE_WITH_KNOTS ( 'NONE', 3,
 ( #36214, #36564, #56522, #10967, #25265, #31252, #51558, #6003, #19953, #26259, #5005, #11293, #55540, #45543, #31562, #51865 ),
 .UNSPECIFIED., .F., .F.,
 ( 4, 3, 3, 3, 3, 4 ),
 ( 4.336808689942017736E-19, 0.0002176109881720250270, 0.0004352086762394615340, 0.0006528017811446905436, 0.0007615147961451741200, 0.0009453342004947430264 ),
 .UNSPECIFIED. ) ;
#63577 = CARTESIAN_POINT ( 'NONE',  ( 0.2956976708475470006, -7.708404409946589375, -9.528782683728165281 ) ) ;
#63578 = ADVANCED_FACE ( 'NONE', ( #16719 ), #51985, .T. ) ;
#63579 = CARTESIAN_POINT ( 'NONE',  ( 2.260457164927185847, -7.131443009846823777, 2.742969430850495272 ) ) ;
#63580 = ORIENTED_EDGE ( 'NONE', *, *, #49636, .F. ) ;
#63581 = EDGE_CURVE ( 'NONE', #42983, #9845, #42732, .T. ) ;
#63582 = CARTESIAN_POINT ( 'NONE',  ( 2.770579946183327369, 5.784075095088785368, 5.249166435139375864 ) ) ;
#63583 = DIRECTION ( 'NONE',  ( -1.000000000000000000, -1.836970198721029688E-16, -0.000000000000000000 ) ) ;
#63584 = DIRECTION ( 'NONE',  ( 0.000000000000000000, 0.000000000000000000, 1.000000000000000000 ) ) ;
#63585 = DIRECTION ( 'NONE',  ( -1.000000000000000000, 0.000000000000000000, -0.000000000000000000 ) ) ;
#63586 = ORIENTED_EDGE ( 'NONE', *, *, #50012, .F. ) ;
#63587 = DIRECTION ( 'NONE',  ( -0.000000000000000000, -0.000000000000000000, -1.000000000000000000 ) ) ;
#63588 = AXIS2_PLACEMENT_3D ( 'NONE', #21781, #42338, #57023 ) ;
#63589 = CARTESIAN_POINT ( 'NONE',  ( 17.02556425888772296, -28.50707051634331890, 9.313930266526256219 ) ) ;
#63590 = DIRECTION ( 'NONE',  ( -0.000000000000000000, -1.000000000000000000, -0.000000000000000000 ) ) ;
#63592 = ORIENTED_EDGE ( 'NONE', *, *, #16660, .T. ) ;
#63591 = CARTESIAN_POINT ( 'NONE',  ( -35.00000000000000000, 0.000000000000000000, 0.000000000000000000 ) ) ;
#63593 = EDGE_CURVE ( 'NONE', #55770, #36445, #48087, .T. ) ;
#63594 = CYLINDRICAL_SURFACE ( 'NONE', #49032, 6.615568257478080305 ) ;
#63595 = ORIENTED_EDGE ( 'NONE', *, *, #57973, .F. ) ;
#63596 = CARTESIAN_POINT ( 'NONE',  ( 0.2801149460245161982, -6.294737133725727851, -10.51028947658250345 ) ) ;
#63597 = EDGE_LOOP ( 'NONE', ( #36992, #2477, #7145, #24352 ) ) ;
#63598 = CYLINDRICAL_SURFACE ( 'NONE', #27358, 7.499999999999988454 ) ;
#63600 = CARTESIAN_POINT ( 'NONE',  ( 0.2958664285830434615, 3.984029505266722726, -11.59077733151251621 ) ) ;
#63599 = AXIS2_PLACEMENT_3D ( 'NONE', #25774, #51048, #57682 ) ;
#63601 = AXIS2_PLACEMENT_3D ( 'NONE', #1303, #5975, #21228 ) ;
#63602 = DIRECTION ( 'NONE',  ( -1.000000000000000000, -0.000000000000000000, -0.000000000000000000 ) ) ;
#63603 = CARTESIAN_POINT ( 'NONE',  ( 0.3109076770649074062, -3.971171685427473452, 11.60048803586498245 ) ) ;
#63604 = CARTESIAN_POINT ( 'NONE',  ( 0.3474126878361875059, 9.566300984424410458, 7.689340002166765053 ) ) ;
#63605 = CARTESIAN_POINT ( 'NONE',  ( -37.00000000000000711, 0.000000000000000000, 0.000000000000000000 ) ) ;
#63606 = DIRECTION ( 'NONE',  ( -1.000000000000000000, 0.000000000000000000, 0.000000000000000000 ) ) ;
#63607 = CIRCLE ( 'NONE', #36015, 2.899999999999995026 ) ;
#63608 = ORIENTED_EDGE ( 'NONE', *, *, #48461, .F. ) ;
#63609 = LINE ( 'NONE', #34348, #48640 ) ;
#63610 = ORIENTED_EDGE ( 'NONE', *, *, #28431, .T. ) ;
#63611 = VERTEX_POINT ( 'NONE', #30690 ) ;
#63612 = LINE ( 'NONE', #38353, #47660 ) ;
#63613 = CARTESIAN_POINT ( 'NONE',  ( -22.30527770659433173, 3.381761229713386552, 1.656864125491224193 ) ) ;
#63614 = CIRCLE ( 'NONE', #34930, 12.75000000000000178 ) ;
#63615 = DIRECTION ( 'NONE',  ( 0.000000000000000000, 0.000000000000000000, 1.000000000000000000 ) ) ;
#63616 = CARTESIAN_POINT ( 'NONE',  ( -22.28023996335807411, 2.118259050016095379, 3.022323476748264515 ) ) ;
#63617 = DIRECTION ( 'NONE',  ( -0.000000000000000000, -0.000000000000000000, -1.000000000000000000 ) ) ;
#63618 = EDGE_CURVE ( 'NONE', #5644, #21398, #52325, .T. ) ;
#63619 = CARTESIAN_POINT ( 'NONE',  ( 0.000000000000000000, -30.50000000000000000, 0.000000000000000000 ) ) ;
#63620 = EDGE_CURVE ( 'NONE', #20463, #10376, #5460, .T. ) ;
#63621 = VERTEX_POINT ( 'NONE', #28663 ) ;
#63622 = CARTESIAN_POINT ( 'NONE',  ( 37.00000000000000711, 2.968224442958566911, 11.81949347079743440 ) ) ;
#63623 = CARTESIAN_POINT ( 'NONE',  ( 2.284126774967663920, -5.756079777200378444, -5.036818232552951358 ) ) ;
#63624 = DIRECTION ( 'NONE',  ( -1.000000000000000000, -0.000000000000000000, -0.000000000000000000 ) ) ;
#63625 = EDGE_CURVE ( 'NONE', #14997, #21918, #37586, .T. ) ;
#63626 = CARTESIAN_POINT ( 'NONE',  ( 2.241352910868908754, -4.843133558968167662, 5.901537464758438212 ) ) ;
#63627 = CARTESIAN_POINT ( 'NONE',  ( 2.000000000000001776, -3.786546189469212731, 5.663561025469122434 ) ) ;
#63628 = AXIS2_PLACEMENT_3D ( 'NONE', #34451, #54753, #9487 ) ;
#63629 = CIRCLE ( 'NONE', #47706, 4.999999999999999112 ) ;
#63630 = CARTESIAN_POINT ( 'NONE',  ( -11.36165340985849426, -6.759379395737725282, 11.68799443367750612 ) ) ;
#63631 = CARTESIAN_POINT ( 'NONE',  ( -10.89441910033722571, -7.164245653068409325, 11.44400242214513241 ) ) ;
#63632 = EDGE_CURVE ( 'NONE', #37233, #11603, #22713, .T. ) ;
#63634 = VERTEX_POINT ( 'NONE', #43292 ) ;
#63633 = EDGE_CURVE ( 'NONE', #41254, #4226, #12057, .T. ) ;
#63635 = CYLINDRICAL_SURFACE ( 'NONE', #43614, 12.74999999999999822 ) ;
#63636 = CARTESIAN_POINT ( 'NONE',  ( 35.00000000000000000, 8.052525312709883920, -8.551552972817113130 ) ) ;
#63637 = EDGE_CURVE ( 'NONE', #6620, #45368, #62928, .T. ) ;
#63638 = AXIS2_PLACEMENT_3D ( 'NONE', #18311, #48261, #13615 ) ;
#63639 = CARTESIAN_POINT ( 'NONE',  ( -10.00000000000000178, 0.000000000000000000, 0.000000000000000000 ) ) ;
#63640 = DIRECTION ( 'NONE',  ( 0.000000000000000000, -0.01356324068817992175, 0.9999080150203990547 ) ) ;
#63641 = VECTOR ( 'NONE', #43539, 1000.000000000000000 ) ;
#63642 = ORIENTED_EDGE ( 'NONE', *, *, #21484, .T. ) ;
#63643 = CARTESIAN_POINT ( 'NONE',  ( -37.00000000000000711, -9.621072037177057723, 8.366449238204328509 ) ) ;
#63644 = DIRECTION ( 'NONE',  ( -1.000000000000000000, 0.000000000000000000, 0.000000000000000000 ) ) ;
#63645 = DIRECTION ( 'NONE',  ( 0.000000000000000000, -0.01356324068817998940, 0.9999080150203990547 ) ) ;
#63646 = EDGE_LOOP ( 'NONE', ( #49245, #50232, #8044, #14100 ) ) ;
#63647 = DIRECTION ( 'NONE',  ( 0.000000000000000000, 0.000000000000000000, 1.000000000000000000 ) ) ;
#63648 = DIRECTION ( 'NONE',  ( 0.000000000000000000, -0.01356324068817998593, 0.9999080150203990547 ) ) ;
#63649 = ORIENTED_EDGE ( 'NONE', *, *, #8449, .F. ) ;
#63650 = ORIENTED_EDGE ( 'NONE', *, *, #65600, .F. ) ;
#63651 = DIRECTION ( 'NONE',  ( 0.000000000000000000, 0.01356324068817998940, -0.9999080150203990547 ) ) ;
#63652 = EDGE_CURVE ( 'NONE', #55219, #42057, #23260, .T. ) ;
#63653 = B_SPLINE_CURVE_WITH_KNOTS ( 'NONE', 3,
 ( #23294, #12637, #13625, #8325, #32916, #53888, #17979, #42913, #22977, #38239, #33601, #3363, #7677, #27961, #58561, #48909, #42561, #53231, #23631, #2717, #28599, #48270 ),
 .UNSPECIFIED., .F., .F.,
 ( 4, 3, 3, 3, 3, 3, 3, 4 ),
 ( 0.000000000000000000, 4.447697177976545497E-05, 6.624143997791643668E-05, 8.800576886944832850E-05, 0.0001097699864780960676, 0.0001315341395364451067, 0.0001760120188223387831, 0.0001867971373174843357 ),
 .UNSPECIFIED. ) ;
#63654 = ORIENTED_EDGE ( 'NONE', *, *, #41966, .T. ) ;
#63655 = EDGE_CURVE ( 'NONE', #4485, #451, #2436, .T. ) ;
#63656 = CARTESIAN_POINT ( 'NONE',  ( 0.000000000000000000, 7.414200355365271555, -1.131208685655096691 ) ) ;
#63657 = DIRECTION ( 'NONE',  ( 1.000000000000000000, 0.000000000000000000, -0.000000000000000000 ) ) ;
#63659 = DIRECTION ( 'NONE',  ( 0.000000000000000000, -0.4380125133594039433, 0.8989688749565125647 ) ) ;
#63658 = SHAPE_REPRESENTATION ( 'BR-837', ( #20731, #9047, #43029, #14354, #23973, #39852, #37723 ), #12225 ) ;
#63660 = DIRECTION ( 'NONE',  ( -1.000000000000000000, 0.000000000000000000, 0.000000000000000000 ) ) ;
#63661 = CYLINDRICAL_SURFACE ( 'NONE', #2385, 12.18650000000000055 ) ;
#63662 = CYLINDRICAL_SURFACE ( 'NONE', #45099, 2.899999999999994582 ) ;
#63664 = ORIENTED_EDGE ( 'NONE', *, *, #54758, .F. ) ;
#63663 = DIRECTION ( 'NONE',  ( 0.000000000000000000, 0.01356324068817991828, -0.9999080150203990547 ) ) ;
#63665 = DIRECTION ( 'NONE',  ( 1.000000000000000000, 0.000000000000000000, -0.000000000000000000 ) ) ;
#63666 = EDGE_LOOP ( 'NONE', ( #1231, #19129, #41520, #7251 ) ) ;
#63667 = LINE ( 'NONE', #44371, #17922 ) ;
#63668 = VERTEX_POINT ( 'NONE', #2777 ) ;
#63669 = ORIENTED_EDGE ( 'NONE', *, *, #17856, .F. ) ;
#63670 = CARTESIAN_POINT ( 'NONE',  ( -17.65983200964312516, 7.462298296871543002, 11.25245064142463747 ) ) ;
#63671 = B_SPLINE_CURVE_WITH_KNOTS ( 'NONE', 3,
 ( #35829, #41484, #41831, #6923, #20579, #47172, #61137, #21890, #56132, #25897 ),
 .UNSPECIFIED., .F., .F.,
 ( 4, 3, 3, 4 ),
 ( 4.336808689942017736E-19, 6.607638129004537672E-05, 9.911389841680465337E-05, 0.0001667630577588625010 ),
 .UNSPECIFIED. ) ;
#63672 = CARTESIAN_POINT ( 'NONE',  ( -2.112161198359963521, -26.60281475960710296, 16.15113466974340639 ) ) ;
#63673 = CARTESIAN_POINT ( 'NONE',  ( -24.67543046828737729, 11.54621877779729289, 6.997874691641950307 ) ) ;
#63674 = VECTOR ( 'NONE', #24457, 1000.000000000000000 ) ;
#63675 = CARTESIAN_POINT ( 'NONE',  ( 22.85860294180936947, -4.209476205790071646, 11.23990550851312342 ) ) ;
#63676 = EDGE_CURVE ( 'NONE', #54376, #44474, #54449, .T. ) ;
#63677 = DIRECTION ( 'NONE',  ( 1.000000000000000000, 0.000000000000000000, 0.000000000000000000 ) ) ;
#63678 = LINE ( 'NONE', #57751, #38399 ) ;
#63679 = ORIENTED_EDGE ( 'NONE', *, *, #34370, .T. ) ;
#63680 = CARTESIAN_POINT ( 'NONE',  ( -22.27706485742869091, 0.3729136217356220917, 3.662257305743802149 ) ) ;
#63681 =( BOUNDED_SURFACE ( )  B_SPLINE_SURFACE ( 3, 1, ( 
 ( #8515, #58771 ),
 ( #14153, #29766 ),
 ( #19153, #24807 ),
 ( #33477, #8855 ) ),
 .UNSPECIFIED., .F., .F., .F. ) 
 B_SPLINE_SURFACE_WITH_KNOTS ( ( 4, 4 ),
 ( 2, 2 ),
 ( 0.000000000000000000, 1.000000000000000000 ),
 ( 0.000000000000000000, 1.000000000000000000 ),
 .UNSPECIFIED. ) 
 GEOMETRIC_REPRESENTATION_ITEM ( )  RATIONAL_B_SPLINE_SURFACE ( (
 ( 1.000000000000000000, 1.000000000000000000),
 ( 0.6933888150995267674, 0.9895912004443193632),
 ( 0.6933888150995267674, 0.9895912004443193632),
 ( 1.000000000000000000, 1.000000000000000000) ) ) 
 REPRESENTATION_ITEM ( '' )  SURFACE ( )  );
#63682 = CIRCLE ( 'NONE', #16949, 12.74999999999999822 ) ;
#63683 = CARTESIAN_POINT ( 'NONE',  ( 2.297017764050092836, 5.755222757172114179, -5.044319338147307263 ) ) ;
#63684 = FACE_OUTER_BOUND ( 'NONE', #16153, .T. ) ;
#63685 = ORIENTED_EDGE ( 'NONE', *, *, #40531, .T. ) ;
#63686 = DIRECTION ( 'NONE',  ( -0.3865475372811021937, 0.7888450329201810440, -0.4778122177791956915 ) ) ;
#63687 = VERTEX_POINT ( 'NONE', #58628 ) ;
#63688 = CARTESIAN_POINT ( 'NONE',  ( 37.00000000000000711, 4.400442035670943497, -11.96656215839370851 ) ) ;
#63689 = CARTESIAN_POINT ( 'NONE',  ( -10.71060692978931783, -9.068875453414413812, 7.876602834927732388 ) ) ;
#63690 = FACE_OUTER_BOUND ( 'NONE', #28358, .T. ) ;
#63692 = CIRCLE ( 'NONE', #35005, 5.000000000000000000 ) ;
#63691 = CARTESIAN_POINT ( 'NONE',  ( 2.000000000000001776, 2.315790869867166091, -7.133520354428107169 ) ) ;
#63693 = DIRECTION ( 'NONE',  ( 0.000000000000000000, 0.9796553971857735466, 0.2006870767258926436 ) ) ;
#63694 = CARTESIAN_POINT ( 'NONE',  ( -27.08871896697731785, -1.896680818246860412, 1.309412067287320847 ) ) ;
#63695 = CARTESIAN_POINT ( 'NONE',  ( 2.247206125382829711, 3.917979829727999075, -6.554642244888417402 ) ) ;
#63696 = VECTOR ( 'NONE', #26793, 1000.000000000000000 ) ;
#63697 = ADVANCED_FACE ( 'NONE', ( #43969 ), #23354, .T. ) ;
#63698 = VERTEX_POINT ( 'NONE', #48637 ) ;
#63699 = DIRECTION ( 'NONE',  ( 1.000000000000000000, -0.000000000000000000, 0.000000000000000000 ) ) ;
#63700 = ORIENTED_EDGE ( 'NONE', *, *, #25341, .T. ) ;
#63701 = CARTESIAN_POINT ( 'NONE',  ( 1.719304012338833676, 3.626341562670448493, 12.20344780066006152 ) ) ;
#63702 = LINE ( 'NONE', #64045, #63674 ) ;
#63703 = CIRCLE ( 'NONE', #61578, 3.999999999999999112 ) ;
#63704 = CARTESIAN_POINT ( 'NONE',  ( -35.00000000000000000, -11.72195762423409349, -0.7536123767499773862 ) ) ;
#63705 = VERTEX_POINT ( 'NONE', #3092 ) ;
#63706 = EDGE_CURVE ( 'NONE', #36273, #46695, #18387, .T. ) ;
#63707 = CARTESIAN_POINT ( 'NONE',  ( 35.00000000000000000, 4.603882218679549609, -10.80631716521668828 ) ) ;
#63708 = ORIENTED_EDGE ( 'NONE', *, *, #39280, .F. ) ;
#63709 = CARTESIAN_POINT ( 'NONE',  ( 0.3164563675027635137, 7.696930404785163660, -9.546944054903010013 ) ) ;
#63710 = CARTESIAN_POINT ( 'NONE',  ( 5.515539859299206427, -0.001886660928063817059, 0.005751553894235436962 ) ) ;
#63711 = DIRECTION ( 'NONE',  ( 0.000000000000000000, 0.8989688749565143411, 0.4380125133594006681 ) ) ;
#63712 = DIRECTION ( 'NONE',  ( 0.000000000000000000, -0.01356324068817998940, 0.9999080150203990547 ) ) ;
#63713 = EDGE_CURVE ( 'NONE', #27787, #22102, #22419, .T. ) ;
#63714 = ORIENTED_EDGE ( 'NONE', *, *, #43234, .T. ) ;
#63715 = CARTESIAN_POINT ( 'NONE',  ( -47.00000000000000711, 0.000000000000000000, 0.000000000000000000 ) ) ;
#63716 = CARTESIAN_POINT ( 'NONE',  ( -22.28546858134833641, -2.587024666338645584, 2.654201075783120700 ) ) ;
#63717 = CARTESIAN_POINT ( 'NONE',  ( 2.653899356900444761, -1.091629880170381428, 7.694895988366584838 ) ) ;
#63718 = CARTESIAN_POINT ( 'NONE',  ( -29.10325845542003975, -3.352553978523134415, -24.67444324980779413 ) ) ;
#63719 = EDGE_CURVE ( 'NONE', #7910, #44848, #39290, .T. ) ;
#63720 = VECTOR ( 'NONE', #41571, 1000.000000000000000 ) ;
#63721 = PRESENTATION_LAYER_ASSIGNMENT (  '', '', ( #18093 ) ) ;
#63722 = CARTESIAN_POINT ( 'NONE',  ( 0.000000000000000000, -5.585096664091960150, 4.113602740025890547 ) ) ;
#63723 = DIRECTION ( 'NONE',  ( -1.000000000000000000, 0.000000000000000000, 0.000000000000000000 ) ) ;
#63724 = EDGE_LOOP ( 'NONE', ( #15813, #447, #37034, #41322 ) ) ;
#63725 = CARTESIAN_POINT ( 'NONE',  ( -20.32764961709473184, -11.53253557995959788, -3.332158659635061859 ) ) ;
#63726 = CARTESIAN_POINT ( 'NONE',  ( 28.77117211474471503, 12.20468600494871403, 5.784778099440913479 ) ) ;
#63727 = CARTESIAN_POINT ( 'NONE',  ( -5.876491384319547429, -28.27454061773107696, -11.46433771796954382 ) ) ;
#63728 = VERTEX_POINT ( 'NONE', #55591 ) ;
#63729 = DIRECTION ( 'NONE',  ( 1.000000000000000000, -0.000000000000000000, -0.000000000000000000 ) ) ;
#63730 = CARTESIAN_POINT ( 'NONE',  ( 1.287602823386651441, -8.506034117234991143, 9.277923463524135883 ) ) ;
#63731 = DIRECTION ( 'NONE',  ( 1.000000000000000000, -0.000000000000000000, -0.000000000000000000 ) ) ;
#63732 = FACE_OUTER_BOUND ( 'NONE', #49425, .T. ) ;
#63733 = CARTESIAN_POINT ( 'NONE',  ( -35.00000000000000000, 6.475373545682302279, 10.32377448871670467 ) ) ;
#63734 = VECTOR ( 'NONE', #46677, 1000.000000000000000 ) ;
#63735 = EDGE_CURVE ( 'NONE', #27041, #1393, #19420, .T. ) ;
#63736 = EDGE_LOOP ( 'NONE', ( #7079, #18558, #55987, #24784 ) ) ;
#63737 = CARTESIAN_POINT ( 'NONE',  ( -37.25000000000000711, -1.694065894508600678E-18, 0.000000000000000000 ) ) ;
#63738 = ORIENTED_EDGE ( 'NONE', *, *, #46672, .T. ) ;
#63739 = AXIS2_PLACEMENT_3D ( 'NONE', #44735, #29145, #5180 ) ;
#63740 = DIRECTION ( 'NONE',  ( 1.000000000000000000, -0.000000000000000000, -0.000000000000000000 ) ) ;
#63741 = CARTESIAN_POINT ( 'NONE',  ( 0.2872850955227749803, -9.519656861923676772, -7.715220952083337913 ) ) ;
#63742 = CARTESIAN_POINT ( 'NONE',  ( 35.00000000000000000, 12.70128625845192616, -1.113475361586538481 ) ) ;
#63743 = CARTESIAN_POINT ( 'NONE',  ( 1.372161826076970792, 3.755740169579696808, -12.04315837901310893 ) ) ;
#63744 = LINE ( 'NONE', #39462, #52272 ) ;
#63745 = CARTESIAN_POINT ( 'NONE',  ( 2.241317068080787234, -1.235499051333821319, 7.533758201955880196 ) ) ;
#63746 = DIRECTION ( 'NONE',  ( 0.3939253465568943180, 0.1691689424289825050, -0.9034404741085547696 ) ) ;
#63747 = EDGE_LOOP ( 'NONE', ( #62234, #20240, #37780, #50983 ) ) ;
#63748 = ORIENTED_EDGE ( 'NONE', *, *, #22801, .F. ) ;
#63749 = PRESENTATION_STYLE_ASSIGNMENT (( #2945 ) ) ;
#63750 = ORIENTED_EDGE ( 'NONE', *, *, #28548, .T. ) ;
#63751 = CARTESIAN_POINT ( 'NONE',  ( -22.28415773361649954, 2.588610893123072021, -2.647149619609363569 ) ) ;
#63752 = EDGE_CURVE ( 'NONE', #54995, #50756, #24022, .T. ) ;
#63753 = CYLINDRICAL_SURFACE ( 'NONE', #35339, 2.809571291727933851 ) ;
#63754 = LINE ( 'NONE', #53813, #23459 ) ;
#63755 = VERTEX_POINT ( 'NONE', #59590 ) ;
#63756 = DIRECTION ( 'NONE',  ( 0.000000000000000000, 0.4380125133593975595, -0.8989688749565157844 ) ) ;
#63757 = CARTESIAN_POINT ( 'NONE',  ( 2.280717697723833037, 6.543326285614686988, -3.958470850374239181 ) ) ;
#63758 = CARTESIAN_POINT ( 'NONE',  ( -35.00000000000000000, 5.015831474386455824, -10.62137734850263016 ) ) ;
#63759 = ORIENTED_EDGE ( 'NONE', *, *, #24987, .F. ) ;
#63760 = ORIENTED_EDGE ( 'NONE', *, *, #4882, .F. ) ;
#63761 = DIRECTION ( 'NONE',  ( -1.000000000000000000, -0.000000000000000000, -0.000000000000000000 ) ) ;
#63762 = VECTOR ( 'NONE', #44774, 1000.000000000000000 ) ;
#63764 = ORIENTED_EDGE ( 'NONE', *, *, #7329, .F. ) ;
#63763 =( REPRESENTATION_RELATIONSHIP ('NONE','NONE', #63658, #29683 ) REPRESENTATION_RELATIONSHIP_WITH_TRANSFORMATION ( #21837 )SHAPE_REPRESENTATION_RELATIONSHIP( ) );
#63765 = ORIENTED_EDGE ( 'NONE', *, *, #56412, .T. ) ;
#63766 = ORIENTED_EDGE ( 'NONE', *, *, #20161, .T. ) ;
#63767 = CARTESIAN_POINT ( 'NONE',  ( 35.00000000000000000, -11.42599468261425955, 4.237620530777920003 ) ) ;
#63768 = EDGE_CURVE ( 'NONE', #48033, #3518, #17277, .T. ) ;
#63769 = CARTESIAN_POINT ( 'NONE',  ( -27.08850691366518859, -1.609738257842364462, 1.648570643966299265 ) ) ;
#63770 = VECTOR ( 'NONE', #14887, 1000.000000000000114 ) ;
#63772 = VECTOR ( 'NONE', #16216, 1000.000000000000114 ) ;
#63771 = CARTESIAN_POINT ( 'NONE',  ( -27.09483304420799143, -2.317106154747429425, 0.1669215111592681211 ) ) ;
#63773 = DIRECTION ( 'NONE',  ( -1.000000000000000000, 0.000000000000000000, -0.000000000000000000 ) ) ;
#63774 = CARTESIAN_POINT ( 'NONE',  ( 41.00000000000000711, -45.00200000000000244, -4.500000000000000888 ) ) ;
#63775 = CIRCLE ( 'NONE', #43603, 5.000000000000000888 ) ;
#63776 = CARTESIAN_POINT ( 'NONE',  ( 1.719304012338398246, 7.581471372739840398, 10.22720798541364395 ) ) ;
#63777 = EDGE_CURVE ( 'NONE', #27211, #44463, #48250, .T. ) ;
#63778 = ORIENTED_EDGE ( 'NONE', *, *, #41270, .T. ) ;
#63779 = DIRECTION ( 'NONE',  ( 1.000000000000000000, 0.000000000000000000, -0.000000000000000000 ) ) ;
#63780 = CARTESIAN_POINT ( 'NONE',  ( -22.27719443589224113, 2.737335337013115932, -2.462030382548423546 ) ) ;
#63781 = ADVANCED_FACE ( 'NONE', ( #45589 ), #18261, .F. ) ;
#63782 = DIRECTION ( 'NONE',  ( -1.000000000000000000, 0.000000000000000000, 0.000000000000000000 ) ) ;
#63783 = CARTESIAN_POINT ( 'NONE',  ( -35.00000000000000000, 0.000000000000000000, 0.000000000000000000 ) ) ;
#63784 = CARTESIAN_POINT ( 'NONE',  ( 29.66268546517093796, 8.643908359168339217, 8.338268269882382455 ) ) ;
#63785 = CARTESIAN_POINT ( 'NONE',  ( 1.287602823388156237, 0.5522659225156872909, -12.57487505104594128 ) ) ;
#63786 = CARTESIAN_POINT ( 'NONE',  ( -27.08418179957658367, 1.521007404704319388, 1.713622993062704714 ) ) ;
#63787 = DIRECTION ( 'NONE',  ( 1.000000000000000000, -0.000000000000000000, -0.000000000000000000 ) ) ;
#63788 = CARTESIAN_POINT ( 'NONE',  ( 0.4626703367443177339, 5.909149965571010021, 10.80124546303551902 ) ) ;
#63789 = CIRCLE ( 'NONE', #53224, 2.899999999999995470 ) ;
#63790 = AXIS2_PLACEMENT_3D ( 'NONE', #29076, #34378, #49385 ) ;
#63791 = ORIENTED_EDGE ( 'NONE', *, *, #49447, .F. ) ;
#63792 = EDGE_CURVE ( 'NONE', #8949, #15374, #45941, .T. ) ;
#63793 = CARTESIAN_POINT ( 'NONE',  ( 3.047904605210429274, -7.270585891216597929, -3.098478597269381130 ) ) ;
#63794 = AXIS2_PLACEMENT_3D ( 'NONE', #15136, #39761, #24458 ) ;
#63795 = ORIENTED_EDGE ( 'NONE', *, *, #40026, .T. ) ;
#63796 = CARTESIAN_POINT ( 'NONE',  ( -10.95212338237647920, -9.902220863987562183, 6.778349501228839280 ) ) ;
#63797 = CARTESIAN_POINT ( 'NONE',  ( -17.71439793346019798, -28.67846309484135858, -8.502197385450024569 ) ) ;
#63798 = CARTESIAN_POINT ( 'NONE',  ( 12.67279215479052112, -12.94353850923882909, -3.840530738146114675 ) ) ;
#63799 = AXIS2_PLACEMENT_3D ( 'NONE', #61749, #41801, #16854 ) ;
#63800 = LINE ( 'NONE', #23927, #13950 ) ;
#63801 = CARTESIAN_POINT ( 'NONE',  ( 2.242819959140645469, -6.662619100654771032, 3.728423299584962436 ) ) ;
#63802 = EDGE_CURVE ( 'NONE', #37649, #12199, #50273, .T. ) ;
#63803 = ORIENTED_EDGE ( 'NONE', *, *, #18866, .T. ) ;
#63804 = CARTESIAN_POINT ( 'NONE',  ( 0.4613984246114868348, 10.51786362586223156, -6.399144685811604560 ) ) ;
#63806 = CIRCLE ( 'NONE', #21330, 20.00000000000000000 ) ;
#63805 = CARTESIAN_POINT ( 'NONE',  ( -22.27384469013076185, 3.663183248998794106, -0.3730095848193202279 ) ) ;
#63807 = CARTESIAN_POINT ( 'NONE',  ( -27.09861164373112885, 2.097104182796081240, 1.025570525056623161 ) ) ;
#63808 = CARTESIAN_POINT ( 'NONE',  ( 9.648902782401016509, -32.13880772995998569, -13.06387094876276223 ) ) ;
#63809 = ADVANCED_FACE ( 'NONE', ( #60556 ), #14349, .F. ) ;
#63810 = CIRCLE ( 'NONE', #17115, 5.000000000000000888 ) ;
#63811 = CARTESIAN_POINT ( 'NONE',  ( 35.00000000000000000, -12.01765980939840439, 2.021542716731525413 ) ) ;
#63812 = VERTEX_POINT ( 'NONE', #20323 ) ;
#63813 = DIRECTION ( 'NONE',  ( 0.000000000000000000, -0.01356324068817991828, 0.9999080150203990547 ) ) ;
#63814 = AXIS2_PLACEMENT_3D ( 'NONE', #51747, #31119, #1199 ) ;
#63815 = CARTESIAN_POINT ( 'NONE',  ( 1.633930747252546833, -8.702439996575384029, -9.253127167384830543 ) ) ;
#63816 = CARTESIAN_POINT ( 'NONE',  ( 2.273267844204866606, -3.952852893982251814, -6.543821324256922090 ) ) ;
#63817 = VECTOR ( 'NONE', #3162, 1000.000000000000000 ) ;
#63818 = VECTOR ( 'NONE', #31428, 1000.000000000000000 ) ;
#63819 = AXIS2_PLACEMENT_3D ( 'NONE', #33960, #61434, #56465 ) ;
#63820 = ORIENTED_EDGE ( 'NONE', *, *, #44195, .T. ) ;
#63821 = ORIENTED_EDGE ( 'NONE', *, *, #6470, .T. ) ;
#63822 = CARTESIAN_POINT ( 'NONE',  ( 0.000000000000000000, 0.000000000000000000, 0.000000000000000000 ) ) ;
#63823 = EDGE_LOOP ( 'NONE', ( #61461, #57060, #13139, #64285 ) ) ;
#63824 = CARTESIAN_POINT ( 'NONE',  ( -37.00000000000000711, 6.307491713049167004, -9.908974237959577991 ) ) ;
#63825 = CARTESIAN_POINT ( 'NONE',  ( 3.152665057734104437, -3.546019893116280741, -7.102135024645891193 ) ) ;
#63826 = AXIS2_PLACEMENT_3D ( 'NONE', #1887, #17176, #57762 ) ;
#63827 = CARTESIAN_POINT ( 'NONE',  ( 26.58307969160927087, -3.634951060761374197, 23.96081192854775210 ) ) ;
#63828 = CARTESIAN_POINT ( 'NONE',  ( 0.2872850955227778114, 9.251080475901458655, -8.035297825011268102 ) ) ;
#63829 = CARTESIAN_POINT ( 'NONE',  ( -22.28023996335807411, -2.118259050016081613, -3.022323476748290716 ) ) ;
#63830 = ORIENTED_EDGE ( 'NONE', *, *, #20942, .F. ) ;
#63831 = EDGE_LOOP ( 'NONE', ( #18542, #65166, #44916, #58884 ) ) ;
#63832 = VERTEX_POINT ( 'NONE', #34623 ) ;
#63833 = CARTESIAN_POINT ( 'NONE',  ( 1.719304012338199517, 0.000000000000000000, 0.000000000000000000 ) ) ;
#63834 = CIRCLE ( 'NONE', #25595, 2.899999999999995026 ) ;
#63835 = ADVANCED_FACE ( 'NONE', ( #29631 ), #49938, .T. ) ;
#63836 = CARTESIAN_POINT ( 'NONE',  ( 2.000000000000001776, -5.888698556700742159, -3.665823448873470003 ) ) ;
#63837 = ORIENTED_EDGE ( 'NONE', *, *, #39156, .T. ) ;
#63838 = CARTESIAN_POINT ( 'NONE',  ( -35.00000000000000000, -1.039216533672986387, 11.70009620280411333 ) ) ;
#63839 = AXIS2_PLACEMENT_3D ( 'NONE', #65017, #14471, #19816 ) ;
#63840 = CARTESIAN_POINT ( 'NONE',  ( 2.241352910868908754, -7.532448145350516988, 1.243507963608069700 ) ) ;
#63841 = ORIENTED_EDGE ( 'NONE', *, *, #18854, .T. ) ;
#63842 = CARTESIAN_POINT ( 'NONE',  ( 0.000000000000000000, 0.000000000000000000, 0.000000000000000000 ) ) ;
#63843 = DIRECTION ( 'NONE',  ( -1.000000000000000000, 0.000000000000000000, 0.000000000000000000 ) ) ;
#63844 = DIRECTION ( 'NONE',  ( -1.000000000000000000, -0.000000000000000000, -0.000000000000000000 ) ) ;
#63845 = ORIENTED_EDGE ( 'NONE', *, *, #4672, .T. ) ;
#63846 = AXIS2_PLACEMENT_3D ( 'NONE', #64488, #38231, #59516 ) ;
#63847 = ORIENTED_EDGE ( 'NONE', *, *, #15516, .F. ) ;
#63848 = CARTESIAN_POINT ( 'NONE',  ( 2.177405672431364181, 3.189307221898113998, -10.73538068360681663 ) ) ;
#63849 = ORIENTED_EDGE ( 'NONE', *, *, #52887, .F. ) ;
#63850 = CARTESIAN_POINT ( 'NONE',  ( -18.49080574448724690, 11.99999999999999645, 2.510045011421233839E-15 ) ) ;
#63851 = EDGE_LOOP ( 'NONE', ( #37351, #57464, #7365, #54141 ) ) ;
#63852 = VECTOR ( 'NONE', #58083, 1000.000000000000000 ) ;
#63853 = CARTESIAN_POINT ( 'NONE',  ( 0.2653141617321017609, -4.229807441322391171, 11.49253039221381201 ) ) ;
#63854 = CARTESIAN_POINT ( 'NONE',  ( 37.00000000000000711, 4.705694406421931860E-17, -3.469127814946512892E-15 ) ) ;
#63855 = CARTESIAN_POINT ( 'NONE',  ( -18.01523681890432371, -28.74990419755712878, 8.100995087731217126 ) ) ;
#63856 = CYLINDRICAL_SURFACE ( 'NONE', #12562, 12.75000000000000178 ) ;
#63857 = ADVANCED_FACE ( 'NONE', ( #29973 ), #42895, .F. ) ;
#63858 = DIRECTION ( 'NONE',  ( 0.9207114435679737419, 0.000000000000000000, -0.3902440745007897949 ) ) ;
#63859 = DIRECTION ( 'NONE',  ( -1.000000000000000000, -0.000000000000000000, 0.000000000000000000 ) ) ;
#63860 = ORIENTED_EDGE ( 'NONE', *, *, #4596, .F. ) ;
#63861 = CARTESIAN_POINT ( 'NONE',  ( 37.25000000000000711, -27.21021009056489603, 4.499999999999997335 ) ) ;
#63862 = AXIS2_PLACEMENT_3D ( 'NONE', #61487, #46226, #667 ) ;
#63863 = ORIENTED_EDGE ( 'NONE', *, *, #60422, .F. ) ;
#63864 = CARTESIAN_POINT ( 'NONE',  ( 2.000000000000001776, -5.585096664091900642, -4.113602740025990911 ) ) ;
#63865 = ADVANCED_FACE ( 'NONE', ( #57225 ), #26960, .T. ) ;
#63866 = CARTESIAN_POINT ( 'NONE',  ( -35.00000000000000000, 0.000000000000000000, 0.000000000000000000 ) ) ;
#63867 = AXIS2_PLACEMENT_3D ( 'NONE', #59945, #9059, #44296 ) ;
#63868 = AXIS2_PLACEMENT_3D ( 'NONE', #785, #6767, #26067 ) ;
#63869 = ADVANCED_FACE ( 'NONE', ( #60900 ), #714, .T. ) ;
#63870 = ORIENTED_EDGE ( 'NONE', *, *, #13296, .F. ) ;
#63871 = DIRECTION ( 'NONE',  ( -1.000000000000000000, 0.000000000000000000, 0.000000000000000000 ) ) ;
#63872 = DIRECTION ( 'NONE',  ( 0.000000000000000000, 0.000000000000000000, -1.000000000000000000 ) ) ;
#63873 = CARTESIAN_POINT ( 'NONE',  ( 3.031336079628918156, -7.694633165537201336, 1.779751109289165356 ) ) ;
#63874 = VERTEX_POINT ( 'NONE', #1374 ) ;
#63875 = VECTOR ( 'NONE', #31210, 1000.000000000000000 ) ;
#63876 = AXIS2_PLACEMENT_3D ( 'NONE', #5325, #6313, #61826 ) ;
#63877 = AXIS2_PLACEMENT_3D ( 'NONE', #39699, #64621, #30045 ) ;
#63878 = VERTEX_POINT ( 'NONE', #11653 ) ;
#63879 = EDGE_CURVE ( 'NONE', #58896, #46955, #31294, .T. ) ;
#63880 = DIRECTION ( 'NONE',  ( -0.8758382566188793739, 0.4826047536471247956, 0.000000000000000000 ) ) ;
#63881 =( BOUNDED_SURFACE ( )  B_SPLINE_SURFACE ( 3, 1, ( 
 ( #25889, #30214 ),
 ( #65756, #10913 ),
 ( #15560, #61129 ),
 ( #38964, #28991 ) ),
 .UNSPECIFIED., .F., .F., .F. ) 
 B_SPLINE_SURFACE_WITH_KNOTS ( ( 4, 4 ),
 ( 2, 2 ),
 ( 0.000000000000000000, 1.000000000000000000 ),
 ( 0.000000000000000000, 1.000000000000000000 ),
 .UNSPECIFIED. ) 
 GEOMETRIC_REPRESENTATION_ITEM ( )  RATIONAL_B_SPLINE_SURFACE ( (
 ( 1.000000000000000000, 1.000000000000000000),
 ( 0.6933888150995267674, 0.9895912004443193632),
 ( 0.6933888150995267674, 0.9895912004443193632),
 ( 1.000000000000000000, 1.000000000000000000) ) ) 
 REPRESENTATION_ITEM ( '' )  SURFACE ( )  );
#63882 = ORIENTED_EDGE ( 'NONE', *, *, #10552, .F. ) ;
#63883 = EDGE_CURVE ( 'NONE', #33520, #17827, #55766, .T. ) ;
#63884 = DIRECTION ( 'NONE',  ( 0.000000000000000000, -0.9551603052523448545, 0.2960891610144612551 ) ) ;
#63885 = DIRECTION ( 'NONE',  ( 1.000000000000000000, 0.000000000000000000, 0.000000000000000000 ) ) ;
#63886 = CARTESIAN_POINT ( 'NONE',  ( -27.08418179957658367, 2.174042548349535586, 0.7235373421492506951 ) ) ;
#63887 = CARTESIAN_POINT ( 'NONE',  ( 0.2676618633000459879, -9.277614237849222789, -7.994628339664919814 ) ) ;
#63888 = CARTESIAN_POINT ( 'NONE',  ( -35.00000000000000000, 3.213188559034398040, -11.29812557209473667 ) ) ;
#63889 = ORIENTED_EDGE ( 'NONE', *, *, #23067, .T. ) ;
#63890 = B_SPLINE_CURVE_WITH_KNOTS ( 'NONE', 3,
 ( #43518, #23594, #13908, #39187, #64771, #53540 ),
 .UNSPECIFIED., .F., .F.,
 ( 4, 2, 4 ),
 ( 9.965227682168975268E-18, 0.001456900940518678468, 0.002913801881037346962 ),
 .UNSPECIFIED. ) ;
#63891 = CARTESIAN_POINT ( 'NONE',  ( 0.000000000000000000, -6.906413915731167918, -0.6453518998148343178 ) ) ;
#63892 = ADVANCED_FACE ( 'NONE', ( #52577 ), #62851, .T. ) ;
#63893 = CIRCLE ( 'NONE', #53275, 5.000000000000000000 ) ;
#63894 = CIRCLE ( 'NONE', #29905, 12.74999999999999822 ) ;
#63896 = EDGE_CURVE ( 'NONE', #37836, #58571, #42218, .T. ) ;
#63895 = CIRCLE ( 'NONE', #28820, 5.000000000000000000 ) ;
#63897 = CARTESIAN_POINT ( 'NONE',  ( 10.75388052849567799, -27.84561629232752011, -14.03224735226135245 ) ) ;
#63898 = AXIS2_PLACEMENT_3D ( 'NONE', #65625, #55687, #10125 ) ;
#63899 = EDGE_CURVE ( 'NONE', #7557, #48895, #52880, .T. ) ;
#63900 = CARTESIAN_POINT ( 'NONE',  ( -28.71071236259717807, 3.670376459565063421, 11.42521152978763155 ) ) ;
#63901 = FACE_OUTER_BOUND ( 'NONE', #11658, .T. ) ;
#63902 = CARTESIAN_POINT ( 'NONE',  ( 0.2651627682582937129, 7.938957913267755018, 9.324228491541544983 ) ) ;
#63903 = CARTESIAN_POINT ( 'NONE',  ( 7.265852764334843172, -6.972182010717725476, -9.777817421782533103 ) ) ;
#63904 = DIRECTION ( 'NONE',  ( 0.000000000000000000, 0.000000000000000000, 1.000000000000000000 ) ) ;
#63905 = AXIS2_PLACEMENT_3D ( 'NONE', #57344, #32693, #38024 ) ;
#63906 = ORIENTED_EDGE ( 'NONE', *, *, #52381, .T. ) ;
#63907 = CARTESIAN_POINT ( 'NONE',  ( 12.48116093077668154, -11.51604155625666515, -3.378324846013889715 ) ) ;
#63908 = ORIENTED_EDGE ( 'NONE', *, *, #10282, .T. ) ;
#63909 = CARTESIAN_POINT ( 'NONE',  ( 0.2958664285830440721, 1.910785783655738035, -12.10650684287251977 ) ) ;
#63910 = DIRECTION ( 'NONE',  ( 0.000000000000000000, 0.000000000000000000, 1.000000000000000000 ) ) ;
#63911 = CARTESIAN_POINT ( 'NONE',  ( 12.10998784662220729, 25.00000000000000000, -8.526922110106905706 ) ) ;
#63912 = VERTEX_POINT ( 'NONE', #37593 ) ;
#63913 = CARTESIAN_POINT ( 'NONE',  ( -27.30970368864377207, 11.82098433594889109, -2.066507538000780464 ) ) ;
#63914 = CARTESIAN_POINT ( 'NONE',  ( 2.241537034860906719, 4.910958050585514378, -5.845308934728727479 ) ) ;
#63915 = ORIENTED_EDGE ( 'NONE', *, *, #16447, .F. ) ;
#63916 = CIRCLE ( 'NONE', #16173, 12.18649999999999878 ) ;
#63917 = ORIENTED_EDGE ( 'NONE', *, *, #14260, .F. ) ;
#63918 = ORIENTED_EDGE ( 'NONE', *, *, #54236, .T. ) ;
#63919 = CARTESIAN_POINT ( 'NONE',  ( 29.70647529080776650, -10.34008595192405977, 8.691137256207259298 ) ) ;
#63921 = EDGE_CURVE ( 'NONE', #9046, #25109, #42547, .T. ) ;
#63920 = CARTESIAN_POINT ( 'NONE',  ( 2.256373768223413290, -7.132139410180986516, 2.737361830682297104 ) ) ;
#63922 = AXIS2_PLACEMENT_3D ( 'NONE', #56089, #30491, #10528 ) ;
#63923 = ADVANCED_FACE ( 'NONE', ( #32573 ), #16973, .T. ) ;
#63924 = B_SPLINE_CURVE_WITH_KNOTS ( 'NONE', 3,
 ( #36756, #545, #57052, #35440, #20810, #55741, #41078, #15798, #10171, #36076, #26447, #61053, #30451, #25465, #10828, #31113, #15483, #35749, #51428, #5876, #26132, #854 ),
 .UNSPECIFIED., .F., .F.,
 ( 4, 2, 2, 2, 2, 2, 2, 2, 2, 2, 4 ),
 ( 0.000000000000000000, 0.0009985635585561321737, 0.001497845337834194032, 0.001997127117112255674, 0.002496408896390317749, 0.002995690675668379391, 0.003994254234224500939, 0.004992817792780622488, 0.005991381351336744036, 0.006989944909892865585, 0.007988508468448986266 ),
 .UNSPECIFIED. ) ;
#63925 = AXIS2_PLACEMENT_3D ( 'NONE', #3830, #48056, #32716 ) ;
#63926 = VERTEX_POINT ( 'NONE', #27946 ) ;
#63927 = CARTESIAN_POINT ( 'NONE',  ( -22.27706485742869091, -2.580541389029911148, -2.625261754997698205 ) ) ;
#63928 = CARTESIAN_POINT ( 'NONE',  ( 1.937341776064131160, 1.073324468469882165, 13.46190213546479875 ) ) ;
#63929 = CARTESIAN_POINT ( 'NONE',  ( 19.67311005600952711, -0.7004819783312107306, 25.00000000000000000 ) ) ;
#63930 = DIRECTION ( 'NONE',  ( 0.000000000000000000, 0.01356324068817998940, -0.9999080150203990547 ) ) ;
#63931 = ORIENTED_EDGE ( 'NONE', *, *, #13597, .F. ) ;
#63932 = CARTESIAN_POINT ( 'NONE',  ( -37.00000000000000711, 0.000000000000000000, 0.000000000000000000 ) ) ;
#63933 = CARTESIAN_POINT ( 'NONE',  ( 17.33919137821584044, -28.58640580301184286, 8.960163943132222641 ) ) ;
#63934 = CARTESIAN_POINT ( 'NONE',  ( -29.51989888335948820, -3.283075202658972902, -11.54828650488808250 ) ) ;
#63936 = EDGE_LOOP ( 'NONE', ( #50614, #6439, #25590, #39921 ) ) ;
#63935 = CARTESIAN_POINT ( 'NONE',  ( 37.00000000000000711, 4.705694406421931860E-17, -3.469127814946512892E-15 ) ) ;
#63937 = CARTESIAN_POINT ( 'NONE',  ( 0.3040950598368152291, 3.956873563689688567, -11.60568999039890770 ) ) ;
#63938 = ORIENTED_EDGE ( 'NONE', *, *, #23683, .T. ) ;
#63939 = CARTESIAN_POINT ( 'NONE',  ( 0.000000000000000000, -4.409940824963459960, 5.354199675985231721 ) ) ;
#63940 = EDGE_CURVE ( 'NONE', #4569, #2269, #63493, .T. ) ;
#63941 = ORIENTED_EDGE ( 'NONE', *, *, #19697, .T. ) ;
#63942 = CARTESIAN_POINT ( 'NONE',  ( 2.350038591458107007, 3.024612895785500744, 10.18214835919902050 ) ) ;
#63943 = AXIS2_PLACEMENT_3D ( 'NONE', #39985, #55279, #13406 ) ;
#63944 = CARTESIAN_POINT ( 'NONE',  ( -35.04834644901396956, 0.01046409687784605365, 0.009049049589488470172 ) ) ;
#63945 = CARTESIAN_POINT ( 'NONE',  ( 0.9232058338315048962, 8.301689855530291595, -9.306586124266512883 ) ) ;
#63946 = CARTESIAN_POINT ( 'NONE',  ( 35.00000000000000000, -5.636262487437393887, -10.80478261802180207 ) ) ;
#63947 = VECTOR ( 'NONE', #30613, 1000.000000000000000 ) ;
#63948 = CARTESIAN_POINT ( 'NONE',  ( 0.2650492594609241692, -11.54478160586240065, 4.084774262246043008 ) ) ;
#63949 = EDGE_CURVE ( 'NONE', #1369, #58016, #16053, .T. ) ;
#63950 = DIRECTION ( 'NONE',  ( 0.000000000000000000, 0.000000000000000000, 1.000000000000000000 ) ) ;
#63951 = CARTESIAN_POINT ( 'NONE',  ( -22.28546858134833286, -3.592117891549503117, -0.9133285433746950455 ) ) ;
#63952 = EDGE_LOOP ( 'NONE', ( #688, #37535, #63514, #225 ) ) ;
#63953 = ORIENTED_EDGE ( 'NONE', *, *, #3945, .T. ) ;
#63954 = AXIS2_PLACEMENT_3D ( 'NONE', #65551, #54939, #25332 ) ;
#63955 = EDGE_CURVE ( 'NONE', #57557, #60039, #34299, .T. ) ;
#63956 = ORIENTED_EDGE ( 'NONE', *, *, #23246, .T. ) ;
#63957 = LINE ( 'NONE', #18434, #30652 ) ;
#63958 = CARTESIAN_POINT ( 'NONE',  ( 0.3040950598368152291, 12.11647736519421059, 1.881452845810416719 ) ) ;
#63959 = CARTESIAN_POINT ( 'NONE',  ( 35.00000000000000000, 4.705694406421931860E-17, -3.469127814946512892E-15 ) ) ;
#63960 = CARTESIAN_POINT ( 'NONE',  ( 0.2648978790185619880, -10.53870023327867855, 6.237101853238509186 ) ) ;
#63961 = CARTESIAN_POINT ( 'NONE',  ( 1.452237505248555660, -11.24427360515637986, -5.807998527926010013 ) ) ;
#63962 = CARTESIAN_POINT ( 'NONE',  ( -47.00000000000000711, 0.000000000000000000, 0.000000000000000000 ) ) ;
#63963 = CARTESIAN_POINT ( 'NONE',  ( 1.194176325881338263, -11.12159247766668990, -5.827386336992995908 ) ) ;
#63964 = ORIENTED_EDGE ( 'NONE', *, *, #43146, .F. ) ;
#63965 = EDGE_CURVE ( 'NONE', #11657, #41367, #43544, .T. ) ;
#63966 = CARTESIAN_POINT ( 'NONE',  ( -27.08429572838383947, -0.6096735944848084010, 2.208905845566022208 ) ) ;
#63967 = LINE ( 'NONE', #34029, #65329 ) ;
#63968 = B_SPLINE_CURVE_WITH_KNOTS ( 'NONE', 3,
 ( #42579, #41619, #36638, #62881 ),
 .UNSPECIFIED., .F., .F.,
 ( 4, 4 ),
 ( 0.000000000000000000, 0.002391677032556851785 ),
 .UNSPECIFIED. ) ;
#63969 = CARTESIAN_POINT ( 'NONE',  ( 1.719304012338199517, 0.000000000000000000, 0.000000000000000000 ) ) ;
#63970 = EDGE_CURVE ( 'NONE', #20003, #60501, #42900, .T. ) ;
#63971 = VECTOR ( 'NONE', #44219, 1000.000000000000000 ) ;
#63972 = ADVANCED_FACE ( 'NONE', ( #58204 ), #12625, .T. ) ;
#63973 = AXIS2_PLACEMENT_3D ( 'NONE', #53272, #58259, #57619 ) ;
#63974 = CARTESIAN_POINT ( 'NONE',  ( 2.000000000000001776, -1.693411908627248774, 7.306323022404580314 ) ) ;
#63975 = DIRECTION ( 'NONE',  ( -1.000000000000000000, 0.000000000000000000, 0.000000000000000000 ) ) ;
#63976 = AXIS2_PLACEMENT_3D ( 'NONE', #5257, #29849, #14546 ) ;
#63977 = EDGE_CURVE ( 'NONE', #48647, #60647, #64482, .T. ) ;
#63978 = CARTESIAN_POINT ( 'NONE',  ( -7.757791118878088810, -1.606844526199946221, 13.40434846090924204 ) ) ;
#63979 = EDGE_CURVE ( 'NONE', #35317, #54327, #33258, .T. ) ;
#63980 = CARTESIAN_POINT ( 'NONE',  ( -9.921280308801140535, -4.188103626763136411, 12.83514249654943207 ) ) ;
#63981 = VERTEX_POINT ( 'NONE', #8971 ) ;
#63982 = CARTESIAN_POINT ( 'NONE',  ( 0.2652384770603647413, 2.191555293694135376, -12.04846497255940818 ) ) ;
#63983 = CARTESIAN_POINT ( 'NONE',  ( 2.000000000000001776, 1.018311147294167274, 6.861346417234447159 ) ) ;
#63984 = DIRECTION ( 'NONE',  ( 0.000000000000000000, 0.6269146997507930585, 0.7790879021242551605 ) ) ;
#63985 = AXIS2_PLACEMENT_3D ( 'NONE', #64481, #18948, #38224 ) ;
#63986 = DIRECTION ( 'NONE',  ( -1.000000000000000000, 0.000000000000000000, 0.000000000000000000 ) ) ;
#63987 = CYLINDRICAL_SURFACE ( 'NONE', #20254, 12.18649999999999878 ) ;
#63988 = AXIS2_PLACEMENT_3D ( 'NONE', #41263, #46593, #56236 ) ;
#63989 = VERTEX_POINT ( 'NONE', #54539 ) ;
#63990 = DIRECTION ( 'NONE',  ( 0.000000000000000000, 0.9987865678893279586, -0.04924826701374244303 ) ) ;
#63991 = CARTESIAN_POINT ( 'NONE',  ( -8.966652592027504198, -7.722572881235366005, -9.193810145090301589 ) ) ;
#63992 = CIRCLE ( 'NONE', #55508, 12.18649999999999878 ) ;
#63993 = PLANE ( 'NONE',  #19060 ) ;
#63994 = ORIENTED_EDGE ( 'NONE', *, *, #27405, .F. ) ;
#63995 = CARTESIAN_POINT ( 'NONE',  ( 0.2801149460245124789, 2.320387321174167017, 12.02936836014264088 ) ) ;
#63996 = CARTESIAN_POINT ( 'NONE',  ( -27.28563798457903644, -1.483130241384912784, 2.487904455214888344 ) ) ;
#63997 = VERTEX_POINT ( 'NONE', #64798 ) ;
#63998 = VERTEX_POINT ( 'NONE', #14905 ) ;
#63999 = DIRECTION ( 'NONE',  ( -1.000000000000000000, 0.000000000000000000, -0.000000000000000000 ) ) ;
#64000 = EDGE_CURVE ( 'NONE', #17645, #11684, #24587, .T. ) ;
#64001 = ORIENTED_EDGE ( 'NONE', *, *, #59646, .T. ) ;
#64002 = CARTESIAN_POINT ( 'NONE',  ( 0.7446945582518622597, -12.15064199164609526, -2.504154979876258569 ) ) ;
#64003 = ADVANCED_FACE ( 'NONE', ( #23951 ), #29253, .T. ) ;
#64004 = CARTESIAN_POINT ( 'NONE',  ( -21.04919400413958996, -12.98042452237757161, -3.710884547572582459 ) ) ;
#64005 = FACE_OUTER_BOUND ( 'NONE', #46057, .T. ) ;
#64006 = DIRECTION ( 'NONE',  ( -1.000000000000000000, 0.000000000000000000, 0.000000000000000000 ) ) ;
#64007 = CARTESIAN_POINT ( 'NONE',  ( 5.536195898058073439, 0.004027525919832952543, -0.007485416011288117955 ) ) ;
#64009 = ORIENTED_EDGE ( 'NONE', *, *, #61930, .F. ) ;
#64008 = FACE_OUTER_BOUND ( 'NONE', #9676, .T. ) ;
#64010 = CARTESIAN_POINT ( 'NONE',  ( 0.2638984909335716500, 9.252728947331076981, 8.023974293733212804 ) ) ;
#64011 = ORIENTED_EDGE ( 'NONE', *, *, #36386, .F. ) ;
#64012 = CYLINDRICAL_SURFACE ( 'NONE', #21086, 5.000000000000000888 ) ;
#64013 = EDGE_LOOP ( 'NONE', ( #21357, #18996, #46269, #63227 ) ) ;
#64014 = EDGE_CURVE ( 'NONE', #29486, #47095, #56633, .T. ) ;
#64015 = AXIS2_PLACEMENT_3D ( 'NONE', #12248, #1951, #22223 ) ;
#64016 = VERTEX_POINT ( 'NONE', #60157 ) ;
#64017 = CARTESIAN_POINT ( 'NONE',  ( -15.49418265353465785, 8.465735697530092807, 10.51590495851239915 ) ) ;
#64018 = CARTESIAN_POINT ( 'NONE',  ( -3.650755842799271012, -28.29207189712390402, 13.56609188631020935 ) ) ;
#64020 = DIRECTION ( 'NONE',  ( 0.000000000000000000, -0.1387779952735677669, 0.9903235168508569553 ) ) ;
#64019 = AXIS2_PLACEMENT_3D ( 'NONE', #35741, #14480, #39434 ) ;
#64021 = LINE ( 'NONE', #8170, #25383 ) ;
#64022 = DIRECTION ( 'NONE',  ( 1.000000000000000000, 0.000000000000000000, 0.000000000000000000 ) ) ;
#64023 = CARTESIAN_POINT ( 'NONE',  ( -27.08421723179412410, 0.6782017488087925816, -2.188590898430384790 ) ) ;
#64024 = ORIENTED_EDGE ( 'NONE', *, *, #31732, .T. ) ;
#64025 = CYLINDRICAL_SURFACE ( 'NONE', #16645, 13.50000000000000178 ) ;
#64026 = CARTESIAN_POINT ( 'NONE',  ( 2.266490820343226353, 5.760233951938587893, -5.023127813992145363 ) ) ;
#64027 = CARTESIAN_POINT ( 'NONE',  ( -35.00000000000000000, 0.000000000000000000, 0.000000000000000000 ) ) ;
#64028 = EDGE_LOOP ( 'NONE', ( #54970, #42496, #46015, #36807 ) ) ;
#64029 = VECTOR ( 'NONE', #7049, 1000.000000000000114 ) ;
#64030 = CARTESIAN_POINT ( 'NONE',  ( -35.00000000000000000, 0.000000000000000000, 0.000000000000000000 ) ) ;
#64031 = ADVANCED_FACE ( 'NONE', ( #18949 ), #4657, .T. ) ;
#64032 = ORIENTED_EDGE ( 'NONE', *, *, #57736, .F. ) ;
#64033 = AXIS2_PLACEMENT_3D ( 'NONE', #15957, #26287, #62494 ) ;
#64034 = CARTESIAN_POINT ( 'NONE',  ( 2.241317068080785013, -7.501982551779182273, 1.415707718487486000 ) ) ;
#64035 = CARTESIAN_POINT ( 'NONE',  ( 1.948354844646975170, -9.982942661981358157, 6.595573209515230850 ) ) ;
#64036 = CYLINDRICAL_SURFACE ( 'NONE', #59704, 4.999999999999999112 ) ;
#64037 = EDGE_CURVE ( 'NONE', #37153, #3684, #44934, .T. ) ;
#64038 = CARTESIAN_POINT ( 'NONE',  ( -22.29290468048228036, 3.083035815361912402, -2.097193667172387421 ) ) ;
#64039 = AXIS2_PLACEMENT_3D ( 'NONE', #3608, #58459, #52805 ) ;
#64040 = CARTESIAN_POINT ( 'NONE',  ( -27.09252613521643127, -1.914180209342509320, 1.304094283668840282 ) ) ;
#64041 = DIRECTION ( 'NONE',  ( -1.000000000000000000, -0.000000000000000000, -0.000000000000000000 ) ) ;
#64042 = ORIENTED_EDGE ( 'NONE', *, *, #29269, .F. ) ;
#64043 = ORIENTED_EDGE ( 'NONE', *, *, #43343, .F. ) ;
#64044 = CARTESIAN_POINT ( 'NONE',  ( 1.462291587748811184, 3.724645088507181789, 12.08418494300826218 ) ) ;
#64045 = CARTESIAN_POINT ( 'NONE',  ( 1.000000000000000888, 7.387287142779368487, -1.295372019972108601 ) ) ;
#64046 = CARTESIAN_POINT ( 'NONE',  ( 0.2651627682582914369, -11.53745347823612910, -4.105539787731825818 ) ) ;
#64047 = EDGE_CURVE ( 'NONE', #43973, #31716, #55167, .T. ) ;
#64048 = DIRECTION ( 'NONE',  ( 0.000000000000000000, 0.000000000000000000, 1.000000000000000000 ) ) ;
#64049 = VECTOR ( 'NONE', #32587, 1000.000000000000000 ) ;
#64050 = DIRECTION ( 'NONE',  ( -1.000000000000000000, 0.000000000000000000, 0.000000000000000000 ) ) ;
#64051 = EDGE_CURVE ( 'NONE', #35661, #18660, #50202, .T. ) ;
#64052 = ORIENTED_EDGE ( 'NONE', *, *, #17715, .F. ) ;
#64053 = CARTESIAN_POINT ( 'NONE',  ( 5.982824234232984928, -9.655473559075929302, -9.442377055868243829 ) ) ;
#64054 = CARTESIAN_POINT ( 'NONE',  ( -35.00000000000000000, -12.21925492305359562, -3.640372113593682624 ) ) ;
#64055 = EDGE_CURVE ( 'NONE', #47570, #61002, #18455, .T. ) ;
#64056 = CARTESIAN_POINT ( 'NONE',  ( 2.241352910868908310, 1.407733736974867034, 7.503490710578237355 ) ) ;
#64057 = CYLINDRICAL_SURFACE ( 'NONE', #18035, 12.74999999999999822 ) ;
#64058 = ORIENTED_EDGE ( 'NONE', *, *, #20194, .T. ) ;
#64059 = CIRCLE ( 'NONE', #36486, 12.74999999999999822 ) ;
#64060 = CARTESIAN_POINT ( 'NONE',  ( -36.00000000000000711, 12.60630747491665993, -1.908798535168239718 ) ) ;
#64061 = CARTESIAN_POINT ( 'NONE',  ( -22.94572469358971389, -0.4123340087948151322, 4.870584850960092638 ) ) ;
#64062 = CIRCLE ( 'NONE', #24816, 5.000000000000000888 ) ;
#64063 = DIRECTION ( 'NONE',  ( 1.000000000000000000, -0.000000000000000000, 0.000000000000000000 ) ) ;
#64064 = CARTESIAN_POINT ( 'NONE',  ( -35.31912638668785576, -2.544741887441773986, -22.78557353984778544 ) ) ;
#64065 = AXIS2_PLACEMENT_3D ( 'NONE', #46335, #774, #61599 ) ;
#64066 = AXIS2_PLACEMENT_3D ( 'NONE', #51527, #15899, #34860 ) ;
#64067 = EDGE_CURVE ( 'NONE', #43944, #10662, #11983, .T. ) ;
#64068 = CARTESIAN_POINT ( 'NONE',  ( 2.430348790457182329, -3.678671624790087247, 6.761480562106249259 ) ) ;
#64069 = CARTESIAN_POINT ( 'NONE',  ( 2.247206125382827935, -5.923516414428620536, 4.819320926502617120 ) ) ;
#64070 =( BOUNDED_SURFACE ( )  B_SPLINE_SURFACE ( 3, 1, ( 
 ( #50360, #15411 ),
 ( #20404, #4806 ),
 ( #20075, #60977 ),
 ( #778, #46013 ) ),
 .UNSPECIFIED., .F., .F., .F. ) 
 B_SPLINE_SURFACE_WITH_KNOTS ( ( 4, 4 ),
 ( 2, 2 ),
 ( 0.000000000000000000, 1.000000000000000000 ),
 ( 0.000000000000000000, 1.000000000000000000 ),
 .UNSPECIFIED. ) 
 GEOMETRIC_REPRESENTATION_ITEM ( )  RATIONAL_B_SPLINE_SURFACE ( (
 ( 1.000000000000000000, 1.000000000000000000),
 ( 0.9942764183789327692, 0.8450855930916585379),
 ( 0.9942764183789327692, 0.8450855930916585379),
 ( 1.000000000000000000, 1.000000000000000000) ) ) 
 REPRESENTATION_ITEM ( '' )  SURFACE ( )  );
#64071 = VERTEX_POINT ( 'NONE', #30233 ) ;
#64072 = CARTESIAN_POINT ( 'NONE',  ( 2.244591118396557672, -2.510215291309266128, 7.211060161907638211 ) ) ;
#64073 = DIRECTION ( 'NONE',  ( 0.000000000000000000, 0.01356324068817992175, -0.9999080150203990547 ) ) ;
#64074 = CIRCLE ( 'NONE', #32223, 5.000000000000000000 ) ;
#64075 = CARTESIAN_POINT ( 'NONE',  ( -6.714735010819111949, -31.93429545817926751, -13.37736225704815141 ) ) ;
#64076 = ORIENTED_EDGE ( 'NONE', *, *, #47684, .F. ) ;
#64077 = CARTESIAN_POINT ( 'NONE',  ( 0.2655924914740778187, 12.05257978623653869, 2.169924872618101297 ) ) ;
#64078 = CYLINDRICAL_SURFACE ( 'NONE', #54423, 12.75000000000000178 ) ;
#64079 = LINE ( 'NONE', #19177, #54239 ) ;
#64080 = CIRCLE ( 'NONE', #39631, 12.74999999999999822 ) ;
#64081 = CARTESIAN_POINT ( 'NONE',  ( 0.3053067050349125289, -8.055646999028066801, 9.241336250185334222 ) ) ;
#64082 = CARTESIAN_POINT ( 'NONE',  ( 35.00000000000000000, 10.28547182238015978, 5.672855678558568648 ) ) ;
#64083 = AXIS2_PLACEMENT_3D ( 'NONE', #40356, #29724, #39721 ) ;
#64084 = CARTESIAN_POINT ( 'NONE',  ( -37.00000000000000711, 0.000000000000000000, 0.000000000000000000 ) ) ;
#64085 = ORIENTED_EDGE ( 'NONE', *, *, #55046, .F. ) ;
#64086 = DIRECTION ( 'NONE',  ( -1.000000000000000000, 0.000000000000000000, -0.000000000000000000 ) ) ;
#64087 = EDGE_CURVE ( 'NONE', #56264, #41059, #61529, .T. ) ;
#64088 = DIRECTION ( 'NONE',  ( -1.000000000000000000, 0.000000000000000000, 0.000000000000000000 ) ) ;
#64089 = CARTESIAN_POINT ( 'NONE',  ( 0.3006302518452032002, -9.533790235540692493, -7.704827863860894688 ) ) ;
#64090 = CARTESIAN_POINT ( 'NONE',  ( 2.827825597296805604, -7.250702617666013872, 5.372687261161241956 ) ) ;
#64091 =( BOUNDED_SURFACE ( )  B_SPLINE_SURFACE ( 3, 1, ( 
 ( #53901, #53245 ),
 ( #59220, #7689 ),
 ( #42928, #58575 ),
 ( #22988, #17990 ) ),
 .UNSPECIFIED., .F., .F., .F. ) 
 B_SPLINE_SURFACE_WITH_KNOTS ( ( 4, 4 ),
 ( 2, 2 ),
 ( 0.000000000000000000, 1.000000000000000000 ),
 ( 0.000000000000000000, 1.000000000000000000 ),
 .UNSPECIFIED. ) 
 GEOMETRIC_REPRESENTATION_ITEM ( )  RATIONAL_B_SPLINE_SURFACE ( (
 ( 1.000000000000000000, 1.000000000000000000),
 ( 0.9942764183789327692, 0.8450855930916580938),
 ( 0.9942764183789327692, 0.8450855930916580938),
 ( 1.000000000000000000, 1.000000000000000000) ) ) 
 REPRESENTATION_ITEM ( '' )  SURFACE ( )  );
#64092 = CARTESIAN_POINT ( 'NONE',  ( 2.268878695253355282, 7.551766617932588410, -1.181158368266874037 ) ) ;
#64093 = CARTESIAN_POINT ( 'NONE',  ( -27.10719052120871098, -1.962717903527672059, 1.310802520592011966 ) ) ;
#64094 = AXIS2_PLACEMENT_3D ( 'NONE', #23315, #23655, #18000 ) ;
#64095 = DIRECTION ( 'NONE',  ( 1.000000000000000000, 0.000000000000000000, -0.000000000000000000 ) ) ;
#64096 = CARTESIAN_POINT ( 'NONE',  ( -17.19065538327509657, 2.658487034042159802, -13.23633903133955414 ) ) ;
#64097 = VERTEX_POINT ( 'NONE', #33901 ) ;
#64098 = ORIENTED_EDGE ( 'NONE', *, *, #23293, .F. ) ;
#64099 = CARTESIAN_POINT ( 'NONE',  ( 2.350038591458114112, -7.305692696275646547, 7.710465783963738495 ) ) ;
#64100 = ORIENTED_EDGE ( 'NONE', *, *, #54503, .T. ) ;
#64101 = CARTESIAN_POINT ( 'NONE',  ( -22.27706089016750113, 2.622757446538697579, -2.583072118615352242 ) ) ;
#64102 = DIRECTION ( 'NONE',  ( -1.000000000000000000, 0.000000000000000000, 0.000000000000000000 ) ) ;
#64103 = CIRCLE ( 'NONE', #42883, 7.499999999999988454 ) ;
#64104 = CARTESIAN_POINT ( 'NONE',  ( -22.28023996335807411, -1.558279384310075510, 3.345627887484353913 ) ) ;
#64105 = ORIENTED_EDGE ( 'NONE', *, *, #17502, .T. ) ;
#64106 = DIRECTION ( 'NONE',  ( -1.000000000000000000, 0.000000000000000000, -0.000000000000000000 ) ) ;
#64107 = DIRECTION ( 'NONE',  ( 1.000000000000000000, 0.000000000000000000, -0.000000000000000000 ) ) ;
#64108 = DIRECTION ( 'NONE',  ( 0.3865475372811021382, 0.6938894834606000872, 0.6075346789811233439 ) ) ;
#64109 = EDGE_LOOP ( 'NONE', ( #53794, #65646, #10285, #9562 ) ) ;
#64110 = ORIENTED_EDGE ( 'NONE', *, *, #17360, .F. ) ;
#64111 = CARTESIAN_POINT ( 'NONE',  ( 1.000000000000000888, 7.484036900328569608, -0.4890722589968761191 ) ) ;
#64112 = EDGE_CURVE ( 'NONE', #47275, #59432, #4613, .T. ) ;
#64114 = DIRECTION ( 'NONE',  ( 1.000000000000000000, -0.000000000000000000, 0.000000000000000000 ) ) ;
#64113 = VECTOR ( 'NONE', #60396, 1000.000000000000000 ) ;
#64115 = CIRCLE ( 'NONE', #57777, 12.18650000000000055 ) ;
#64116 = ORIENTED_EDGE ( 'NONE', *, *, #7002, .F. ) ;
#64117 = VERTEX_POINT ( 'NONE', #4973 ) ;
#64118 = CARTESIAN_POINT ( 'NONE',  ( -35.00000000000000000, -2.772148766916031182, -11.86701198550359315 ) ) ;
#64119 = EDGE_CURVE ( 'NONE', #9450, #14653, #60846, .T. ) ;
#64120 = DIRECTION ( 'NONE',  ( -1.000000000000000000, -0.000000000000000000, 0.000000000000000000 ) ) ;
#64121 = VECTOR ( 'NONE', #42059, 1000.000000000000000 ) ;
#64122 = CARTESIAN_POINT ( 'NONE',  ( 2.000000000000001776, 6.906413915731192787, 0.6453518998147528274 ) ) ;
#64123 = CARTESIAN_POINT ( 'NONE',  ( -37.00000000000000711, -7.146664589317976102, 9.321877890560418933 ) ) ;
#64124 = DIRECTION ( 'NONE',  ( -0.9606638835031803270, -0.1984016392583687061, 0.1943236796486219886 ) ) ;
#64125 = CARTESIAN_POINT ( 'NONE',  ( -37.00000000000000711, -8.235637554476577193, -9.733281772932249609 ) ) ;
#64126 = VERTEX_POINT ( 'NONE', #46833 ) ;
#64127 = CIRCLE ( 'NONE', #48211, 12.18649999999999878 ) ;
#64128 = DIRECTION ( 'NONE',  ( 1.000000000000000000, -0.000000000000000000, -0.000000000000000000 ) ) ;
#64130 = CARTESIAN_POINT ( 'NONE',  ( 2.000000000000001776, -6.586971819220303281, -3.586335490831480843 ) ) ;
#64129 = AXIS2_PLACEMENT_3D ( 'NONE', #63707, #47147, #32144 ) ;
#64131 = FACE_OUTER_BOUND ( 'NONE', #988, .T. ) ;
#64132 = DIRECTION ( 'NONE',  ( 1.000000000000000000, 0.000000000000000000, 0.000000000000000000 ) ) ;
#64133 = CARTESIAN_POINT ( 'NONE',  ( 29.73648668909451587, 7.552544575588006737, 9.338272984228474627 ) ) ;
#64134 = AXIS2_PLACEMENT_3D ( 'NONE', #50967, #26337, #46620 ) ;
#64135 = CARTESIAN_POINT ( 'NONE',  ( -22.46225619532222595, -3.586917175123511381, 2.255146441673801405 ) ) ;
#64136 = DIRECTION ( 'NONE',  ( 1.000000000000000000, 0.000000000000000000, 0.000000000000000000 ) ) ;
#64137 = DIRECTION ( 'NONE',  ( 0.000000000000000000, 0.000000000000000000, 1.000000000000000000 ) ) ;
#64138 = DIRECTION ( 'NONE',  ( -0.8514458006899927600, 0.000000000000000000, -0.5244426074294281648 ) ) ;
#64139 = EDGE_CURVE ( 'NONE', #10582, #37098, #62010, .T. ) ;
#64140 = VECTOR ( 'NONE', #62140, 1000.000000000000000 ) ;
#64141 = VERTEX_POINT ( 'NONE', #21580 ) ;
#64142 = CARTESIAN_POINT ( 'NONE',  ( 2.000000000000001776, -2.664846396702537312, 6.404188155572974495 ) ) ;
#64143 = VERTEX_POINT ( 'NONE', #41498 ) ;
#64144 = CARTESIAN_POINT ( 'NONE',  ( -35.00000000000000000, 9.512294188641000403, -6.891188680298720115 ) ) ;
#64145 = CARTESIAN_POINT ( 'NONE',  ( 2.284126774967656370, -7.503320429541872727, -1.483972655035289190 ) ) ;
#64146 = VECTOR ( 'NONE', #31798, 1000.000000000000000 ) ;
#64147 = LINE ( 'NONE', #32880, #57947 ) ;
#64148 = CARTESIAN_POINT ( 'NONE',  ( 35.00000000000000000, 4.705694406421931860E-17, -3.469127814946512892E-15 ) ) ;
#64149 = DIRECTION ( 'NONE',  ( -1.000000000000000000, 0.000000000000000000, 0.000000000000000000 ) ) ;
#64150 = ORIENTED_EDGE ( 'NONE', *, *, #27308, .F. ) ;
#64151 = CARTESIAN_POINT ( 'NONE',  ( 2.990245332647774923, 0.5125330575219455564, -8.465748356453799417 ) ) ;
#64152 = FACE_OUTER_BOUND ( 'NONE', #24571, .T. ) ;
#64153 = B_SPLINE_CURVE_WITH_KNOTS ( 'NONE', 3,
 ( #49304, #3752, #19348, #19013, #33961, #35270 ),
 .UNSPECIFIED., .F., .F.,
 ( 4, 2, 4 ),
 ( 0.0002637379172157169513, 0.0009975831966609807061, 0.001731428476106244407 ),
 .UNSPECIFIED. ) ;
#64154 = DIRECTION ( 'NONE',  ( 0.000000000000000000, -0.01356324068817998940, 0.9999080150203990547 ) ) ;
#64155 = CARTESIAN_POINT ( 'NONE',  ( -22.29382655386184808, 2.689927793811030643, 2.586160974799802226 ) ) ;
#64156 = EDGE_CURVE ( 'NONE', #54308, #40020, #27977, .T. ) ;
#64157 = AXIS2_PLACEMENT_3D ( 'NONE', #7788, #28072, #64288 ) ;
#64158 = DIRECTION ( 'NONE',  ( -1.000000000000000000, 0.000000000000000000, 0.000000000000000000 ) ) ;
#64159 = ORIENTED_EDGE ( 'NONE', *, *, #57035, .F. ) ;
#64160 = DIRECTION ( 'NONE',  ( 0.000000000000000000, 0.9868265225415254749, 0.1617819965527686199 ) ) ;
#64161 = VERTEX_POINT ( 'NONE', #35843 ) ;
#64162 = CARTESIAN_POINT ( 'NONE',  ( 2.653899356899350526, 5.782420802795862791, -5.192946150929053317 ) ) ;
#64163 = DIRECTION ( 'NONE',  ( -1.000000000000000000, 0.000000000000000000, -0.000000000000000000 ) ) ;
#64164 = CIRCLE ( 'NONE', #35480, 12.18650000000000055 ) ;
#64165 = AXIS2_PLACEMENT_3D ( 'NONE', #1285, #16571, #47485 ) ;
#64166 = B_SPLINE_CURVE_WITH_KNOTS ( 'NONE', 3,
 ( #63, #20686, #5072, #40961, #29347, #49643, #55930, #4083, #59954, #54942, #9371, #49962, #24692, #44971, #19719, #39973 ),
 .UNSPECIFIED., .F., .F.,
 ( 4, 3, 3, 3, 3, 4 ),
 ( 0.000000000000000000, 0.0002999043160757389670, 0.0005998071753051078311, 0.0008997092107374667037, 0.001204458948195704076, 0.001510329163476617368 ),
 .UNSPECIFIED. ) ;
#64167 = CARTESIAN_POINT ( 'NONE',  ( 6.401101480914875630, -8.123926338959122972, 10.78346351568197470 ) ) ;
#64168 = EDGE_LOOP ( 'NONE', ( #12243, #14549, #55589, #61301 ) ) ;
#64169 = ORIENTED_EDGE ( 'NONE', *, *, #30056, .T. ) ;
#64170 = CARTESIAN_POINT ( 'NONE',  ( -27.10512513516275845, 2.256292013315186473, -0.6711200423626798583 ) ) ;
#64171 = EDGE_CURVE ( 'NONE', #12912, #54893, #18432, .T. ) ;
#64172 = CARTESIAN_POINT ( 'NONE',  ( 2.276905613633471326, 5.031956778294004451, 5.757134111949740785 ) ) ;
#64173 = CARTESIAN_POINT ( 'NONE',  ( 2.889800649504073782, -0.06738247734054683691, 6.121013568931506832 ) ) ;
#64174 = CARTESIAN_POINT ( 'NONE',  ( 35.00000000000000000, 10.91536515067648239, 4.339012074899986970 ) ) ;
#64175 = CARTESIAN_POINT ( 'NONE',  ( 0.2915757698887319060, 9.248369946372635653, -8.040595355212850848 ) ) ;
#64176 = CARTESIAN_POINT ( 'NONE',  ( 0.3675815128205912052, -10.76447900494944321, 5.910255304480407368 ) ) ;
#64177 = EDGE_CURVE ( 'NONE', #35942, #54366, #16586, .T. ) ;
#64178 = ORIENTED_EDGE ( 'NONE', *, *, #7586, .T. ) ;
#64179 = ORIENTED_EDGE ( 'NONE', *, *, #3993, .T. ) ;
#64180 = ORIENTED_EDGE ( 'NONE', *, *, #62091, .T. ) ;
#64181 = CARTESIAN_POINT ( 'NONE',  ( -35.00000000000000000, 10.91072401419410554, 5.428340790341743549 ) ) ;
#64182 = CIRCLE ( 'NONE', #35503, 12.18650000000000055 ) ;
#64183 = DIRECTION ( 'NONE',  ( 0.000000000000000000, -0.5243256840888623760, -0.8515178078024829844 ) ) ;
#64184 = EDGE_CURVE ( 'NONE', #22230, #58425, #60459, .T. ) ;
#64185 = ORIENTED_EDGE ( 'NONE', *, *, #8383, .T. ) ;
#64186 = CARTESIAN_POINT ( 'NONE',  ( 0.2648978790185610999, -2.256510822326061483, -12.03635331166814382 ) ) ;
#64187 = CARTESIAN_POINT ( 'NONE',  ( 2.255723233588952770, -7.544965460065571783, 1.196143347838687143 ) ) ;
#64188 = VERTEX_POINT ( 'NONE', #36852 ) ;
#64189 = CARTESIAN_POINT ( 'NONE',  ( 2.305787727787083519, 7.135468203929983488, 2.774453000917173284 ) ) ;
#64190 = CIRCLE ( 'NONE', #59928, 12.75000000000000178 ) ;
#64191 = CARTESIAN_POINT ( 'NONE',  ( -35.00000000000000000, -3.827046518385164742, 11.56998259273176188 ) ) ;
#64192 = DIRECTION ( 'NONE',  ( 0.000000000000000000, 0.000000000000000000, 1.000000000000000000 ) ) ;
#64193 = ORIENTED_EDGE ( 'NONE', *, *, #30380, .T. ) ;
#64194 = ORIENTED_EDGE ( 'NONE', *, *, #24711, .F. ) ;
#64195 = CARTESIAN_POINT ( 'NONE',  ( -4.989057617119011745, -0.9162120371760335003, 11.96497202265570259 ) ) ;
#64196 = UNCERTAINTY_MEASURE_WITH_UNIT (LENGTH_MEASURE( 1.000000000000000082E-05 ), #50125, 'distance_accuracy_value', 'NONE');
#64197 = ORIENTED_EDGE ( 'NONE', *, *, #22832, .F. ) ;
#64198 = ADVANCED_FACE ( 'NONE', ( #30866 ), #56144, .T. ) ;
#64199 = DIRECTION ( 'NONE',  ( 0.000000000000000000, 0.01356324068817992175, -0.9999080150203990547 ) ) ;
#64200 = ORIENTED_EDGE ( 'NONE', *, *, #48114, .F. ) ;
#64201 = ORIENTED_EDGE ( 'NONE', *, *, #45696, .F. ) ;
#64202 = CARTESIAN_POINT ( 'NONE',  ( 0.2650492433740054277, -4.084772052580676771, 11.54478237753290770 ) ) ;
#64203 = LINE ( 'NONE', #50234, #42583 ) ;
#64204 = CARTESIAN_POINT ( 'NONE',  ( 35.00000000000000000, 6.564808257521768553, -10.93004082984021075 ) ) ;
#64205 = VECTOR ( 'NONE', #34521, 1000.000000000000000 ) ;
#64206 = DIRECTION ( 'NONE',  ( 0.000000000000000000, 0.2618041379715562722, -0.9651210252299813330 ) ) ;
#64207 = DIRECTION ( 'NONE',  ( -1.000000000000000000, 0.000000000000000000, 0.000000000000000000 ) ) ;
#64208 = CARTESIAN_POINT ( 'NONE',  ( -22.59983133926798260, -4.650609684383241849, -0.06110861519531800984 ) ) ;
#64209 = ORIENTED_EDGE ( 'NONE', *, *, #134, .F. ) ;
#64210 = CARTESIAN_POINT ( 'NONE',  ( 37.00000000000000711, -11.17622378668003691, 3.614449339633606595 ) ) ;
#64211 = EDGE_LOOP ( 'NONE', ( #56126, #49270, #19930, #63564 ) ) ;
#64212 = CARTESIAN_POINT ( 'NONE',  ( 37.00000000000000711, 9.557269938331552694, -7.561043153948004303 ) ) ;
#64213 = CYLINDRICAL_SURFACE ( 'NONE', #55302, 2.899999999999994582 ) ;
#64214 = ORIENTED_EDGE ( 'NONE', *, *, #18431, .T. ) ;
#64215 = DIRECTION ( 'NONE',  ( 1.000000000000000000, -0.000000000000000000, 0.000000000000000000 ) ) ;
#64216 = DIRECTION ( 'NONE',  ( -1.000000000000000000, 0.000000000000000000, 0.000000000000000000 ) ) ;
#64217 = CARTESIAN_POINT ( 'NONE',  ( 2.000000000000001776, -1.018311147294094443, -6.861346417234492456 ) ) ;
#64218 = ORIENTED_EDGE ( 'NONE', *, *, #59741, .T. ) ;
#64219 = VERTEX_POINT ( 'NONE', #56486 ) ;
#64220 = CARTESIAN_POINT ( 'NONE',  ( 2.589278595513797576, -6.829211973730751950, -3.664724287895283261 ) ) ;
#64221 = VERTEX_POINT ( 'NONE', #15260 ) ;
#64222 = CARTESIAN_POINT ( 'NONE',  ( -24.75896104215371096, -11.63928102839248879, 6.841611787138283773 ) ) ;
#64223 = CARTESIAN_POINT ( 'NONE',  ( -10.00000000000000178, 0.000000000000000000, 0.000000000000000000 ) ) ;
#64224 = CARTESIAN_POINT ( 'NONE',  ( 0.2657645697724694833, -9.283243433323022487, -7.987126944299723696 ) ) ;
#64225 = CARTESIAN_POINT ( 'NONE',  ( 1.014383007554951144, -9.280879504740996211, 8.367379244277097783 ) ) ;
#64226 = ORIENTED_EDGE ( 'NONE', *, *, #18942, .T. ) ;
#64227 = DIRECTION ( 'NONE',  ( 0.000000000000000000, -0.1118654143051476951, -0.9937233664769775654 ) ) ;
#64228 = AXIS2_PLACEMENT_3D ( 'NONE', #24346, #63590, #29341 ) ;
#64229 = EDGE_CURVE ( 'NONE', #65410, #14359, #25908, .T. ) ;
#64230 = CARTESIAN_POINT ( 'NONE',  ( 15.74859868605383717, -29.13321728093753649, -10.87107032828078701 ) ) ;
#64231 = CARTESIAN_POINT ( 'NONE',  ( 9.022832866668583307, 5.316194047393634214, -12.41044072607060400 ) ) ;
#64232 = CARTESIAN_POINT ( 'NONE',  ( -22.27384469013076185, 2.625926801827887846, -2.581192766446249731 ) ) ;
#64233 = CARTESIAN_POINT ( 'NONE',  ( 5.530133899448235191, 0.01111090067015107867, 0.01149180883054605647 ) ) ;
#64234 = CARTESIAN_POINT ( 'NONE',  ( 4.838183347715137472, -10.56890113247325047, -5.693500808758303222 ) ) ;
#64235 = CARTESIAN_POINT ( 'NONE',  ( -36.00000000000000711, -0.1414404973751254013, -12.74921544981111410 ) ) ;
#64236 = VECTOR ( 'NONE', #53352, 1000.000000000000000 ) ;
#64237 = EDGE_CURVE ( 'NONE', #17594, #55487, #26545, .T. ) ;
#64238 = ORIENTED_EDGE ( 'NONE', *, *, #11053, .F. ) ;
#64239 = CARTESIAN_POINT ( 'NONE',  ( -23.18047892478189453, 2.037851053449341698, 4.338318103648280299 ) ) ;
#64240 = VERTEX_POINT ( 'NONE', #42819 ) ;
#64241 = DIRECTION ( 'NONE',  ( -0.02770351589312032917, 0.9996161839461982224, 0.000000000000000000 ) ) ;
#64242 = ADVANCED_FACE ( 'NONE', ( #37840 ), #37170, .T. ) ;
#64243 = CARTESIAN_POINT ( 'NONE',  ( -22.27706485742869091, -3.563814065926672381, 0.9221835209182321913 ) ) ;
#64244 = DIRECTION ( 'NONE',  ( -1.000000000000000000, -0.000000000000000000, -0.000000000000000000 ) ) ;
#64245 = CARTESIAN_POINT ( 'NONE',  ( 0.2653141617321040369, -12.24612535104215638, -0.04404194803643789180 ) ) ;
#64246 = EDGE_CURVE ( 'NONE', #36643, #27041, #26853, .T. ) ;
#64247 = ORIENTED_EDGE ( 'NONE', *, *, #62425, .T. ) ;
#64248 = AXIS2_PLACEMENT_3D ( 'NONE', #37680, #47654, #2100 ) ;
#64249 = ORIENTED_EDGE ( 'NONE', *, *, #24025, .F. ) ;
#64250 = ORIENTED_EDGE ( 'NONE', *, *, #62214, .T. ) ;
#64251 = CARTESIAN_POINT ( 'NONE',  ( -36.00000000000000711, 0.6593684648222306599, -12.73293890771482850 ) ) ;
#64252 = CARTESIAN_POINT ( 'NONE',  ( -22.28121537037576871, -3.345440028056690274, -1.565596675942159788 ) ) ;
#64253 = EDGE_CURVE ( 'NONE', #35323, #21896, #55531, .T. ) ;
#64254 = ORIENTED_EDGE ( 'NONE', *, *, #16861, .F. ) ;
#64255 = CARTESIAN_POINT ( 'NONE',  ( -22.27718150314433387, -2.479231311682827066, -2.721613812022972478 ) ) ;
#64256 = CARTESIAN_POINT ( 'NONE',  ( 2.889800649504073782, -6.121013568931505944, -0.06738247734056820870 ) ) ;
#64257 = CARTESIAN_POINT ( 'NONE',  ( 24.82652845881425208, 10.42385221765396608, -8.578654028722157321 ) ) ;
#64258 = CARTESIAN_POINT ( 'NONE',  ( 0.2646305136544072623, -11.55263159009961704, 4.064188116014512353 ) ) ;
#64259 = ORIENTED_EDGE ( 'NONE', *, *, #15424, .T. ) ;
#64260 = CARTESIAN_POINT ( 'NONE',  ( 35.00000000000000000, 11.65554240571056788, -1.456211999474385843 ) ) ;
#64261 = EDGE_CURVE ( 'NONE', #42095, #36790, #4889, .T. ) ;
#64262 = CYLINDRICAL_SURFACE ( 'NONE', #112, 5.000000000000000888 ) ;
#64263 = FACE_OUTER_BOUND ( 'NONE', #7076, .T. ) ;
#64265 = ORIENTED_EDGE ( 'NONE', *, *, #10751, .F. ) ;
#64264 = CARTESIAN_POINT ( 'NONE',  ( 2.000000000000001776, 0.000000000000000000, 0.000000000000000000 ) ) ;
#64266 = CARTESIAN_POINT ( 'NONE',  ( 0.2646305136544065406, 4.064188116014703311, -11.55263159009954421 ) ) ;
#64267 = ORIENTED_EDGE ( 'NONE', *, *, #10656, .F. ) ;
#64268 = CARTESIAN_POINT ( 'NONE',  ( -35.00000000000000000, -11.10408318471063716, 6.265926637539457111 ) ) ;
#64269 = B_SPLINE_CURVE_WITH_KNOTS ( 'NONE', 3,
 ( #36485, #4929, #29843, #35496, #60438, #21183, #55794, #30501, #65413, #25192 ),
 .UNSPECIFIED., .F., .F.,
 ( 4, 3, 3, 4 ),
 ( 0.000000000000000000, 6.607638129004513277E-05, 9.911389841680569692E-05, 0.0001667630577588627449 ),
 .UNSPECIFIED. ) ;
#64270 = ORIENTED_EDGE ( 'NONE', *, *, #30754, .T. ) ;
#64271 = CARTESIAN_POINT ( 'NONE',  ( -36.00000000000000711, -7.094637218249278732, -10.59380114696477904 ) ) ;
#64272 = CARTESIAN_POINT ( 'NONE',  ( 0.3474126878361829540, 3.953748424960800811, -11.61929161290141721 ) ) ;
#64273 = CIRCLE ( 'NONE', #49444, 5.000000000000000000 ) ;
#64274 = CARTESIAN_POINT ( 'NONE',  ( 5.516018279890452902, -0.002104829434641057422, -0.006440244342253404787 ) ) ;
#64275 = CARTESIAN_POINT ( 'NONE',  ( 0.3341166715381352348, -3.958014133396687839, 11.61315925169693664 ) ) ;
#64276 = CARTESIAN_POINT ( 'NONE',  ( 0.2652384770603681829, -11.53005438969046814, 4.126289928142361951 ) ) ;
#64277 = CARTESIAN_POINT ( 'NONE',  ( -35.00000000000000000, 1.908798535168378274, 12.60630747491664039 ) ) ;
#64278 = CARTESIAN_POINT ( 'NONE',  ( 11.67759032571662736, 13.41004018116123042, -1.561691431055280299 ) ) ;
#64279 = EDGE_CURVE ( 'NONE', #40664, #47275, #32151, .T. ) ;
#64280 =( BOUNDED_SURFACE ( )  B_SPLINE_SURFACE ( 3, 1, ( 
 ( #60464, #53864 ),
 ( #13600, #3975 ),
 ( #44198, #59494 ),
 ( #24237, #14566 ) ),
 .UNSPECIFIED., .F., .F., .F. ) 
 B_SPLINE_SURFACE_WITH_KNOTS ( ( 4, 4 ),
 ( 2, 2 ),
 ( 0.000000000000000000, 1.000000000000000000 ),
 ( 0.000000000000000000, 1.000000000000000000 ),
 .UNSPECIFIED. ) 
 GEOMETRIC_REPRESENTATION_ITEM ( )  RATIONAL_B_SPLINE_SURFACE ( (
 ( 1.000000000000000000, 1.000000000000000000),
 ( 0.9856612449720755231, 0.9999558406602322425),
 ( 0.9856612449720755231, 0.9999558406602322425),
 ( 1.000000000000000000, 1.000000000000000000) ) ) 
 REPRESENTATION_ITEM ( '' )  SURFACE ( )  );
#64281 = ORIENTED_EDGE ( 'NONE', *, *, #44360, .F. ) ;
#64282 = CARTESIAN_POINT ( 'NONE',  ( 36.00000000000000711, 6.415447294506860132, 11.01837265713066039 ) ) ;
#64283 = ORIENTED_EDGE ( 'NONE', *, *, #59253, .F. ) ;
#64284 = EDGE_CURVE ( 'NONE', #25922, #27962, #43738, .T. ) ;
#64285 = ORIENTED_EDGE ( 'NONE', *, *, #17675, .T. ) ;
#64286 = CARTESIAN_POINT ( 'NONE',  ( 1.633930747253119486, 1.494486044208924946, -12.61425129500200093 ) ) ;
#64287 = CARTESIAN_POINT ( 'NONE',  ( -22.28939870658739864, 3.352428181135941543, 1.608176106660523130 ) ) ;
#64288 = DIRECTION ( 'NONE',  ( 0.000000000000000000, 0.01356324068817992001, -0.9999080150203990547 ) ) ;
#64289 = B_SPLINE_CURVE_WITH_KNOTS ( 'NONE', 3,
 ( #45186, #56150, #55844, #46202, #25570, #45203, #45515, #25915, #30873, #56845, #51842, #31537, #40877, #50537, #15904, #14913 ),
 .UNSPECIFIED., .F., .F.,
 ( 4, 2, 2, 2, 2, 2, 2, 4 ),
 ( 9.697399036122160616E-18, 0.002292800386316098255, 0.003439200579474143912, 0.004585600772632189570, 0.005732000965790236963, 0.006878401158948284355, 0.008024801352106331748, 0.009171201545264380875 ),
 .UNSPECIFIED. ) ;
#64290 = CARTESIAN_POINT ( 'NONE',  ( -22.28939870658739864, 2.099199915896319268, 3.068935452695135346 ) ) ;
#64291 = FACE_OUTER_BOUND ( 'NONE', #27513, .T. ) ;
#64292 = CARTESIAN_POINT ( 'NONE',  ( 0.3218525148189821383, 10.74192973049796151, -5.919623386703225520 ) ) ;
#64293 = VECTOR ( 'NONE', #7981, 1000.000000000000000 ) ;
#64294 = FACE_OUTER_BOUND ( 'NONE', #49067, .T. ) ;
#64295 = VERTEX_POINT ( 'NONE', #6937 ) ;
#64296 = DIRECTION ( 'NONE',  ( 1.000000000000000000, -0.000000000000000000, 0.000000000000000000 ) ) ;
#64297 = LINE ( 'NONE', #4113, #17548 ) ;
#64298 = DIRECTION ( 'NONE',  ( -1.000000000000000000, -0.000000000000000000, 0.000000000000000000 ) ) ;
#64299 =( GEOMETRIC_REPRESENTATION_CONTEXT ( 3 ) GLOBAL_UNCERTAINTY_ASSIGNED_CONTEXT ( ( #47887 ) ) GLOBAL_UNIT_ASSIGNED_CONTEXT ( ( #34154, #14201, #55431 ) ) REPRESENTATION_CONTEXT ( 'NONE', 'WORKASPACE' ) );
#64300 = ADVANCED_FACE ( 'NONE', ( #53135 ), #32178, .T. ) ;
#64301 = VECTOR ( 'NONE', #21198, 1000.000000000000000 ) ;
#64302 = EDGE_CURVE ( 'NONE', #44696, #42318, #17318, .T. ) ;
#64303 = CARTESIAN_POINT ( 'NONE',  ( -10.84719144215113218, -4.830053348895781085, 12.61335488639389446 ) ) ;
#64304 = CARTESIAN_POINT ( 'NONE',  ( 9.102085259661365058, 3.314740859770817227, -11.53545134040598796 ) ) ;
#64305 = EDGE_LOOP ( 'NONE', ( #38352, #34571, #14087, #8573 ) ) ;
#64306 = DIRECTION ( 'NONE',  ( 0.000000000000000000, -0.8169148498130338609, 0.5767582926624880146 ) ) ;
#64307 = CYLINDRICAL_SURFACE ( 'NONE', #8123, 6.936499999999988120 ) ;
#64308 = ADVANCED_FACE ( 'NONE', ( #7238 ), #47499, .F. ) ;
#64309 = CIRCLE ( 'NONE', #39868, 2.899999999999995914 ) ;
#64310 = ADVANCED_FACE ( 'NONE', ( #63419 ), #17889, .T. ) ;
#64311 = CARTESIAN_POINT ( 'NONE',  ( -35.00000000000000000, 0.000000000000000000, 0.000000000000000000 ) ) ;
#64312 = DIRECTION ( 'NONE',  ( 0.000000000000000000, 0.2149704402110246548, -0.9766205557100865464 ) ) ;
#64313 = ORIENTED_EDGE ( 'NONE', *, *, #2929, .F. ) ;
#64314 = EDGE_CURVE ( 'NONE', #11411, #2844, #18222, .T. ) ;
#64315 = CARTESIAN_POINT ( 'NONE',  ( 35.00000000000000000, 9.700295462048766026, 7.376655759824770620 ) ) ;
#64316 = CARTESIAN_POINT ( 'NONE',  ( -37.00000000000000711, 0.000000000000000000, 0.000000000000000000 ) ) ;
#64317 = ORIENTED_EDGE ( 'NONE', *, *, #14987, .F. ) ;
#64318 = CARTESIAN_POINT ( 'NONE',  ( 22.19367488060846227, 12.07937757942956658, -6.038551727115931911 ) ) ;
#64319 = DIRECTION ( 'NONE',  ( -1.000000000000000000, 0.000000000000000000, 0.000000000000000000 ) ) ;
#64320 = ADVANCED_FACE ( 'NONE', ( #62436 ), #31849, .F. ) ;
#64321 = VERTEX_POINT ( 'NONE', #8891 ) ;
#64322 = ORIENTED_EDGE ( 'NONE', *, *, #27839, .T. ) ;
#64323 = DIRECTION ( 'NONE',  ( 0.000000000000000000, 0.01356324068817998073, -0.9999080150203990547 ) ) ;
#64324 = ORIENTED_EDGE ( 'NONE', *, *, #27777, .T. ) ;
#64325 = DIRECTION ( 'NONE',  ( 1.000000000000000000, 0.000000000000000000, 0.000000000000000000 ) ) ;
#64326 = DIRECTION ( 'NONE',  ( 1.000000000000000000, 0.000000000000000000, -0.000000000000000000 ) ) ;
#64327 = CARTESIAN_POINT ( 'NONE',  ( -38.57634030218385846, -26.62784119520750892, 4.499999999999997335 ) ) ;
#64328 = CARTESIAN_POINT ( 'NONE',  ( 2.000000000000001776, -6.906413915731192787, 0.6453518998147164121 ) ) ;
#64329 = EDGE_CURVE ( 'NONE', #22231, #17057, #29181, .T. ) ;
#64330 = DIRECTION ( 'NONE',  ( 0.000000000000000000, 0.2618041379715633776, -0.9651210252299794456 ) ) ;
#64332 = ORIENTED_EDGE ( 'NONE', *, *, #11703, .F. ) ;
#64331 = CARTESIAN_POINT ( 'NONE',  ( 2.241536586108912488, -7.634468130435847044, 0.006292724672621609859 ) ) ;
#64333 = DIRECTION ( 'NONE',  ( 0.000000000000000000, 0.01356324068817998940, -0.9999080150203990547 ) ) ;
#64334 = EDGE_CURVE ( 'NONE', #7333, #52741, #49782, .T. ) ;
#64335 = ORIENTED_EDGE ( 'NONE', *, *, #26941, .T. ) ;
#64336 = CARTESIAN_POINT ( 'NONE',  ( 0.2653519991613824680, 10.61652626436036506, -6.104031847944908939 ) ) ;
#64337 = ORIENTED_EDGE ( 'NONE', *, *, #62843, .T. ) ;
#64338 = VERTEX_POINT ( 'NONE', #9200 ) ;
#64339 = DIRECTION ( 'NONE',  ( 0.000000000000000000, -0.01356324068818000848, 0.9999080150203990547 ) ) ;
#64340 = EDGE_CURVE ( 'NONE', #50020, #34013, #11004, .T. ) ;
#64341 = CARTESIAN_POINT ( 'NONE',  ( -16.37486794060187734, -29.30468282063785779, 10.24044889374758149 ) ) ;
#64342 = DIRECTION ( 'NONE',  ( 0.000000000000000000, -0.9651210252299767811, -0.2618041379715732031 ) ) ;
#64343 = CARTESIAN_POINT ( 'NONE',  ( 24.34326217128684888, -1.446676816449340208, 11.91385012721646319 ) ) ;
#64344 = CARTESIAN_POINT ( 'NONE',  ( 3.388896915696422152, -10.79019736087639458, -5.264843862020488707 ) ) ;
#64345 = EDGE_CURVE ( 'NONE', #14524, #21230, #53506, .T. ) ;
#64346 = DIRECTION ( 'NONE',  ( -1.000000000000000000, -0.000000000000000000, 0.000000000000000000 ) ) ;
#64348 = ORIENTED_EDGE ( 'NONE', *, *, #24185, .T. ) ;
#64347 = EDGE_CURVE ( 'NONE', #36171, #25992, #19501, .T. ) ;
#64349 = VECTOR ( 'NONE', #5452, 1000.000000000000114 ) ;
#64350 = LINE ( 'NONE', #34969, #42111 ) ;
#64351 = EDGE_LOOP ( 'NONE', ( #34396, #16602, #37299, #30733 ) ) ;
#64352 = DIRECTION ( 'NONE',  ( 0.000000000000000000, 0.9346839223284527653, -0.3554799084909002205 ) ) ;
#64353 = EDGE_CURVE ( 'NONE', #36589, #6075, #17620, .T. ) ;
#64354 = FACE_OUTER_BOUND ( 'NONE', #3615, .T. ) ;
#64355 = ORIENTED_EDGE ( 'NONE', *, *, #3130, .F. ) ;
#64356 = CARTESIAN_POINT ( 'NONE',  ( 2.259025283528087957, -7.499281868334244372, 1.461109758650534829 ) ) ;
#64357 = DIRECTION ( 'NONE',  ( -1.000000000000000000, -1.685093406416449860E-16, 1.011030131491573426E-17 ) ) ;
#64358 = CARTESIAN_POINT ( 'NONE',  ( 12.10998784662220729, -10.46621227226782835, -8.526922110106905706 ) ) ;
#64359 = AXIS2_PLACEMENT_3D ( 'NONE', #26406, #9797, #30082 ) ;
#64360 = CARTESIAN_POINT ( 'NONE',  ( -27.10719052120871098, -2.261993590776032459, 0.6736837626858792616 ) ) ;
#64361 = CARTESIAN_POINT ( 'NONE',  ( 2.827825597296802496, -8.776379025186162863, -2.100863646776143234 ) ) ;
#64362 = CARTESIAN_POINT ( 'NONE',  ( -35.00000000000000000, -1.456211999474261054, -11.65554240571058742 ) ) ;
#64363 = ORIENTED_EDGE ( 'NONE', *, *, #11090, .T. ) ;
#64364 = ORIENTED_EDGE ( 'NONE', *, *, #26352, .F. ) ;
#64365 = CARTESIAN_POINT ( 'NONE',  ( 1.287602823385632034, 3.781900355162443272, 12.00540336274424646 ) ) ;
#64366 = CARTESIAN_POINT ( 'NONE',  ( 0.000000000000000000, -6.160607635185357367, -4.277489166005654653 ) ) ;
#64367 = CARTESIAN_POINT ( 'NONE',  ( -10.95212338237647920, -9.902220863987562183, 6.778349501228839280 ) ) ;
#64368 = EDGE_CURVE ( 'NONE', #22798, #3384, #60893, .T. ) ;
#64369 = DIRECTION ( 'NONE',  ( 0.000000000000000000, -0.01356324068818685717, 0.9999080150203989437 ) ) ;
#64370 = DIRECTION ( 'NONE',  ( -1.000000000000000000, 0.000000000000000000, 0.000000000000000000 ) ) ;
#64371 = CYLINDRICAL_SURFACE ( 'NONE', #7594, 12.75000000000000178 ) ;
#64372 = CARTESIAN_POINT ( 'NONE',  ( -35.00000000000000000, -9.040300684349640292, -7.499679039484155041 ) ) ;
#64373 = CARTESIAN_POINT ( 'NONE',  ( -27.08579483061203064, -2.081508743190409572, -0.9690219683547880436 ) ) ;
#64374 = DIRECTION ( 'NONE',  ( 1.000000000000000000, 0.000000000000000000, 0.000000000000000000 ) ) ;
#64375 = EDGE_LOOP ( 'NONE', ( #12064, #44661, #55832, #26539 ) ) ;
#64376 = CARTESIAN_POINT ( 'NONE',  ( 0.2653519789438778531, 12.06397564829376101, 2.104833950422620337 ) ) ;
#64377 = CARTESIAN_POINT ( 'NONE',  ( -22.28415773361650309, -2.588610893123045820, 2.647149619609370230 ) ) ;
#64378 = EDGE_CURVE ( 'NONE', #47095, #50460, #8236, .T. ) ;
#64379 = CARTESIAN_POINT ( 'NONE',  ( 2.034671305880032754, 8.476347594673310226, 8.030508024279379597 ) ) ;
#64380 = AXIS2_PLACEMENT_3D ( 'NONE', #32095, #6858, #2534 ) ;
#64381 = CARTESIAN_POINT ( 'NONE',  ( 2.280717697723839255, -0.1564731737569588776, -7.645922213779910770 ) ) ;
#64382 = CARTESIAN_POINT ( 'NONE',  ( 2.245754705088395031, -5.920355780195118989, 4.822435078157726984 ) ) ;
#64383 = CIRCLE ( 'NONE', #7058, 12.74999999999999822 ) ;
#64384 = VERTEX_POINT ( 'NONE', #3264 ) ;
#64385 = LINE ( 'NONE', #14172, #34406 ) ;
#64386 = CARTESIAN_POINT ( 'NONE',  ( 28.55105714595230637, 12.36547357143752990, 5.429635869807071025 ) ) ;
#64387 = CARTESIAN_POINT ( 'NONE',  ( 4.682340427901537261, -31.48164499408211014, -13.94155213824621953 ) ) ;
#64388 = ORIENTED_EDGE ( 'NONE', *, *, #39194, .T. ) ;
#64389 = DIRECTION ( 'NONE',  ( 0.000000000000000000, 0.000000000000000000, 1.000000000000000000 ) ) ;
#64390 = DIRECTION ( 'NONE',  ( 1.000000000000000000, 0.000000000000000000, 0.000000000000000000 ) ) ;
#64391 = LINE ( 'NONE', #53468, #41296 ) ;
#64392 = EDGE_CURVE ( 'NONE', #47265, #30454, #57720, .T. ) ;
#64393 = CARTESIAN_POINT ( 'NONE',  ( 0.2648978790185584908, -7.972372351883092456, 9.295532325666423290 ) ) ;
#64394 = DIRECTION ( 'NONE',  ( 0.000000000000000000, 0.01356324068818000328, -0.9999080150203990547 ) ) ;
#64395 = CARTESIAN_POINT ( 'NONE',  ( 36.00000000000000711, 12.60630747491662973, -1.908798535168425792 ) ) ;
#64396 = ORIENTED_EDGE ( 'NONE', *, *, #34136, .T. ) ;
#64397 = DIRECTION ( 'NONE',  ( 0.000000000000000000, 0.9970832820307036215, 0.07632122047556835764 ) ) ;
#64398 = CARTESIAN_POINT ( 'NONE',  ( 0.2646305136544065406, 10.67138229758237955, -6.008537389229304360 ) ) ;
#64399 = CARTESIAN_POINT ( 'NONE',  ( 3.100650473569440901, 7.585586315875629815, -2.280184661131237078 ) ) ;
#64400 = CARTESIAN_POINT ( 'NONE',  ( 3.152665057734045373, -6.378477742800418682, 4.725420687650736085 ) ) ;
#64401 = DIRECTION ( 'NONE',  ( 0.3865475372811021382, -0.4442537292684384798, -0.8082200352954632683 ) ) ;
#64402 = CARTESIAN_POINT ( 'NONE',  ( 35.00000000000000000, 4.986700593229853595, 10.63508530065516311 ) ) ;
#64403 = DIRECTION ( 'NONE',  ( 0.000000000000000000, -0.01356324068817998940, 0.9999080150203990547 ) ) ;
#64404 = CARTESIAN_POINT ( 'NONE',  ( 2.297017764049619437, 1.166330442180481652, -7.563558677601394997 ) ) ;
#64405 = ORIENTED_EDGE ( 'NONE', *, *, #18431, .F. ) ;
#64406 = EDGE_LOOP ( 'NONE', ( #3644, #10170, #14587, #5998 ) ) ;
#64407 = LINE ( 'NONE', #54122, #4536 ) ;
#64408 = ORIENTED_EDGE ( 'NONE', *, *, #24959, .F. ) ;
#64409 = B_SPLINE_CURVE_WITH_KNOTS ( 'NONE', 3,
 ( #28225, #22586, #26916, #42850, #1330, #62160, #58160, #32856 ),
 .UNSPECIFIED., .F., .F.,
 ( 4, 2, 2, 4 ),
 ( 0.004099133380581623104, 0.006211397827347840857, 0.007267530050730946697, 0.008323662274114053405 ),
 .UNSPECIFIED. ) ;
#64410 = FILL_AREA_STYLE ('',( #44145 ) ) ;
#64411 = EDGE_CURVE ( 'NONE', #5936, #30787, #29480, .T. ) ;
#64412 = CARTESIAN_POINT ( 'NONE',  ( -22.29195009621226831, 2.585382421603450442, -2.682867222693505749 ) ) ;
#64413 = DIRECTION ( 'NONE',  ( 0.000000000000000000, -0.8009703041134234036, -0.5987040770935587730 ) ) ;
#64414 = ADVANCED_FACE ( 'NONE', ( #19190 ), #39461, .T. ) ;
#64415 = CARTESIAN_POINT ( 'NONE',  ( -22.31099767395441091, -1.667781795950512347, 3.395517675085599762 ) ) ;
#64416 = ORIENTED_EDGE ( 'NONE', *, *, #38751, .T. ) ;
#64417 = CARTESIAN_POINT ( 'NONE',  ( 0.2717059086739028184, 5.971041827598971174, -10.69429229731970743 ) ) ;
#64418 = CARTESIAN_POINT ( 'NONE',  ( 2.273267844204860832, 6.543821324256936300, -3.952852893982225613 ) ) ;
#64419 = FACE_OUTER_BOUND ( 'NONE', #29601, .T. ) ;
#64420 = ORIENTED_EDGE ( 'NONE', *, *, #42375, .F. ) ;
#64421 = ORIENTED_EDGE ( 'NONE', *, *, #38876, .F. ) ;
#64422 = EDGE_CURVE ( 'NONE', #56824, #17810, #26908, .T. ) ;
#64423 = CARTESIAN_POINT ( 'NONE',  ( -37.00000000000000711, 6.547236723514155976, -9.752226076388824438 ) ) ;
#64424 = CARTESIAN_POINT ( 'NONE',  ( 35.00000000000000000, 4.705694406421931860E-17, -3.469127814946512892E-15 ) ) ;
#64425 = ORIENTED_EDGE ( 'NONE', *, *, #61758, .F. ) ;
#64426 = AXIS2_PLACEMENT_3D ( 'NONE', #53741, #8174, #28447 ) ;
#64427 = ORIENTED_EDGE ( 'NONE', *, *, #40752, .F. ) ;
#64428 = FACE_OUTER_BOUND ( 'NONE', #51203, .T. ) ;
#64429 = CARTESIAN_POINT ( 'NONE',  ( -27.08935880048797529, -1.608762129669640606, 1.653090150968469674 ) ) ;
#64430 = CARTESIAN_POINT ( 'NONE',  ( -27.10719052120871098, -2.355164825213512003, 0.1538293304135223694 ) ) ;
#64431 = CARTESIAN_POINT ( 'NONE',  ( -7.389643752995847414, 8.206056478905821905, -10.72177447465196209 ) ) ;
#64432 = DIRECTION ( 'NONE',  ( -1.000000000000000000, 0.000000000000000000, -0.000000000000000000 ) ) ;
#64433 = AXIS2_PLACEMENT_3D ( 'NONE', #34323, #24339, #45601 ) ;
#64434 = DIRECTION ( 'NONE',  ( -1.000000000000000000, 0.000000000000000000, 0.000000000000000000 ) ) ;
#64435 = ORIENTED_EDGE ( 'NONE', *, *, #34750, .F. ) ;
#64436 = DIRECTION ( 'NONE',  ( -1.000000000000000000, 0.000000000000000000, 0.000000000000000000 ) ) ;
#64437 = CARTESIAN_POINT ( 'NONE',  ( 1.719304012338200849, 11.38834240361387096, 5.690355757826642602 ) ) ;
#64438 = CARTESIAN_POINT ( 'NONE',  ( -35.00000000000000000, 6.415447294506704701, 11.01837265713075453 ) ) ;
#64439 = CARTESIAN_POINT ( 'NONE',  ( -35.04660725145885891, 0.003326400506041530918, -0.01184012236748529200 ) ) ;
#64440 = CARTESIAN_POINT ( 'NONE',  ( 0.000000000000000000, -30.50000000000000000, 0.000000000000000000 ) ) ;
#64441 = CARTESIAN_POINT ( 'NONE',  ( 1.020182472824201936, 0.4462553704991011339, -12.48987306958628274 ) ) ;
#64442 = CARTESIAN_POINT ( 'NONE',  ( 37.00000000000000711, 3.033604067594577902, -12.38385022362083454 ) ) ;
#64443 = DIRECTION ( 'NONE',  ( -0.000000000000000000, -0.000000000000000000, -1.000000000000000000 ) ) ;
#64444 = DIRECTION ( 'NONE',  ( 0.000000000000000000, 0.01356324068817992175, -0.9999080150203990547 ) ) ;
#64445 = PRODUCT_DEFINITION ( 'UNKNOWN', '', #3767, #2005 ) ;
#64446 = EDGE_CURVE ( 'NONE', #1625, #64819, #28007, .T. ) ;
#64447 = VERTEX_POINT ( 'NONE', #22421 ) ;
#64448 = CARTESIAN_POINT ( 'NONE',  ( 2.000000000000001776, 0.000000000000000000, 0.000000000000000000 ) ) ;
#64449 = EDGE_CURVE ( 'NONE', #29328, #23145, #62989, .T. ) ;
#64450 =( BOUNDED_SURFACE ( )  B_SPLINE_SURFACE ( 3, 1, ( 
 ( #56887, #11312 ),
 ( #31579, #49523 ),
 ( #27920, #18921 ),
 ( #48228, #13280 ) ),
 .UNSPECIFIED., .F., .F., .F. ) 
 B_SPLINE_SURFACE_WITH_KNOTS ( ( 4, 4 ),
 ( 2, 2 ),
 ( 0.000000000000000000, 1.000000000000000000 ),
 ( 0.000000000000000000, 1.000000000000000000 ),
 .UNSPECIFIED. ) 
 GEOMETRIC_REPRESENTATION_ITEM ( )  RATIONAL_B_SPLINE_SURFACE ( (
 ( 1.000000000000000000, 1.000000000000000000),
 ( 0.6933888150995267674, 0.9895912004443193632),
 ( 0.6933888150995267674, 0.9895912004443193632),
 ( 1.000000000000000000, 1.000000000000000000) ) ) 
 REPRESENTATION_ITEM ( '' )  SURFACE ( )  );
#64451 = ORIENTED_EDGE ( 'NONE', *, *, #52837, .F. ) ;
#64452 = DIRECTION ( 'NONE',  ( 1.000000000000000000, 0.000000000000000000, 0.000000000000000000 ) ) ;
#64453 = CYLINDRICAL_SURFACE ( 'NONE', #42541, 12.18649999999999878 ) ;
#64454 = CYLINDRICAL_SURFACE ( 'NONE', #63238, 12.18649999999999878 ) ;
#64455 = CARTESIAN_POINT ( 'NONE',  ( 0.2650492433740059828, 9.451472485870558771, 7.786978278830003042 ) ) ;
#64456 = CARTESIAN_POINT ( 'NONE',  ( 2.969415267405026704, 5.354299007565745505, 5.777543886622345859 ) ) ;
#64457 = ORIENTED_EDGE ( 'NONE', *, *, #36780, .T. ) ;
#64458 = DIRECTION ( 'NONE',  ( 0.000000000000000000, -1.000000000000000000, 0.000000000000000000 ) ) ;
#64459 = CARTESIAN_POINT ( 'NONE',  ( 145.1370849898475797, 3.309064568108273190E-14, 0.000000000000000000 ) ) ;
#64460 = EDGE_CURVE ( 'NONE', #26477, #6288, #48039, .T. ) ;
#64461 = LINE ( 'NONE', #18930, #46009 ) ;
#64462 = CARTESIAN_POINT ( 'NONE',  ( 0.7400311444011721251, 2.502569705372971409, 12.14938086789863370 ) ) ;
#64463 = CARTESIAN_POINT ( 'NONE',  ( 2.000000000000001776, 4.444115772890121718, 5.163689623839328391 ) ) ;
#64464 =( BOUNDED_SURFACE ( )  B_SPLINE_SURFACE ( 3, 1, ( 
 ( #24992, #46264 ),
 ( #9671, #10332 ),
 ( #705, #30607 ),
 ( #15331, #55898 ) ),
 .UNSPECIFIED., .F., .F., .F. ) 
 B_SPLINE_SURFACE_WITH_KNOTS ( ( 4, 4 ),
 ( 2, 2 ),
 ( 0.000000000000000000, 1.000000000000000000 ),
 ( 0.000000000000000000, 1.000000000000000000 ),
 .UNSPECIFIED. ) 
 GEOMETRIC_REPRESENTATION_ITEM ( )  RATIONAL_B_SPLINE_SURFACE ( (
 ( 1.000000000000000000, 1.000000000000000000),
 ( 0.6933888150995267674, 0.9895912004443193632),
 ( 0.6933888150995267674, 0.9895912004443193632),
 ( 1.000000000000000000, 1.000000000000000000) ) ) 
 REPRESENTATION_ITEM ( '' )  SURFACE ( )  );
#64465 = ORIENTED_EDGE ( 'NONE', *, *, #47388, .T. ) ;
#64466 = LINE ( 'NONE', #24905, #5244 ) ;
#64467 = EDGE_LOOP ( 'NONE', ( #41610, #59718, #22757, #20521 ) ) ;
#64468 = CARTESIAN_POINT ( 'NONE',  ( 2.844750968615307851, 5.783165144077117681, -5.286885609674412123 ) ) ;
#64470 = EDGE_CURVE ( 'NONE', #21573, #35230, #8862, .T. ) ;
#64469 = CARTESIAN_POINT ( 'NONE',  ( 2.242418902651939661, -3.903399295463796825, -6.561482094363286777 ) ) ;
#64471 = EDGE_CURVE ( 'NONE', #17391, #1614, #35381, .T. ) ;
#64472 = CIRCLE ( 'NONE', #61298, 12.18650000000000055 ) ;
#64473 = LINE ( 'NONE', #9264, #16142 ) ;
#64474 = ADVANCED_FACE ( 'NONE', ( #2501 ), #6825, .T. ) ;
#64475 = CARTESIAN_POINT ( 'NONE',  ( 6.776630524595501193, -5.710973591730284404, 12.23820960985696793 ) ) ;
#64476 = ORIENTED_EDGE ( 'NONE', *, *, #11633, .F. ) ;
#64477 = VECTOR ( 'NONE', #24115, 1000.000000000000000 ) ;
#64478 = ORIENTED_EDGE ( 'NONE', *, *, #62262, .T. ) ;
#64479 = CARTESIAN_POINT ( 'NONE',  ( -27.09125059358653331, 2.223272438024538555, -0.6356863790372204726 ) ) ;
#64480 = CARTESIAN_POINT ( 'NONE',  ( 5.516018279890452902, 0.004180585980734981624, 0.005331956019561726046 ) ) ;
#64481 = CARTESIAN_POINT ( 'NONE',  ( 37.00000000000000711, 4.705694406421931860E-17, -3.469127814946512892E-15 ) ) ;
#64482 = LINE ( 'NONE', #14276, #58778 ) ;
#64483 = DIRECTION ( 'NONE',  ( 0.000000000000000000, 0.01356324068817998940, -0.9999080150203989437 ) ) ;
#64484 = CARTESIAN_POINT ( 'NONE',  ( -35.00000000000000000, 2.627174906296914525, 11.44858830469741129 ) ) ;
#64485 = VERTEX_POINT ( 'NONE', #12117 ) ;
#64486 = ORIENTED_EDGE ( 'NONE', *, *, #36752, .F. ) ;
#64487 = ORIENTED_EDGE ( 'NONE', *, *, #65034, .F. ) ;
#64488 = CARTESIAN_POINT ( 'NONE',  ( -22.00000000000000711, -20.00000000000000000, 2.449293598294706907E-15 ) ) ;
#64489 = ADVANCED_FACE ( 'NONE', ( #63308 ), #37726, .T. ) ;
#64490 = CARTESIAN_POINT ( 'NONE',  ( 0.2646305136544072623, -2.256625640822394807, 12.03696649559613974 ) ) ;
#64491 = VERTEX_POINT ( 'NONE', #23415 ) ;
#64492 = CYLINDRICAL_SURFACE ( 'NONE', #39003, 5.000000000000000888 ) ;
#64493 = EDGE_CURVE ( 'NONE', #20149, #30137, #52404, .T. ) ;
#64494 = CYLINDRICAL_SURFACE ( 'NONE', #6678, 6.595312090839647645 ) ;
#64495 = VERTEX_POINT ( 'NONE', #62640 ) ;
#64496 = DIRECTION ( 'NONE',  ( 1.000000000000000000, 0.000000000000000000, 0.000000000000000000 ) ) ;
#64497 = CARTESIAN_POINT ( 'NONE',  ( 3.152665057735194232, -3.161213418914472051, -7.281573230474045921 ) ) ;
#64498 = DIRECTION ( 'NONE',  ( -0.000000000000000000, -0.000000000000000000, -1.000000000000000000 ) ) ;
#64499 = VERTEX_POINT ( 'NONE', #13427 ) ;
#64500 = ORIENTED_EDGE ( 'NONE', *, *, #37462, .T. ) ;
#64501 = CARTESIAN_POINT ( 'NONE',  ( -35.00000000000000000, 2.497432891017006718, -11.47758908105691766 ) ) ;
#64502 = ORIENTED_EDGE ( 'NONE', *, *, #53787, .F. ) ;
#64503 = CARTESIAN_POINT ( 'NONE',  ( 2.000000000000001776, -6.539067737394485214, -2.314222412769890713 ) ) ;
#64504 = ORIENTED_EDGE ( 'NONE', *, *, #7957, .T. ) ;
#64505 = VERTEX_POINT ( 'NONE', #59013 ) ;
#64506 = ORIENTED_EDGE ( 'NONE', *, *, #25777, .T. ) ;
#64507 = DIRECTION ( 'NONE',  ( -1.000000000000000000, 0.000000000000000000, 0.000000000000000000 ) ) ;
#64509 = AXIS2_PLACEMENT_3D ( 'NONE', #40630, #30334, #39652 ) ;
#64508 = CARTESIAN_POINT ( 'NONE',  ( -15.09490394635370336, -34.00569493827350698, -8.490101771330714087 ) ) ;
#64510 = CARTESIAN_POINT ( 'NONE',  ( -22.30398854582848145, 3.656532484463047350, 0.8844201765541789273 ) ) ;
#64511 = CARTESIAN_POINT ( 'NONE',  ( 2.000000000000001776, 0.2704997240205054276, 6.931223712253452796 ) ) ;
#64512 = CARTESIAN_POINT ( 'NONE',  ( -37.00000000000000711, -11.02904044024211849, 4.041347439435823752 ) ) ;
#64513 = ORIENTED_EDGE ( 'NONE', *, *, #16761, .T. ) ;
#64514 = CARTESIAN_POINT ( 'NONE',  ( 38.57634030218385846, -26.62784119520750892, 4.499999999999997335 ) ) ;
#64515 = VECTOR ( 'NONE', #43498, 1000.000000000000000 ) ;
#64516 = EDGE_LOOP ( 'NONE', ( #42951, #55902, #56242, #20221 ) ) ;
#64517 = DIRECTION ( 'NONE',  ( -1.000000000000000000, 0.000000000000000000, -0.000000000000000000 ) ) ;
#64518 = CARTESIAN_POINT ( 'NONE',  ( -17.64417118620952252, -7.220089482685009052, -11.41077800675886245 ) ) ;
#64519 = ORIENTED_EDGE ( 'NONE', *, *, #52622, .T. ) ;
#64520 = CARTESIAN_POINT ( 'NONE',  ( 2.889800649504073782, 6.016320774579824615, -1.129261637821548980 ) ) ;
#64521 = CARTESIAN_POINT ( 'NONE',  ( 37.00000000000000711, -6.564808257521689505, 10.93004082984025160 ) ) ;
#64522 = CARTESIAN_POINT ( 'NONE',  ( 2.305787727787084407, -6.711944854845797614, -3.682701754025583085 ) ) ;
#64523 = AXIS2_PLACEMENT_3D ( 'NONE', #10463, #30738, #51051 ) ;
#64524 = ORIENTED_EDGE ( 'NONE', *, *, #48493, .F. ) ;
#64525 = ORIENTED_EDGE ( 'NONE', *, *, #927, .F. ) ;
#64526 = CIRCLE ( 'NONE', #12360, 4.999999999999999112 ) ;
#64527 = CARTESIAN_POINT ( 'NONE',  ( 2.305787727787084407, -7.654065630109508689, 0.1666591538752418555 ) ) ;
#64528 = ADVANCED_FACE ( 'NONE', ( #3151 ), #17112, .T. ) ;
#64529 = ORIENTED_EDGE ( 'NONE', *, *, #17636, .T. ) ;
#64530 = FACE_OUTER_BOUND ( 'NONE', #61176, .T. ) ;
#64531 = DIRECTION ( 'NONE',  ( -1.000000000000000000, -0.000000000000000000, 0.000000000000000000 ) ) ;
#64532 = CARTESIAN_POINT ( 'NONE',  ( -30.18541646480308671, -0.9647385960114739367, 13.47312881255922257 ) ) ;
#64533 = CARTESIAN_POINT ( 'NONE',  ( 0.3537226245948373315, -9.233810598191725560, -8.088784578751390342 ) ) ;
#64534 = DIRECTION ( 'NONE',  ( 0.000000000000000000, 0.9970832820307041766, 0.07632122047556143263 ) ) ;
#64535 = ORIENTED_EDGE ( 'NONE', *, *, #35011, .F. ) ;
#64536 = CARTESIAN_POINT ( 'NONE',  ( -22.51237073810381162, -3.263711251981912476, -2.986282257334758050 ) ) ;
#64537 = CARTESIAN_POINT ( 'NONE',  ( -30.18541646480390384, -1.416020129149325513, 13.42553116244798517 ) ) ;
#64538 = EDGE_CURVE ( 'NONE', #786, #4699, #34350, .T. ) ;
#64539 = CARTESIAN_POINT ( 'NONE',  ( -14.99915657824959325, -28.92607294587373090, -11.47448459775364604 ) ) ;
#64540 = LINE ( 'NONE', #4728, #61468 ) ;
#64541 = DIRECTION ( 'NONE',  ( -1.000000000000000000, 0.000000000000000000, 0.000000000000000000 ) ) ;
#64542 = CARTESIAN_POINT ( 'NONE',  ( 1.000000000000000888, -7.387287142779349836, 1.295372019972131028 ) ) ;
#64543 = CYLINDRICAL_SURFACE ( 'NONE', #17323, 7.499999999999988454 ) ;
#64544 = AXIS2_PLACEMENT_3D ( 'NONE', #21250, #30894, #25933 ) ;
#64545 = B_SPLINE_CURVE_WITH_KNOTS ( 'NONE', 3,
 ( #59291, #24047, #28056, #7417, #63942, #2465, #13714 ),
 .UNSPECIFIED., .F., .F.,
 ( 4, 3, 4 ),
 ( 0.000000000000000000, 0.001700533616330550564, 0.005002426799371241864 ),
 .UNSPECIFIED. ) ;
#64546 = ORIENTED_EDGE ( 'NONE', *, *, #4648, .T. ) ;
#64547 = CARTESIAN_POINT ( 'NONE',  ( -35.00000000000000000, 12.00000000000000000, 1.469576158976823947E-15 ) ) ;
#64548 = CIRCLE ( 'NONE', #4056, 2.899999999999996358 ) ;
#64549 = ORIENTED_EDGE ( 'NONE', *, *, #19810, .T. ) ;
#64550 = CARTESIAN_POINT ( 'NONE',  ( 22.36482863261543486, 25.00000000000000000, -0.9234811557364158707 ) ) ;
#64551 = CARTESIAN_POINT ( 'NONE',  ( -22.27721701579900682, -3.615531902032089295, 0.6950008646884325847 ) ) ;
#64552 = CARTESIAN_POINT ( 'NONE',  ( 2.507146904658099196, -7.328382489803290767, 2.437115546363195051 ) ) ;
#64553 = CIRCLE ( 'NONE', #22094, 2.899999999999994582 ) ;
#64554 = CARTESIAN_POINT ( 'NONE',  ( 37.00000000000000711, 0.000000000000000000, 0.000000000000000000 ) ) ;
#64555 = ORIENTED_EDGE ( 'NONE', *, *, #16302, .T. ) ;
#64556 = ORIENTED_EDGE ( 'NONE', *, *, #45767, .T. ) ;
#64557 = AXIS2_PLACEMENT_3D ( 'NONE', #16023, #43183, #63456 ) ;
#64558 = EDGE_LOOP ( 'NONE', ( #30061, #18276, #59676, #31212 ) ) ;
#64559 = CARTESIAN_POINT ( 'NONE',  ( 0.2911222467163562255, -7.711756541611626936, -9.524109243548050330 ) ) ;
#64560 = EDGE_CURVE ( 'NONE', #52347, #51211, #32704, .T. ) ;
#64561 = ORIENTED_EDGE ( 'NONE', *, *, #58362, .T. ) ;
#64562 = CARTESIAN_POINT ( 'NONE',  ( 0.000000000000000000, -1.530946385938423582, 7.342084388195347699 ) ) ;
#64563 = DIRECTION ( 'NONE',  ( -1.000000000000000000, 0.000000000000000000, 0.000000000000000000 ) ) ;
#64564 = CARTESIAN_POINT ( 'NONE',  ( 0.2657645697724707046, 10.52916014490830321, 6.253766234003959923 ) ) ;
#64565 = CARTESIAN_POINT ( 'NONE',  ( 21.90174657591892071, 11.97747433400151884, -0.7349207973210698519 ) ) ;
#64566 = ORIENTED_EDGE ( 'NONE', *, *, #34321, .F. ) ;
#64567 = CARTESIAN_POINT ( 'NONE',  ( 2.889800649504073782, 6.121013568931506832, 0.06738247734052546511 ) ) ;
#64568 = DIRECTION ( 'NONE',  ( 0.000000000000000000, 0.01356324068817998940, -0.9999080150203990547 ) ) ;
#64569 = CARTESIAN_POINT ( 'NONE',  ( 37.00000000000000711, -6.891188680298889757, -9.512294188640879611 ) ) ;
#64571 = ORIENTED_EDGE ( 'NONE', *, *, #57858, .F. ) ;
#64570 = DIRECTION ( 'NONE',  ( -1.000000000000000000, 0.000000000000000000, 0.000000000000000000 ) ) ;
#64572 = CARTESIAN_POINT ( 'NONE',  ( 5.515539859299206427, -0.005991790098943843880, 0.0008592514567754646780 ) ) ;
#64573 = EDGE_LOOP ( 'NONE', ( #49740, #47089, #53301, #6909 ) ) ;
#64574 = DIRECTION ( 'NONE',  ( -0.000000000000000000, -0.000000000000000000, -1.000000000000000000 ) ) ;
#64575 = VERTEX_POINT ( 'NONE', #27407 ) ;
#64576 = LINE ( 'NONE', #64271, #707 ) ;
#64577 = CARTESIAN_POINT ( 'NONE',  ( -35.05175862995318425, 0.01253051761585140256, -0.001087818442121676887 ) ) ;
#64578 = CARTESIAN_POINT ( 'NONE',  ( 5.536195898058073439, -0.008071068258923586383, -0.002666509901870041388 ) ) ;
#64579 = DIRECTION ( 'NONE',  ( 0.000000000000000000, 0.000000000000000000, 1.000000000000000000 ) ) ;
#64580 = EDGE_CURVE ( 'NONE', #31862, #21361, #29048, .T. ) ;
#64581 = CARTESIAN_POINT ( 'NONE',  ( 0.2801149460245148104, 9.509848747524184631, 7.723514566794011493 ) ) ;
#64582 = CARTESIAN_POINT ( 'NONE',  ( 2.000000000000001776, -2.480520636974139936, -6.345145617221269241 ) ) ;
#64583 = CARTESIAN_POINT ( 'NONE',  ( 0.000000000000000000, 6.643843315911800218, 1.507714007300793968 ) ) ;
#64585 = ORIENTED_EDGE ( 'NONE', *, *, #35520, .F. ) ;
#64584 = CARTESIAN_POINT ( 'NONE',  ( 10.54028985821272180, 13.47274386308714256, -0.8611671757873611277 ) ) ;
#64586 = B_SPLINE_CURVE_WITH_KNOTS ( 'NONE', 3,
 ( #59000, #18754, #27392, #37712, #58007, #2819, #58675, #47689 ),
 .UNSPECIFIED., .F., .F.,
 ( 4, 2, 2, 4 ),
 ( 4.336808689942017736E-19, 0.002017501633567611672, 0.003026252450351417291, 0.004035003267135222477 ),
 .UNSPECIFIED. ) ;
#64587 = VERTEX_POINT ( 'NONE', #7448 ) ;
#64588 = CIRCLE ( 'NONE', #35910, 7.499999999999988454 ) ;
#64589 = ORIENTED_EDGE ( 'NONE', *, *, #16344, .F. ) ;
#64590 = ORIENTED_EDGE ( 'NONE', *, *, #24570, .T. ) ;
#64591 = CARTESIAN_POINT ( 'NONE',  ( 47.00000000000000711, 4.705694406421931860E-17, -3.469127814946512892E-15 ) ) ;
#64592 = DIRECTION ( 'NONE',  ( 1.000000000000000000, -0.000000000000000000, 0.000000000000000000 ) ) ;
#64593 = DIRECTION ( 'NONE',  ( 0.000000000000000000, -0.9718671068226435450, 0.2355298848897615926 ) ) ;
#64594 = LINE ( 'NONE', #59001, #23589 ) ;
#64595 = CARTESIAN_POINT ( 'NONE',  ( 35.00000000000000000, 0.7008968033240532414, 12.16632754454235332 ) ) ;
#64596 = AXIS2_PLACEMENT_3D ( 'NONE', #6647, #1663, #21611 ) ;
#64597 = CARTESIAN_POINT ( 'NONE',  ( 0.2648978790185584908, 10.67083876753500427, -6.008231198268870976 ) ) ;
#64598 = EDGE_CURVE ( 'NONE', #41782, #16541, #12762, .T. ) ;
#64599 = CARTESIAN_POINT ( 'NONE',  ( -35.00000000000000000, 0.000000000000000000, 0.000000000000000000 ) ) ;
#64600 = AXIS2_PLACEMENT_3D ( 'NONE', #31282, #5033, #61207 ) ;
#64601 = AXIS2_PLACEMENT_3D ( 'NONE', #11119, #62292, #1798 ) ;
#64602 = EDGE_CURVE ( 'NONE', #47144, #18362, #64059, .T. ) ;
#64603 = VERTEX_POINT ( 'NONE', #8131 ) ;
#64604 = FACE_OUTER_BOUND ( 'NONE', #54847, .T. ) ;
#64605 = CARTESIAN_POINT ( 'NONE',  ( 2.249013661412229137, -5.772355099776643961, -5.000301708456380112 ) ) ;
#64606 = AXIS2_PLACEMENT_3D ( 'NONE', #55548, #55206, #30271 ) ;
#64607 = EDGE_CURVE ( 'NONE', #21985, #39116, #28399, .T. ) ;
#64608 = CARTESIAN_POINT ( 'NONE',  ( -17.37148431026360740, -6.070708735758810093, 12.06204800037487246 ) ) ;
#64609 = ORIENTED_EDGE ( 'NONE', *, *, #5223, .T. ) ;
#64610 = CIRCLE ( 'NONE', #35929, 12.18649999999999878 ) ;
#64611 = EDGE_CURVE ( 'NONE', #49200, #2142, #23743, .T. ) ;
#64612 = CARTESIAN_POINT ( 'NONE',  ( -9.378203292903490862, -2.735599985537505940, 13.22402823059322863 ) ) ;
#64613 = EDGE_CURVE ( 'NONE', #57759, #62557, #5709, .T. ) ;
#64614 = CARTESIAN_POINT ( 'NONE',  ( -5.388074842124701114, -1.427462443323999741, 13.42432431655054970 ) ) ;
#64615 = ORIENTED_EDGE ( 'NONE', *, *, #35849, .T. ) ;
#64616 = CYLINDRICAL_SURFACE ( 'NONE', #18151, 12.74999999999999822 ) ;
#64617 = CARTESIAN_POINT ( 'NONE',  ( -37.00000000000000711, 0.000000000000000000, 0.000000000000000000 ) ) ;
#64618 = DIRECTION ( 'NONE',  ( 0.000000000000000000, 0.07632122047556488820, -0.9970832820307038435 ) ) ;
#64619 = CIRCLE ( 'NONE', #43361, 2.899999999999995026 ) ;
#64620 = EDGE_CURVE ( 'NONE', #30956, #22366, #45918, .T. ) ;
#64621 = DIRECTION ( 'NONE',  ( 1.000000000000000000, 0.000000000000000000, 0.000000000000000000 ) ) ;
#64622 = CARTESIAN_POINT ( 'NONE',  ( -37.00000000000000711, 11.78745411414839950, 3.093009498343969099 ) ) ;
#64623 = ORIENTED_EDGE ( 'NONE', *, *, #23404, .F. ) ;
#64624 = CARTESIAN_POINT ( 'NONE',  ( -37.00000000000000711, 0.000000000000000000, 0.000000000000000000 ) ) ;
#64625 = CARTESIAN_POINT ( 'NONE',  ( -9.351388602708162523, -11.42638970207761950, -3.665735721005252135 ) ) ;
#64626 = CARTESIAN_POINT ( 'NONE',  ( 2.000000000000001776, -3.805198749487401777, -5.799611601383285020 ) ) ;
#64627 = ORIENTED_EDGE ( 'NONE', *, *, #16389, .T. ) ;
#64628 = CARTESIAN_POINT ( 'NONE',  ( 21.44698719852729596, 13.04659800062481523, -3.493617502577392120 ) ) ;
#64629 = CYLINDRICAL_SURFACE ( 'NONE', #6551, 12.18650000000000055 ) ;
#64630 = ORIENTED_EDGE ( 'NONE', *, *, #46024, .F. ) ;
#64631 = APPLICATION_CONTEXT ( 'automotive_design' ) ;
#64632 = ORIENTED_EDGE ( 'NONE', *, *, #59206, .T. ) ;
#64633 = DIRECTION ( 'NONE',  ( 1.000000000000000000, 0.000000000000000000, -0.000000000000000000 ) ) ;
#64634 = AXIS2_PLACEMENT_3D ( 'NONE', #33768, #38442, #58758 ) ;
#64635 = EDGE_LOOP ( 'NONE', ( #49672, #32281, #12567, #58453 ) ) ;
#64636 = CARTESIAN_POINT ( 'NONE',  ( 18.98898312442695158, 6.102278294184976914, 12.04338967756598144 ) ) ;
#64637 = CARTESIAN_POINT ( 'NONE',  ( -27.19357181888462094, 10.84410562793473431, 5.138615876886901468 ) ) ;
#64638 = AXIS2_PLACEMENT_3D ( 'NONE', #62743, #52139, #62410 ) ;
#64639 = CARTESIAN_POINT ( 'NONE',  ( -35.00000000000000000, -2.865935305911712749, 12.42372387097881514 ) ) ;
#64640 = CARTESIAN_POINT ( 'NONE',  ( 35.00000000000000000, 4.705694406421931860E-17, -3.469127814946512892E-15 ) ) ;
#64641 =( BOUNDED_SURFACE ( )  B_SPLINE_SURFACE ( 3, 1, ( 
 ( #47677, #52017 ),
 ( #38012, #33023 ),
 ( #32371, #52990 ),
 ( #32041, #37704 ) ),
 .UNSPECIFIED., .F., .F., .F. ) 
 B_SPLINE_SURFACE_WITH_KNOTS ( ( 4, 4 ),
 ( 2, 2 ),
 ( 0.000000000000000000, 1.000000000000000000 ),
 ( 0.000000000000000000, 1.000000000000000000 ),
 .UNSPECIFIED. ) 
 GEOMETRIC_REPRESENTATION_ITEM ( )  RATIONAL_B_SPLINE_SURFACE ( (
 ( 1.000000000000000000, 1.000000000000000000),
 ( 0.9257577194822556033, 0.9980522942447415113),
 ( 0.9257577194822556033, 0.9980522942447415113),
 ( 1.000000000000000000, 1.000000000000000000) ) ) 
 REPRESENTATION_ITEM ( '' )  SURFACE ( )  );
#64642 = CARTESIAN_POINT ( 'NONE',  ( -22.27218376572352554, -3.330959526935390880, -1.571356284315152285 ) ) ;
#64644 = VERTEX_POINT ( 'NONE', #4724 ) ;
#64643 = FACE_OUTER_BOUND ( 'NONE', #48614, .T. ) ;
#64645 = CIRCLE ( 'NONE', #35979, 5.000000000000000000 ) ;
#64646 = PRODUCT_DEFINITION_SHAPE ( 'NONE', 'NONE',  #7550 ) ;
#64647 = FACE_OUTER_BOUND ( 'NONE', #59878, .T. ) ;
#64648 = EDGE_LOOP ( 'NONE', ( #38445, #61268, #14161, #32982 ) ) ;
#64649 = DIRECTION ( 'NONE',  ( -1.000000000000000000, -0.000000000000000000, -0.000000000000000000 ) ) ;
#64650 = ORIENTED_EDGE ( 'NONE', *, *, #34019, .F. ) ;
#64651 = VECTOR ( 'NONE', #56719, 1000.000000000000000 ) ;
#64652 = ORIENTED_EDGE ( 'NONE', *, *, #22036, .F. ) ;
#64653 = CARTESIAN_POINT ( 'NONE',  ( -27.10719052120871098, -2.116547233941210138, -1.044362304621491377 ) ) ;
#64654 = CARTESIAN_POINT ( 'NONE',  ( 3.702144525957873356, -26.71142515285348651, 15.98786919972943288 ) ) ;
#64655 = DIRECTION ( 'NONE',  ( -1.000000000000000000, -0.000000000000000000, -0.000000000000000000 ) ) ;
#64656 = EDGE_CURVE ( 'NONE', #34425, #54645, #35597, .T. ) ;
#64657 = CARTESIAN_POINT ( 'NONE',  ( 24.22861315122816706, -1.970758474066428345, 11.83836876581584185 ) ) ;
#64658 = CARTESIAN_POINT ( 'NONE',  ( 37.00000000000000711, 8.389074212634284322, -8.839356091080075473 ) ) ;
#64659 = CARTESIAN_POINT ( 'NONE',  ( 36.00000000000000711, -6.018036132182079889, 11.24036214326526562 ) ) ;
#64660 = ORIENTED_EDGE ( 'NONE', *, *, #52488, .T. ) ;
#64661 = EDGE_LOOP ( 'NONE', ( #2828, #64042, #28739, #51644 ) ) ;
#64662 = CARTESIAN_POINT ( 'NONE',  ( 5.530133899448235191, -0.01550764871776272834, 0.003876417824003489630 ) ) ;
#64663 = ORIENTED_EDGE ( 'NONE', *, *, #4952, .F. ) ;
#64664 = CARTESIAN_POINT ( 'NONE',  ( 2.000000000000001776, 0.000000000000000000, 0.000000000000000000 ) ) ;
#64665 = CARTESIAN_POINT ( 'NONE',  ( 0.2657645697724694833, -10.52916014490826591, -6.253766234004032754 ) ) ;
#64666 = LINE ( 'NONE', #8842, #45897 ) ;
#64667 = CARTESIAN_POINT ( 'NONE',  ( -36.00000000000000711, 12.63095688309031495, -1.738225594539863472 ) ) ;
#64668 = CARTESIAN_POINT ( 'NONE',  ( 2.350038591458080361, -10.33030559206120813, -2.471682575235316648 ) ) ;
#64669 = AXIS2_PLACEMENT_3D ( 'NONE', #50258, #54901, #45253 ) ;
#64670 = EDGE_CURVE ( 'NONE', #57350, #20149, #17371, .T. ) ;
#64671 = DIRECTION ( 'NONE',  ( -1.000000000000000000, 0.000000000000000000, 0.000000000000000000 ) ) ;
#64672 = ORIENTED_EDGE ( 'NONE', *, *, #35006, .F. ) ;
#64673 = CIRCLE ( 'NONE', #40281, 12.18650000000000055 ) ;
#64674 = EDGE_CURVE ( 'NONE', #63181, #52362, #42841, .T. ) ;
#64675 = ORIENTED_EDGE ( 'NONE', *, *, #54136, .T. ) ;
#64676 = EDGE_CURVE ( 'NONE', #50460, #58025, #39670, .T. ) ;
#64677 = CARTESIAN_POINT ( 'NONE',  ( -27.10719052120871098, 1.310802520592036391, 1.962717903527646079 ) ) ;
#64678 = CARTESIAN_POINT ( 'NONE',  ( 2.844750968616247544, 4.777247819183518374, -6.210802026112414609 ) ) ;
#64679 = CARTESIAN_POINT ( 'NONE',  ( -36.00000000000000711, -3.033604067594665832, 12.38385022362080967 ) ) ;
#64680 = AXIS2_PLACEMENT_3D ( 'NONE', #41161, #40858, #61781 ) ;
#64681 = DIRECTION ( 'NONE',  ( 1.000000000000000000, 0.000000000000000000, -0.000000000000000000 ) ) ;
#64682 = DIRECTION ( 'NONE',  ( 0.000000000000000000, 0.01356324068817998940, -0.9999080150203990547 ) ) ;
#64683 = EDGE_CURVE ( 'NONE', #853, #13869, #5030, .T. ) ;
#64684 = AXIS2_PLACEMENT_3D ( 'NONE', #24569, #23608, #54526 ) ;
#64685 = CARTESIAN_POINT ( 'NONE',  ( -6.614609636016250072, -1.684350297699918286, -11.88140433430720933 ) ) ;
#64686 = EDGE_CURVE ( 'NONE', #21596, #2181, #55571, .T. ) ;
#64687 = DIRECTION ( 'NONE',  ( 1.000000000000000000, 0.000000000000000000, 0.000000000000000000 ) ) ;
#64688 = CARTESIAN_POINT ( 'NONE',  ( 37.00000000000000711, 11.26103545359850955, -3.340853584269734000 ) ) ;
#64689 = CARTESIAN_POINT ( 'NONE',  ( 2.781367136452661537, -5.255136723410572586, -5.783466416658777476 ) ) ;
#64690 = VERTEX_POINT ( 'NONE', #20652 ) ;
#64691 = CARTESIAN_POINT ( 'NONE',  ( -37.00000000000000711, -1.039216533672986387, 11.70009620280411333 ) ) ;
#64692 = CARTESIAN_POINT ( 'NONE',  ( 5.515539859299206427, -0.005618668168217172236, -0.002251761459665588272 ) ) ;
#64693 = B_SPLINE_CURVE_WITH_KNOTS ( 'NONE', 3,
 ( #44260, #64533, #33311, #54900, #63547, #43948, #29305, #49598, #23016, #28322, #33953, #54598, #9324, #39604, #58606, #63887, #64224, #53614, #19338 ),
 .UNSPECIFIED., .F., .F.,
 ( 4, 3, 3, 3, 3, 3, 4 ),
 ( 1.039534490390255925E-17, 4.457896483014696203E-05, 6.639290541541784888E-05, 8.820687556478307243E-05, 0.0001100173248778876675, 0.0001545671401658054074, 0.0001830328308068552429 ),
 .UNSPECIFIED. ) ;
#64694 = CARTESIAN_POINT ( 'NONE',  ( 22.36482863261543486, 13.46837713145128923, -0.9234811557364158707 ) ) ;
#64695 = CIRCLE ( 'NONE', #44527, 12.18650000000000055 ) ;
#64696 = EDGE_CURVE ( 'NONE', #53805, #54601, #51249, .T. ) ;
#64697 = VECTOR ( 'NONE', #36227, 1000.000000000000000 ) ;
#64698 = EDGE_CURVE ( 'NONE', #61317, #49256, #8772, .T. ) ;
#64699 = CARTESIAN_POINT ( 'NONE',  ( -35.00000000000000000, -10.70999494708497046, 5.814360711498253842 ) ) ;
#64700 = CARTESIAN_POINT ( 'NONE',  ( 3.455078800971972619, 8.284346402942340148, 10.65933643386987484 ) ) ;
#64701 = ORIENTED_EDGE ( 'NONE', *, *, #49069, .F. ) ;
#64702 = DIRECTION ( 'NONE',  ( -0.000000000000000000, -1.000000000000000000, -0.000000000000000000 ) ) ;
#64703 = DIRECTION ( 'NONE',  ( 0.000000000000000000, 0.8515178078024850938, -0.5243256840888592674 ) ) ;
#64705 = EDGE_CURVE ( 'NONE', #60283, #32649, #35262, .T. ) ;
#64704 = CARTESIAN_POINT ( 'NONE',  ( -5.261125060311115931, -26.02247534669140094, -15.21511059005040423 ) ) ;
#64706 = VERTEX_POINT ( 'NONE', #40589 ) ;
#64707 = CARTESIAN_POINT ( 'NONE',  ( 37.00000000000000711, 11.74226168163341377, 0.3025107581129941048 ) ) ;
#64708 = DIRECTION ( 'NONE',  ( 0.000000000000000000, -0.4134677391718576955, -0.9105187689795926076 ) ) ;
#64709 = CARTESIAN_POINT ( 'NONE',  ( 18.66452694970452697, -6.623337850070971200, 11.78786257686909700 ) ) ;
#64710 = CARTESIAN_POINT ( 'NONE',  ( 1.020182472820972963, 12.48987306958525068, 0.4462553704978033942 ) ) ;
#64711 = CARTESIAN_POINT ( 'NONE',  ( 3.152665057736013132, 7.281573230473836311, -3.161213418915250095 ) ) ;
#64712 = AXIS2_PLACEMENT_3D ( 'NONE', #36503, #46168, #31507 ) ;
#64713 = DIRECTION ( 'NONE',  ( -1.000000000000000000, 0.000000000000000000, 0.000000000000000000 ) ) ;
#64714 = ORIENTED_EDGE ( 'NONE', *, *, #24260, .T. ) ;
#64715 = CARTESIAN_POINT ( 'NONE',  ( 2.253265082352431836, -7.220580418434031422, 2.491579069691566062 ) ) ;
#64716 = DIRECTION ( 'NONE',  ( 0.000000000000000000, 0.000000000000000000, 1.000000000000000000 ) ) ;
#64717 = CARTESIAN_POINT ( 'NONE',  ( -15.21472318775516008, 8.472363384278436271, -10.51049469413687198 ) ) ;
#64718 = DIRECTION ( 'NONE',  ( 0.9582930651793755139, -0.2568015617827265618, -0.1254087680151175499 ) ) ;
#64719 = DIRECTION ( 'NONE',  ( -0.9582930651793754029, 0.1972632429577076685, -0.2067888154783172894 ) ) ;
#64721 = DIRECTION ( 'NONE',  ( 0.3865475372811021382, 0.9046932595863036441, 0.1791957239473755126 ) ) ;
#64720 = AXIS2_PLACEMENT_3D ( 'NONE', #16544, #46461, #26187 ) ;
#64722 = DIRECTION ( 'NONE',  ( 0.000000000000000000, -0.5767582926624851281, -0.8169148498130359703 ) ) ;
#64723 = CARTESIAN_POINT ( 'NONE',  ( 2.256373768221670684, 1.195444820372209227, -7.545294827889062361 ) ) ;
#64724 = ORIENTED_EDGE ( 'NONE', *, *, #3123, .F. ) ;
#64725 = ORIENTED_EDGE ( 'NONE', *, *, #32374, .F. ) ;
#64726 = CARTESIAN_POINT ( 'NONE',  ( -19.55532226645861726, -4.268374217007646187, -11.21543595443842456 ) ) ;
#64727 = VERTEX_POINT ( 'NONE', #10642 ) ;
#64728 = CIRCLE ( 'NONE', #19140, 12.75000000000000178 ) ;
#64729 = CARTESIAN_POINT ( 'NONE',  ( 35.00000000000000000, 9.913596905230225076, 8.017674001891672120 ) ) ;
#64730 = ADVANCED_FACE ( 'NONE', ( #25971 ), #15324, .T. ) ;
#64731 = EDGE_CURVE ( 'NONE', #18732, #60108, #59907, .T. ) ;
#64732 = CARTESIAN_POINT ( 'NONE',  ( 0.3675815128205912052, -6.367184624550238148, 10.50067073900649461 ) ) ;
#64733 = VERTEX_POINT ( 'NONE', #23763 ) ;
#64734 = DIRECTION ( 'NONE',  ( 1.000000000000000000, -0.000000000000000000, 0.000000000000000000 ) ) ;
#64735 = CARTESIAN_POINT ( 'NONE',  ( -37.00000000000000711, -6.547236723514086698, 9.752226076388870624 ) ) ;
#64736 = CARTESIAN_POINT ( 'NONE',  ( 2.266490820343744605, -5.023127813992656066, -5.760233951938361407 ) ) ;
#64737 = VERTEX_POINT ( 'NONE', #44029 ) ;
#64738 = ORIENTED_EDGE ( 'NONE', *, *, #1799, .F. ) ;
#64739 = CARTESIAN_POINT ( 'NONE',  ( 2.297017764050091948, -7.246120070222743514, -2.462009443075682924 ) ) ;
#64740 = DIRECTION ( 'NONE',  ( 0.000000000000000000, -0.01356324068817992522, 0.9999080150203990547 ) ) ;
#64741 = EDGE_CURVE ( 'NONE', #52228, #27224, #65207, .T. ) ;
#64742 = ORIENTED_EDGE ( 'NONE', *, *, #27782, .T. ) ;
#64743 = CIRCLE ( 'NONE', #13766, 12.15774668701806149 ) ;
#64744 = CARTESIAN_POINT ( 'NONE',  ( 2.000000000000001776, -5.450255447309769963, 4.087611905901399112 ) ) ;
#64745 = ORIENTED_EDGE ( 'NONE', *, *, #16681, .T. ) ;
#64746 = LINE ( 'NONE', #34173, #55374 ) ;
#64747 = CARTESIAN_POINT ( 'NONE',  ( -27.08430792439084556, -1.625846845508331695, 1.614882584890338757 ) ) ;
#64748 = DIRECTION ( 'NONE',  ( -1.000000000000000000, 0.000000000000000000, 0.000000000000000000 ) ) ;
#64749 = DIRECTION ( 'NONE',  ( 0.000000000000000000, 0.9937233664769765662, -0.1118654143051581590 ) ) ;
#64750 = EDGE_CURVE ( 'NONE', #63267, #14741, #21485, .T. ) ;
#64751 = LINE ( 'NONE', #28875, #55654 ) ;
#64752 = VERTEX_POINT ( 'NONE', #62493 ) ;
#64753 = CARTESIAN_POINT ( 'NONE',  ( 2.305787727787084407, 7.654065630109506913, -0.1666591538752953128 ) ) ;
#64754 = CARTESIAN_POINT ( 'NONE',  ( -14.29135464769095520, 7.782112657557433089, 9.134479874907178498 ) ) ;
#64755 = CARTESIAN_POINT ( 'NONE',  ( 2.000000000000001776, -3.786546189469129686, -5.663561025469209476 ) ) ;
#64756 = EDGE_CURVE ( 'NONE', #62968, #14946, #62026, .T. ) ;
#64757 = LINE ( 'NONE', #54493, #52950 ) ;
#64758 = CARTESIAN_POINT ( 'NONE',  ( 9.575800908719084958, 13.45729701195361372, -1.072919909436246266 ) ) ;
#64759 = CARTESIAN_POINT ( 'NONE',  ( -22.38932658256920760, -3.361598243548632237, 2.201197575855957211 ) ) ;
#64760 = DIRECTION ( 'NONE',  ( -1.000000000000000000, -0.000000000000000000, -0.000000000000000000 ) ) ;
#64761 = DIRECTION ( 'NONE',  ( -1.000000000000000000, 0.000000000000000000, 0.000000000000000000 ) ) ;
#64762 = DIRECTION ( 'NONE',  ( 0.000000000000000000, -0.4698238015817425839, -0.8827602140260283337 ) ) ;
#64763 = AXIS2_PLACEMENT_3D ( 'NONE', #37581, #43205, #17302 ) ;
#64764 = AXIS2_PLACEMENT_3D ( 'NONE', #54078, #29444, #8510 ) ;
#64765 = ORIENTED_EDGE ( 'NONE', *, *, #38512, .T. ) ;
#64766 = CARTESIAN_POINT ( 'NONE',  ( 0.2671309869109501078, 0.1620273132355689594, 12.24572650704445032 ) ) ;
#64767 = VERTEX_POINT ( 'NONE', #1357 ) ;
#64768 = DIRECTION ( 'NONE',  ( -1.000000000000000000, 0.000000000000000000, 0.000000000000000000 ) ) ;
#64769 = DIRECTION ( 'NONE',  ( -1.000000000000000000, 0.000000000000000000, 0.000000000000000000 ) ) ;
#64770 = DIRECTION ( 'NONE',  ( 0.000000000000000000, -0.9903235168508535136, -0.1387779952735919697 ) ) ;
#64771 = CARTESIAN_POINT ( 'NONE',  ( -10.90165637462999726, -7.918284569530332107, 10.94501414979677456 ) ) ;
#64772 = DIRECTION ( 'NONE',  ( 0.000000000000000000, 0.04924826701374598187, 0.9987865678893278476 ) ) ;
#64773 = ORIENTED_EDGE ( 'NONE', *, *, #30170, .T. ) ;
#64774 = DIRECTION ( 'NONE',  ( 0.000000000000000000, 1.000000000000000000, 0.000000000000000000 ) ) ;
#64775 = DIRECTION ( 'NONE',  ( -1.000000000000000000, 0.000000000000000000, 0.000000000000000000 ) ) ;
#64776 = CARTESIAN_POINT ( 'NONE',  ( -35.00000000000000000, 0.000000000000000000, 0.000000000000000000 ) ) ;
#64777 = DIRECTION ( 'NONE',  ( 0.000000000000000000, -0.01356324068818000328, 0.9999080150203990547 ) ) ;
#64778 = EDGE_CURVE ( 'NONE', #42091, #25715, #27262, .T. ) ;
#64779 = AXIS2_PLACEMENT_3D ( 'NONE', #17240, #63112, #37844 ) ;
#64780 = EDGE_CURVE ( 'NONE', #25468, #50714, #11318, .T. ) ;
#64781 = CIRCLE ( 'NONE', #11681, 7.938172270156617749 ) ;
#64782 = FACE_OUTER_BOUND ( 'NONE', #38169, .T. ) ;
#64783 = ORIENTED_EDGE ( 'NONE', *, *, #26416, .T. ) ;
#64785 = ADVANCED_FACE ( 'NONE', ( #1020 ), #16638, .T. ) ;
#64784 = CARTESIAN_POINT ( 'NONE',  ( -18.22913673819321190, 11.73512385886278686, 2.593994127463341126 ) ) ;
#64786 = ORIENTED_EDGE ( 'NONE', *, *, #55240, .T. ) ;
#64787 = CARTESIAN_POINT ( 'NONE',  ( 2.297017764050091060, 6.543724852214733545, -3.968300849026689558 ) ) ;
#64788 = DIRECTION ( 'NONE',  ( 0.000000000000000000, 0.6051742151937609115, 0.7960930657056469739 ) ) ;
#64789 = AXIS2_PLACEMENT_3D ( 'NONE', #65396, #29823, #50135 ) ;
#64790 = CARTESIAN_POINT ( 'NONE',  ( 2.990245332647883281, 5.834301250882278467, -6.155689586375134859 ) ) ;
#64791 = DIRECTION ( 'NONE',  ( 0.000000000000000000, -1.000000000000000000, -0.000000000000000000 ) ) ;
#64792 = ORIENTED_EDGE ( 'NONE', *, *, #14322, .F. ) ;
#64793 = VERTEX_POINT ( 'NONE', #47879 ) ;
#64794 = CARTESIAN_POINT ( 'NONE',  ( 35.00000000000000000, 11.50504120060948487, 4.018060380616274685 ) ) ;
#64795 = CIRCLE ( 'NONE', #79, 12.74999999999999822 ) ;
#64796 = DIRECTION ( 'NONE',  ( -1.000000000000000000, 0.000000000000000000, 0.000000000000000000 ) ) ;
#64797 = CARTESIAN_POINT ( 'NONE',  ( 35.00000000000000000, -3.213188559034160452, 11.29812557209479706 ) ) ;
#64798 = CARTESIAN_POINT ( 'NONE',  ( 37.00000000000000711, -2.220215194441986561, -11.98254675519227597 ) ) ;
#64799 = CARTESIAN_POINT ( 'NONE',  ( -35.00000000000000000, -11.71932350927023414, 3.511386971104904386 ) ) ;
#64800 = CARTESIAN_POINT ( 'NONE',  ( 2.000000000000001776, 1.754183803416655474, -6.711026108862266248 ) ) ;
#64801 = CARTESIAN_POINT ( 'NONE',  ( -18.47110435980187049, -11.89396356225322648, 1.625996358069915049 ) ) ;
#64802 = VERTEX_POINT ( 'NONE', #41900 ) ;
#64803 = AXIS2_PLACEMENT_3D ( 'NONE', #28759, #49073, #43061 ) ;
#64804 = ORIENTED_EDGE ( 'NONE', *, *, #41872, .F. ) ;
#64805 = ORIENTED_EDGE ( 'NONE', *, *, #45320, .T. ) ;
#64806 = CARTESIAN_POINT ( 'NONE',  ( -22.51237073810381517, 4.218051923713606932, -1.333315726166068194 ) ) ;
#64807 = DIRECTION ( 'NONE',  ( 0.000000000000000000, -0.000000000000000000, 1.000000000000000000 ) ) ;
#64808 = EDGE_CURVE ( 'NONE', #52522, #31241, #50369, .T. ) ;
#64809 = AXIS2_PLACEMENT_3D ( 'NONE', #36410, #20792, #56359 ) ;
#64810 = AXIS2_PLACEMENT_3D ( 'NONE', #12454, #32726, #48400 ) ;
#64811 = ORIENTED_EDGE ( 'NONE', *, *, #8335, .T. ) ;
#64812 = CARTESIAN_POINT ( 'NONE',  ( 37.00000000000000711, 4.705694406421931860E-17, -3.469127814946512892E-15 ) ) ;
#64813 = CARTESIAN_POINT ( 'NONE',  ( 35.00000000000000000, -2.865935305911542663, 12.42372387097884534 ) ) ;
#64814 = EDGE_CURVE ( 'NONE', #50945, #54151, #36908, .T. ) ;
#64815 = VERTEX_POINT ( 'NONE', #63168 ) ;
#64816 = CARTESIAN_POINT ( 'NONE',  ( 3.100650473569692256, 7.276570693048406646, 3.129198107107961313 ) ) ;
#64817 = LINE ( 'NONE', #9969, #6397 ) ;
#64818 = CARTESIAN_POINT ( 'NONE',  ( 7.195872910760210850, -7.348025474021660841, 9.498045278114711110 ) ) ;
#64819 = VERTEX_POINT ( 'NONE', #37577 ) ;
#64820 = VERTEX_POINT ( 'NONE', #57209 ) ;
#64821 = CARTESIAN_POINT ( 'NONE',  ( 0.3675815128205894289, -7.689697408877210094, -9.574637318042043432 ) ) ;
#64822 = ORIENTED_EDGE ( 'NONE', *, *, #27736, .T. ) ;
#64823 = DIRECTION ( 'NONE',  ( -1.000000000000000000, 0.000000000000000000, 0.000000000000000000 ) ) ;
#64824 = ORIENTED_EDGE ( 'NONE', *, *, #17102, .F. ) ;
#64825 = EDGE_CURVE ( 'NONE', #62364, #40488, #11636, .T. ) ;
#64826 = VERTEX_POINT ( 'NONE', #22265 ) ;
#64827 = ORIENTED_EDGE ( 'NONE', *, *, #29721, .T. ) ;
#64828 = AXIS2_PLACEMENT_3D ( 'NONE', #11424, #36701, #6449 ) ;
#64829 = CARTESIAN_POINT ( 'NONE',  ( 0.2653519991613835782, 11.50013121838207653, 4.209134909048784401 ) ) ;
#64830 = CARTESIAN_POINT ( 'NONE',  ( -22.30625920655495165, 1.076742202099183254, 3.635849356906398544 ) ) ;
#64831 = CARTESIAN_POINT ( 'NONE',  ( -26.43258404273186812, 3.148308537883197200, -1.478864324198215119 ) ) ;
#64832 = DIRECTION ( 'NONE',  ( 0.000000000000000000, -0.07632122047557186872, 0.9970832820307033995 ) ) ;
#64833 = ORIENTED_EDGE ( 'NONE', *, *, #4830, .T. ) ;
#64834 = AXIS2_PLACEMENT_3D ( 'NONE', #63704, #18183, #38451 ) ;
#64835 = CARTESIAN_POINT ( 'NONE',  ( 2.249013661412229581, -7.134443398813858472, -2.724484898587359982 ) ) ;
#64836 = CIRCLE ( 'NONE', #4352, 12.75000000000000178 ) ;
#64837 =( BOUNDED_SURFACE ( )  B_SPLINE_SURFACE ( 3, 1, ( 
 ( #38581, #49240 ),
 ( #42907, #58553 ),
 ( #33262, #33596 ),
 ( #39222, #17975 ) ),
 .UNSPECIFIED., .F., .F., .F. ) 
 B_SPLINE_SURFACE_WITH_KNOTS ( ( 4, 4 ),
 ( 2, 2 ),
 ( 0.000000000000000000, 1.000000000000000000 ),
 ( 0.000000000000000000, 1.000000000000000000 ),
 .UNSPECIFIED. ) 
 GEOMETRIC_REPRESENTATION_ITEM ( )  RATIONAL_B_SPLINE_SURFACE ( (
 ( 1.000000000000000000, 1.000000000000000000),
 ( 0.9942764183789327692, 0.8450855930916585379),
 ( 0.9942764183789327692, 0.8450855930916585379),
 ( 1.000000000000000000, 1.000000000000000000) ) ) 
 REPRESENTATION_ITEM ( '' )  SURFACE ( )  );
#64838 = VERTEX_POINT ( 'NONE', #1689 ) ;
#64839 = DIRECTION ( 'NONE',  ( 1.000000000000000000, 0.000000000000000000, 0.000000000000000000 ) ) ;
#64840 = CARTESIAN_POINT ( 'NONE',  ( -18.12306279865811476, -9.252926135531010843, -9.833831937096134013 ) ) ;
#64841 = VECTOR ( 'NONE', #55127, 1000.000000000000000 ) ;
#64842 = EDGE_CURVE ( 'NONE', #34385, #6738, #10009, .T. ) ;
#64843 = ORIENTED_EDGE ( 'NONE', *, *, #38899, .F. ) ;
#64844 = CARTESIAN_POINT ( 'NONE',  ( 5.514970785353741078, 0.004233694591582955018, 0.002093325033903826408 ) ) ;
#64845 = CARTESIAN_POINT ( 'NONE',  ( -35.00000000000000000, 5.273331777780488672, -10.49591321039675229 ) ) ;
#64846 = CARTESIAN_POINT ( 'NONE',  ( 0.3675815128205894289, -2.391755495700522705, -12.04510820461661780 ) ) ;
#64847 = EDGE_CURVE ( 'NONE', #58835, #17087, #46087, .T. ) ;
#64848 = ORIENTED_EDGE ( 'NONE', *, *, #36104, .T. ) ;
#64849 = EDGE_LOOP ( 'NONE', ( #11751, #20772, #5879, #18617 ) ) ;
#64850 = CARTESIAN_POINT ( 'NONE',  ( 0.7400311444011672402, 6.506979270898180623, 10.56075429936769616 ) ) ;
#64851 = ORIENTED_EDGE ( 'NONE', *, *, #3897, .T. ) ;
#64852 = CARTESIAN_POINT ( 'NONE',  ( 37.00000000000000711, 12.74068829017553917, 0.4871980014161897410 ) ) ;
#64853 = DIRECTION ( 'NONE',  ( 0.000000000000000000, 0.01356324068817998940, -0.9999080150203990547 ) ) ;
#64854 = CARTESIAN_POINT ( 'NONE',  ( -16.12286248669609634, -29.23548504417003713, 10.48934106169928704 ) ) ;
#64856 = CIRCLE ( 'NONE', #13922, 12.73084802173761787 ) ;
#64855 = CARTESIAN_POINT ( 'NONE',  ( 37.00000000000000711, -4.824807283154208370, -11.80185301892979410 ) ) ;
#64857 = CARTESIAN_POINT ( 'NONE',  ( 0.5547464869798233167, -9.256151063740606588, 8.164898018378787370 ) ) ;
#64858 = VERTEX_POINT ( 'NONE', #22616 ) ;
#64859 = CARTESIAN_POINT ( 'NONE',  ( -27.28573687977896611, -1.818142657385560801, 2.255103317860390977 ) ) ;
#64860 = DIRECTION ( 'NONE',  ( 0.000000000000000000, -0.01356324068817992175, 0.9999080150203990547 ) ) ;
#64861 = EDGE_CURVE ( 'NONE', #27211, #31372, #42879, .T. ) ;
#64862 = VECTOR ( 'NONE', #14417, 1000.000000000000000 ) ;
#64863 = CIRCLE ( 'NONE', #21300, 12.18650000000000055 ) ;
#64864 = AXIS2_PLACEMENT_3D ( 'NONE', #5291, #25561, #4654 ) ;
#64865 = EDGE_CURVE ( 'NONE', #30718, #31243, #37584, .T. ) ;
#64866 = CARTESIAN_POINT ( 'NONE',  ( 0.2767916011545406008, -12.09541651105894822, -1.940025653808966410 ) ) ;
#64868 = EDGE_CURVE ( 'NONE', #28939, #1614, #45031, .T. ) ;
#64867 = CARTESIAN_POINT ( 'NONE',  ( 2.899286259009687061, -5.316140236670800157, 5.780956296532494321 ) ) ;
#64869 = FACE_OUTER_BOUND ( 'NONE', #60258, .T. ) ;
#64870 = CARTESIAN_POINT ( 'NONE',  ( 22.88594695219327235, 3.421158645304719137, 13.05931366970166962 ) ) ;
#64871 = FACE_OUTER_BOUND ( 'NONE', #37706, .T. ) ;
#64872 = CIRCLE ( 'NONE', #22408, 2.899999999999995914 ) ;
#64873 = VECTOR ( 'NONE', #28628, 1000.000000000000000 ) ;
#64874 = EDGE_CURVE ( 'NONE', #15355, #18319, #16374, .T. ) ;
#64875 = ORIENTED_EDGE ( 'NONE', *, *, #54038, .T. ) ;
#64876 = CARTESIAN_POINT ( 'NONE',  ( -27.10719052120871098, -1.310802520592025955, -1.962717903527680718 ) ) ;
#64877 = VECTOR ( 'NONE', #62182, 1000.000000000000000 ) ;
#64878 = VECTOR ( 'NONE', #17076, 1000.000000000000000 ) ;
#64879 = ORIENTED_EDGE ( 'NONE', *, *, #44910, .F. ) ;
#64880 = DIRECTION ( 'NONE',  ( -1.000000000000000000, 0.000000000000000000, 0.000000000000000000 ) ) ;
#64881 = DIRECTION ( 'NONE',  ( 1.000000000000000000, 0.000000000000000000, 0.000000000000000000 ) ) ;
#64882 = DIRECTION ( 'NONE',  ( 0.000000000000000000, 0.01356324068817998940, -0.9999080150203989437 ) ) ;
#64883 = AXIS2_PLACEMENT_3D ( 'NONE', #2456, #33355, #44298 ) ;
#64884 = CARTESIAN_POINT ( 'NONE',  ( 2.258463476537672765, -1.192666169131278986, -7.546439757229372880 ) ) ;
#64885 = ORIENTED_EDGE ( 'NONE', *, *, #14260, .T. ) ;
#64886 = CIRCLE ( 'NONE', #37274, 5.000000000000000000 ) ;
#64887 = EDGE_LOOP ( 'NONE', ( #63515, #41934, #8989, #10871 ) ) ;
#64888 = ORIENTED_EDGE ( 'NONE', *, *, #15919, .F. ) ;
#64889 = CARTESIAN_POINT ( 'NONE',  ( 0.2646305136544065406, 7.972778379581675345, -9.296005949277144964 ) ) ;
#64890 = DIRECTION ( 'NONE',  ( 0.000000000000000000, -0.01356324068817991828, 0.9999080150203990547 ) ) ;
#64891 = VERTEX_POINT ( 'NONE', #34139 ) ;
#64892 = DIRECTION ( 'NONE',  ( 1.000000000000000000, 0.000000000000000000, 0.000000000000000000 ) ) ;
#64893 = DIRECTION ( 'NONE',  ( 1.000000000000000000, 0.000000000000000000, 0.000000000000000000 ) ) ;
#64894 = CARTESIAN_POINT ( 'NONE',  ( -36.00000000000000711, -2.250029553613845934, 12.54989509947650284 ) ) ;
#64895 = AXIS2_PLACEMENT_3D ( 'NONE', #32768, #1239, #37453 ) ;
#64896 = DIRECTION ( 'NONE',  ( -1.000000000000000000, 0.000000000000000000, 0.000000000000000000 ) ) ;
#64897 = ADVANCED_FACE ( 'NONE', ( #18568 ), #28837, .T. ) ;
#64898 = ORIENTED_EDGE ( 'NONE', *, *, #10217, .F. ) ;
#64899 = DIRECTION ( 'NONE',  ( 0.000000000000000000, 0.4698238015817303159, 0.8827602140260348840 ) ) ;
#64900 = CARTESIAN_POINT ( 'NONE',  ( -7.049735699849408732, -28.78059498260830651, -12.46475915493682152 ) ) ;
#64901 = CARTESIAN_POINT ( 'NONE',  ( 2.305787727787084407, -1.493241775258372872, -7.508843116234172221 ) ) ;
#64903 = VERTEX_POINT ( 'NONE', #65054 ) ;
#64902 = DIRECTION ( 'NONE',  ( -1.000000000000000000, 0.000000000000000000, -0.000000000000000000 ) ) ;
#64904 = CARTESIAN_POINT ( 'NONE',  ( -35.04660725145885891, 0.007231372203155804479, 0.009947898977290411948 ) ) ;
#64905 = VERTEX_POINT ( 'NONE', #19530 ) ;
#64906 = DIRECTION ( 'NONE',  ( 0.000000000000000000, 0.01356324068817992175, -0.9999080150203990547 ) ) ;
#64907 = ORIENTED_EDGE ( 'NONE', *, *, #32633, .T. ) ;
#64908 = CARTESIAN_POINT ( 'NONE',  ( -36.00000000000000711, 12.70128625845194392, -1.113475361586356627 ) ) ;
#64909 = CARTESIAN_POINT ( 'NONE',  ( 13.37010864853758285, -11.07599950531897370, -4.623143634268777724 ) ) ;
#64910 = CARTESIAN_POINT ( 'NONE',  ( 37.00000000000000711, 4.705694406421931860E-17, -3.469127814946512892E-15 ) ) ;
#64911 = CARTESIAN_POINT ( 'NONE',  ( 35.00000000000000000, 4.705694406421931860E-17, -3.469127814946512892E-15 ) ) ;
#64912 = AXIS2_PLACEMENT_3D ( 'NONE', #52798, #43131, #7229 ) ;
#64913 = CIRCLE ( 'NONE', #31976, 5.000000000000000888 ) ;
#64914 = EDGE_CURVE ( 'NONE', #29381, #19030, #18316, .T. ) ;
#64916 = VECTOR ( 'NONE', #27753, 999.9999999999998863 ) ;
#64915 = CARTESIAN_POINT ( 'NONE',  ( 0.3474126878361796789, -12.27082419038178784, 0.2587235634077604818 ) ) ;
#64917 = CARTESIAN_POINT ( 'NONE',  ( -27.09729107899852352, -0.1622107421537205552, -2.324833743198346347 ) ) ;
#64918 = CARTESIAN_POINT ( 'NONE',  ( 0.3401186441510197223, -3.955862996551428257, -11.61600526280575707 ) ) ;
#64920 = VERTEX_POINT ( 'NONE', #45118 ) ;
#64919 = CARTESIAN_POINT ( 'NONE',  ( -27.35552965826136429, -2.810569013793742688, 1.320216934008381804 ) ) ;
#64921 = VERTEX_POINT ( 'NONE', #60082 ) ;
#64922 = CARTESIAN_POINT ( 'NONE',  ( 0.000000000000000000, 6.338823199656720142, -2.816798305433633853 ) ) ;
#64923 = EDGE_LOOP ( 'NONE', ( #36112, #27802, #44373, #49741 ) ) ;
#64924 = ADVANCED_FACE ( 'NONE', ( #9512 ), #8886, .T. ) ;
#64925 = ORIENTED_EDGE ( 'NONE', *, *, #26145, .T. ) ;
#64926 = LINE ( 'NONE', #20048, #1832 ) ;
#64927 = FACE_OUTER_BOUND ( 'NONE', #38695, .T. ) ;
#64928 = CYLINDRICAL_SURFACE ( 'NONE', #11938, 12.18650000000000055 ) ;
#64930 = CIRCLE ( 'NONE', #55395, 5.000000000000000888 ) ;
#64929 = CARTESIAN_POINT ( 'NONE',  ( 3.152665057735760445, 4.725420687649616092, -6.378477742801607953 ) ) ;
#64931 = ADVANCED_FACE ( 'NONE', ( #54457 ), #3606, .T. ) ;
#64932 = AXIS2_PLACEMENT_3D ( 'NONE', #41908, #6348, #41574 ) ;
#64933 = CARTESIAN_POINT ( 'NONE',  ( 0.000000000000000000, -5.097042323172408906, -5.501832381651512449 ) ) ;
#64934 = CYLINDRICAL_SURFACE ( 'NONE', #49207, 12.18650000000000055 ) ;
#64935 = CIRCLE ( 'NONE', #33083, 4.999999999999998224 ) ;
#64936 = ORIENTED_EDGE ( 'NONE', *, *, #56867, .F. ) ;
#64937 = CARTESIAN_POINT ( 'NONE',  ( 2.000000000000001776, 3.979254915827366901, 5.681598592373755530 ) ) ;
#64938 = AXIS2_PLACEMENT_3D ( 'NONE', #50946, #10686, #20988 ) ;
#64939 = DIRECTION ( 'NONE',  ( 1.000000000000000000, -0.000000000000000000, 0.000000000000000000 ) ) ;
#64940 = CARTESIAN_POINT ( 'NONE',  ( 0.2648978790185584908, -7.769924372105139199, -9.465406350830686932 ) ) ;
#64941 = ORIENTED_EDGE ( 'NONE', *, *, #37851, .T. ) ;
#64942 = CIRCLE ( 'NONE', #19305, 4.999999999999999112 ) ;
#64943 = EDGE_CURVE ( 'NONE', #6133, #59647, #8910, .T. ) ;
#64944 = CIRCLE ( 'NONE', #27797, 5.000000000000001776 ) ;
#64945 = CARTESIAN_POINT ( 'NONE',  ( 40.19089168456218175, -1.800105668799817593, -19.87241647152735169 ) ) ;
#64946 = CARTESIAN_POINT ( 'NONE',  ( -5.795121526828563852, -1.480313353269908649, 13.41892790137997338 ) ) ;
#64947 = CIRCLE ( 'NONE', #36287, 6.936499999999991672 ) ;
#64948 = ORIENTED_EDGE ( 'NONE', *, *, #28508, .T. ) ;
#64949 = CARTESIAN_POINT ( 'NONE',  ( 0.2648978790185584908, 2.256510822326303956, -12.03635331166809941 ) ) ;
#64950 = CARTESIAN_POINT ( 'NONE',  ( 0.2638984909335720941, -11.43908195192332578, 4.375449752477094556 ) ) ;
#64951 = DIRECTION ( 'NONE',  ( 0.000000000000000000, -0.8827602140260265573, 0.4698238015817460256 ) ) ;
#64952 = B_SPLINE_CURVE_WITH_KNOTS ( 'NONE', 3,
 ( #61596, #46645, #41977, #30679, #47321, #1767, #56287, #22025, #771, #461, #31992, #21033, #52313, #16401, #46331, #60969, #36981, #46985, #20728 ),
 .UNSPECIFIED., .F., .F.,
 ( 4, 3, 3, 3, 3, 3, 4 ),
 ( 9.550984261304515293E-18, 4.457896483014562033E-05, 6.639290541541465049E-05, 8.820687556478086337E-05, 0.0001100173248778839812, 0.0001545671401658083347, 0.0001830328308068577365 ),
 .UNSPECIFIED. ) ;
#64953 = B_SPLINE_CURVE_WITH_KNOTS ( 'NONE', 3,
 ( #51537, #36541, #27216, #62447, #47831, #42827, #22567, #52175, #15908, #41507, #56848, #26893, #47509, #5982, #22221, #37521, #32509, #42481, #62780, #17246 ),
 .UNSPECIFIED., .F., .F.,
 ( 4, 2, 2, 2, 2, 2, 2, 2, 2, 4 ),
 ( 0.000000000000000000, 0.001212774353530760669, 0.002425548707061521338, 0.003638323060592281357, 0.004244710237357661800, 0.004851097414123040942, 0.006063871767653796624, 0.007276646121184551438, 0.008489420474715306253, 0.009702194828246061067 ),
 .UNSPECIFIED. ) ;
#64954 = ADVANCED_FACE ( 'NONE', ( #4570 ), #29802, .T. ) ;
#64955 = AXIS2_PLACEMENT_3D ( 'NONE', #32419, #26791, #18128 ) ;
#64956 = VECTOR ( 'NONE', #741, 1000.000000000000000 ) ;
#64957 = CIRCLE ( 'NONE', #22502, 2.899999999999994582 ) ;
#64958 = DIRECTION ( 'NONE',  ( 0.000000000000000000, 0.9987865678893277366, -0.04924826701374931254 ) ) ;
#64959 = CARTESIAN_POINT ( 'NONE',  ( 2.000000000000001776, 0.000000000000000000, 0.000000000000000000 ) ) ;
#64960 = EDGE_LOOP ( 'NONE', ( #37676, #52830, #46375, #43751 ) ) ;
#64961 = DIRECTION ( 'NONE',  ( 1.000000000000000000, -0.000000000000000000, 0.000000000000000000 ) ) ;
#64962 = CARTESIAN_POINT ( 'NONE',  ( -8.806666233050373549, -7.414420935576055527, -9.443457017163492395 ) ) ;
#64963 = CARTESIAN_POINT ( 'NONE',  ( -18.36540788822463099, 3.954298550336713181, -11.33046690914046195 ) ) ;
#64964 = ORIENTED_EDGE ( 'NONE', *, *, #31128, .F. ) ;
#64965 = DIRECTION ( 'NONE',  ( -1.000000000000000000, 0.000000000000000000, 0.000000000000000000 ) ) ;
#64966 = CARTESIAN_POINT ( 'NONE',  ( -37.00000000000000711, 12.66641127287626034, 1.457575200925590453 ) ) ;
#64967 = ORIENTED_EDGE ( 'NONE', *, *, #29345, .F. ) ;
#64968 = ORIENTED_EDGE ( 'NONE', *, *, #35880, .T. ) ;
#64969 = ORIENTED_EDGE ( 'NONE', *, *, #43492, .F. ) ;
#64970 = CARTESIAN_POINT ( 'NONE',  ( -37.00000000000000711, -0.7536123767499333104, 11.72195762423409704 ) ) ;
#64971 = VECTOR ( 'NONE', #65764, 1000.000000000000000 ) ;
#64972 = AXIS2_PLACEMENT_3D ( 'NONE', #28578, #64163, #48882 ) ;
#64973 = EDGE_LOOP ( 'NONE', ( #45179, #39369, #51530, #1451 ) ) ;
#64974 = AXIS2_PLACEMENT_3D ( 'NONE', #61595, #41312, #31662 ) ;
#64975 = DIRECTION ( 'NONE',  ( 1.000000000000000000, 0.000000000000000000, 0.000000000000000000 ) ) ;
#64976 = DIRECTION ( 'NONE',  ( -1.000000000000000000, 0.000000000000000000, 0.000000000000000000 ) ) ;
#64977 = CARTESIAN_POINT ( 'NONE',  ( 0.3106921474978425746, -6.333448016104122225, 10.49891314301084044 ) ) ;
#64978 = CARTESIAN_POINT ( 'NONE',  ( 0.2653519890518162283, 4.188437879978412326, -11.50766430042464883 ) ) ;
#64979 = EDGE_CURVE ( 'NONE', #239, #65794, #30195, .T. ) ;
#64980 = VECTOR ( 'NONE', #36626, 1000.000000000000000 ) ;
#64981 = CARTESIAN_POINT ( 'NONE',  ( 0.3632410797595258534, -10.76277061791635958, -5.910360611678935783 ) ) ;
#64982 = CARTESIAN_POINT ( 'NONE',  ( 2.241531873784868623, 0.01153688368842444717, 7.634454672504356054 ) ) ;
#64984 = VERTEX_POINT ( 'NONE', #14187 ) ;
#64983 = CARTESIAN_POINT ( 'NONE',  ( 2.241451721903215510, -7.634225434981129155, -0.06083185034804090840 ) ) ;
#64985 = EDGE_CURVE ( 'NONE', #23007, #4893, #34476, .T. ) ;
#64986 = CARTESIAN_POINT ( 'NONE',  ( 0.2646305136544065406, 9.296005949277226676, 7.972778379581582975 ) ) ;
#64987 = EDGE_LOOP ( 'NONE', ( #30026, #46602, #16014, #10537 ) ) ;
#64988 = FACE_OUTER_BOUND ( 'NONE', #21073, .T. ) ;
#64989 = AXIS2_PLACEMENT_3D ( 'NONE', #26189, #46463, #11535 ) ;
#64990 = ORIENTED_EDGE ( 'NONE', *, *, #16472, .T. ) ;
#64991 = ORIENTED_EDGE ( 'NONE', *, *, #32785, .T. ) ;
#64992 = CARTESIAN_POINT ( 'NONE',  ( -22.27706089016750113, -0.9798385173596184661, 3.548384797797526691 ) ) ;
#64993 = CARTESIAN_POINT ( 'NONE',  ( -6.778443870680312067, -27.08263571440717854, 15.40204062588007616 ) ) ;
#64994 = CARTESIAN_POINT ( 'NONE',  ( -35.04709527796842394, 0.01016988845958452514, 0.007030359780618375409 ) ) ;
#64995 = EDGE_CURVE ( 'NONE', #48418, #52930, #14212, .T. ) ;
#64996 = FACE_OUTER_BOUND ( 'NONE', #54534, .T. ) ;
#64997 = DIRECTION ( 'NONE',  ( -1.000000000000000000, -0.000000000000000000, 0.000000000000000000 ) ) ;
#64998 = CARTESIAN_POINT ( 'NONE',  ( 2.244591118395373286, 5.917635828472982418, 4.825158615935962736 ) ) ;
#64999 = EDGE_LOOP ( 'NONE', ( #10680, #56436, #18356, #46290 ) ) ;
#65000 = ORIENTED_EDGE ( 'NONE', *, *, #36157, .F. ) ;
#65001 = DIRECTION ( 'NONE',  ( 0.000000000000000000, 0.9635499925192236859, -0.2675283385292184235 ) ) ;
#65002 = ORIENTED_EDGE ( 'NONE', *, *, #31916, .F. ) ;
#65003 = ADVANCED_FACE ( 'NONE', ( #51442 ), #40788, .T. ) ;
#65004 = ORIENTED_EDGE ( 'NONE', *, *, #10550, .F. ) ;
#65006 = CIRCLE ( 'NONE', #7688, 12.18649999999999878 ) ;
#65005 = CARTESIAN_POINT ( 'NONE',  ( 2.247112776671468470, -7.499199956302002867, 1.440655381229448029 ) ) ;
#65007 = CARTESIAN_POINT ( 'NONE',  ( -22.27878402819508352, 0.9457981527432597346, -3.562981801125743697 ) ) ;
#65008 = CARTESIAN_POINT ( 'NONE',  ( 0.7400311444011681283, -12.14938086789864258, 2.502569705372930109 ) ) ;
#65009 = CARTESIAN_POINT ( 'NONE',  ( -22.27720387087365239, 1.337073746937897711, -3.430312021254875443 ) ) ;
#65010 = CIRCLE ( 'NONE', #7693, 2.899999999999995026 ) ;
#65011 = DIRECTION ( 'NONE',  ( -1.000000000000000000, 0.000000000000000000, 0.000000000000000000 ) ) ;
#65012 = CARTESIAN_POINT ( 'NONE',  ( 26.73057806998188468, -13.02598523147789678, 3.554326270227990303 ) ) ;
#65013 = ORIENTED_EDGE ( 'NONE', *, *, #12286, .T. ) ;
#65014 = ORIENTED_EDGE ( 'NONE', *, *, #10293, .T. ) ;
#65015 = CARTESIAN_POINT ( 'NONE',  ( 2.080613030138687147, 0.000000000000000000, 0.000000000000000000 ) ) ;
#65016 = DIRECTION ( 'NONE',  ( 0.000000000000000000, 0.8369827122275325104, 0.5472293298355300761 ) ) ;
#65017 = CARTESIAN_POINT ( 'NONE',  ( 37.00000000000000711, 4.705694406421931860E-17, -3.469127814946512892E-15 ) ) ;
#65018 = CIRCLE ( 'NONE', #58700, 12.18650000000000055 ) ;
#65019 = AXIS2_PLACEMENT_3D ( 'NONE', #39289, #53293, #64241 ) ;
#65020 = FACE_OUTER_BOUND ( 'NONE', #49948, .T. ) ;
#65021 = FACE_OUTER_BOUND ( 'NONE', #25473, .T. ) ;
#65022 = B_SPLINE_CURVE_WITH_KNOTS ( 'NONE', 3,
 ( #53396, #12805, #41181, #27135, #35852, #56152, #10595, #5647, #46204, #11823, #32106, #52423, #1867, #42391, #49711, #44064, #44369, #23453, #53726, #18802, #24422, #8819 ),
 .UNSPECIFIED., .F., .F.,
 ( 4, 3, 3, 3, 3, 3, 3, 4 ),
 ( 0.000000000000000000, 6.990956068646337414E-05, 0.0001398191187764040878, 0.0002097286751720215986, 0.0002796382307041359386, 0.0003495477861619810745, 0.0004194573423310289542, 0.0005586102576333142793 ),
 .UNSPECIFIED. ) ;
#65023 = AXIS2_PLACEMENT_3D ( 'NONE', #5730, #10679, #51928 ) ;
#65024 = CARTESIAN_POINT ( 'NONE',  ( 6.305306969373864590, -9.257074684086198602, -9.828058395331741082 ) ) ;
#65025 = CARTESIAN_POINT ( 'NONE',  ( 2.241506898688419902, 5.822995664778323643, -4.937416071751777658 ) ) ;
#65026 = CARTESIAN_POINT ( 'NONE',  ( 5.530133899448235191, -0.003876417824003551213, 0.01550764871776215414 ) ) ;
#65027 = DIRECTION ( 'NONE',  ( 0.000000000000000000, 0.01356324068817998940, -0.9999080150203990547 ) ) ;
#65028 = ORIENTED_EDGE ( 'NONE', *, *, #26273, .F. ) ;
#65029 = APPLICATION_CONTEXT ( 'automotive_design' ) ;
#65030 = CARTESIAN_POINT ( 'NONE',  ( 2.907497136249938663, -6.243048412628442456, -4.769582063554289597 ) ) ;
#65031 = CARTESIAN_POINT ( 'NONE',  ( 2.000000000000001776, -6.643843315911820646, 1.507714007300648307 ) ) ;
#65032 = DIRECTION ( 'NONE',  ( 0.000000000000000000, 0.8369827122275362852, 0.5472293298355244140 ) ) ;
#65033 = ADVANCED_BREP_SHAPE_REPRESENTATION ( '', ( #30113, #24966 ), #7986 ) ;
#65034 = EDGE_CURVE ( 'NONE', #11018, #28687, #6411, .T. ) ;
#65035 = CARTESIAN_POINT ( 'NONE',  ( -6.008663266769909583, -31.76136623419866822, -13.60005156547899041 ) ) ;
#65036 = CARTESIAN_POINT ( 'NONE',  ( 2.290907136833251201, -5.963935563308454313, 4.792500160339664639 ) ) ;
#65037 =( BOUNDED_SURFACE ( )  B_SPLINE_SURFACE ( 3, 1, ( 
 ( #15012, #45958 ),
 ( #413, #20682 ),
 ( #35939, #51286 ),
 ( #5736, #21677 ) ),
 .UNSPECIFIED., .F., .F., .F. ) 
 B_SPLINE_SURFACE_WITH_KNOTS ( ( 4, 4 ),
 ( 2, 2 ),
 ( 0.000000000000000000, 1.000000000000000000 ),
 ( 0.000000000000000000, 1.000000000000000000 ),
 .UNSPECIFIED. ) 
 GEOMETRIC_REPRESENTATION_ITEM ( )  RATIONAL_B_SPLINE_SURFACE ( (
 ( 1.000000000000000000, 1.000000000000000000),
 ( 0.9942764183789327692, 0.8450855930916585379),
 ( 0.9942764183789327692, 0.8450855930916585379),
 ( 1.000000000000000000, 1.000000000000000000) ) ) 
 REPRESENTATION_ITEM ( '' )  SURFACE ( )  );
#65038 = ORIENTED_EDGE ( 'NONE', *, *, #49618, .F. ) ;
#65039 = CARTESIAN_POINT ( 'NONE',  ( 2.260457164927185847, -2.482766715766957510, 7.226149053012477452 ) ) ;
#65040 = CARTESIAN_POINT ( 'NONE',  ( 2.963017218115493012, 6.619413971958212350, 4.265970453343873814 ) ) ;
#65041 = CARTESIAN_POINT ( 'NONE',  ( -6.641947195041168150, -28.39580239767160919, -11.12859478088952336 ) ) ;
#65042 = ORIENTED_EDGE ( 'NONE', *, *, #29690, .T. ) ;
#65043 = CARTESIAN_POINT ( 'NONE',  ( 37.00000000000000711, 4.705694406421931860E-17, -3.469127814946512892E-15 ) ) ;
#65044 = CARTESIAN_POINT ( 'NONE',  ( -27.45775109278350712, -13.35262336282553441, -1.989333891161978674 ) ) ;
#65045 = FACE_OUTER_BOUND ( 'NONE', #3185, .T. ) ;
#65046 = VECTOR ( 'NONE', #26973, 1000.000000000000000 ) ;
#65047 = LINE ( 'NONE', #19524, #15842 ) ;
#65048 = CARTESIAN_POINT ( 'NONE',  ( -27.08429572838383947, 2.208905845566027537, 0.6096735944847788691 ) ) ;
#65049 = CIRCLE ( 'NONE', #35340, 2.899999999999995026 ) ;
#65050 = CIRCLE ( 'NONE', #35341, 5.000000000000000000 ) ;
#65051 = EDGE_CURVE ( 'NONE', #34193, #3983, #33361, .T. ) ;
#65052 = CARTESIAN_POINT ( 'NONE',  ( 1.194176325881335154, 12.26540585042612719, -2.684784923266161361 ) ) ;
#65053 = EDGE_LOOP ( 'NONE', ( #4958, #59243, #49339, #55789 ) ) ;
#65054 = CARTESIAN_POINT ( 'NONE',  ( -35.00000000000000000, 7.110831038798278492, 9.896810808925417646 ) ) ;
#65055 = CARTESIAN_POINT ( 'NONE',  ( -8.502077647541781857, 10.07266980514430621, -8.994062260280561105 ) ) ;
#65056 = DIRECTION ( 'NONE',  ( -1.000000000000000000, 0.000000000000000000, 0.000000000000000000 ) ) ;
#65057 = CARTESIAN_POINT ( 'NONE',  ( 37.00000000000000711, 4.339012074899953220, -10.91536515067649660 ) ) ;
#65058 = CARTESIAN_POINT ( 'NONE',  ( 2.259830038565000088, 7.547174990768423797, -1.190932096469573320 ) ) ;
#65059 = DIRECTION ( 'NONE',  ( -1.000000000000000000, 0.000000000000000000, 0.000000000000000000 ) ) ;
#65060 = EDGE_CURVE ( 'NONE', #53158, #29384, #6803, .T. ) ;
#65061 = CARTESIAN_POINT ( 'NONE',  ( -27.35552965826137140, 2.810569013793760007, -1.320216934008374920 ) ) ;
#65062 = LINE ( 'NONE', #5897, #1103 ) ;
#65063 = VERTEX_POINT ( 'NONE', #36446 ) ;
#65064 = ADVANCED_FACE ( 'NONE', ( #228 ), #54380, .F. ) ;
#65065 = ORIENTED_EDGE ( 'NONE', *, *, #5727, .T. ) ;
#65066 = CARTESIAN_POINT ( 'NONE',  ( -18.03417828546679047, -5.815239346579785362, -10.49772883765438358 ) ) ;
#65067 = AXIS2_PLACEMENT_3D ( 'NONE', #4725, #45258, #24310 ) ;
#65068 = VERTEX_POINT ( 'NONE', #35762 ) ;
#65069 = AXIS2_PLACEMENT_3D ( 'NONE', #56837, #12234, #52161 ) ;
#65070 = LINE ( 'NONE', #23885, #14120 ) ;
#65071 = ADVANCED_FACE ( 'NONE', ( #51098 ), #5554, .T. ) ;
#65072 = DIRECTION ( 'NONE',  ( -0.000000000000000000, -1.000000000000000000, -0.000000000000000000 ) ) ;
#65073 = ORIENTED_EDGE ( 'NONE', *, *, #36858, .T. ) ;
#65074 = DIRECTION ( 'NONE',  ( 0.000000000000000000, -0.01356324068817998940, 0.9999080150203990547 ) ) ;
#65075 = CARTESIAN_POINT ( 'NONE',  ( 9.575800908719084958, 11.95193887484099093, -1.072919909436247154 ) ) ;
#65077 = EDGE_CURVE ( 'NONE', #24451, #24519, #65204, .T. ) ;
#65076 = CARTESIAN_POINT ( 'NONE',  ( 24.66186213270750116, -2.307346164574797687, 13.30714139060018653 ) ) ;
#65078 = ORIENTED_EDGE ( 'NONE', *, *, #56796, .F. ) ;
#65079 = VECTOR ( 'NONE', #6076, 1000.000000000000000 ) ;
#65080 = ORIENTED_EDGE ( 'NONE', *, *, #53469, .T. ) ;
#65081 = CARTESIAN_POINT ( 'NONE',  ( 3.047904605210431939, 0.4249306449416465070, -7.891858004695958329 ) ) ;
#65082 = ORIENTED_EDGE ( 'NONE', *, *, #11450, .F. ) ;
#65083 = CARTESIAN_POINT ( 'NONE',  ( 4.481592184329596940, -10.18497286202598318, -6.347143897620531661 ) ) ;
#65084 = ORIENTED_EDGE ( 'NONE', *, *, #49946, .T. ) ;
#65085 = CYLINDRICAL_SURFACE ( 'NONE', #42622, 5.000000000000000888 ) ;
#65086 = CARTESIAN_POINT ( 'NONE',  ( -28.41827485489077532, 3.509237424706437292, 11.47541949982830722 ) ) ;
#65087 = CARTESIAN_POINT ( 'NONE',  ( 2.000000000000001776, 0.000000000000000000, 0.000000000000000000 ) ) ;
#65088 = CARTESIAN_POINT ( 'NONE',  ( -14.29135464769095520, 7.782112657557433977, 11.03126115115966499 ) ) ;
#65089 = AXIS2_PLACEMENT_3D ( 'NONE', #40955, #61547, #45604 ) ;
#65090 = EDGE_CURVE ( 'NONE', #45080, #47268, #19844, .T. ) ;
#65091 = CARTESIAN_POINT ( 'NONE',  ( 2.000000000000001776, -2.469490258309361419, -6.482025155313371201 ) ) ;
#65092 = ORIENTED_EDGE ( 'NONE', *, *, #37797, .T. ) ;
#65093 = CARTESIAN_POINT ( 'NONE',  ( 2.247112776671467582, 7.635437439951565430, -0.1165461824817972114 ) ) ;
#65094 = CARTESIAN_POINT ( 'NONE',  ( -35.00000000000000000, 0.000000000000000000, 0.000000000000000000 ) ) ;
#65095 = EDGE_CURVE ( 'NONE', #8838, #26102, #36092, .T. ) ;
#65096 = CARTESIAN_POINT ( 'NONE',  ( 1.719304012340734378, -11.38834240361519612, -5.690355757825884986 ) ) ;
#65097 = DIRECTION ( 'NONE',  ( 0.000000000000000000, 0.01356324068817992175, -0.9999080150203990547 ) ) ;
#65099 = CARTESIAN_POINT ( 'NONE',  ( -18.57917586897355378, 13.44592621184941805, 1.251652577239034558 ) ) ;
#65098 = AXIS2_PLACEMENT_3D ( 'NONE', #65459, #23618, #44520 ) ;
#65100 = CARTESIAN_POINT ( 'NONE',  ( 24.39670892413253256, -1.088878361238891923, 13.46081842674021090 ) ) ;
#65101 = CYLINDRICAL_SURFACE ( 'NONE', #4357, 2.899999999999994582 ) ;
#65102 = DIRECTION ( 'NONE',  ( 0.000000000000000000, 0.5767582926624911233, 0.8169148498130317515 ) ) ;
#65103 = VECTOR ( 'NONE', #50127, 1000.000000000000000 ) ;
#65104 = DIRECTION ( 'NONE',  ( -0.000000000000000000, -0.000000000000000000, -1.000000000000000000 ) ) ;
#65105 = CIRCLE ( 'NONE', #53456, 12.18650000000000055 ) ;
#65106 = AXIS2_PLACEMENT_3D ( 'NONE', #16250, #62437, #36534 ) ;
#65107 = ORIENTED_EDGE ( 'NONE', *, *, #45580, .F. ) ;
#65108 = CARTESIAN_POINT ( 'NONE',  ( 1.937114397841935398, -10.63710405811938742, 7.182898292393728568 ) ) ;
#65109 = VERTEX_POINT ( 'NONE', #5890 ) ;
#65110 = CARTESIAN_POINT ( 'NONE',  ( 2.305787727787083519, 5.970480882365222897, 4.792270232040915623 ) ) ;
#65111 = CARTESIAN_POINT ( 'NONE',  ( 35.00000000000000000, -11.26103545359853264, 3.340853584269647847 ) ) ;
#65112 = LINE ( 'NONE', #8946, #36711 ) ;
#65113 = VECTOR ( 'NONE', #35587, 1000.000000000000000 ) ;
#65114 = CARTESIAN_POINT ( 'NONE',  ( 0.2651627682582914924, -12.04449770099952843, 2.213224986694545038 ) ) ;
#65115 = CARTESIAN_POINT ( 'NONE',  ( 0.3665391374699472626, -4.447929964102772082, -11.44911061034390976 ) ) ;
#65116 = ORIENTED_EDGE ( 'NONE', *, *, #61641, .F. ) ;
#65117 = VECTOR ( 'NONE', #20224, 1000.000000000000000 ) ;
#65118 = DIRECTION ( 'NONE',  ( 1.000000000000000000, 0.000000000000000000, -0.000000000000000000 ) ) ;
#65119 = CARTESIAN_POINT ( 'NONE',  ( -37.00000000000000711, 2.936739658820028520, -11.37311665002360783 ) ) ;
#65120 = CARTESIAN_POINT ( 'NONE',  ( -27.09364415740165555, 2.088137158971423268, 1.009938549038068567 ) ) ;
#65121 = CARTESIAN_POINT ( 'NONE',  ( 3.459614771489464946, -11.09853614738469396, 4.563167253695070258 ) ) ;
#65122 = B_SPLINE_CURVE_WITH_KNOTS ( 'NONE', 3,
 ( #52760, #27466, #28145, #63689, #18168, #59710 ),
 .UNSPECIFIED., .F., .F.,
 ( 4, 2, 4 ),
 ( 0.009913722359341532037, 0.01153912928143344119, 0.01316453620352535034 ),
 .UNSPECIFIED. ) ;
#65123 = EDGE_CURVE ( 'NONE', #38116, #40447, #41413, .T. ) ;
#65124 = CARTESIAN_POINT ( 'NONE',  ( 0.2648978790185584908, -6.008231198268910056, -10.67083876753498117 ) ) ;
#65125 = ADVANCED_FACE ( 'NONE', ( #6857 ), #6520, .T. ) ;
#65126 = ORIENTED_EDGE ( 'NONE', *, *, #21774, .F. ) ;
#65127 = AXIS2_PLACEMENT_3D ( 'NONE', #47858, #2315, #36888 ) ;
#65128 = CYLINDRICAL_SURFACE ( 'NONE', #11592, 4.785769192180104881 ) ;
#65129 = ORIENTED_EDGE ( 'NONE', *, *, #32779, .T. ) ;
#65130 = DIRECTION ( 'NONE',  ( 0.000000000000000000, -0.01356324068817999114, 0.9999080150203989437 ) ) ;
#65131 = CARTESIAN_POINT ( 'NONE',  ( -37.00000000000000711, 8.534258022646220354, -8.699265615722891809 ) ) ;
#65132 = ADVANCED_FACE ( 'NONE', ( #27127 ), #11491, .T. ) ;
#65133 = CARTESIAN_POINT ( 'NONE',  ( 35.00000000000000000, 10.59380114696469732, -7.094637218249395971 ) ) ;
#65134 = CARTESIAN_POINT ( 'NONE',  ( -29.60173393771532346, -2.916829795459872088, -13.20259329781003466 ) ) ;
#65135 = AXIS2_PLACEMENT_3D ( 'NONE', #27539, #47836, #42833 ) ;
#65136 = EDGE_CURVE ( 'NONE', #45350, #15359, #7881, .T. ) ;
#65137 = ORIENTED_EDGE ( 'NONE', *, *, #11476, .T. ) ;
#65138 = VERTEX_POINT ( 'NONE', #62052 ) ;
#65139 = DIRECTION ( 'NONE',  ( -1.000000000000000000, -0.000000000000000000, 0.000000000000000000 ) ) ;
#65140 = ORIENTED_EDGE ( 'NONE', *, *, #64598, .F. ) ;
#65141 = LINE ( 'NONE', #40866, #23442 ) ;
#65142 = FACE_OUTER_BOUND ( 'NONE', #44539, .T. ) ;
#65143 = CARTESIAN_POINT ( 'NONE',  ( 2.241528039335008771, 4.919377664485172552, -5.838210500619323895 ) ) ;
#65144 = DIRECTION ( 'NONE',  ( 1.000000000000000000, 0.000000000000000000, 0.000000000000000000 ) ) ;
#65145 = CARTESIAN_POINT ( 'NONE',  ( 2.368238019615410028, 6.556525400300650119, -3.992969450835625711 ) ) ;
#65146 = FACE_OUTER_BOUND ( 'NONE', #56001, .T. ) ;
#65147 = EDGE_LOOP ( 'NONE', ( #2726, #50132, #14321, #44183 ) ) ;
#65148 = EDGE_CURVE ( 'NONE', #38736, #37992, #1551, .T. ) ;
#65149 = VECTOR ( 'NONE', #24175, 1000.000000000000000 ) ;
#65150 = VERTEX_POINT ( 'NONE', #7836 ) ;
#65151 = ORIENTED_EDGE ( 'NONE', *, *, #40446, .T. ) ;
#65152 = CARTESIAN_POINT ( 'NONE',  ( 0.1900979142430820334, -0.2738684153833554902, 13.49791647769710679 ) ) ;
#65153 = LINE ( 'NONE', #33909, #42735 ) ;
#65154 = ORIENTED_EDGE ( 'NONE', *, *, #6461, .F. ) ;
#65155 = B_SPLINE_CURVE_WITH_KNOTS ( 'NONE', 3,
 ( #50066, #24796, #45076, #65344, #19808, #9809, #50408, #60354, #4854, #25122, #26110, #16462, #41715, #1510, #56023, #30428, #20783, #41055, #21444, #518, #35728, #16117 ),
 .UNSPECIFIED., .F., .F.,
 ( 4, 2, 2, 2, 2, 2, 2, 2, 2, 2, 4 ),
 ( 0.003549775680923942470, 0.004881064640633089174, 0.005546709120487661009, 0.006212353600342233710, 0.007543642560051378246, 0.008209287039905950947, 0.008874931519760523649, 0.01020622047946966905, 0.01153750943917881445, 0.01286879839888795986, 0.01420008735859710700 ),
 .UNSPECIFIED. ) ;
#65156 = CARTESIAN_POINT ( 'NONE',  ( -35.00000000000000000, 0.000000000000000000, 0.000000000000000000 ) ) ;
#65157 = ORIENTED_EDGE ( 'NONE', *, *, #10656, .T. ) ;
#65158 = DIRECTION ( 'NONE',  ( -0.000000000000000000, -0.000000000000000000, -1.000000000000000000 ) ) ;
#65159 = VECTOR ( 'NONE', #12872, 1000.000000000000000 ) ;
#65160 = CARTESIAN_POINT ( 'NONE',  ( 37.00000000000000711, 8.029056188533806093, 8.573591947375229338 ) ) ;
#65162 = EDGE_CURVE ( 'NONE', #62155, #64321, #64164, .T. ) ;
#65161 = FACE_OUTER_BOUND ( 'NONE', #33561, .T. ) ;
#65163 = CARTESIAN_POINT ( 'NONE',  ( 7.266065016736156679, -6.970945981239493605, 9.778723759522906178 ) ) ;
#65164 = EDGE_LOOP ( 'NONE', ( #7601, #45851, #30890, #54353 ) ) ;
#65165 = CIRCLE ( 'NONE', #45005, 5.000000000000000888 ) ;
#65166 = ORIENTED_EDGE ( 'NONE', *, *, #12556, .T. ) ;
#65167 = DIRECTION ( 'NONE',  ( -1.000000000000000000, 0.000000000000000000, 0.000000000000000000 ) ) ;
#65169 = ORIENTED_EDGE ( 'NONE', *, *, #2612, .T. ) ;
#65168 = EDGE_CURVE ( 'NONE', #16649, #28605, #21826, .T. ) ;
#65170 = LINE ( 'NONE', #4010, #48630 ) ;
#65171 = ORIENTED_EDGE ( 'NONE', *, *, #49376, .F. ) ;
#65172 = CIRCLE ( 'NONE', #17386, 5.000000000000000000 ) ;
#65173 = ORIENTED_EDGE ( 'NONE', *, *, #39320, .F. ) ;
#65175 = EDGE_CURVE ( 'NONE', #28152, #25175, #62353, .T. ) ;
#65174 = VERTEX_POINT ( 'NONE', #58048 ) ;
#65176 = CARTESIAN_POINT ( 'NONE',  ( -35.00000000000000000, -10.75351884295731253, 4.725891942574718563 ) ) ;
#65177 = AXIS2_PLACEMENT_3D ( 'NONE', #28758, #35372, #30395 ) ;
#65178 = CARTESIAN_POINT ( 'NONE',  ( -1.318817192132426526E-11, -30.53649492335491544, -15.30974548841782834 ) ) ;
#65179 = DIRECTION ( 'NONE',  ( -1.000000000000000000, 0.000000000000000000, -0.000000000000000000 ) ) ;
#65180 = FACE_OUTER_BOUND ( 'NONE', #33178, .T. ) ;
#65181 = ORIENTED_EDGE ( 'NONE', *, *, #44997, .T. ) ;
#65182 = EDGE_CURVE ( 'NONE', #52513, #27353, #60943, .T. ) ;
#65183 = CARTESIAN_POINT ( 'NONE',  ( 2.245754705088262693, -2.506725724682980161, -7.212684575686632904 ) ) ;
#65184 = VERTEX_POINT ( 'NONE', #11813 ) ;
#65185 = FACE_OUTER_BOUND ( 'NONE', #56986, .T. ) ;
#65186 = AXIS2_PLACEMENT_3D ( 'NONE', #47455, #1895, #17184 ) ;
#65187 = CARTESIAN_POINT ( 'NONE',  ( 37.00000000000000711, -11.80185301892977279, 4.824807283154243898 ) ) ;
#65188 = EDGE_CURVE ( 'NONE', #25928, #16089, #32253, .T. ) ;
#65189 = VERTEX_POINT ( 'NONE', #62678 ) ;
#65190 = CARTESIAN_POINT ( 'NONE',  ( 0.7446945582530672958, 9.728576129010571449, -7.698291984229237883 ) ) ;
#65191 = DIRECTION ( 'NONE',  ( 0.000000000000000000, -0.6269146997507875074, -0.7790879021242596014 ) ) ;
#65192 = CARTESIAN_POINT ( 'NONE',  ( 2.257661810676414582, -6.682681612748183397, -3.702552158175678176 ) ) ;
#65193 = ORIENTED_EDGE ( 'NONE', *, *, #64000, .F. ) ;
#65194 = AXIS2_PLACEMENT_3D ( 'NONE', #34595, #9, #49907 ) ;
#65195 = ORIENTED_EDGE ( 'NONE', *, *, #21728, .F. ) ;
#65196 = CARTESIAN_POINT ( 'NONE',  ( 2.256373768223416842, -7.638251659827610673, 0.1329433694244051001 ) ) ;
#65197 = ORIENTED_EDGE ( 'NONE', *, *, #55583, .T. ) ;
#65198 = CARTESIAN_POINT ( 'NONE',  ( -24.67014067453516901, -8.921734260348005208, 10.13897465123165453 ) ) ;
#65199 = CARTESIAN_POINT ( 'NONE',  ( 1.000000000000000888, -0.7281529553921430864, -7.464569195442815719 ) ) ;
#65200 = CARTESIAN_POINT ( 'NONE',  ( 2.507146904658099640, 6.793847219607499710, -3.672650549645595230 ) ) ;
#65201 = CARTESIAN_POINT ( 'NONE',  ( 0.000000000000000000, -6.643843315911796665, -1.507714007300762660 ) ) ;
#65202 = CARTESIAN_POINT ( 'NONE',  ( 13.30993466298489913, 10.25874852760247968, -6.229666527591529501 ) ) ;
#65203 = ORIENTED_EDGE ( 'NONE', *, *, #26975, .F. ) ;
#65204 = CIRCLE ( 'NONE', #39711, 12.18650000000000055 ) ;
#65205 = CIRCLE ( 'NONE', #11099, 12.74999999999999822 ) ;
#65206 = CARTESIAN_POINT ( 'NONE',  ( 2.259025283528092842, -4.805599953367692301, 5.939720477913342123 ) ) ;
#65207 = LINE ( 'NONE', #52865, #57775 ) ;
#65208 = CARTESIAN_POINT ( 'NONE',  ( -35.00000000000000000, 0.000000000000000000, 0.000000000000000000 ) ) ;
#65209 = DIRECTION ( 'NONE',  ( -1.000000000000000000, 0.000000000000000000, 0.000000000000000000 ) ) ;
#65210 = EDGE_CURVE ( 'NONE', #5409, #43973, #22287, .T. ) ;
#65211 = CARTESIAN_POINT ( 'NONE',  ( -5.041025311761536898, -26.84022127302798921, -15.79220748139830910 ) ) ;
#65212 = CARTESIAN_POINT ( 'NONE',  ( 2.994568964204209038, -5.368337437440291460, 5.775954174106914252 ) ) ;
#65213 = DIRECTION ( 'NONE',  ( 0.000000000000000000, 0.000000000000000000, 1.000000000000000000 ) ) ;
#65214 = DIRECTION ( 'NONE',  ( 0.000000000000000000, 0.01356324068817999114, -0.9999080150203989437 ) ) ;
#65215 = DIRECTION ( 'NONE',  ( 0.000000000000000000, -0.5155538571770286183, 0.8568571761675851661 ) ) ;
#65216 = VECTOR ( 'NONE', #58014, 1000.000000000000000 ) ;
#65217 = ADVANCED_FACE ( 'NONE', ( #53044 ), #7481, .T. ) ;
#65218 = CIRCLE ( 'NONE', #36562, 4.999999999999997335 ) ;
#65219 = ORIENTED_EDGE ( 'NONE', *, *, #22706, .F. ) ;
#65220 = DIRECTION ( 'NONE',  ( 0.000000000000000000, -0.9937233664769772323, 0.1118654143051511785 ) ) ;
#65221 = ORIENTED_EDGE ( 'NONE', *, *, #51117, .T. ) ;
#65222 = CARTESIAN_POINT ( 'NONE',  ( 37.00000000000000711, 6.280308599560279426, 9.926225166346956286 ) ) ;
#65223 = DIRECTION ( 'NONE',  ( -0.1298914529148032515, 0.000000000000000000, -0.9915282196991074271 ) ) ;
#65224 = LINE ( 'NONE', #29632, #39581 ) ;
#65225 = CIRCLE ( 'NONE', #36572, 7.499999999999988454 ) ;
#65226 = CARTESIAN_POINT ( 'NONE',  ( -35.00000000000000000, 6.280308599560139093, 9.926225166347048656 ) ) ;
#65227 = ORIENTED_EDGE ( 'NONE', *, *, #2730, .F. ) ;
#65228 = EDGE_CURVE ( 'NONE', #52347, #19909, #5803, .T. ) ;
#65229 = CIRCLE ( 'NONE', #16405, 12.74999999999999822 ) ;
#65230 = ORIENTED_EDGE ( 'NONE', *, *, #3428, .F. ) ;
#65231 = ORIENTED_EDGE ( 'NONE', *, *, #23764, .F. ) ;
#65232 = CARTESIAN_POINT ( 'NONE',  ( 29.72995639581280969, -7.926718941844264954, 9.022826046292943047 ) ) ;
#65233 = EDGE_CURVE ( 'NONE', #23443, #21834, #28756, .T. ) ;
#65234 = AXIS2_PLACEMENT_3D ( 'NONE', #11947, #46241, #26928 ) ;
#65235 = CARTESIAN_POINT ( 'NONE',  ( 25.00000000000000355, -9.999999999999998224, 1.530808498934191521E-15 ) ) ;
#65236 = VERTEX_POINT ( 'NONE', #28422 ) ;
#65237 = CARTESIAN_POINT ( 'NONE',  ( 35.00000000000000000, -9.821084925794620446, -7.215058775251224077 ) ) ;
#65238 = FACE_OUTER_BOUND ( 'NONE', #12327, .T. ) ;
#65239 = CARTESIAN_POINT ( 'NONE',  ( 5.514970785353741078, -0.001326349372336325721, 0.004532877335078709831 ) ) ;
#65240 = LINE ( 'NONE', #9056, #8889 ) ;
#65241 = ORIENTED_EDGE ( 'NONE', *, *, #30663, .T. ) ;
#65242 =( BOUNDED_SURFACE ( )  B_SPLINE_SURFACE ( 3, 1, ( 
 ( #7945, #17589 ),
 ( #47517, #33529 ),
 ( #37856, #7256 ),
 ( #27541, #63437 ) ),
 .UNSPECIFIED., .F., .F., .F. ) 
 B_SPLINE_SURFACE_WITH_KNOTS ( ( 4, 4 ),
 ( 2, 2 ),
 ( 0.000000000000000000, 1.000000000000000000 ),
 ( 0.000000000000000000, 1.000000000000000000 ),
 .UNSPECIFIED. ) 
 GEOMETRIC_REPRESENTATION_ITEM ( )  RATIONAL_B_SPLINE_SURFACE ( (
 ( 1.000000000000000000, 1.000000000000000000),
 ( 0.9932032654565553509, 0.8386279382598736953),
 ( 0.9932032654565553509, 0.8386279382598736953),
 ( 1.000000000000000000, 1.000000000000000000) ) ) 
 REPRESENTATION_ITEM ( '' )  SURFACE ( )  );
#65243 = DIRECTION ( 'NONE',  ( -0.1298914529148032515, 0.000000000000000000, -0.9915282196991074271 ) ) ;
#65244 = CARTESIAN_POINT ( 'NONE',  ( -7.278994278378523752, -27.16225867570108932, -15.27062364585639287 ) ) ;
#65245 = DIRECTION ( 'NONE',  ( -1.000000000000000000, 0.000000000000000000, 0.000000000000000000 ) ) ;
#65247 = ORIENTED_EDGE ( 'NONE', *, *, #54006, .T. ) ;
#65246 = DIRECTION ( 'NONE',  ( 0.000000000000000000, 0.000000000000000000, 1.000000000000000000 ) ) ;
#65248 = CARTESIAN_POINT ( 'NONE',  ( 2.000000000000001776, 0.000000000000000000, 0.000000000000000000 ) ) ;
#65249 = EDGE_LOOP ( 'NONE', ( #60641, #16964, #65151, #15925 ) ) ;
#65250 = AXIS2_PLACEMENT_3D ( 'NONE', #55990, #30393, #46030 ) ;
#65251 = CARTESIAN_POINT ( 'NONE',  ( 2.000000000000001776, 1.956810415765184219, 6.654767106875543625 ) ) ;
#65252 = CIRCLE ( 'NONE', #46140, 12.18649999999999878 ) ;
#65253 = ORIENTED_EDGE ( 'NONE', *, *, #45596, .T. ) ;
#65254 = DIRECTION ( 'NONE',  ( -1.000000000000000000, 0.000000000000000000, 0.000000000000000000 ) ) ;
#65255 = CARTESIAN_POINT ( 'NONE',  ( -35.00000000000000000, 0.000000000000000000, 0.000000000000000000 ) ) ;
#65256 = ADVANCED_FACE ( 'NONE', ( #59347 ), #48724, .T. ) ;
#65257 = DIRECTION ( 'NONE',  ( 0.000000000000000000, 0.01356324068817998940, -0.9999080150203990547 ) ) ;
#65258 = DIRECTION ( 'NONE',  ( -1.000000000000000000, 0.000000000000000000, 0.000000000000000000 ) ) ;
#65259 = FACE_OUTER_BOUND ( 'NONE', #24525, .T. ) ;
#65260 = DIRECTION ( 'NONE',  ( -1.000000000000000000, 0.000000000000000000, 0.000000000000000000 ) ) ;
#65261 = CARTESIAN_POINT ( 'NONE',  ( -27.08429572838383947, 2.217805374070540125, -0.5764601019425888984 ) ) ;
#65262 = CARTESIAN_POINT ( 'NONE',  ( -37.00000000000000711, -3.805206332242559775, 12.16893194857548899 ) ) ;
#65264 = VERTEX_POINT ( 'NONE', #18486 ) ;
#65263 = DIRECTION ( 'NONE',  ( 1.000000000000000000, 0.000000000000000000, 0.000000000000000000 ) ) ;
#65265 = EDGE_CURVE ( 'NONE', #27835, #35397, #16417, .T. ) ;
#65266 = VERTEX_POINT ( 'NONE', #39379 ) ;
#65267 = CARTESIAN_POINT ( 'NONE',  ( 42.50000000000000000, -2.710505431213761085E-17, 1.201363017033314212E-18 ) ) ;
#65268 = EDGE_LOOP ( 'NONE', ( #40696, #25005, #44155, #45283 ) ) ;
#65269 = EDGE_CURVE ( 'NONE', #10311, #17416, #30221, .T. ) ;
#65270 = ORIENTED_EDGE ( 'NONE', *, *, #22626, .F. ) ;
#65271 = CARTESIAN_POINT ( 'NONE',  ( 0.8320506296491583242, -12.42924193558400425, 0.3827056590416399451 ) ) ;
#65272 = DIRECTION ( 'NONE',  ( -1.000000000000000000, 0.000000000000000000, -0.000000000000000000 ) ) ;
#65273 = DIRECTION ( 'NONE',  ( 0.000000000000000000, -0.8827602140260265573, 0.4698238015817460256 ) ) ;
#65274 = DIRECTION ( 'NONE',  ( 0.000000000000000000, 0.01356324068817998940, -0.9999080150203990547 ) ) ;
#65275 = CARTESIAN_POINT ( 'NONE',  ( 2.273267844203311405, 7.234348261135926883, 2.472013099046034057 ) ) ;
#65276 = EDGE_CURVE ( 'NONE', #41059, #43621, #8812, .T. ) ;
#65277 = DIRECTION ( 'NONE',  ( 1.000000000000000000, -0.000000000000000000, -0.000000000000000000 ) ) ;
#65278 = ORIENTED_EDGE ( 'NONE', *, *, #64119, .F. ) ;
#65279 = DIRECTION ( 'NONE',  ( -1.977578355587678392E-17, 0.1764146379942750364, 0.9843159429275484262 ) ) ;
#65280 = CARTESIAN_POINT ( 'NONE',  ( 37.00000000000000711, 0.000000000000000000, -1.750000000000000000 ) ) ;
#65281 = DIRECTION ( 'NONE',  ( 0.000000000000000000, -0.01356324068817991828, 0.9999080150203990547 ) ) ;
#65282 = ORIENTED_EDGE ( 'NONE', *, *, #46126, .F. ) ;
#65283 = PRODUCT_DEFINITION ( 'UNKNOWN', '', #44125, #37234 ) ;
#65284 = CIRCLE ( 'NONE', #52548, 12.00000000000000000 ) ;
#65285 = ADVANCED_FACE ( 'NONE', ( #33735 ), #49405, .T. ) ;
#65286 = CARTESIAN_POINT ( 'NONE',  ( 48.66712064925836501, -0.2684213679329396918, -8.095633725969733518 ) ) ;
#65287 = CARTESIAN_POINT ( 'NONE',  ( -27.27855387000350262, -10.59660315834921107, 5.631341004100471892 ) ) ;
#65288 = CYLINDRICAL_SURFACE ( 'NONE', #4151, 5.000000000000000888 ) ;
#65289 = ORIENTED_EDGE ( 'NONE', *, *, #15988, .F. ) ;
#65290 = DIRECTION ( 'NONE',  ( 1.000000000000000000, 0.000000000000000000, 0.000000000000000000 ) ) ;
#65291 = AXIS2_PLACEMENT_3D ( 'NONE', #40620, #60913, #47195 ) ;
#65292 = CARTESIAN_POINT ( 'NONE',  ( 0.9207726606957047366, -30.53649492335506466, 15.30974548841765426 ) ) ;
#65293 = CARTESIAN_POINT ( 'NONE',  ( 0.2851083653049504285, -0.4107471485392698018, 11.99296822225285730 ) ) ;
#65294 = EDGE_CURVE ( 'NONE', #17087, #54467, #33, .T. ) ;
#65295 = CARTESIAN_POINT ( 'NONE',  ( -27.10719052120871098, 0.1538293304135379680, 2.355164825213503121 ) ) ;
#65296 = FACE_OUTER_BOUND ( 'NONE', #51027, .T. ) ;
#65297 = EDGE_LOOP ( 'NONE', ( #62429, #27969, #56138, #12714 ) ) ;
#65298 = CARTESIAN_POINT ( 'NONE',  ( 2.242418902651940105, 0.09970190380433034683, 7.634109827927228586 ) ) ;
#65299 = CARTESIAN_POINT ( 'NONE',  ( -7.489022030332961322, -5.127957880411574187, -10.84914964302385521 ) ) ;
#65300 = CARTESIAN_POINT ( 'NONE',  ( 1.452237505248555660, 5.807998527926049093, -11.24427360515636032 ) ) ;
#65301 = ORIENTED_EDGE ( 'NONE', *, *, #55381, .T. ) ;
#65302 = CARTESIAN_POINT ( 'NONE',  ( 9.383873380784992335, 1.701316094559147230, 13.39399859679633487 ) ) ;
#65303 = DIRECTION ( 'NONE',  ( 0.000000000000000000, 0.3218879778915972878, -0.9467777615094571386 ) ) ;
#65304 = ORIENTED_EDGE ( 'NONE', *, *, #21976, .T. ) ;
#65305 = ADVANCED_FACE ( 'NONE', ( #24101 ), #48407, .T. ) ;
#65306 = EDGE_CURVE ( 'NONE', #10842, #42133, #2535, .T. ) ;
#65307 = EDGE_LOOP ( 'NONE', ( #34578, #62886, #12768, #26712 ) ) ;
#65308 = ORIENTED_EDGE ( 'NONE', *, *, #38897, .F. ) ;
#65309 = EDGE_CURVE ( 'NONE', #60760, #27227, #47242, .T. ) ;
#65310 = CIRCLE ( 'NONE', #35549, 4.999999999999999112 ) ;
#65311 = ORIENTED_EDGE ( 'NONE', *, *, #41164, .F. ) ;
#65312 = DIRECTION ( 'NONE',  ( 0.000000000000000000, -6.879075853011489629E-15, 1.000000000000000000 ) ) ;
#65313 = CARTESIAN_POINT ( 'NONE',  ( -36.00000000000000711, 9.196955404009424129, -8.830544224262844466 ) ) ;
#65314 = DIRECTION ( 'NONE',  ( -1.000000000000000000, 0.000000000000000000, 0.000000000000000000 ) ) ;
#65315 = CARTESIAN_POINT ( 'NONE',  ( 2.000000000000001776, 0.000000000000000000, 0.000000000000000000 ) ) ;
#65316 = CARTESIAN_POINT ( 'NONE',  ( -11.13200843151504849, -27.03228069553586010, 13.43438493493725616 ) ) ;
#65317 = CARTESIAN_POINT ( 'NONE',  ( -17.58076563216013355, 11.47010079780622682, 3.542952125472129232 ) ) ;
#65319 = VERTEX_POINT ( 'NONE', #19450 ) ;
#65318 = DIRECTION ( 'NONE',  ( 0.000000000000000000, 0.01356324068817998940, -0.9999080150203990547 ) ) ;
#65320 = CARTESIAN_POINT ( 'NONE',  ( 2.241352910868908310, -2.689314586382399952, 7.145045428366567641 ) ) ;
#65321 = ORIENTED_EDGE ( 'NONE', *, *, #60966, .F. ) ;
#65322 = DIRECTION ( 'NONE',  ( 1.000000000000000000, 0.000000000000000000, 0.000000000000000000 ) ) ;
#65323 = ORIENTED_EDGE ( 'NONE', *, *, #6188, .F. ) ;
#65324 = VERTEX_POINT ( 'NONE', #9126 ) ;
#65325 = CARTESIAN_POINT ( 'NONE',  ( -22.29770266787582500, -0.8895590726606950049, 3.635870259503088064 ) ) ;
#65326 = CARTESIAN_POINT ( 'NONE',  ( 13.98043512791166698, -30.12632228061958273, 5.689268883804715848 ) ) ;
#65327 = EDGE_CURVE ( 'NONE', #10194, #44696, #24414, .T. ) ;
#65328 = DIRECTION ( 'NONE',  ( 0.000000000000000000, 0.7790879021242527180, -0.6269146997507960561 ) ) ;
#65329 = VECTOR ( 'NONE', #54344, 1000.000000000000000 ) ;
#65330 = CARTESIAN_POINT ( 'NONE',  ( 2.573738926104377267, 7.664876274722926652, -1.112690714006459247 ) ) ;
#65331 = CYLINDRICAL_SURFACE ( 'NONE', #52620, 2.899999999999994582 ) ;
#65332 = CARTESIAN_POINT ( 'NONE',  ( -35.00000000000000000, -12.09831040184925044, 1.463443770872731919 ) ) ;
#65333 = ORIENTED_EDGE ( 'NONE', *, *, #58242, .F. ) ;
#65334 = VERTEX_POINT ( 'NONE', #23115 ) ;
#65335 = DIRECTION ( 'NONE',  ( 1.000000000000000000, -0.000000000000000000, -0.000000000000000000 ) ) ;
#65336 = VERTEX_POINT ( 'NONE', #63656 ) ;
#65337 = VERTEX_POINT ( 'NONE', #38404 ) ;
#65338 = DIRECTION ( 'NONE',  ( -0.000000000000000000, -0.000000000000000000, -1.000000000000000000 ) ) ;
#65339 = LINE ( 'NONE', #40733, #19227 ) ;
#65340 = CARTESIAN_POINT ( 'NONE',  ( 1.104777566491140117, -12.24382064406180959, 2.644034362100653901 ) ) ;
#65341 = B_SPLINE_CURVE_WITH_KNOTS ( 'NONE', 3,
 ( #61138, #60810, #15567, #35832, #15247, #35531, #16239, #56133, #6274, #55827, #945, #62121, #10253, #61441, #21213, #41487, #15885, #36522 ),
 .UNSPECIFIED., .F., .F.,
 ( 4, 2, 2, 2, 2, 2, 2, 2, 4 ),
 ( 1.086801142668811545E-17, 0.002754147681809471920, 0.004131221522714200942, 0.005508295363618930830, 0.006196832284071292739, 0.006885369204523654647, 0.008262443045428381067, 0.009639516886333108353, 0.01101659072723783737 ),
 .UNSPECIFIED. ) ;
#65342 = CARTESIAN_POINT ( 'NONE',  ( 2.241311220309554653, 7.633829235838275551, 0.09281826062098677554 ) ) ;
#65343 = EDGE_CURVE ( 'NONE', #41765, #38476, #32301, .T. ) ;
#65344 = CARTESIAN_POINT ( 'NONE',  ( -11.28047536261793304, -6.236380125593958823, -10.25457663355916083 ) ) ;
#65345 = FACE_OUTER_BOUND ( 'NONE', #50228, .T. ) ;
#65346 = ORIENTED_EDGE ( 'NONE', *, *, #14014, .F. ) ;
#65347 = CIRCLE ( 'NONE', #1628, 4.999999999999999112 ) ;
#65348 = EDGE_LOOP ( 'NONE', ( #33983, #17802, #1909, #57679 ) ) ;
#65349 = CARTESIAN_POINT ( 'NONE',  ( -35.00000000000000000, -10.62137734850264614, -5.015831474386418520 ) ) ;
#65350 = CARTESIAN_POINT ( 'NONE',  ( -47.00000000000000711, 0.000000000000000000, 0.000000000000000000 ) ) ;
#65351 = CIRCLE ( 'NONE', #18690, 3.552075659825890241 ) ;
#65352 = DIRECTION ( 'NONE',  ( -0.000000000000000000, -1.000000000000000000, -0.000000000000000000 ) ) ;
#65353 = CARTESIAN_POINT ( 'NONE',  ( -35.00000000000000000, 6.753013023069858178, -10.14433819232427147 ) ) ;
#65354 = EDGE_CURVE ( 'NONE', #47008, #45297, #29142, .T. ) ;
#65355 = CARTESIAN_POINT ( 'NONE',  ( -7.008316857174801129, -1.821497689352610694, -11.86115302356136780 ) ) ;
#65356 = DIRECTION ( 'NONE',  ( -1.000000000000000000, -0.000000000000000000, 0.000000000000000000 ) ) ;
#65357 = CARTESIAN_POINT ( 'NONE',  ( 5.520433897694421610, -0.0005131706886600394431, 0.01505375422439068044 ) ) ;
#65358 = VERTEX_POINT ( 'NONE', #56312 ) ;
#65359 = CARTESIAN_POINT ( 'NONE',  ( 0.000000000000000000, 0.000000000000000000, 0.000000000000000000 ) ) ;
#65360 = FACE_OUTER_BOUND ( 'NONE', #18048, .T. ) ;
#65361 = FACE_OUTER_BOUND ( 'NONE', #7104, .T. ) ;
#65362 = AXIS2_PLACEMENT_3D ( 'NONE', #24893, #20218, #40495 ) ;
#65363 = EDGE_CURVE ( 'NONE', #53403, #22226, #12125, .T. ) ;
#65364 = CARTESIAN_POINT ( 'NONE',  ( -3.498383876438375228, -31.27426290440411094, -14.18200193795731145 ) ) ;
#65365 = DIRECTION ( 'NONE',  ( -1.000000000000000000, 0.000000000000000000, 0.000000000000000000 ) ) ;
#65366 = ORIENTED_EDGE ( 'NONE', *, *, #54628, .T. ) ;
#65367 = CARTESIAN_POINT ( 'NONE',  ( 5.514624014163232779, 0.003278974416024606296, -0.002529391395135317452 ) ) ;
#65368 = CARTESIAN_POINT ( 'NONE',  ( 5.516018279890452902, 0.003580555109620875767, -0.005752102158674359499 ) ) ;
#65369 = CARTESIAN_POINT ( 'NONE',  ( 12.91449914267798960, -27.44768092100439461, -12.53791341943762916 ) ) ;
#65370 = VERTEX_POINT ( 'NONE', #41020 ) ;
#65371 = DIRECTION ( 'NONE',  ( 1.000000000000000000, 0.000000000000000000, 0.000000000000000000 ) ) ;
#65372 = CARTESIAN_POINT ( 'NONE',  ( 37.00000000000000711, -4.041347439435937439, -11.02904044024207764 ) ) ;
#65373 = CARTESIAN_POINT ( 'NONE',  ( -22.30861784526115699, -1.070462554923801601, -3.620936716852776627 ) ) ;
#65374 = CARTESIAN_POINT ( 'NONE',  ( 0.5572780756278377101, 12.33974848088617549, 0.3055340344618433512 ) ) ;
#65375 = DIRECTION ( 'NONE',  ( 0.000000000000000000, -0.01356324068817991828, 0.9999080150203990547 ) ) ;
#65376 = AXIS2_PLACEMENT_3D ( 'NONE', #42577, #41940, #62538 ) ;
#65377 = DIRECTION ( 'NONE',  ( 1.000000000000000000, 0.000000000000000000, 0.000000000000000000 ) ) ;
#65378 = VERTEX_POINT ( 'NONE', #4821 ) ;
#65379 = DIRECTION ( 'NONE',  ( 0.000000000000000000, -0.01356324068817991828, 0.9999080150203990547 ) ) ;
#65380 = CARTESIAN_POINT ( 'NONE',  ( -37.00000000000000711, 9.908974237959645492, 6.307491713049065751 ) ) ;
#65382 = VECTOR ( 'NONE', #25536, 1000.000000000000000 ) ;
#65381 = FACE_OUTER_BOUND ( 'NONE', #34576, .T. ) ;
#65383 = CARTESIAN_POINT ( 'NONE',  ( -47.00000000000000711, 0.000000000000000000, 0.000000000000000000 ) ) ;
#65384 = CARTESIAN_POINT ( 'NONE',  ( 0.3278977287071223601, -11.44003061923228159, -4.427879319183004370 ) ) ;
#65385 = CARTESIAN_POINT ( 'NONE',  ( 35.00000000000000000, 10.49591321039688019, 5.273331777780226659 ) ) ;
#65386 = DIRECTION ( 'NONE',  ( -1.000000000000000000, -0.000000000000000000, 0.000000000000000000 ) ) ;
#65387 = EDGE_LOOP ( 'NONE', ( #39286, #39956, #6147, #19730 ) ) ;
#65388 = VERTEX_POINT ( 'NONE', #14747 ) ;
#65389 = CARTESIAN_POINT ( 'NONE',  ( 2.255723233588951437, -5.010912740808161736, 5.766109278028616281 ) ) ;
#65390 = VERTEX_POINT ( 'NONE', #45356 ) ;
#65391 = CARTESIAN_POINT ( 'NONE',  ( 25.00000000000000355, -30.00000000000000000, 24.00000000000000000 ) ) ;
#65392 = LINE ( 'NONE', #5226, #8599 ) ;
#65393 = ORIENTED_EDGE ( 'NONE', *, *, #2861, .T. ) ;
#65394 = CYLINDRICAL_SURFACE ( 'NONE', #26609, 14.19297241773857188 ) ;
#65395 = CARTESIAN_POINT ( 'NONE',  ( -27.22214261968803939, -12.41558776886551740, 5.304269109247355729 ) ) ;
#65396 = CARTESIAN_POINT ( 'NONE',  ( 37.00000000000000711, 4.705694406421931860E-17, -3.469127814946512892E-15 ) ) ;
#65397 = ORIENTED_EDGE ( 'NONE', *, *, #23413, .F. ) ;
#65398 = ORIENTED_EDGE ( 'NONE', *, *, #27265, .T. ) ;
#65399 = CARTESIAN_POINT ( 'NONE',  ( -35.00000000000000000, 0.000000000000000000, 0.000000000000000000 ) ) ;
#65400 = EDGE_CURVE ( 'NONE', #50412, #48610, #49340, .T. ) ;
#65401 = ORIENTED_EDGE ( 'NONE', *, *, #13297, .T. ) ;
#65402 = CARTESIAN_POINT ( 'NONE',  ( 1.719304012338199517, 0.000000000000000000, 0.000000000000000000 ) ) ;
#65403 = ORIENTED_EDGE ( 'NONE', *, *, #10166, .T. ) ;
#65404 = LINE ( 'NONE', #10875, #9696 ) ;
#65405 = CARTESIAN_POINT ( 'NONE',  ( 2.288423627607478750, 7.131972212895042240, -2.767471693622725049 ) ) ;
#65406 = EDGE_CURVE ( 'NONE', #58425, #52767, #51360, .T. ) ;
#65407 = DIRECTION ( 'NONE',  ( -0.000000000000000000, -0.000000000000000000, -1.000000000000000000 ) ) ;
#65408 = DIRECTION ( 'NONE',  ( 0.000000000000000000, 1.000000000000000000, 0.000000000000000000 ) ) ;
#65409 = CARTESIAN_POINT ( 'NONE',  ( -14.23194138997495450, 7.940651831586622578, -10.91941811743712876 ) ) ;
#65410 = VERTEX_POINT ( 'NONE', #55678 ) ;
#65411 = CARTESIAN_POINT ( 'NONE',  ( 2.262775599886257094, -1.465770593192945226, 7.499645832851606464 ) ) ;
#65412 = CARTESIAN_POINT ( 'NONE',  ( 0.2652384770603698483, -9.423432754625777008, 7.820955051613289299 ) ) ;
#65413 = CARTESIAN_POINT ( 'NONE',  ( 2.241451721903216399, 5.809054012306858361, 4.953785420083431035 ) ) ;
#65414 = CARTESIAN_POINT ( 'NONE',  ( -18.79799054488956145, 13.49111078119409157, 0.5911816625682176918 ) ) ;
#65415 = CARTESIAN_POINT ( 'NONE',  ( 24.20164632272273764, 0.6982551168995920765, 13.48650918581359548 ) ) ;
#65416 = DIRECTION ( 'NONE',  ( 0.000000000000000000, -0.4698238015817237656, -0.8827602140260383257 ) ) ;
#65417 = DIRECTION ( 'NONE',  ( 0.000000000000000000, -0.1081190184239280011, -0.9941379571543611515 ) ) ;
#65418 = B_SPLINE_CURVE_WITH_KNOTS ( 'NONE', 3,
 ( #23365, #23046, #18399, #7753, #18054, #64252, #52963, #47990, #39882, #8084, #38316, #38664, #58638, #62940, #63261, #58969, #48649, #42635, #28351, #13381, #13062, #33666 ),
 .UNSPECIFIED., .F., .F.,
 ( 4, 3, 3, 3, 3, 3, 3, 4 ),
 ( 0.000000000000000000, 4.447697177976158572E-05, 6.624143997791090725E-05, 8.800576886944027830E-05, 0.0001097699864780866350, 0.0001315341395364341833, 0.0001760120188223243090, 0.0001867971373174694279 ),
 .UNSPECIFIED. ) ;
#65419 = CARTESIAN_POINT ( 'NONE',  ( 19.56743653832046803, -33.00000000000000000, -5.000000000000012434 ) ) ;
#65420 = ADVANCED_FACE ( 'NONE', ( #19777 ), #58928, .T. ) ;
#65421 = EDGE_LOOP ( 'NONE', ( #4998, #53895, #660, #61168 ) ) ;
#65422 = CARTESIAN_POINT ( 'NONE',  ( -18.13077481406540414, 6.846344537678046294, -9.858992475546884293 ) ) ;
#65423 = AXIS2_PLACEMENT_3D ( 'NONE', #52662, #1124, #47014 ) ;
#65424 = VECTOR ( 'NONE', #59992, 1000.000000000000000 ) ;
#65425 = EDGE_CURVE ( 'NONE', #51491, #7491, #53600, .T. ) ;
#65426 =( BOUNDED_SURFACE ( )  B_SPLINE_SURFACE ( 3, 1, ( 
 ( #2320, #57193 ),
 ( #58166, #12272 ),
 ( #32536, #52847 ),
 ( #22594, #42859 ) ),
 .UNSPECIFIED., .F., .F., .F. ) 
 B_SPLINE_SURFACE_WITH_KNOTS ( ( 4, 4 ),
 ( 2, 2 ),
 ( 0.000000000000000000, 1.000000000000000000 ),
 ( 0.000000000000000000, 1.000000000000000000 ),
 .UNSPECIFIED. ) 
 GEOMETRIC_REPRESENTATION_ITEM ( )  RATIONAL_B_SPLINE_SURFACE ( (
 ( 1.000000000000000000, 1.000000000000000000),
 ( 0.9856612449720755231, 0.9999558406602322425),
 ( 0.9856612449720755231, 0.9999558406602322425),
 ( 1.000000000000000000, 1.000000000000000000) ) ) 
 REPRESENTATION_ITEM ( '' )  SURFACE ( )  );
#65427 = ORIENTED_EDGE ( 'NONE', *, *, #553, .T. ) ;
#65428 = EDGE_CURVE ( 'NONE', #63812, #25246, #8962, .T. ) ;
#65429 = CARTESIAN_POINT ( 'NONE',  ( 0.3675815128205894289, 12.27743992903066328, -0.2638082659428851451 ) ) ;
#65430 = CARTESIAN_POINT ( 'NONE',  ( -22.28023996335807411, -3.676538434326165561, 0.3233044107360762420 ) ) ;
#65431 = CARTESIAN_POINT ( 'NONE',  ( 5.520433897694421610, -0.01505375422439067697, -0.0005131706886600855217 ) ) ;
#65432 = CARTESIAN_POINT ( 'NONE',  ( 3.031336079629178393, -7.839300734793016368, -0.9593005538808098143 ) ) ;
#65433 = EDGE_CURVE ( 'NONE', #64603, #49077, #20649, .T. ) ;
#65434 = DIRECTION ( 'NONE',  ( 1.000000000000000000, 0.000000000000000000, 0.000000000000000000 ) ) ;
#65435 = VERTEX_POINT ( 'NONE', #40034 ) ;
#65436 = DIRECTION ( 'NONE',  ( -1.000000000000000000, 0.000000000000000000, 0.000000000000000000 ) ) ;
#65437 = LINE ( 'NONE', #290, #27858 ) ;
#65438 = CARTESIAN_POINT ( 'NONE',  ( 9.102723003675967206, 3.312403327918474361, 11.53614311619802812 ) ) ;
#65439 = CARTESIAN_POINT ( 'NONE',  ( 2.827825597296808713, 4.975864478227498111, -7.528560921609551926 ) ) ;
#65440 = EDGE_CURVE ( 'NONE', #13128, #56608, #46139, .T. ) ;
#65441 = CARTESIAN_POINT ( 'NONE',  ( 10.75853767213705225, 7.830989516993144051, -10.99661780661415733 ) ) ;
#65442 = LINE ( 'NONE', #29238, #51032 ) ;
#65443 = ORIENTED_EDGE ( 'NONE', *, *, #63398, .T. ) ;
#65444 = ADVANCED_FACE ( 'NONE', ( #10761 ), #10114, .T. ) ;
#65445 = CARTESIAN_POINT ( 'NONE',  ( 3.152665057734040488, 0.000000000000000000, 0.000000000000000000 ) ) ;
#65446 = ORIENTED_EDGE ( 'NONE', *, *, #27389, .T. ) ;
#65447 = CARTESIAN_POINT ( 'NONE',  ( 0.2653141334712581512, 12.24612529725264132, -0.04405251235385006237 ) ) ;
#65448 = CARTESIAN_POINT ( 'NONE',  ( -35.00000000000000000, -4.986700593229626222, -10.63508530065527147 ) ) ;
#65449 = DIRECTION ( 'NONE',  ( 0.000000000000000000, 0.000000000000000000, 1.000000000000000000 ) ) ;
#65450 = CARTESIAN_POINT ( 'NONE',  ( 35.00000000000000000, 4.705694406421931860E-17, -3.469127814946512892E-15 ) ) ;
#65451 = VERTEX_POINT ( 'NONE', #56672 ) ;
#65452 = ORIENTED_EDGE ( 'NONE', *, *, #27050, .F. ) ;
#65454 = EDGE_CURVE ( 'NONE', #10789, #13395, #35024, .T. ) ;
#65453 = CARTESIAN_POINT ( 'NONE',  ( 0.2648978790185602672, 12.24533305150758089, -0.1321385342562831633 ) ) ;
#65455 = ORIENTED_EDGE ( 'NONE', *, *, #24483, .F. ) ;
#65456 = CARTESIAN_POINT ( 'NONE',  ( 2.258463476536643366, -6.547539277368008115, -3.937122681832554427 ) ) ;
#65457 = CARTESIAN_POINT ( 'NONE',  ( 0.3665391374699472626, -0.2638605131386310143, -12.27992639892678639 ) ) ;
#65458 = CARTESIAN_POINT ( 'NONE',  ( -22.27706485742869091, -3.358064672837095976, -1.508175983031630585 ) ) ;
#65459 = CARTESIAN_POINT ( 'NONE',  ( 35.00000000000000000, -6.036400161834636791, -10.07641281632175634 ) ) ;
#65460 = CARTESIAN_POINT ( 'NONE',  ( 0.5547464869798230946, 9.256151063740663432, -8.164898018378718092 ) ) ;
#65461 = CARTESIAN_POINT ( 'NONE',  ( -35.00000000000000000, 10.80631716521666874, 4.603882218679588689 ) ) ;
#65462 = CARTESIAN_POINT ( 'NONE',  ( -19.02967556479664069, -11.99999999999998934, 9.262893081595934602E-16 ) ) ;
#65463 = VERTEX_POINT ( 'NONE', #50691 ) ;
#65465 = ORIENTED_EDGE ( 'NONE', *, *, #35702, .F. ) ;
#65464 = CARTESIAN_POINT ( 'NONE',  ( 3.100650473569755317, -2.280184661131145596, -7.585586315875764818 ) ) ;
#65466 = ORIENTED_EDGE ( 'NONE', *, *, #8534, .F. ) ;
#65467 = VECTOR ( 'NONE', #23817, 1000.000000000000000 ) ;
#65468 = CARTESIAN_POINT ( 'NONE',  ( 3.152665057735613008, -6.378477742801520023, -4.725420687649700469 ) ) ;
#65469 = CARTESIAN_POINT ( 'NONE',  ( 3.152665057734004073, 7.102135024645805039, -3.546019893116331811 ) ) ;
#65470 = ORIENTED_EDGE ( 'NONE', *, *, #37699, .F. ) ;
#65471 = AXIS2_PLACEMENT_3D ( 'NONE', #37922, #16985, #33268 ) ;
#65472 = CARTESIAN_POINT ( 'NONE',  ( 35.00000000000000000, 4.705694406421931860E-17, -3.469127814946512892E-15 ) ) ;
#65473 = ORIENTED_EDGE ( 'NONE', *, *, #55830, .T. ) ;
#65474 = CARTESIAN_POINT ( 'NONE',  ( 1.719304012338199295, 12.64775761152512423, 1.452142814150486183 ) ) ;
#65475 = CARTESIAN_POINT ( 'NONE',  ( 3.347841273039249721, -10.61118957148187825, -8.345816669330458737 ) ) ;
#65476 = CARTESIAN_POINT ( 'NONE',  ( 17.27839441901508621, 10.52068335315811076, 5.771933972472480967 ) ) ;
#65477 = CARTESIAN_POINT ( 'NONE',  ( 3.152665057734125309, -6.622010822086626725, -4.377619405892440696 ) ) ;
#65478 = ORIENTED_EDGE ( 'NONE', *, *, #15964, .T. ) ;
#65479 = ORIENTED_EDGE ( 'NONE', *, *, #36269, .F. ) ;
#65480 = CARTESIAN_POINT ( 'NONE',  ( 2.705197763288543999, -6.881024880055373494, 3.649695155981489414 ) ) ;
#65481 = ORIENTED_EDGE ( 'NONE', *, *, #42742, .T. ) ;
#65482 = ORIENTED_EDGE ( 'NONE', *, *, #3568, .T. ) ;
#65483 = ORIENTED_EDGE ( 'NONE', *, *, #25315, .T. ) ;
#65484 = ORIENTED_EDGE ( 'NONE', *, *, #48253, .F. ) ;
#65485 = CARTESIAN_POINT ( 'NONE',  ( 37.00000000000000711, -9.196955404009232282, 8.830544224263041642 ) ) ;
#65486 = CARTESIAN_POINT ( 'NONE',  ( 2.000000000000001776, -0.8935325819928070512, -7.446583077151393226 ) ) ;
#65487 = EDGE_CURVE ( 'NONE', #3518, #44848, #50414, .T. ) ;
#65488 = CARTESIAN_POINT ( 'NONE',  ( 37.00000000000000711, -12.16893194857552629, -3.805206332242429212 ) ) ;
#65489 = CARTESIAN_POINT ( 'NONE',  ( -22.30625920655495165, -1.672644928563074451, 3.403091720605004866 ) ) ;
#65490 = VERTEX_POINT ( 'NONE', #793 ) ;
#65491 = DIRECTION ( 'NONE',  ( 0.000000000000000000, -0.01356324068817998940, 0.9999080150203990547 ) ) ;
#65492 = ORIENTED_EDGE ( 'NONE', *, *, #28974, .T. ) ;
#65493 = CARTESIAN_POINT ( 'NONE',  ( 35.00000000000000000, -7.745827850123079727, -10.12742074351894139 ) ) ;
#65494 = DIRECTION ( 'NONE',  ( 0.000000000000000000, 0.01356324068817998940, -0.9999080150203990547 ) ) ;
#65495 = EDGE_LOOP ( 'NONE', ( #57386, #57092, #35721, #4597 ) ) ;
#65496 = CARTESIAN_POINT ( 'NONE',  ( 1.452237505248552996, 6.833827325205466430, -10.65201107290460492 ) ) ;
#65497 = CARTESIAN_POINT ( 'NONE',  ( 0.2648978790185584908, 4.063980959785046032, 11.55204314799265042 ) ) ;
#65498 = CARTESIAN_POINT ( 'NONE',  ( 2.244591118396555007, -6.665613643996570303, -3.724266936773059644 ) ) ;
#65499 = ADVANCED_FACE ( 'NONE', ( #142 ), #20420, .T. ) ;
#65500 = ORIENTED_EDGE ( 'NONE', *, *, #33858, .F. ) ;
#65501 = CARTESIAN_POINT ( 'NONE',  ( 1.014383007554940264, 6.628652139012910283, 10.59286224865783943 ) ) ;
#65502 = CIRCLE ( 'NONE', #34692, 7.938172270156617749 ) ;
#65503 = ORIENTED_EDGE ( 'NONE', *, *, #46322, .T. ) ;
#65504 = EDGE_CURVE ( 'NONE', #15452, #12898, #23021, .T. ) ;
#65505 = CARTESIAN_POINT ( 'NONE',  ( -35.00000000000000000, -11.65150730582933392, -1.488153103997089888 ) ) ;
#65506 = SURFACE_STYLE_FILL_AREA ( #45250 ) ;
#65507 = CARTESIAN_POINT ( 'NONE',  ( -37.00000000000000711, 12.01765980939845058, -2.021542716731266065 ) ) ;
#65508 = CARTESIAN_POINT ( 'NONE',  ( 37.00000000000000711, -0.4353888892049205261, -11.73808581813437968 ) ) ;
#65509 = ADVANCED_FACE ( 'NONE', ( #31048 ), #32657, .T. ) ;
#65510 = CARTESIAN_POINT ( 'NONE',  ( -19.69476066079020171, -4.201994156881551312, -12.82938989607585789 ) ) ;
#65511 = ORIENTED_EDGE ( 'NONE', *, *, #28508, .F. ) ;
#65512 = DIRECTION ( 'NONE',  ( 0.000000000000000000, 0.01356324068817992175, -0.9999080150203990547 ) ) ;
#65513 = CARTESIAN_POINT ( 'NONE',  ( 35.00000000000000000, -8.029056188533749250, -8.573591947375291511 ) ) ;
#65514 = CARTESIAN_POINT ( 'NONE',  ( 2.241509619876139059, 3.850348903238805409, -6.592435552901080520 ) ) ;
#65515 = VECTOR ( 'NONE', #8673, 1000.000000000000000 ) ;
#65516 = LINE ( 'NONE', #33958, #10451 ) ;
#65517 = AXIS2_PLACEMENT_3D ( 'NONE', #32752, #12165, #22478 ) ;
#65518 = CARTESIAN_POINT ( 'NONE',  ( 0.3341166715381300722, -12.12403120948088464, -1.881279064087967523 ) ) ;
#65519 = EDGE_CURVE ( 'NONE', #9279, #7682, #2631, .T. ) ;
#65520 = CARTESIAN_POINT ( 'NONE',  ( 1.000000000000000888, 6.586971819220387658, -3.586335490831350725 ) ) ;
#65521 = EDGE_CURVE ( 'NONE', #63755, #63127, #6833, .T. ) ;
#65522 = DIRECTION ( 'NONE',  ( 0.000000000000000000, -0.5987040770935736500, 0.8009703041134121904 ) ) ;
#65523 = CARTESIAN_POINT ( 'NONE',  ( 36.00000000000000711, 10.02106554660720050, 7.882940143791662635 ) ) ;
#65524 = CYLINDRICAL_SURFACE ( 'NONE', #19507, 12.74999999999999822 ) ;
#65525 = EDGE_CURVE ( 'NONE', #29925, #27543, #14265, .T. ) ;
#65526 = ORIENTED_EDGE ( 'NONE', *, *, #30837, .T. ) ;
#65527 = CARTESIAN_POINT ( 'NONE',  ( -27.09150307427447757, -1.305148381377968070, -1.909742362151680917 ) ) ;
#65528 = EDGE_CURVE ( 'NONE', #53824, #36705, #40499, .T. ) ;
#65529 = VERTEX_POINT ( 'NONE', #47345 ) ;
#65530 = DIRECTION ( 'NONE',  ( 0.000000000000000000, 0.01356324068817992175, -0.9999080150203990547 ) ) ;
#65531 = CARTESIAN_POINT ( 'NONE',  ( -22.27715526084302056, -3.652257391294512878, 0.4651416883073748454 ) ) ;
#65532 = DIRECTION ( 'NONE',  ( 0.000000000000000000, -0.01356324068817999114, 0.9999080150203989437 ) ) ;
#65533 = ADVANCED_FACE ( 'NONE', ( #42305 ), #52967, .T. ) ;
#65534 = CARTESIAN_POINT ( 'NONE',  ( 5.516018279890452902, -0.005752102158674371642, -0.003580555109620855384 ) ) ;
#65535 = EDGE_LOOP ( 'NONE', ( #23612, #63791 ) ) ;
#65536 = ORIENTED_EDGE ( 'NONE', *, *, #44253, .F. ) ;
#65537 = EDGE_LOOP ( 'NONE', ( #49054, #60745, #26183, #48847 ) ) ;
#65538 = CARTESIAN_POINT ( 'NONE',  ( -27.15511094194037867, 2.499833641087587655, -0.1446243978645330164 ) ) ;
#65539 = CIRCLE ( 'NONE', #53904, 17.19615242270663558 ) ;
#65540 = CARTESIAN_POINT ( 'NONE',  ( 2.556980015513997007, 3.668282146013217559, -6.815084337351887456 ) ) ;
#65541 = ORIENTED_EDGE ( 'NONE', *, *, #1745, .T. ) ;
#65542 = CARTESIAN_POINT ( 'NONE',  ( 2.655192694323576852, -0.5793947661801577276, -9.584054627288868033 ) ) ;
#65543 = FACE_OUTER_BOUND ( 'NONE', #9637, .T. ) ;
#65544 = CARTESIAN_POINT ( 'NONE',  ( 2.653899356899988682, -2.411250235128107100, 7.388433688587405790 ) ) ;
#65545 = ORIENTED_EDGE ( 'NONE', *, *, #63203, .T. ) ;
#65546 = CARTESIAN_POINT ( 'NONE',  ( 2.266490820343738832, 4.800466063945178163, -5.947069344280496495 ) ) ;
#65547 = CARTESIAN_POINT ( 'NONE',  ( -2.647174210752900603, -26.63290002157760128, -16.10638009382239488 ) ) ;
#65548 = DIRECTION ( 'NONE',  ( 0.000000000000000000, 0.8009703041134189627, 0.5987040770935648792 ) ) ;
#65550 = ORIENTED_EDGE ( 'NONE', *, *, #54120, .T. ) ;
#65549 = DIRECTION ( 'NONE',  ( 0.000000000000000000, 0.01356324068817992175, -0.9999080150203990547 ) ) ;
#65551 = CARTESIAN_POINT ( 'NONE',  ( 0.000000000000000000, -30.00000000000000000, 0.000000000000000000 ) ) ;
#65552 = ORIENTED_EDGE ( 'NONE', *, *, #59917, .T. ) ;
#65553 = DIRECTION ( 'NONE',  ( 1.000000000000000000, 0.000000000000000000, 0.000000000000000000 ) ) ;
#65554 = B_SPLINE_CURVE_WITH_KNOTS ( 'NONE', 3,
 ( #40244, #45566, #20302, #65200, #60532, #45913, #10317, #4716, #45251, #4039, #367, #34912, #49597, #39603, #24306, #20645 ),
 .UNSPECIFIED., .F., .F.,
 ( 4, 3, 3, 3, 3, 4 ),
 ( 4.336808689942017255E-19, 0.0002176109881720244036, 0.0004352086762394596366, 0.0006528017811446883752, 0.0007615147961451703253, 0.0009453342004945543752 ),
 .UNSPECIFIED. ) ;
#65555 = EDGE_LOOP ( 'NONE', ( #48199, #33009, #22472, #11961 ) ) ;
#65556 = CIRCLE ( 'NONE', #36910, 5.000000000000001776 ) ;
#65557 = CARTESIAN_POINT ( 'NONE',  ( -29.54288940436046929, 0.2973637493423957889, -11.99820176872441024 ) ) ;
#65558 = CARTESIAN_POINT ( 'NONE',  ( 12.85578295477420951, -9.379166698650648115, -7.488245662904835065 ) ) ;
#65559 = DIRECTION ( 'NONE',  ( -1.000000000000000000, 0.000000000000000000, 0.000000000000000000 ) ) ;
#65560 = FACE_OUTER_BOUND ( 'NONE', #28035, .T. ) ;
#65561 = CYLINDRICAL_SURFACE ( 'NONE', #62294, 4.999999999999999112 ) ;
#65562 = ADVANCED_FACE ( 'NONE', ( #26385 ), #52336, .T. ) ;
#65563 = CARTESIAN_POINT ( 'NONE',  ( 2.000000000000001776, 6.662861565602083758, -1.421313227905602883 ) ) ;
#65564 = CIRCLE ( 'NONE', #51788, 6.936499999999988120 ) ;
#65565 = CARTESIAN_POINT ( 'NONE',  ( 0.3675815128205894289, -9.574637318041910206, -7.689697408877373519 ) ) ;
#65566 = CARTESIAN_POINT ( 'NONE',  ( -27.08423923533013422, 2.274768056034765173, -0.2759775751761893714 ) ) ;
#65567 = DIRECTION ( 'NONE',  ( -1.000000000000000000, 0.000000000000000000, 0.000000000000000000 ) ) ;
#65569 = ORIENTED_EDGE ( 'NONE', *, *, #18551, .T. ) ;
#65568 = CARTESIAN_POINT ( 'NONE',  ( 12.58609921286428879, 13.26567957380986407, -2.535074658557892935 ) ) ;
#65570 = CARTESIAN_POINT ( 'NONE',  ( -22.66110217412718697, -4.941631093908260830, -0.1747008913564142285 ) ) ;
#65571 = ORIENTED_EDGE ( 'NONE', *, *, #24453, .T. ) ;
#65572 = LINE ( 'NONE', #34659, #34832 ) ;
#65573 = ORIENTED_EDGE ( 'NONE', *, *, #58285, .F. ) ;
#65574 = B_SPLINE_CURVE_WITH_KNOTS ( 'NONE', 3,
 ( #26777, #47076, #12447, #32717, #33066, #58032, #57369, #17465, #32077, #27111, #62034, #53372, #11795, #62656, #7819, #2843, #52393, #16485, #47406, #6504, #28102, #6840, #57711, #21810 ),
 .UNSPECIFIED., .F., .F.,
 ( 4, 2, 2, 2, 2, 2, 2, 2, 2, 2, 2, 4 ),
 ( 0.000000000000000000, 0.0005079441056328478201, 0.001015888211265695640, 0.001523832316898543352, 0.002031776422531391280, 0.002539720528164238992, 0.003047664633797086704, 0.004063552845062785163, 0.005079441056328483188, 0.006095329267594181213, 0.007111217478859880106, 0.008127105690125578999 ),
 .UNSPECIFIED. ) ;
#65575 = ORIENTED_EDGE ( 'NONE', *, *, #36917, .T. ) ;
#65576 = ADVANCED_FACE ( 'NONE', ( #7399 ), #62597, .T. ) ;
#65577 = CARTESIAN_POINT ( 'NONE',  ( 0.3654063281920724160, 8.093076148786037649, 9.235228056823945764 ) ) ;
#65578 = CARTESIAN_POINT ( 'NONE',  ( 5.515539859299206427, -0.0008592514567755275617, -0.005991790098943834339 ) ) ;
#65579 = CARTESIAN_POINT ( 'NONE',  ( -27.10719052120871098, -0.6736837626858844796, -2.261993590776034235 ) ) ;
#65580 = CARTESIAN_POINT ( 'NONE',  ( -22.30986928587821794, 1.665628047792451216, -3.392803916780399831 ) ) ;
#65581 = DIRECTION ( 'NONE',  ( 0.000000000000000000, 0.01356324068817998940, -0.9999080150203989437 ) ) ;
#65582 = EDGE_CURVE ( 'NONE', #52407, #42299, #28095, .T. ) ;
#65583 = DIRECTION ( 'NONE',  ( 0.000000000000000000, -0.01356324068817999114, 0.9999080150203989437 ) ) ;
#65584 = ORIENTED_EDGE ( 'NONE', *, *, #65309, .F. ) ;
#65585 = DIRECTION ( 'NONE',  ( -1.000000000000000000, 0.000000000000000000, -0.000000000000000000 ) ) ;
#65586 = CYLINDRICAL_SURFACE ( 'NONE', #41922, 12.18650000000000055 ) ;
#65587 = CARTESIAN_POINT ( 'NONE',  ( 0.2653141617321003731, -7.837919552760664210, -9.409385893408590107 ) ) ;
#65588 = EDGE_CURVE ( 'NONE', #60939, #33165, #41898, .T. ) ;
#65589 = ORIENTED_EDGE ( 'NONE', *, *, #53702, .T. ) ;
#65590 = VECTOR ( 'NONE', #4516, 1000.000000000000000 ) ;
#65591 = CARTESIAN_POINT ( 'NONE',  ( 43.82484328533828233, -1.182663722159852604, 16.53294353590085208 ) ) ;
#65592 = CARTESIAN_POINT ( 'NONE',  ( -6.597603250208732284, -1.668269591273481067, 13.39685896832295953 ) ) ;
#65593 = CARTESIAN_POINT ( 'NONE',  ( -41.49302228377220558, -1.586477970524134085, -18.85982933713411214 ) ) ;
#65594 = ORIENTED_EDGE ( 'NONE', *, *, #1218, .F. ) ;
#65595 = FACE_OUTER_BOUND ( 'NONE', #40660, .T. ) ;
#65596 = B_SPLINE_CURVE_WITH_KNOTS ( 'NONE', 3,
 ( #28174, #18848, #59402, #55394, #19164, #35084, #18546 ),
 .UNSPECIFIED., .F., .F.,
 ( 4, 3, 4 ),
 ( 7.847387629678164802E-15, 0.002398160485434857984, 0.005002426799384661685 ),
 .UNSPECIFIED. ) ;
#65597 = CARTESIAN_POINT ( 'NONE',  ( 37.00000000000000711, -8.295159312811920316, -8.927548052240867449 ) ) ;
#65598 = DIRECTION ( 'NONE',  ( 1.000000000000000000, 0.000000000000000000, 0.000000000000000000 ) ) ;
#65599 = CIRCLE ( 'NONE', #48646, 4.999999999999999112 ) ;
#65600 = EDGE_CURVE ( 'NONE', #54679, #39152, #45126, .T. ) ;
#65601 = EDGE_CURVE ( 'NONE', #34584, #19083, #56828, .T. ) ;
#65602 = DIRECTION ( 'NONE',  ( -1.000000000000000000, 0.000000000000000000, 0.000000000000000000 ) ) ;
#65603 = CARTESIAN_POINT ( 'NONE',  ( 25.00000000000000355, -9.999999999999998224, 1.530808498934191521E-15 ) ) ;
#65604 =( BOUNDED_SURFACE ( )  B_SPLINE_SURFACE ( 3, 1, ( 
 ( #3977, #17956 ),
 ( #24240, #38217 ),
 ( #33889, #33244 ),
 ( #23269, #34217 ) ),
 .UNSPECIFIED., .F., .F., .F. ) 
 B_SPLINE_SURFACE_WITH_KNOTS ( ( 4, 4 ),
 ( 2, 2 ),
 ( 0.000000000000000000, 1.000000000000000000 ),
 ( 0.000000000000000000, 1.000000000000000000 ),
 .UNSPECIFIED. ) 
 GEOMETRIC_REPRESENTATION_ITEM ( )  RATIONAL_B_SPLINE_SURFACE ( (
 ( 1.000000000000000000, 1.000000000000000000),
 ( 0.9257577194822556033, 0.9980522942447415113),
 ( 0.9257577194822556033, 0.9980522942447415113),
 ( 1.000000000000000000, 1.000000000000000000) ) ) 
 REPRESENTATION_ITEM ( '' )  SURFACE ( )  );
#65605 = ORIENTED_EDGE ( 'NONE', *, *, #15651, .T. ) ;
#65606 = CARTESIAN_POINT ( 'NONE',  ( -22.30625920655495165, 3.687109008463850479, 0.8854385781085043483 ) ) ;
#65607 = DIRECTION ( 'NONE',  ( -1.000000000000000000, 0.000000000000000000, 0.000000000000000000 ) ) ;
#65608 = DIRECTION ( 'NONE',  ( 1.000000000000000000, -0.000000000000000000, 0.000000000000000000 ) ) ;
#65609 = ORIENTED_EDGE ( 'NONE', *, *, #63879, .T. ) ;
#65610 = EDGE_CURVE ( 'NONE', #25109, #56567, #51514, .T. ) ;
#65611 = DIRECTION ( 'NONE',  ( 0.5417962735734949131, 0.000000000000000000, -0.8405098440481674205 ) ) ;
#65612 = CARTESIAN_POINT ( 'NONE',  ( 2.241449424704146320, 6.642105568284105921, 3.763973574060562655 ) ) ;
#65613 = ORIENTED_EDGE ( 'NONE', *, *, #46594, .F. ) ;
#65614 = ORIENTED_EDGE ( 'NONE', *, *, #3698, .T. ) ;
#65615 = EDGE_LOOP ( 'NONE', ( #33662, #15417, #56341, #30897 ) ) ;
#65616 = ORIENTED_EDGE ( 'NONE', *, *, #38456, .T. ) ;
#65617 = CARTESIAN_POINT ( 'NONE',  ( 3.152665057734040488, 0.000000000000000000, 0.000000000000000000 ) ) ;
#65618 = CARTESIAN_POINT ( 'NONE',  ( 0.2650492433740058718, 6.027445608088999762, -10.66007796911762995 ) ) ;
#65619 = CARTESIAN_POINT ( 'NONE',  ( -35.00000000000000000, -6.280308599560071592, -9.926225166347094842 ) ) ;
#65620 = DIRECTION ( 'NONE',  ( 0.000000000000000000, 0.000000000000000000, -1.000000000000000000 ) ) ;
#65621 = CIRCLE ( 'NONE', #36967, 12.74999999999999822 ) ;
#65622 = CARTESIAN_POINT ( 'NONE',  ( -18.24374747313077094, 11.99999999999999822, 0.6271958409055273798 ) ) ;
#65624 = ORIENTED_EDGE ( 'NONE', *, *, #34099, .F. ) ;
#65623 = CARTESIAN_POINT ( 'NONE',  ( 22.88594695219327235, 3.421158645304719137, 11.50198563395281148 ) ) ;
#65625 = CARTESIAN_POINT ( 'NONE',  ( 2.000000000000001776, -4.976357229393820525, -4.652926418895619420 ) ) ;
#65626 = ORIENTED_EDGE ( 'NONE', *, *, #35099, .F. ) ;
#65627 = CARTESIAN_POINT ( 'NONE',  ( 0.3665391374699472626, -11.62960183138724446, -3.952034409876412635 ) ) ;
#65628 = EDGE_LOOP ( 'NONE', ( #11656, #53846, #12294, #59272 ) ) ;
#65629 = VERTEX_POINT ( 'NONE', #48651 ) ;
#65630 = CARTESIAN_POINT ( 'NONE',  ( -37.00000000000000711, -12.66641127287624968, -1.457575200925677494 ) ) ;
#65631 = CARTESIAN_POINT ( 'NONE',  ( 8.617947477504868559, -29.08580380500490747, 11.66524603227121659 ) ) ;
#65632 = VECTOR ( 'NONE', #47531, 1000.000000000000000 ) ;
#65633 = CARTESIAN_POINT ( 'NONE',  ( -35.00000000000000000, -11.47758908105692655, -2.497432891016966749 ) ) ;
#65634 = EDGE_CURVE ( 'NONE', #43663, #65715, #42775, .T. ) ;
#65635 = DIRECTION ( 'NONE',  ( 0.000000000000000000, 0.000000000000000000, 1.000000000000000000 ) ) ;
#65636 = DIRECTION ( 'NONE',  ( -0.000000000000000000, -0.000000000000000000, -1.000000000000000000 ) ) ;
#65637 = LINE ( 'NONE', #4511, #58610 ) ;
#65638 = VERTEX_POINT ( 'NONE', #64562 ) ;
#65639 = EDGE_CURVE ( 'NONE', #64188, #65779, #4802, .T. ) ;
#65640 = CIRCLE ( 'NONE', #29526, 1.500000000000000444 ) ;
#65641 = AXIS2_PLACEMENT_3D ( 'NONE', #8163, #28765, #49414 ) ;
#65642 = ORIENTED_EDGE ( 'NONE', *, *, #47111, .T. ) ;
#65643 = DIRECTION ( 'NONE',  ( -1.000000000000000000, 0.000000000000000000, -0.000000000000000000 ) ) ;
#65644 = ORIENTED_EDGE ( 'NONE', *, *, #5047, .T. ) ;
#65645 = AXIS2_PLACEMENT_3D ( 'NONE', #17006, #1414, #47606 ) ;
#65646 = ORIENTED_EDGE ( 'NONE', *, *, #9872, .F. ) ;
#65647 = B_SPLINE_CURVE_WITH_KNOTS ( 'NONE', 3,
 ( #36173, #26540, #51830, #11572, #310, #40521, #30860, #51183, #31527, #10580, #25903, #45853 ),
 .UNSPECIFIED., .F., .F.,
 ( 4, 2, 2, 2, 2, 4 ),
 ( 0.002404377236383827953, 0.003081670566939564634, 0.003758963897495300882, 0.005113550558606773377, 0.006468137219718247607, 0.007822723880829720103 ),
 .UNSPECIFIED. ) ;
#65648 = EDGE_CURVE ( 'NONE', #35595, #61175, #32998, .T. ) ;
#65649 = CARTESIAN_POINT ( 'NONE',  ( 145.1370849898475797, 3.309064568108273190E-14, 0.000000000000000000 ) ) ;
#65650 = CARTESIAN_POINT ( 'NONE',  ( 0.2739690278137261181, 10.51531306167495217, -6.282352088166152981 ) ) ;
#65651 = AXIS2_PLACEMENT_3D ( 'NONE', #51793, #62092, #47137 ) ;
#65652 = CARTESIAN_POINT ( 'NONE',  ( 2.241528039335008327, 1.310213701658589081, 7.521191296022422534 ) ) ;
#65653 = CARTESIAN_POINT ( 'NONE',  ( 17.87400702017532339, 6.562307548641454602, 10.06038912854612022 ) ) ;
#65654 = CARTESIAN_POINT ( 'NONE',  ( -22.27721056931765631, 1.183805672860844815, -3.486117586310724104 ) ) ;
#65655 = CARTESIAN_POINT ( 'NONE',  ( 2.990245332647628818, -8.248134185053306311, -1.974808303407486809 ) ) ;
#65656 = CARTESIAN_POINT ( 'NONE',  ( 28.54778262741603712, -12.36770326177027357, 5.424595989953875375 ) ) ;
#65657 = ORIENTED_EDGE ( 'NONE', *, *, #11915, .F. ) ;
#65658 = VERTEX_POINT ( 'NONE', #8399 ) ;
#65659 = DIRECTION ( 'NONE',  ( 0.000000000000000000, 0.000000000000000000, 1.000000000000000000 ) ) ;
#65660 = EDGE_CURVE ( 'NONE', #11187, #16616, #8737, .T. ) ;
#65661 = CARTESIAN_POINT ( 'NONE',  ( 37.25000000000000711, -45.00200000000000244, -4.500000000000000888 ) ) ;
#65662 = FACE_OUTER_BOUND ( 'NONE', #22923, .T. ) ;
#65663 = ADVANCED_FACE ( 'NONE', ( #53312 ), #33984, .T. ) ;
#65664 = DIRECTION ( 'NONE',  ( -1.000000000000000000, 0.000000000000000000, 0.000000000000000000 ) ) ;
#65665 = DIRECTION ( 'NONE',  ( 0.000000000000000000, -0.4134677391718385997, -0.9105187689796011563 ) ) ;
#65666 = DIRECTION ( 'NONE',  ( 0.000000000000000000, -0.01356324068817998940, 0.9999080150203990547 ) ) ;
#65667 = CARTESIAN_POINT ( 'NONE',  ( 2.241536586108914264, 5.844297002038606692, -4.912162027558427013 ) ) ;
#65668 = CARTESIAN_POINT ( 'NONE',  ( 2.491965175173733282, 6.046355957630737521, 4.796682362486673235 ) ) ;
#65669 = ORIENTED_EDGE ( 'NONE', *, *, #59118, .F. ) ;
#65670 = CARTESIAN_POINT ( 'NONE',  ( 3.047904605210419060, -0.4249306449415868880, 7.891858004695965434 ) ) ;
#65671 = CARTESIAN_POINT ( 'NONE',  ( 0.2638984909335720941, 10.50550771760528690, -6.295352574288876291 ) ) ;
#65672 = CARTESIAN_POINT ( 'NONE',  ( 35.00000000000000000, 8.389074212634284322, -8.839356091080075473 ) ) ;
#65673 = EDGE_CURVE ( 'NONE', #11147, #58967, #55761, .T. ) ;
#65674 = AXIS2_PLACEMENT_3D ( 'NONE', #11725, #2093, #56665 ) ;
#65675 = EDGE_CURVE ( 'NONE', #4186, #51107, #61868, .T. ) ;
#65676 = CARTESIAN_POINT ( 'NONE',  ( 3.152665057734023613, 0.4801242025591827001, -7.923639299008664594 ) ) ;
#65677 = CARTESIAN_POINT ( 'NONE',  ( 2.491965175174425173, -7.177226758613745261, 2.837956678388492637 ) ) ;
#65678 = CIRCLE ( 'NONE', #29616, 4.999999999999998224 ) ;
#65679 = EDGE_LOOP ( 'NONE', ( #57103, #41707, #23753, #55119 ) ) ;
#65680 = CARTESIAN_POINT ( 'NONE',  ( -27.20164183316783024, -2.339520810540427931, -1.232966507052649430 ) ) ;
#65681 = CARTESIAN_POINT ( 'NONE',  ( 5.536195898058073439, -0.003145317580921097589, -0.007896796515810917613 ) ) ;
#65682 = CARTESIAN_POINT ( 'NONE',  ( 15.64085769076060295, -34.91570230176446898, -5.822163132929507157 ) ) ;
#65683 = ORIENTED_EDGE ( 'NONE', *, *, #40224, .F. ) ;
#65684 = CIRCLE ( 'NONE', #61337, 4.999999999999999112 ) ;
#65685 = LINE ( 'NONE', #20154, #57824 ) ;
#65686 = CARTESIAN_POINT ( 'NONE',  ( -14.29135464769095520, 7.782112657557433089, -9.134479874907182051 ) ) ;
#65687 = CARTESIAN_POINT ( 'NONE',  ( -22.29978294495153790, -1.052446240539694378, -3.598607126810737356 ) ) ;
#65688 = AXIS2_PLACEMENT_3D ( 'NONE', #20464, #35731, #56358 ) ;
#65690 = VERTEX_POINT ( 'NONE', #6624 ) ;
#65689 = DIRECTION ( 'NONE',  ( 0.000000000000000000, 0.9796553971857736576, 0.2006870767258926158 ) ) ;
#65691 = DIRECTION ( 'NONE',  ( 1.000000000000000000, 0.000000000000000000, 0.000000000000000000 ) ) ;
#65692 = ADVANCED_FACE ( 'NONE', ( #31857 ), #40275, .F. ) ;
#65693 = CARTESIAN_POINT ( 'NONE',  ( 2.969415267404607928, -7.525730903320708265, -2.326350273511738287 ) ) ;
#65694 = ORIENTED_EDGE ( 'NONE', *, *, #7177, .F. ) ;
#65695 = CARTESIAN_POINT ( 'NONE',  ( -37.00000000000000711, 0.000000000000000000, 0.000000000000000000 ) ) ;
#65696 = DIRECTION ( 'NONE',  ( 1.000000000000000000, 0.000000000000000000, 0.000000000000000000 ) ) ;
#65697 = CARTESIAN_POINT ( 'NONE',  ( -16.05996651011518850, 8.379490699920680186, -10.58476169280406154 ) ) ;
#65698 = CARTESIAN_POINT ( 'NONE',  ( 0.000000000000000000, -6.936109781200700652, 2.853135311045000400 ) ) ;
#65699 = CARTESIAN_POINT ( 'NONE',  ( 0.3160775863651105189, -11.43919651388222647, -4.419114254410010822 ) ) ;
#65700 = CARTESIAN_POINT ( 'NONE',  ( -35.00000000000000000, 7.882940143791919319, -10.02106554660700333 ) ) ;
#65701 = CARTESIAN_POINT ( 'NONE',  ( -25.00000000000000355, -30.00000000000000000, 25.00000000000000000 ) ) ;
#65702 = ORIENTED_EDGE ( 'NONE', *, *, #45281, .T. ) ;
#65703 = DIRECTION ( 'NONE',  ( -1.000000000000000000, 0.000000000000000000, 0.000000000000000000 ) ) ;
#65704 = VERTEX_POINT ( 'NONE', #35623 ) ;
#65705 = DIRECTION ( 'NONE',  ( -1.000000000000000000, 0.000000000000000000, 0.000000000000000000 ) ) ;
#65706 = DIRECTION ( 'NONE',  ( 0.3865475372811021382, 0.7187975063895720718, -0.5778504531711020631 ) ) ;
#65707 = VECTOR ( 'NONE', #50167, 1000.000000000000000 ) ;
#65708 = DIRECTION ( 'NONE',  ( 1.000000000000000000, 0.000000000000000000, 0.000000000000000000 ) ) ;
#65709 = EDGE_LOOP ( 'NONE', ( #39052, #38197, #32544, #16106 ) ) ;
#65710 = DIRECTION ( 'NONE',  ( 0.000000000000000000, -0.8369827122275401710, -0.5472293298355184188 ) ) ;
#65711 = EDGE_CURVE ( 'NONE', #7123, #35706, #53640, .T. ) ;
#65712 = FACE_OUTER_BOUND ( 'NONE', #57871, .T. ) ;
#65713 = CIRCLE ( 'NONE', #39199, 5.000000000000001776 ) ;
#65714 = DIRECTION ( 'NONE',  ( 0.000000000000000000, -1.000000000000000000, 0.000000000000000000 ) ) ;
#65715 = VERTEX_POINT ( 'NONE', #24679 ) ;
#65716 = ORIENTED_EDGE ( 'NONE', *, *, #241, .T. ) ;
#65717 = DIRECTION ( 'NONE',  ( -1.000000000000000000, -0.000000000000000000, 0.000000000000000000 ) ) ;
#65718 = ORIENTED_EDGE ( 'NONE', *, *, #63248, .T. ) ;
#65719 = CARTESIAN_POINT ( 'NONE',  ( 22.36482863261543486, -11.96441317219524514, -0.9234811557364158707 ) ) ;
#65720 = CARTESIAN_POINT ( 'NONE',  ( -27.10719052120871098, 0.5475695427849553987, -2.295785794152566339 ) ) ;
#65721 = CARTESIAN_POINT ( 'NONE',  ( -27.08430418657511751, 2.280643121250624628, -0.2231435303617068100 ) ) ;
#65722 = AXIS2_PLACEMENT_3D ( 'NONE', #52849, #1674, #58505 ) ;
#65724 = AXIS2_PLACEMENT_3D ( 'NONE', #41751, #45421, #21480 ) ;
#65723 = CARTESIAN_POINT ( 'NONE',  ( 2.273267844204864829, 7.130811676080313077, -2.756477528575228320 ) ) ;
#65726 = EDGE_CURVE ( 'NONE', #217, #18633, #14312, .T. ) ;
#65725 = CARTESIAN_POINT ( 'NONE',  ( 2.000000000000001776, -3.937687286050771895, -6.383151168292510391 ) ) ;
#65727 = CARTESIAN_POINT ( 'NONE',  ( 0.2653519789438754106, -10.59450269107738585, 6.142177718873902847 ) ) ;
#65728 = CARTESIAN_POINT ( 'NONE',  ( 0.3632410797595194141, 11.62558329798851098, 3.951633449030948153 ) ) ;
#65729 = ORIENTED_EDGE ( 'NONE', *, *, #9349, .F. ) ;
#65730 = CARTESIAN_POINT ( 'NONE',  ( 0.8375941296802019709, -11.81283813871866961, 3.890418817177930588 ) ) ;
#65731 = FACE_OUTER_BOUND ( 'NONE', #47804, .T. ) ;
#65732 = EDGE_CURVE ( 'NONE', #8648, #60414, #12177, .T. ) ;
#65733 = LINE ( 'NONE', #25865, #40166 ) ;
#65734 = CARTESIAN_POINT ( 'NONE',  ( 10.87033471826838138, 13.40550848972586273, -1.597425313190320662 ) ) ;
#65735 = DIRECTION ( 'NONE',  ( -0.000000000000000000, -1.000000000000000000, -0.000000000000000000 ) ) ;
#65736 = LINE ( 'NONE', #50160, #36162 ) ;
#65737 = CYLINDRICAL_SURFACE ( 'NONE', #519, 12.75000000000000178 ) ;
#65738 = B_SPLINE_CURVE_WITH_KNOTS ( 'NONE', 3,
 ( #23023, #18705, #53935, #38963, #53280, #63240, #53621, #8375, #52635, #27656, #62911, #12362, #48624, #23341, #28650, #28330 ),
 .UNSPECIFIED., .F., .F.,
 ( 4, 3, 3, 3, 3, 4 ),
 ( 0.000000000000000000, 0.0002176109881720234278, 0.0004352086762394595824, 0.0006528017811446865321, 0.0007615147961451697832, 0.0009453342004943755903 ),
 .UNSPECIFIED. ) ;
#65739 = DIRECTION ( 'NONE',  ( -0.9582930651793755139, 0.2777159889015691219, 0.06744057189511871997 ) ) ;
#65740 = EDGE_CURVE ( 'NONE', #50026, #51491, #34949, .T. ) ;
#65741 = VERTEX_POINT ( 'NONE', #29985 ) ;
#65742 = CARTESIAN_POINT ( 'NONE',  ( -36.00000000000000711, -6.415447294506629206, -11.01837265713080072 ) ) ;
#65743 = ORIENTED_EDGE ( 'NONE', *, *, #19881, .T. ) ;
#65744 = CYLINDRICAL_SURFACE ( 'NONE', #47704, 5.000000000000000888 ) ;
#65745 = CARTESIAN_POINT ( 'NONE',  ( 0.3040950598368144520, 12.25911170648142878, 0.2511348647276071544 ) ) ;
#65746 = CARTESIAN_POINT ( 'NONE',  ( 5.536195898058073439, -0.007230647766619060536, -0.004468797463753857412 ) ) ;
#65747 = CARTESIAN_POINT ( 'NONE',  ( 2.907497136250466241, -7.791429554169687854, -1.009055026158189428 ) ) ;
#65748 = CARTESIAN_POINT ( 'NONE',  ( 5.520433897694421610, 0.01397038704729914628, -0.005630909886753002538 ) ) ;
#65749 = ORIENTED_EDGE ( 'NONE', *, *, #57734, .T. ) ;
#65750 = FACE_OUTER_BOUND ( 'NONE', #36968, .T. ) ;
#65751 = CARTESIAN_POINT ( 'NONE',  ( 2.589278595512906289, 2.423168677232077517, -7.361833592938230808 ) ) ;
#65752 = CARTESIAN_POINT ( 'NONE',  ( -27.08429572838383947, 2.089332284968718145, 0.9410937941433747955 ) ) ;
#65753 = CARTESIAN_POINT ( 'NONE',  ( 2.241526690369556096, -6.620271521148406890, -3.802233103835238825 ) ) ;
#65754 = ADVANCED_FACE ( 'NONE', ( #55257 ), #57159, .T. ) ;
#65755 = VECTOR ( 'NONE', #38883, 1000.000000000000000 ) ;
#65756 = CARTESIAN_POINT ( 'NONE',  ( 5.520433897694421610, -0.002108682515300378500, 0.01491416502703865263 ) ) ;
#65757 = CARTESIAN_POINT ( 'NONE',  ( 0.000000000000000000, 4.915517050588409376, 4.717154614762108622 ) ) ;
#65758 = VERTEX_POINT ( 'NONE', #50615 ) ;
#65759 = CIRCLE ( 'NONE', #37106, 5.000000000000000888 ) ;
#65760 = CARTESIAN_POINT ( 'NONE',  ( -35.00000000000000000, 11.07407352312212723, 3.916263239775389149 ) ) ;
#65761 = ORIENTED_EDGE ( 'NONE', *, *, #52223, .F. ) ;
#65762 = DIRECTION ( 'NONE',  ( 1.000000000000000000, 0.000000000000000000, 0.000000000000000000 ) ) ;
#65763 = CARTESIAN_POINT ( 'NONE',  ( -27.04788180060269198, -2.923150379392646325, 1.373100113388785237 ) ) ;
#65764 = DIRECTION ( 'NONE',  ( -0.000000000000000000, -0.000000000000000000, -1.000000000000000000 ) ) ;
#65765 = FACE_OUTER_BOUND ( 'NONE', #35066, .T. ) ;
#65766 = VECTOR ( 'NONE', #6046, 1000.000000000000000 ) ;
#65767 = EDGE_CURVE ( 'NONE', #15829, #38263, #11587, .T. ) ;
#65768 = VERTEX_POINT ( 'NONE', #20011 ) ;
#65769 = ORIENTED_EDGE ( 'NONE', *, *, #4155, .F. ) ;
#65770 = DIRECTION ( 'NONE',  ( -1.000000000000000000, 0.000000000000000000, 0.000000000000000000 ) ) ;
#65771 = ORIENTED_EDGE ( 'NONE', *, *, #37204, .F. ) ;
#65772 = DIRECTION ( 'NONE',  ( 1.000000000000000000, 0.000000000000000000, 0.000000000000000000 ) ) ;
#65773 = DIRECTION ( 'NONE',  ( 1.000000000000000000, 0.000000000000000000, 0.000000000000000000 ) ) ;
#65774 = CARTESIAN_POINT ( 'NONE',  ( 1.452237505248552996, 10.65201107290467597, 6.833827325205354519 ) ) ;
#65775 = CARTESIAN_POINT ( 'NONE',  ( -27.20164183316781248, 2.237540722393175585, -1.409601201084038191 ) ) ;
#65776 = DIRECTION ( 'NONE',  ( 1.000000000000000000, 0.000000000000000000, 0.000000000000000000 ) ) ;
#65777 = CARTESIAN_POINT ( 'NONE',  ( 1.375507693220547001, 11.20969178069697492, -5.789143338281640183 ) ) ;
#65778 = DIRECTION ( 'NONE',  ( -0.000000000000000000, -0.000000000000000000, -1.000000000000000000 ) ) ;
#65779 = VERTEX_POINT ( 'NONE', #52174 ) ;
#65780 = DIRECTION ( 'NONE',  ( 1.000000000000000000, 0.000000000000000000, 0.000000000000000000 ) ) ;
#65781 = VECTOR ( 'NONE', #48192, 1000.000000000000000 ) ;
#65782 = ORIENTED_EDGE ( 'NONE', *, *, #30774, .T. ) ;
#65783 = CARTESIAN_POINT ( 'NONE',  ( 35.00000000000000000, 4.705694406421931860E-17, -3.469127814946512892E-15 ) ) ;
#65784 = DIRECTION ( 'NONE',  ( 0.000000000000000000, 0.5987040770935676548, -0.8009703041134168533 ) ) ;
#65785 = ORIENTED_EDGE ( 'NONE', *, *, #11214, .F. ) ;
#65786 = DIRECTION ( 'NONE',  ( -0.7738190875236917732, 0.000000000000000000, 0.6334066780386838902 ) ) ;
#65787 = ORIENTED_EDGE ( 'NONE', *, *, #37142, .T. ) ;
#65788 =( BOUNDED_SURFACE ( )  B_SPLINE_SURFACE ( 3, 1, ( 
 ( #14808, #35750 ),
 ( #40422, #10172 ),
 ( #39782, #213 ),
 ( #15484, #40092 ) ),
 .UNSPECIFIED., .F., .F., .F. ) 
 B_SPLINE_SURFACE_WITH_KNOTS ( ( 4, 4 ),
 ( 2, 2 ),
 ( 0.000000000000000000, 1.000000000000000000 ),
 ( 0.000000000000000000, 1.000000000000000000 ),
 .UNSPECIFIED. ) 
 GEOMETRIC_REPRESENTATION_ITEM ( )  RATIONAL_B_SPLINE_SURFACE ( (
 ( 1.000000000000000000, 1.000000000000000000),
 ( 0.9942764183789327692, 0.8450855930916585379),
 ( 0.9942764183789327692, 0.8450855930916585379),
 ( 1.000000000000000000, 1.000000000000000000) ) ) 
 REPRESENTATION_ITEM ( '' )  SURFACE ( )  );
#65789 = CARTESIAN_POINT ( 'NONE',  ( -2.532614230583022152, -11.30437021680553222, 4.026315189028233377 ) ) ;
#65790 = EDGE_CURVE ( 'NONE', #36164, #44780, #30273, .T. ) ;
#65791 = CARTESIAN_POINT ( 'NONE',  ( 6.633398917601865286, -5.025995922460137599, -12.53510885642684158 ) ) ;
#65792 = DIRECTION ( 'NONE',  ( -1.000000000000000000, 0.000000000000000000, -0.000000000000000000 ) ) ;
#65793 = CARTESIAN_POINT ( 'NONE',  ( 2.491965175174054359, 7.177226758613687529, -2.837956678388308340 ) ) ;
#65794 = VERTEX_POINT ( 'NONE', #45600 ) ;
#65795 = ORIENTED_EDGE ( 'NONE', *, *, #54329, .T. ) ;
#65796 = CARTESIAN_POINT ( 'NONE',  ( 37.00000000000000711, -3.307597835713332213, -12.31350058095522115 ) ) ;
#65797 = EDGE_CURVE ( 'NONE', #12912, #4057, #13450, .T. ) ;
#65798 = ORIENTED_EDGE ( 'NONE', *, *, #3544, .F. ) ;
#65799 = CARTESIAN_POINT ( 'NONE',  ( 0.3106921474978477926, 11.60027394202204398, -3.971572160646637872 ) ) ;
#65800 = ORIENTED_EDGE ( 'NONE', *, *, #13190, .T. ) ;
#65801 = ORIENTED_EDGE ( 'NONE', *, *, #53934, .T. ) ;
#65802 = B_SPLINE_CURVE_WITH_KNOTS ( 'NONE', 3,
 ( #10873, #4598, #588, #4920, #60765, #19870, #55108, #46448, #41441, #26176, #9539, #5920, #9885, #20850, #55445, #50787, #14526, #21171, #65720 ),
 .UNSPECIFIED., .F., .F.,
 ( 4, 3, 3, 3, 3, 3, 4 ),
 ( 0.000000000000000000, 2.832085443540607455E-05, 4.217789847394679871E-05, 5.603488375046066227E-05, 6.989180858579203070E-05, 9.821094829918603994E-05, 0.0001178165571465128561 ),
 .UNSPECIFIED. ) ;
#65803 = ORIENTED_EDGE ( 'NONE', *, *, #16671, .T. ) ;
#65804 = CARTESIAN_POINT ( 'NONE',  ( 1.000000000000000888, -2.315790869867006219, -7.133520354428148025 ) ) ;
#65805 = CARTESIAN_POINT ( 'NONE',  ( 17.05919086487388370, -28.51594916623512432, 9.278936603800783445 ) ) ;
#65806 = AXIS2_PLACEMENT_3D ( 'NONE', #9666, #59914, #39611 ) ;
#65807 = DIRECTION ( 'NONE',  ( 0.000000000000000000, -0.8009703041134103030, -0.5987040770935762035 ) ) ;
#65808 = NEXT_ASSEMBLY_USAGE_OCCURRENCE ( 'NAUO1', ' ', ' ', #23030, #57568, $ ) ;
#65809 = NEXT_ASSEMBLY_USAGE_OCCURRENCE ( 'NAUO2', ' ', ' ', #23030, #7550, $ ) ;
#65810 = NEXT_ASSEMBLY_USAGE_OCCURRENCE ( 'NAUO3', ' ', ' ', #23030, #31126, $ ) ;
#65811 = NEXT_ASSEMBLY_USAGE_OCCURRENCE ( 'NAUO4', ' ', ' ', #23030, #64445, $ ) ;
#65812 = NEXT_ASSEMBLY_USAGE_OCCURRENCE ( 'NAUO5', ' ', ' ', #23030, #65283, $ ) ;
#65813 = NEXT_ASSEMBLY_USAGE_OCCURRENCE ( 'NAUO6', ' ', ' ', #23030, #64445, $ ) ;
ENDSEC;
END-ISO-10303-21;
